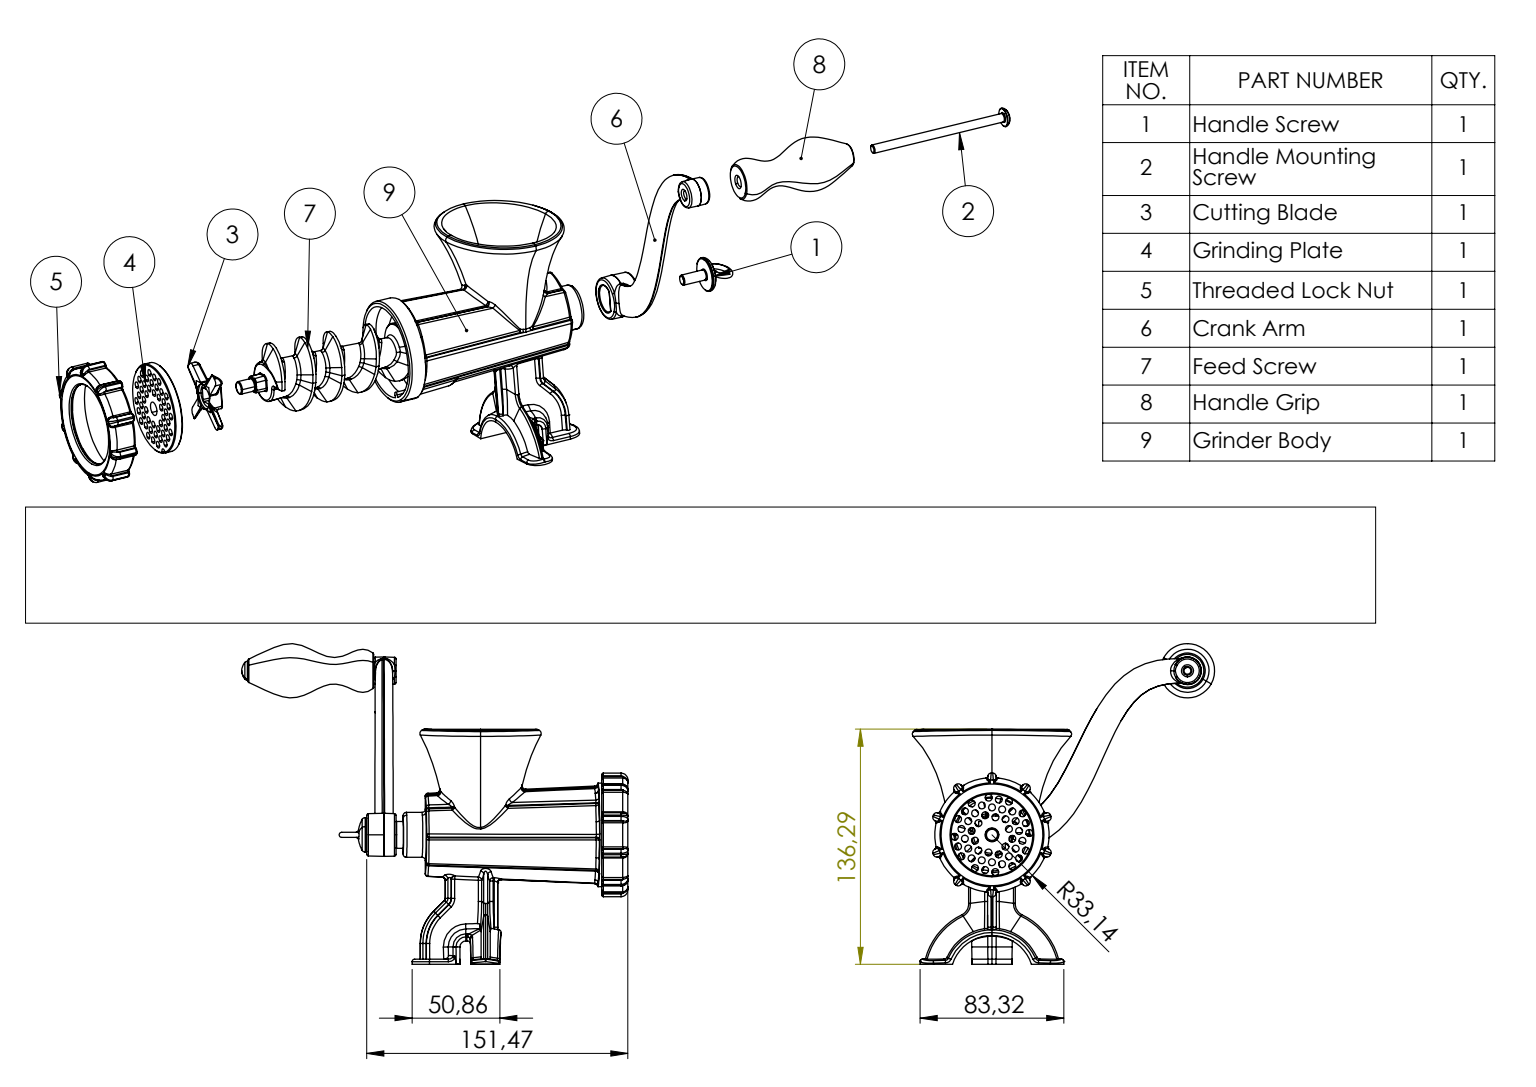
ISO-10303-21;
HEADER;
FILE_DESCRIPTION (('STEP AP214'),
    '1' );
FILE_NAME ('MAS-682',
    '2026-10-06T09:49:54',
    ( '' ),
    ( '' ),
    'SwSTEP 2.0',
    'SolidWorks 2020',
    '' );
FILE_SCHEMA (( 'AUTOMOTIVE_DESIGN' ));
ENDSEC;

DATA;
#1 = CARTESIAN_POINT ( 'NONE',  ( 0.9799183408087254188, 1466.964356560554961, 235.3982928250779310 ) ) ;
#2 = CIRCLE ( 'NONE', #35720, 101.7125698847119821 ) ;
#3 = CARTESIAN_POINT ( 'NONE',  ( -1.842962214803815835, 1515.372048948338943, 213.3835825141717351 ) ) ;
#4 = CARTESIAN_POINT ( 'NONE',  ( 9.183457267990059236, 1463.661210998930073, 215.2718514178839939 ) ) ;
#5 = CARTESIAN_POINT ( 'NONE',  ( -18.76815915579999938, 1485.949708182629820, 189.5055391954980166 ) ) ;
#6 = DIRECTION ( 'NONE',  ( -0.6736849260863841948, 0.000000000000000000, 0.7390186874254148774 ) ) ;
#7 = CARTESIAN_POINT ( 'NONE',  ( -29.55438145523249815, 1510.073575141020228, 200.5476930356480239 ) ) ;
#8 = AXIS2_PLACEMENT_3D ( 'NONE', #3263, #37391, #36278 ) ;
#9 = CARTESIAN_POINT ( 'NONE',  ( 24.07566136850000049, 1410.921070243630083, 209.6344585171510175 ) ) ;
#10 = CARTESIAN_POINT ( 'NONE',  ( 0.5551898266394985626, 1477.809674746627479, 198.7211068470872135 ) ) ;
#11 = CARTESIAN_POINT ( 'NONE',  ( 25.61451705386228284, 1436.639619060958239, 137.1797875125824362 ) ) ;
#12 = CARTESIAN_POINT ( 'NONE',  ( -1.480872463509999903, 1515.456375364289897, 204.9462865469589872 ) ) ;
#13 = CARTESIAN_POINT ( 'NONE',  ( 11.94438321470466136, 1435.361109817459010, 151.2115117280330310 ) ) ;
#14 =( BOUNDED_SURFACE ( )  B_SPLINE_SURFACE ( 3, 2, ( 
 ( #99288, #98203, #90906 ),
 ( #48377, #13076, #82520 ),
 ( #4699, #39956, #23138 ),
 ( #107158, #74130, #50021 ),
 ( #94768, #67940, #76875 ),
 ( #33745, #24238, #102047 ) ),
 .UNSPECIFIED., .F., .F., .F. ) 
 B_SPLINE_SURFACE_WITH_KNOTS ( ( 4, 2, 4 ),
 ( 3, 3 ),
 ( -1.474514954580286030E-17, 0.001312027981647312597, 0.002624055963294639939 ),
 ( 0.000000000000000000, 1.000000000000000000 ),
 .UNSPECIFIED. ) 
 GEOMETRIC_REPRESENTATION_ITEM ( )  RATIONAL_B_SPLINE_SURFACE ( (
 ( 1.000000000000000000, 0.9376006582765906705, 1.000000000000000000),
 ( 1.000000000000000000, 0.9569320108021501792, 1.000000000000000000),
 ( 1.000000000000000000, 0.9725743441620362528, 1.000000000000000000),
 ( 1.000000000000000000, 0.9942095667134138726, 1.000000000000000000),
 ( 1.000000000000000000, 1.000043666450818769, 1.000000000000000000),
 ( 1.000000000000000000, 1.000000000000000000, 1.000000000000000000) ) ) 
 REPRESENTATION_ITEM ( '' )  SURFACE ( )  );
#15 = CARTESIAN_POINT ( 'NONE',  ( 18.94656044352759849, 1455.761274322379904, 200.3458232381809694 ) ) ;
#16 = CARTESIAN_POINT ( 'NONE',  ( 1.715361092244999996, 1516.743010792419909, 212.5670474586069929 ) ) ;
#17 = CARTESIAN_POINT ( 'NONE',  ( -11.86274611122550127, 1422.387374207680068, 206.9860570071450070 ) ) ;
#18 = CARTESIAN_POINT ( 'NONE',  ( 0.1771307642749359867, 1476.157344213379929, 182.2594403546649744 ) ) ;
#20 = ORIENTED_EDGE ( 'NONE', *, *, #50403, .T. ) ;
#19 = DIRECTION ( 'NONE',  ( 0.9858563016923833633, 0.000000000000000000, 0.1675928173085483863 ) ) ;
#21 = B_SPLINE_CURVE_WITH_KNOTS ( 'NONE', 3,
 ( #95105, #62085, #88907, #54776, #87831, #29014 ),
 .UNSPECIFIED., .F., .F.,
 ( 4, 2, 4 ),
 ( 0.000000000000000000, 0.5000000000000000000, 1.000000000000000000 ),
 .UNSPECIFIED. ) ;
#22 = CARTESIAN_POINT ( 'NONE',  ( -25.18254675756193350, 1451.154070787092223, 137.5782062022625212 ) ) ;
#23 = CARTESIAN_POINT ( 'NONE',  ( -22.28696231330000188, 1506.798305107829947, 208.8466800722590051 ) ) ;
#24 = DIRECTION ( 'NONE',  ( -8.590429545572335868E-16, 0.9993908270191126375, 0.03489949670201628051 ) ) ;
#25 = CARTESIAN_POINT ( 'NONE',  ( -41.44976345434149323, 1445.539178997049930, 134.0999999985149884 ) ) ;
#26 = CARTESIAN_POINT ( 'NONE',  ( 1.285879139104720042E-15, 1391.913060387289988, 209.1218459572589836 ) ) ;
#27 = ORIENTED_EDGE ( 'NONE', *, *, #23843, .F. ) ;
#28 = CARTESIAN_POINT ( 'NONE',  ( -10.29516445159999982, 1471.669286221989978, 209.3797728120900103 ) ) ;
#29 = DIRECTION ( 'NONE',  ( -3.697785493223495027E-32, -1.000000000000000000, 1.836970198721029688E-16 ) ) ;
#30 = CARTESIAN_POINT ( 'NONE',  ( -14.66127766699999846, 1415.087974640030097, 218.7479844957980220 ) ) ;
#31 = CARTESIAN_POINT ( 'NONE',  ( -109.1321487942470014, 1384.869787291219836, 311.2644937792119322 ) ) ;
#32 = EDGE_CURVE ( 'NONE', #37900, #21516, #96808, .T. ) ;
#33 = CARTESIAN_POINT ( 'NONE',  ( -4.766037424247389964, 1433.470086930039997, 216.3697912905370231 ) ) ;
#34 = CARTESIAN_POINT ( 'NONE',  ( -2.760778634279479782, 1409.009468901610035, 188.0459411385839985 ) ) ;
#35 = AXIS2_PLACEMENT_3D ( 'NONE', #53186, #17882, #45348 ) ;
#36 = CARTESIAN_POINT ( 'NONE',  ( 21.19319384159999942, 1471.316885394430074, 209.8523956812749702 ) ) ;
#37 = CARTESIAN_POINT ( 'NONE',  ( -5.360823448879425079, 1422.265545810137382, 143.1524318712457386 ) ) ;
#38 = CARTESIAN_POINT ( 'NONE',  ( -12.43709857819999876, 1391.584050621440156, 209.7498280055400244 ) ) ;
#39 = CARTESIAN_POINT ( 'NONE',  ( -76.44887139282280941, 1385.142738521940146, 277.8929079653030385 ) ) ;
#40 = CARTESIAN_POINT ( 'NONE',  ( -11.42765938226460065, 1391.913060387289988, 211.2666090369880010 ) ) ;
#41 = CARTESIAN_POINT ( 'NONE',  ( 11.68414648092010033, 1426.908524124409951, 207.1431733947370049 ) ) ;
#42 = ORIENTED_EDGE ( 'NONE', *, *, #61891, .F. ) ;
#43 = CARTESIAN_POINT ( 'NONE',  ( -32.69752361389999606, 1451.315419473630072, 135.9818030182980237 ) ) ;
#44 = B_SPLINE_CURVE_WITH_KNOTS ( 'NONE', 3,
 ( #57452, #23800, #13187, #57991, #23253, #13738, #47922, #73698, #82058, #91579, #47375, #49043, #49590, #81500, #38947, #22130, #75882, #17028, #102702, #69152, #101057, #50145, #84272, #85931, #75348, #9234, #24355, #33305, #34970, #15944, #34425, #33864, #66948, #110030, #59640, #58541, #43391, #25996 ),
 .UNSPECIFIED., .F., .F.,
 ( 4, 2, 2, 2, 2, 2, 1, 1, 1, 1, 2, 2, 2, 2, 2, 1, 1, 1, 1, 2, 2, 2, 4 ),
 ( 0.000000000000000000, 0.1250000000000115463, 0.2500000000000230926, 0.3750000000000346390, 0.4375000000000425215, 0.4687500000000464073, 0.4843750000000510147, 0.4921875000000533462, 0.4960937500000545120, 0.4980468750000577316, 0.4990234375000622280, 0.5000000000000668354, 0.6250000000003189671, 0.6875000000004490852, 0.7187500000005095924, 0.7343750000005350165, 0.7421875000005526690, 0.7460937500005614398, 0.7480468750005607736, 0.7490234375005655476, 0.7500000000005703216, 0.8750000000002852163, 1.000000000000000000 ),
 .UNSPECIFIED. ) ;
#45 = CARTESIAN_POINT ( 'NONE',  ( 17.11746647137171706, 1443.086052842848176, 162.7559337440806644 ) ) ;
#47 = ORIENTED_EDGE ( 'NONE', *, *, #28974, .T. ) ;
#46 = CARTESIAN_POINT ( 'NONE',  ( 8.598096571001718758, 1427.995879741943554, 137.0999999980979567 ) ) ;
#48 = CARTESIAN_POINT ( 'NONE',  ( -109.4839102700000097, 1384.920896159549784, 311.2841190732590348 ) ) ;
#49 = CARTESIAN_POINT ( 'NONE',  ( 25.83534073490000083, 1509.142433023230069, 218.8511637550280113 ) ) ;
#50 = CARTESIAN_POINT ( 'NONE',  ( -8.821555121468717786, 1364.295427727885453, 207.6218459616988241 ) ) ;
#51 = CARTESIAN_POINT ( 'NONE',  ( -6.833281637050000690, 1495.558145441189936, 200.1869151102389992 ) ) ;
#52 = AXIS2_PLACEMENT_3D ( 'NONE', #79817, #89846, #28852 ) ;
#53 = CARTESIAN_POINT ( 'NONE',  ( 39.02162918670904901, 1452.247899825818649, 269.5933113026415526 ) ) ;
#54 = CARTESIAN_POINT ( 'NONE',  ( -1.906561575282239904E-08, 1509.051704408389924, 204.1347675157070114 ) ) ;
#55 = CARTESIAN_POINT ( 'NONE',  ( 5.639077273239999855, 1396.170382960830011, 219.3208623031979982 ) ) ;
#56 = CARTESIAN_POINT ( 'NONE',  ( -6.391938843916317836, 1508.551704408389696, 216.1347674408802106 ) ) ;
#57 = CARTESIAN_POINT ( 'NONE',  ( 5.798353088509999864, 1447.164911394289902, 201.8788308129090012 ) ) ;
#58 = DIRECTION ( 'NONE',  ( 0.8730704095473449389, 0.4873619484741930075, 0.01504630028510589926 ) ) ;
#59 = CARTESIAN_POINT ( 'NONE',  ( -7.009540617219531811, 1370.193319312941412, 208.3718459617010978 ) ) ;
#60 = CARTESIAN_POINT ( 'NONE',  ( -2.894710226049999946, 1455.369075570189807, 200.0025452760189921 ) ) ;
#61 = CARTESIAN_POINT ( 'NONE',  ( 2.477373605864999995, 1516.891731298979948, 206.2406231745169976 ) ) ;
#62 = CARTESIAN_POINT ( 'NONE',  ( 4.260142758989999834, 1446.575475407549902, 159.4573513494979693 ) ) ;
#63 = CYLINDRICAL_SURFACE ( 'NONE', #4748, 2.000000000000003553 ) ;
#64 = CARTESIAN_POINT ( 'NONE',  ( 13.58235818350000024, 1416.828044802929981, 196.3349386415980007 ) ) ;
#66 = EDGE_LOOP ( 'NONE', ( #105431, #26314, #4870, #3833, #51565, #60481, #89456, #79002, #97316, #37692 ) ) ;
#65 = CARTESIAN_POINT ( 'NONE',  ( -1.064557613579999895, 1496.012454471690035, 220.6945835667989968 ) ) ;
#67 = CARTESIAN_POINT ( 'NONE',  ( -1.491506560153236682, 1512.187213306747481, 242.6732489767341576 ) ) ;
#68 = ORIENTED_EDGE ( 'NONE', *, *, #43172, .F. ) ;
#69 = CARTESIAN_POINT ( 'NONE',  ( -16.59156838405375112, 1513.042027792487033, 221.1339923359998352 ) ) ;
#70 = ADVANCED_FACE ( 'NONE', ( #49805 ), #75938, .T. ) ;
#71 = CARTESIAN_POINT ( 'NONE',  ( -23.55087209330000064, 1410.914164826029946, 206.5508649875179970 ) ) ;
#73 = CARTESIAN_POINT ( 'NONE',  ( 16.84666619867320136, 1410.587845839309921, 191.9034688781510170 ) ) ;
#72 = CARTESIAN_POINT ( 'NONE',  ( -10.49968249828000033, 1425.371007265300022, 102.3058044465100096 ) ) ;
#74 = ADVANCED_FACE ( 'NONE', ( #10550 ), #8899, .T. ) ;
#75 = CARTESIAN_POINT ( 'NONE',  ( -5.770883602015000058, 1516.603620185149794, 211.4160555996369908 ) ) ;
#76 = CARTESIAN_POINT ( 'NONE',  ( 23.39541812081691674, 1509.845305380639729, 190.2643963894789181 ) ) ;
#77 = EDGE_CURVE ( 'NONE', #86690, #11573, #16701, .T. ) ;
#78 = TOROIDAL_SURFACE ( 'NONE', #103817, 9.500000000000000000, 0.5000000000000000000 ) ;
#79 = CARTESIAN_POINT ( 'NONE',  ( 21.64985223704960049, 1524.547395018738371, 234.6923279487310197 ) ) ;
#80 = B_SPLINE_CURVE_WITH_KNOTS ( 'NONE', 5,
 ( #89898, #13169, #47358, #81485, #38932, #107253 ),
 .UNSPECIFIED., .F., .F.,
 ( 6, 6 ),
 ( 0.000000000000000000, 1.000000000000000000 ),
 .UNSPECIFIED. ) ;
#81 = CARTESIAN_POINT ( 'NONE',  ( -39.02581108420000078, 1422.344276296430053, 266.4771448061979982 ) ) ;
#82 = CARTESIAN_POINT ( 'NONE',  ( -12.50903734399489942, 1378.842647904740033, 209.0065662253330174 ) ) ;
#83 = EDGE_CURVE ( 'NONE', #58839, #22042, #17431, .T. ) ;
#84 = CARTESIAN_POINT ( 'NONE',  ( 16.07415551216847049, 1461.167067577646549, 229.3519873809775333 ) ) ;
#85 = CONTEXT_DEPENDENT_SHAPE_REPRESENTATION ( #69986, #23231 ) ;
#86 = EDGE_CURVE ( 'NONE', #1893, #51148, #21, .T. ) ;
#87 = CARTESIAN_POINT ( 'NONE',  ( -4.994992778070000305, 1391.721842379389955, 214.6484993776389842 ) ) ;
#88 = CARTESIAN_POINT ( 'NONE',  ( 15.23962836178434799, 1416.181292664740113, 211.4166089860522106 ) ) ;
#89 = ORIENTED_EDGE ( 'NONE', *, *, #96759, .T. ) ;
#90 = CARTESIAN_POINT ( 'NONE',  ( 10.26791835527880004, 1396.449850368310081, 216.1922904392330338 ) ) ;
#91 = CARTESIAN_POINT ( 'NONE',  ( 9.827367186236088514, 1460.770885483560050, 206.7613957114989773 ) ) ;
#92 = AXIS2_PLACEMENT_3D ( 'NONE', #81436, #4747, #22069 ) ;
#93 = CARTESIAN_POINT ( 'NONE',  ( -17.53303485170000187, 1459.032577061930169, 228.4504051497980015 ) ) ;
#94 = ORIENTED_EDGE ( 'NONE', *, *, #44106, .T. ) ;
#96 = ORIENTED_EDGE ( 'NONE', *, *, #80068, .T. ) ;
#95 = AXIS2_PLACEMENT_3D ( 'NONE', #82965, #55590, #47722 ) ;
#97 = CARTESIAN_POINT ( 'NONE',  ( 2.803078862940000082, 1426.178365722219951, 191.2633630063989756 ) ) ;
#98 = CARTESIAN_POINT ( 'NONE',  ( 32.97913964219430483, 1512.187213306747481, 197.9697544589745632 ) ) ;
#99 = DIRECTION ( 'NONE',  ( 0.9858563016923833633, 0.000000000000000000, 0.1675928173085483863 ) ) ;
#100 = CARTESIAN_POINT ( 'NONE',  ( -12.21821484229520927, 1417.425190588804981, 199.7413714526001911 ) ) ;
#101 = AXIS2_PLACEMENT_3D ( 'NONE', #52542, #86674, #33491 ) ;
#102 = CARTESIAN_POINT ( 'NONE',  ( 4.324092179420000015, 1515.269353058490196, 209.1218459615519976 ) ) ;
#103 = CARTESIAN_POINT ( 'NONE',  ( -2.622430729442981168, 1523.621879633028584, 242.1535192357228254 ) ) ;
#104 = CARTESIAN_POINT ( 'NONE',  ( 2.470168521978398868, 1512.187213306747481, 175.3649660270905315 ) ) ;
#105 = CARTESIAN_POINT ( 'NONE',  ( 3.199785385034799923, 1421.555840881979975, 183.4721396264059763 ) ) ;
#106 = CARTESIAN_POINT ( 'NONE',  ( 9.417062327005512046, 1451.666586838229932, 209.4644760955090135 ) ) ;
#107 = CARTESIAN_POINT ( 'NONE',  ( 17.11714618744633754, 1443.086052842848630, 162.7561046190426737 ) ) ;
#108 = EDGE_CURVE ( 'NONE', #73608, #106056, #21407, .T. ) ;
#109 = CARTESIAN_POINT ( 'NONE',  ( -98.27039657997829636, 1384.868559307870100, 295.9020111865049785 ) ) ;
#110 = ORIENTED_EDGE ( 'NONE', *, *, #5630, .F. ) ;
#111 = CARTESIAN_POINT ( 'NONE',  ( 6.939219482805000005, 1516.783701990830195, 203.3409846960470020 ) ) ;
#112 = CARTESIAN_POINT ( 'NONE',  ( 5.786847739675000213, 1517.104497701820037, 209.8595134730280165 ) ) ;
#113 = ORIENTED_EDGE ( 'NONE', *, *, #67279, .T. ) ;
#114 = CARTESIAN_POINT ( 'NONE',  ( 10.79382126600000014, 1414.913060387329779, 222.1041115775979904 ) ) ;
#115 = CARTESIAN_POINT ( 'NONE',  ( 3.849857897463838885, 1511.509056589855390, 217.2694430494650248 ) ) ;
#116 = ORIENTED_EDGE ( 'NONE', *, *, #25867, .F. ) ;
#117 = CARTESIAN_POINT ( 'NONE',  ( -14.19373553490000006, 1416.535385209630022, 221.7254479851980022 ) ) ;
#118 = CARTESIAN_POINT ( 'NONE',  ( -12.93811130839999812, 1442.831169986189934, 169.4238961894979809 ) ) ;
#119 = DIRECTION ( 'NONE',  ( -5.980589973904019347E-17, 1.000000000000000000, -1.736889445713099699E-16 ) ) ;
#120 = EDGE_CURVE ( 'NONE', #81793, #103948, #97600, .T. ) ;
#121 = CARTESIAN_POINT ( 'NONE',  ( -9.628359219779209610, 1460.738556064009799, 208.1949697569470175 ) ) ;
#122 = CARTESIAN_POINT ( 'NONE',  ( -5.139599399479999775, 1425.322806783530041, 186.3313725629980127 ) ) ;
#123 = CARTESIAN_POINT ( 'NONE',  ( 10.94055631708340037, 1470.192781946979949, 206.9724510450730008 ) ) ;
#124 = CARTESIAN_POINT ( 'NONE',  ( -3.048415848927723992, 1468.134006689671196, 219.8853015524805699 ) ) ;
#125 = EDGE_CURVE ( 'NONE', #75164, #6066, #41467, .T. ) ;
#126 = CARTESIAN_POINT ( 'NONE',  ( -15.90471755817952548, 1410.840444494871690, 191.2727014167670916 ) ) ;
#127 = CARTESIAN_POINT ( 'NONE',  ( -16.54254117820000047, 1379.596826475559965, 208.2028925074129688 ) ) ;
#128 = CARTESIAN_POINT ( 'NONE',  ( 22.53878404599999641, 1411.058442739730026, 206.1986151668880041 ) ) ;
#130 = DIRECTION ( 'NONE',  ( -0.6736849260863839728, 0.000000000000000000, 0.7390186874254150995 ) ) ;
#129 = CARTESIAN_POINT ( 'NONE',  ( 17.81158319340000062, 1457.914457808930138, 229.9274238559980006 ) ) ;
#131 = CARTESIAN_POINT ( 'NONE',  ( -4.952890104507372548, 1423.293534163835830, 184.7224492574210615 ) ) ;
#132 = AXIS2_PLACEMENT_3D ( 'NONE', #29173, #87435, #11285 ) ;
#133 = B_SPLINE_SURFACE_WITH_KNOTS ( 'NONE', 5, 3, ( 
 ( #34867, #77434, #42173, #67396 ),
 ( #93646, #52248, #60652, #69055 ),
 ( #103155, #43831, #101494, #16929 ),
 ( #41622, #26457, #43287, #93111 ),
 ( #86374, #34317, #94776, #76885 ),
 ( #8007, #734, #1283, #85822 ),
 ( #35424, #50030, #76324, #8554 ),
 ( #51130, #69611, #84159, #18053 ),
 ( #24248, #109929, #16382, #42726 ) ),
 .UNSPECIFIED., .F., .F., .F.,
 ( 6, 3, 6 ),
 ( 4, 4 ),
 ( 0.000000000000000000, 5.782490304330000441, 11.25975508159999983 ),
 ( 37.69911184309999896, 40.20365518519999881 ),
 .UNSPECIFIED. ) ;
#134 = CARTESIAN_POINT ( 'NONE',  ( -17.39685236538799984, 1503.136637835580132, 222.8801028628849963 ) ) ;
#135 = ORIENTED_EDGE ( 'NONE', *, *, #51675, .F. ) ;
#136 = CARTESIAN_POINT ( 'NONE',  ( -2.793439186891359949, 1486.025328193850100, 182.0741020391329812 ) ) ;
#137 = DIRECTION ( 'NONE',  ( -1.000000000000000000, 0.000000000000000000, 0.000000000000000000 ) ) ;
#138 = CARTESIAN_POINT ( 'NONE',  ( -2.931110993877138249, 1485.094118085803984, 183.0973985693935617 ) ) ;
#139 = CARTESIAN_POINT ( 'NONE',  ( 5.979558325686289422, 1406.768155905330104, 269.6447222190780053 ) ) ;
#141 = ORIENTED_EDGE ( 'NONE', *, *, #18307, .F. ) ;
#140 = CARTESIAN_POINT ( 'NONE',  ( 0.7783252048321530614, 1515.125841190099891, 204.7939957918700316 ) ) ;
#142 = CARTESIAN_POINT ( 'NONE',  ( 0.9041354327699999693, 1416.839648768630013, 190.2140802940980109 ) ) ;
#143 = AXIS2_PLACEMENT_3D ( 'NONE', #57309, #48343, #30414 ) ;
#144 = CARTESIAN_POINT ( 'NONE',  ( -0.9578802547590020700, 1508.340034268889895, 220.7784182282989889 ) ) ;
#145 = CARTESIAN_POINT ( 'NONE',  ( -11.74804893329999800, 1426.270137612329790, 145.0346010018980110 ) ) ;
#146 = DIRECTION ( 'NONE',  ( -1.110223024629289185E-15, -0.7071067811865475727, -0.7071067811865475727 ) ) ;
#147 = CARTESIAN_POINT ( 'NONE',  ( 0.000000000000000000, 1511.163060387329779, 209.1218459616979999 ) ) ;
#148 = DIRECTION ( 'NONE',  ( 1.000000000000000000, 5.309750374689999822E-19, 2.343158368729999945E-19 ) ) ;
#149 = CARTESIAN_POINT ( 'NONE',  ( -5.649091365077420157, 1427.323616392150143, 201.6849725672220188 ) ) ;
#150 = CARTESIAN_POINT ( 'NONE',  ( -15.65821252386499829, 1513.518111364920060, 223.8216251916669819 ) ) ;
#151 = CARTESIAN_POINT ( 'NONE',  ( 9.215280650669999574, 1410.394055827930060, 230.1315963332980061 ) ) ;
#153 = FACE_OUTER_BOUND ( 'NONE', #32956, .T. ) ;
#152 = CARTESIAN_POINT ( 'NONE',  ( -25.75006378359999815, 1482.723232260229906, 211.9130519178279997 ) ) ;
#154 = DIRECTION ( 'NONE',  ( -0.02617375475769094517, 0.9996573249755578150, 0.0004088821302708953143 ) ) ;
#155 = ORIENTED_EDGE ( 'NONE', *, *, #76478, .F. ) ;
#156 = CARTESIAN_POINT ( 'NONE',  ( -2.881222795715000284, 1516.891731298979948, 206.6444723262370076 ) ) ;
#157 = CARTESIAN_POINT ( 'NONE',  ( 27.01536995560000065, 1412.459480457830068, 266.9350197775979723 ) ) ;
#158 = DIRECTION ( 'NONE',  ( 0.8672669759446630655, 0.000000000000000000, -0.4978433412588735285 ) ) ;
#159 = CARTESIAN_POINT ( 'NONE',  ( 22.53781764839999724, 1430.293776123330190, 201.7931574036180109 ) ) ;
#160 = CARTESIAN_POINT ( 'NONE',  ( -0.2682927907274870183, 1508.576597181550142, 237.9003827947630043 ) ) ;
#161 = CARTESIAN_POINT ( 'NONE',  ( -7.567241880450000124, 1385.515695150829970, 219.0512258816089854 ) ) ;
#162 = CARTESIAN_POINT ( 'NONE',  ( 21.91792426780000369, 1509.678451168330184, 227.8819284857980279 ) ) ;
#163 = CARTESIAN_POINT ( 'NONE',  ( -6.501609782144661231, 1517.151704408390060, 200.8207946853451631 ) ) ;
#164 = AXIS2_PLACEMENT_3D ( 'NONE', #96746, #87233, #71584 ) ;
#165 = CARTESIAN_POINT ( 'NONE',  ( -14.80402621179999834, 1415.917690476640018, 204.7946628682890093 ) ) ;
#166 = CARTESIAN_POINT ( 'NONE',  ( -13.11944326200000077, 1446.139497881190209, 187.9998882741980140 ) ) ;
#167 = CARTESIAN_POINT ( 'NONE',  ( -4.911821946417970430, 1485.009740505319996, 198.2803573512069875 ) ) ;
#168 = B_SPLINE_SURFACE_WITH_KNOTS ( 'NONE', 5, 5, ( 
 ( #106952, #71755, #28601, #29694, #97994, #64429 ),
 ( #81736, #88517, #89050, #98547, #97459, #20727 ),
 ( #54922, #21816, #107503, #56015, #12336, #105310 ),
 ( #90139, #13422, #62802, #46527, #11801, #45969 ),
 ( #80104, #37555, #80661, #98449, #4411, #47512 ),
 ( #96816, #3329, #28500, #89503, #82194, #106305 ),
 ( #97348, #37453, #12795, #72186, #90039, #21163 ),
 ( #90596, #62695, #38004, #13317, #4937, #12239 ),
 ( #72718, #45871, #80005, #29056, #106840, #63242 ) ),
 .UNSPECIFIED., .F., .F., .F.,
 ( 6, 3, 6 ),
 ( 6, 6 ),
 ( 14.29638737439180041, 25.07790639679999956, 35.02433850343369670 ),
 ( 0.000000000000000000, 2.000134677740009970 ),
 .UNSPECIFIED. ) ;
#169 = CARTESIAN_POINT ( 'NONE',  ( -8.621279951388869378, 1436.974942194019832, 209.5887057810519991 ) ) ;
#170 = CARTESIAN_POINT ( 'NONE',  ( -4.720696006799999900, 1497.300349750090163, 219.8012105612990013 ) ) ;
#171 = ORIENTED_EDGE ( 'NONE', *, *, #62426, .F. ) ;
#172 = CARTESIAN_POINT ( 'NONE',  ( 4.989246313819999834, 1471.909539260290103, 189.7082128665990126 ) ) ;
#173 = CARTESIAN_POINT ( 'NONE',  ( -12.50898706442170116, 1409.349883841199926, 217.3002069970499974 ) ) ;
#174 = EDGE_CURVE ( 'NONE', #66491, #29176, #106889, .T. ) ;
#175 = CARTESIAN_POINT ( 'NONE',  ( -11.30102602861320094, 1508.425847713210032, 208.0120230822289784 ) ) ;
#176 = CARTESIAN_POINT ( 'NONE',  ( -12.26345067459182658, 1378.041391332198373, 210.3086285185297868 ) ) ;
#177 = CARTESIAN_POINT ( 'NONE',  ( -23.55147266200000189, 1470.760850431830022, 269.0841978914980359 ) ) ;
#178 = DIRECTION ( 'NONE',  ( 0.000000000000000000, 0.000000000000000000, 1.000000000000000000 ) ) ;
#179 = CARTESIAN_POINT ( 'NONE',  ( -13.16128167722848552, 1513.520077403203913, 192.3341213175320092 ) ) ;
#180 = EDGE_CURVE ( 'NONE', #17368, #18936, #5451, .T. ) ;
#181 = CARTESIAN_POINT ( 'NONE',  ( -24.15092527543778189, 1444.494566185576332, 211.6397483413928455 ) ) ;
#182 = CARTESIAN_POINT ( 'NONE',  ( -76.22674438190679780, 1384.646826080419942, 301.0779023118020064 ) ) ;
#183 = CARTESIAN_POINT ( 'NONE',  ( -21.60464161394589766, 1384.953571151939968, 202.1045221056799903 ) ) ;
#184 = CIRCLE ( 'NONE', #28783, 1.000000000000007994 ) ;
#185 = CARTESIAN_POINT ( 'NONE',  ( 11.29240053233250052, 1415.034069327070029, 222.6155400430430120 ) ) ;
#186 = DIRECTION ( 'NONE',  ( -1.000000000000000000, 0.000000000000000000, 0.000000000000000000 ) ) ;
#187 = CARTESIAN_POINT ( 'NONE',  ( -14.61131892634599971, 1485.012037849769968, 224.2679068592169926 ) ) ;
#188 = CARTESIAN_POINT ( 'NONE',  ( -22.86536645260000000, 1410.206636297830073, 204.9906524142479896 ) ) ;
#189 = CIRCLE ( 'NONE', #57423, 12.49965726619999984 ) ;
#190 = CARTESIAN_POINT ( 'NONE',  ( 13.83520663969999909, 1414.913060387329779, 199.8641522158279997 ) ) ;
#191 = CARTESIAN_POINT ( 'NONE',  ( -20.12564951288306503, 1512.187213306747481, 180.7149624981946658 ) ) ;
#192 = ADVANCED_FACE ( 'NONE', ( #107906 ), #49678, .T. ) ;
#193 = CARTESIAN_POINT ( 'NONE',  ( 10.49733858283609855, 1480.659481621079976, 208.1380713321520091 ) ) ;
#194 = DIRECTION ( 'NONE',  ( -0.000000000000000000, -1.000000000000000000, 0.000000000000000000 ) ) ;
#195 = CARTESIAN_POINT ( 'NONE',  ( -17.48499182319999790, 1442.494624508590050, 219.3180649765990040 ) ) ;
#196 = CARTESIAN_POINT ( 'NONE',  ( 17.03788438627352519, 1524.775785348137333, 181.0918340916085754 ) ) ;
#197 = CARTESIAN_POINT ( 'NONE',  ( -21.44637737161449920, 1506.412668956640118, 216.0243792029939982 ) ) ;
#200 = CARTESIAN_POINT ( 'NONE',  ( 10.79382269979189957, 1414.913060387349788, 222.1041130917409987 ) ) ;
#199 = CIRCLE ( 'NONE', #3805, 0.5000000000000157652 ) ;
#198 = CARTESIAN_POINT ( 'NONE',  ( -22.57636395089999937, 1411.060965688729766, 211.7929440282880194 ) ) ;
#201 = CARTESIAN_POINT ( 'NONE',  ( 11.69274081191520054, 1426.725035085969921, 141.0012239352140000 ) ) ;
#202 = CARTESIAN_POINT ( 'NONE',  ( 9.734438220109071338, 1436.124822200840072, 210.5259218765519620 ) ) ;
#203 = CARTESIAN_POINT ( 'NONE',  ( -10.63028651890000020, 1491.023698122589849, 211.9405787866489845 ) ) ;
#204 = CARTESIAN_POINT ( 'NONE',  ( 6.587579149753620023, 1448.214850730340004, 201.2521096501800173 ) ) ;
#205 = CARTESIAN_POINT ( 'NONE',  ( -12.02002121700249937, 1447.120365805550136, 187.5076542713389927 ) ) ;
#206 = CIRCLE ( 'NONE', #57435, 2.000000000000001776 ) ;
#207 = CARTESIAN_POINT ( 'NONE',  ( -5.006329619514999330, 1516.755758396839838, 202.5714564999769891 ) ) ;
#208 = CARTESIAN_POINT ( 'NONE',  ( -4.941360932494764491, 1398.060275951993162, 221.1476519450009164 ) ) ;
#209 = CARTESIAN_POINT ( 'NONE',  ( -3.034707026709789979, 1440.440247136690004, 157.2489849372729793 ) ) ;
#210 = FACE_BOUND ( 'NONE', #98928, .T. ) ;
#211 = CARTESIAN_POINT ( 'NONE',  ( 1.951029617469999922, 1508.751449870530223, 237.3205679125979941 ) ) ;
#213 = EDGE_LOOP ( 'NONE', ( #57511, #100598, #97650, #95419, #60917 ) ) ;
#212 = CARTESIAN_POINT ( 'NONE',  ( -31.38187927383859943, 1379.627610869280034, 219.3043553578710032 ) ) ;
#214 = ORIENTED_EDGE ( 'NONE', *, *, #74162, .T. ) ;
#215 = CARTESIAN_POINT ( 'NONE',  ( 11.97689773866060037, 1433.612225593400126, 149.9683442909959865 ) ) ;
#216 = CARTESIAN_POINT ( 'NONE',  ( 21.50855465202003813, 1524.374578187333327, 184.1253178261501660 ) ) ;
#217 = EDGE_LOOP ( 'NONE', ( #25668, #43396, #24555, #73471 ) ) ;
#218 = CARTESIAN_POINT ( 'NONE',  ( -106.9777543680000065, 1379.497227361900059, 308.7284971550590171 ) ) ;
#219 = EDGE_CURVE ( 'NONE', #44996, #39203, #32843, .T. ) ;
#220 = CARTESIAN_POINT ( 'NONE',  ( -10.22078022364619976, 1448.827725899079724, 207.2905427559460065 ) ) ;
#221 = CARTESIAN_POINT ( 'NONE',  ( -4.554962005479259446, 1508.731359867455467, 211.6097811027402713 ) ) ;
#223 = CARTESIAN_POINT ( 'NONE',  ( 1.188177619867464285, 1416.835288280217583, 190.1185025207718695 ) ) ;
#222 = DIRECTION ( 'NONE',  ( 0.7071067811870476172, 0.000000000000000000, -0.7071067811860475283 ) ) ;
#224 = CARTESIAN_POINT ( 'NONE',  ( 16.85900957629469943, 1498.111060690920112, 230.7389555287900009 ) ) ;
#225 = AXIS2_PLACEMENT_3D ( 'NONE', #60606, #95291, #28634 ) ;
#226 = CARTESIAN_POINT ( 'NONE',  ( 2.328600095410000126, 1488.173045798130033, 182.1148965703980025 ) ) ;
#227 = CARTESIAN_POINT ( 'NONE',  ( 13.43167025587599817, 1509.382104656720003, 235.1752264429409820 ) ) ;
#228 = DIRECTION ( 'NONE',  ( -0.6736849260863839728, 0.000000000000000000, 0.7390186874254150995 ) ) ;
#229 =( LENGTH_UNIT ( ) NAMED_UNIT ( * ) SI_UNIT ( .MILLI., .METRE. ) );
#230 = CARTESIAN_POINT ( 'NONE',  ( 4.229167303610000594, 1436.983388288790138, 227.1518914930990150 ) ) ;
#231 = CARTESIAN_POINT ( 'NONE',  ( 13.54623987573500088, 1415.059973085240017, 197.7769859117730107 ) ) ;
#232 = CARTESIAN_POINT ( 'NONE',  ( 11.57525528770000101, 1432.243446488439986, 151.1962572209980067 ) ) ;
#233 = CARTESIAN_POINT ( 'NONE',  ( 7.300066962235000290, 1513.142795523620180, 201.9269575992269949 ) ) ;
#234 = VERTEX_POINT ( 'NONE', #57535 ) ;
#235 = CARTESIAN_POINT ( 'NONE',  ( 13.94902171141210090, 1435.073072362720040, 149.1168395385139718 ) ) ;
#236 = ORIENTED_EDGE ( 'NONE', *, *, #47228, .T. ) ;
#237 = VERTEX_POINT ( 'NONE', #65385 ) ;
#238 = EDGE_CURVE ( 'NONE', #55027, #57510, #22026, .T. ) ;
#239 = CARTESIAN_POINT ( 'NONE',  ( 13.40011037178709330, 1444.420227106130369, 169.3684798139838676 ) ) ;
#240 = CARTESIAN_POINT ( 'NONE',  ( -11.01696037870000033, 1462.338713412430252, 233.0647636304979926 ) ) ;
#241 = CARTESIAN_POINT ( 'NONE',  ( -9.862951377749247683, 1522.051704408389924, 228.3939896778649654 ) ) ;
#242 = DIRECTION ( 'NONE',  ( -8.555280247707230573E-26, -1.000000000000000000, 1.836970198721029688E-16 ) ) ;
#243 = CARTESIAN_POINT ( 'NONE',  ( -7.886135186697788235, 1512.218159651028827, 212.0631589305448301 ) ) ;
#244 = AXIS2_PLACEMENT_3D ( 'NONE', #101072, #98882, #31677 ) ;
#245 = EDGE_CURVE ( 'NONE', #43735, #91400, #105524, .T. ) ;
#246 = LINE ( 'NONE', #1902, #99740 ) ;
#247 = CARTESIAN_POINT ( 'NONE',  ( -18.61085923841566014, 1379.601406803549708, 208.6983520666371419 ) ) ;
#248 = CARTESIAN_POINT ( 'NONE',  ( -18.76550561599999867, 1380.296266888499986, 210.4015402955490117 ) ) ;
#249 = ORIENTED_EDGE ( 'NONE', *, *, #87778, .F. ) ;
#250 = CARTESIAN_POINT ( 'NONE',  ( -4.043990345725000601, 1516.983612918759945, 206.6425990843970055 ) ) ;
#251 = ORIENTED_EDGE ( 'NONE', *, *, #53107, .T. ) ;
#252 = CARTESIAN_POINT ( 'NONE',  ( 21.27308478715089990, 1440.913060387330006, 223.7805658757509946 ) ) ;
#253 = CARTESIAN_POINT ( 'NONE',  ( -18.65749898560000020, 1509.387464492830077, 230.8014192534980111 ) ) ;
#254 = EDGE_LOOP ( 'NONE', ( #74179, #87875, #88245, #39917, #100540, #44653, #57226, #30791 ) ) ;
#255 = FACE_OUTER_BOUND ( 'NONE', #49988, .T. ) ;
#256 = CARTESIAN_POINT ( 'NONE',  ( 7.213837368615000578, 1512.784460098860109, 215.9877155789269807 ) ) ;
#258 = EDGE_LOOP ( 'NONE', ( #43493, #77998, #28454, #11261 ) ) ;
#257 = CARTESIAN_POINT ( 'NONE',  ( 2.105736771246019767, 1423.442917612190058, 192.6277106367970191 ) ) ;
#259 = CARTESIAN_POINT ( 'NONE',  ( 23.78270988279999898, 1434.944176083839920, 215.5045224494480181 ) ) ;
#260 = CARTESIAN_POINT ( 'NONE',  ( -17.51735096566159910, 1508.551704408389924, 210.4017072017840064 ) ) ;
#261 = EDGE_CURVE ( 'NONE', #100109, #93900, #60124, .T. ) ;
#262 = DIRECTION ( 'NONE',  ( 1.755985294532464991E-16, -1.000000000000000000, 1.338183447452830017E-16 ) ) ;
#263 = CARTESIAN_POINT ( 'NONE',  ( 5.082331142230000154, 1453.684120746589770, 217.0135184815189859 ) ) ;
#264 = CARTESIAN_POINT ( 'NONE',  ( -24.62269181266490037, 1457.704162723289983, 212.0269868133230204 ) ) ;
#265 = EDGE_CURVE ( 'NONE', #68013, #83547, #85444, .T. ) ;
#266 = CARTESIAN_POINT ( 'NONE',  ( 7.720650135305000994, 1516.977993847330026, 214.9014730243169993 ) ) ;
#267 = CARTESIAN_POINT ( 'NONE',  ( -2.999960124414019713, 1428.921094993090037, 200.2473963957619958 ) ) ;
#268 = CARTESIAN_POINT ( 'NONE',  ( 6.161099242332739756, 1511.774605969369986, 217.7619246857520068 ) ) ;
#269 = CARTESIAN_POINT ( 'NONE',  ( 7.260544162646080046, 1508.878901399440110, 215.8879859943839961 ) ) ;
#270 = CARTESIAN_POINT ( 'NONE',  ( 3.268859396054999866, 1516.922519270759949, 211.5998327024669834 ) ) ;
#271 = CARTESIAN_POINT ( 'NONE',  ( 14.81130958389999996, 1410.375311269529902, 191.5354464119980094 ) ) ;
#272 = AXIS2_PLACEMENT_3D ( 'NONE', #31208, #50242, #83816 ) ;
#273 = CARTESIAN_POINT ( 'NONE',  ( -16.59643141521007692, 1486.110667197937119, 187.3981733332393844 ) ) ;
#275 = EDGE_LOOP ( 'NONE', ( #35605, #7044, #107686, #49764, #7625 ) ) ;
#274 = CARTESIAN_POINT ( 'NONE',  ( -62.99252469870000937, 1388.208599921950054, 284.2099993179589887 ) ) ;
#276 = CARTESIAN_POINT ( 'NONE',  ( -56.29735061249719763, 1385.085427587770027, 274.2983070328880331 ) ) ;
#277 = CARTESIAN_POINT ( 'NONE',  ( 33.67855476909999624, 1460.266122003729834, 261.9078250184979879 ) ) ;
#278 = CARTESIAN_POINT ( 'NONE',  ( 10.93308164779909930, 1490.452501404730128, 209.9926135395130018 ) ) ;
#279 = CARTESIAN_POINT ( 'NONE',  ( -29.22959469711409852, 1509.933780326070064, 211.7723416727030212 ) ) ;
#280 = CARTESIAN_POINT ( 'NONE',  ( -7.422625755698760486, 1509.173068315250021, 237.5382155034599805 ) ) ;
#281 = CARTESIAN_POINT ( 'NONE',  ( -23.72450110970000026, 1447.345343915189915, 214.6425533432180259 ) ) ;
#282 = AXIS2_PLACEMENT_3D ( 'NONE', #69728, #96558, #36645 ) ;
#284 = CARTESIAN_POINT ( 'NONE',  ( 17.19105300219910148, 1409.567693813439973, 222.3521885693010063 ) ) ;
#283 = LINE ( 'NONE', #53444, #107281 ) ;
#285 = LINE ( 'NONE', #92652, #110374 ) ;
#287 = B_SPLINE_CURVE_WITH_KNOTS ( 'NONE', 3,
 ( #66514, #15499, #49697, #83827, #109592, #28341 ),
 .UNSPECIFIED., .F., .F.,
 ( 4, 2, 4 ),
 ( 2.797157557069881010E-17, 0.001087661325621732452, 0.002175322651243436715 ),
 .UNSPECIFIED. ) ;
#286 = DIRECTION ( 'NONE',  ( 0.8775825618903774217, -3.365001152038843908E-31, 0.4794255386041944567 ) ) ;
#288 = VERTEX_POINT ( 'NONE', #17119 ) ;
#289 = CARTESIAN_POINT ( 'NONE',  ( 2.482067860225000366, 1517.099836525840146, 203.3337487049469985 ) ) ;
#290 = CARTESIAN_POINT ( 'NONE',  ( -11.00800901137619903, 1508.439403004749920, 218.3132624233929846 ) ) ;
#291 = CARTESIAN_POINT ( 'NONE',  ( 29.02628104170000256, 1509.926680456829899, 206.2525988583179810 ) ) ;
#292 = CARTESIAN_POINT ( 'NONE',  ( 24.56509571990000040, 1440.948426447710062, 213.0043250210379995 ) ) ;
#293 = CARTESIAN_POINT ( 'NONE',  ( -4.675540975309999681, 1462.620895424390028, 200.5633310686890241 ) ) ;
#294 = CARTESIAN_POINT ( 'NONE',  ( -19.66678637224480397, 1519.551704408389924, 215.8936635741279986 ) ) ;
#295 = VECTOR ( 'NONE', #1841, 999.9999999999998863 ) ;
#296 = CARTESIAN_POINT ( 'NONE',  ( 27.60463613754729906, 1435.937341596739998, 136.4952273551159863 ) ) ;
#297 = CARTESIAN_POINT ( 'NONE',  ( 36.19701834746070546, 1449.940556718190010, 136.2509691137539960 ) ) ;
#298 = CARTESIAN_POINT ( 'NONE',  ( 18.86027053263898168, 1512.187213306747481, 230.7762769316004778 ) ) ;
#299 = CARTESIAN_POINT ( 'NONE',  ( -107.7923298369999969, 1386.973993580999831, 297.6574877858589616 ) ) ;
#300 = CARTESIAN_POINT ( 'NONE',  ( -16.09127082379999862, 1410.842149181930154, 226.7264691084980086 ) ) ;
#301 = CARTESIAN_POINT ( 'NONE',  ( 11.69460626421270000, 1479.933455554200009, 210.6357844716710019 ) ) ;
#302 = CARTESIAN_POINT ( 'NONE',  ( 5.597778194180000888, 1506.679269386989972, 219.3685102149989916 ) ) ;
#303 = CIRCLE ( 'NONE', #93224, 4.820754716980014010 ) ;
#304 = LINE ( 'NONE', #17034, #54663 ) ;
#305 = ORIENTED_EDGE ( 'NONE', *, *, #65971, .T. ) ;
#306 = CARTESIAN_POINT ( 'NONE',  ( 0.8090580814599999115, 1427.166763959530044, 147.9649995502979891 ) ) ;
#307 = CARTESIAN_POINT ( 'NONE',  ( 3.902542035141590038, 1426.015650130040058, 185.2953857556300079 ) ) ;
#308 = EDGE_CURVE ( 'NONE', #12135, #84259, #7929, .T. ) ;
#309 = CARTESIAN_POINT ( 'NONE',  ( -4.487249408019919450, 1509.038630944639863, 212.6094330731689865 ) ) ;
#310 = CARTESIAN_POINT ( 'NONE',  ( -19.02974267272306719, 1517.051704408389924, 207.1627782414018100 ) ) ;
#311 = CARTESIAN_POINT ( 'NONE',  ( -0.5392968480769999573, 1417.272289817929959, 235.8882545161980033 ) ) ;
#313 = CARTESIAN_POINT ( 'NONE',  ( 31.55762699681125127, 1523.390106123591067, 196.3178534513329794 ) ) ;
#312 = CARTESIAN_POINT ( 'NONE',  ( 11.46319645939999887, 1501.893709296690076, 208.7006337201350163 ) ) ;
#314 = CARTESIAN_POINT ( 'NONE',  ( -12.99045328924907139, 1444.881939451659264, 186.2719392246208656 ) ) ;
#315 = DIRECTION ( 'NONE',  ( 0.2720708970484284062, 0.6839977328998089190, 0.6768489701308448847 ) ) ;
#316 = CARTESIAN_POINT ( 'NONE',  ( -8.788316527315000570, 1511.741868877540128, 215.3741124244170067 ) ) ;
#317 = AXIS2_PLACEMENT_3D ( 'NONE', #43515, #103956, #9895 ) ;
#318 = DIRECTION ( 'NONE',  ( 0.000000000000000000, 1.000000000000000000, -1.836970198721029688E-16 ) ) ;
#319 = CARTESIAN_POINT ( 'NONE',  ( -38.49765372626540483, 1444.525112228479884, 137.1053225085370002 ) ) ;
#320 = CARTESIAN_POINT ( 'NONE',  ( -5.102340803919999779, 1483.010473641589897, 199.7820758705289848 ) ) ;
#321 = CARTESIAN_POINT ( 'NONE',  ( 25.44234826850000175, 1436.623918441529895, 137.2992118829979802 ) ) ;
#322 = CARTESIAN_POINT ( 'NONE',  ( -10.92603999506069989, 1396.294606111510120, 207.3491235618079997 ) ) ;
#323 = VERTEX_POINT ( 'NONE', #26651 ) ;
#324 = EDGE_CURVE ( 'NONE', #40683, #47896, #52438, .T. ) ;
#325 = CARTESIAN_POINT ( 'NONE',  ( -16.89772930833600029, 1410.137463210610122, 226.0661309239629873 ) ) ;
#326 = CARTESIAN_POINT ( 'NONE',  ( 2.488082932330000219, 1441.600846913620217, 150.5962877614979902 ) ) ;
#327 = ORIENTED_EDGE ( 'NONE', *, *, #30892, .T. ) ;
#328 = VERTEX_POINT ( 'NONE', #27220 ) ;
#329 = CARTESIAN_POINT ( 'NONE',  ( -2.217375791810000329, 1495.290970025190290, 217.2501089269190118 ) ) ;
#330 = DIRECTION ( 'NONE',  ( -0.4978433412588676998, 0.000000000000000000, 0.8672669759446663962 ) ) ;
#332 = CARTESIAN_POINT ( 'NONE',  ( -0.6694169535389160597, 1457.182704574260015, 219.7360533319789795 ) ) ;
#331 = FACE_OUTER_BOUND ( 'NONE', #57581, .T. ) ;
#333 = CARTESIAN_POINT ( 'NONE',  ( 23.36041073559999859, 1411.089115351430110, 212.3712601659579775 ) ) ;
#334 = CARTESIAN_POINT ( 'NONE',  ( 4.215774578864469824, 1425.101385327330036, 185.2788908656129934 ) ) ;
#335 = CARTESIAN_POINT ( 'NONE',  ( -2.852637967456935986, 1419.721280333027380, 186.1746705150881098 ) ) ;
#336 = CARTESIAN_POINT ( 'NONE',  ( 7.206186347910000123, 1424.944465238209887, 212.8420735846389960 ) ) ;
#337 = CARTESIAN_POINT ( 'NONE',  ( -9.573037224950001089, 1423.427965722019962, 192.3355728592989919 ) ) ;
#339 = CARTESIAN_POINT ( 'NONE',  ( -5.441672317485815036, 1511.126521620285303, 201.4186169187619839 ) ) ;
#338 = B_SPLINE_CURVE_WITH_KNOTS ( 'NONE', 3,
 ( #14649, #33638, #59986, #52681 ),
 .UNSPECIFIED., .F., .F.,
 ( 4, 4 ),
 ( 0.000000000000000000, 0.0002960034161023847852 ),
 .UNSPECIFIED. ) ;
#340 = CARTESIAN_POINT ( 'NONE',  ( 2.852330403769999911, 1449.230534335530137, 183.5545985393980004 ) ) ;
#341 = PRESENTATION_LAYER_ASSIGNMENT (  '', '', ( #48608 ) ) ;
#342 = CARTESIAN_POINT ( 'NONE',  ( 9.369782510130001185, 1366.497526915280105, 207.6218459616989946 ) ) ;
#344 = ORIENTED_EDGE ( 'NONE', *, *, #61935, .F. ) ;
#343 = CARTESIAN_POINT ( 'NONE',  ( -4.951136445669599511E-10, 1417.070352045260051, 236.6937895817889910 ) ) ;
#345 = VERTEX_POINT ( 'NONE', #33388 ) ;
#346 = CARTESIAN_POINT ( 'NONE',  ( -41.48252549709999926, 1444.135617533290088, 136.5500651578979898 ) ) ;
#347 = DIRECTION ( 'NONE',  ( 0.000000000000000000, 1.000000000000000000, 0.000000000000000000 ) ) ;
#348 = CARTESIAN_POINT ( 'NONE',  ( -0.4691143273430000149, 1471.436294014529949, 269.3346704442980126 ) ) ;
#349 = CARTESIAN_POINT ( 'NONE',  ( 12.17607342826484818, 1434.037890756064598, 147.4852139652959693 ) ) ;
#350 = CARTESIAN_POINT ( 'NONE',  ( -113.4000000000000057, 1358.631207110790001, 311.1659210709989907 ) ) ;
#351 = CARTESIAN_POINT ( 'NONE',  ( 20.46339790889999932, 1475.513060387329915, 205.2504343647379983 ) ) ;
#352 = ADVANCED_FACE ( 'NONE', ( #86566 ), #108998, .T. ) ;
#353 = CARTESIAN_POINT ( 'NONE',  ( -8.173822499230000815, 1384.405547763340110, 199.6789892872290011 ) ) ;
#354 = CARTESIAN_POINT ( 'NONE',  ( 22.51991254300000023, 1410.619212212730190, 206.2037069855880134 ) ) ;
#355 = CARTESIAN_POINT ( 'NONE',  ( -20.80119636470000088, 1475.513060387329915, 204.3591166435880098 ) ) ;
#356 = CARTESIAN_POINT ( 'NONE',  ( 4.911313360425503483, 1370.788543751794350, 208.3718459617010978 ) ) ;
#357 = CARTESIAN_POINT ( 'NONE',  ( -5.603383157293649656E-09, 1406.911841289329914, 196.1218459609980300 ) ) ;
#358 = CARTESIAN_POINT ( 'NONE',  ( -12.11929752427059981, 1407.056436474629891, 267.1741674207860342 ) ) ;
#359 = EDGE_CURVE ( 'NONE', #10483, #4434, #57345, .T. ) ;
#360 = CARTESIAN_POINT ( 'NONE',  ( -13.80543509878039998, 1434.979598264029846, 148.5369193816260065 ) ) ;
#361 = EDGE_LOOP ( 'NONE', ( #97319, #80641, #79673, #74910 ) ) ;
#362 = DIRECTION ( 'NONE',  ( 1.836970198721029688E-16, 1.000000000000000000, -2.953460612019999929E-19 ) ) ;
#363 = CARTESIAN_POINT ( 'NONE',  ( 13.57336059360000036, 1443.191372133680034, 188.8849899699980028 ) ) ;
#364 = EDGE_LOOP ( 'NONE', ( #86550, #29612, #108325, #100325 ) ) ;
#365 = VERTEX_POINT ( 'NONE', #20997 ) ;
#366 = EDGE_CURVE ( 'NONE', #43369, #37055, #92016, .T. ) ;
#367 = AXIS2_PLACEMENT_3D ( 'NONE', #81942, #5812, #24233 ) ;
#368 = CARTESIAN_POINT ( 'NONE',  ( 4.479677203900762628, 1422.012945122907468, 183.9385808951501531 ) ) ;
#369 = CARTESIAN_POINT ( 'NONE',  ( 3.034145577506000446, 1440.440283345010130, 157.2495443575080003 ) ) ;
#370 = CARTESIAN_POINT ( 'NONE',  ( -1.703779643355000095, 1517.057265928030120, 213.1670284501570052 ) ) ;
#371 = CARTESIAN_POINT ( 'NONE',  ( -18.11868862529999902, 1485.487861948229920, 188.9570397301980051 ) ) ;
#372 = EDGE_CURVE ( 'NONE', #74254, #52548, #25231, .T. ) ;
#373 = FACE_OUTER_BOUND ( 'NONE', #57009, .T. ) ;
#374 = ORIENTED_EDGE ( 'NONE', *, *, #31699, .T. ) ;
#375 = CARTESIAN_POINT ( 'NONE',  ( -109.5441724410000006, 1374.437034645689891, 304.2218460466590386 ) ) ;
#376 =( BOUNDED_CURVE ( )  B_SPLINE_CURVE ( 3, ( #102045, #83062, #101486, #40501 ),
 .UNSPECIFIED., .F., .T. ) 
 B_SPLINE_CURVE_WITH_KNOTS ( ( 4, 4 ),
 ( 4.045555810179484624, 4.691360937121570096 ),
 .UNSPECIFIED. ) 
 CURVE ( )  GEOMETRIC_REPRESENTATION_ITEM ( )  RATIONAL_B_SPLINE_CURVE ( ( 1.000000000000000000, 0.9655455809096770148, 0.9655455809096770148, 1.000000000000000000 ) ) 
 REPRESENTATION_ITEM ( '' )  );
#377 = CARTESIAN_POINT ( 'NONE',  ( -3.070761075385165295, 1457.085219852218870, 218.1263196974262826 ) ) ;
#378 = CARTESIAN_POINT ( 'NONE',  ( -3.264778817514999876, 1516.727068157269969, 204.1245957781970048 ) ) ;
#379 = AXIS2_PLACEMENT_3D ( 'NONE', #95016, #67622, #7691 ) ;
#380 = CARTESIAN_POINT ( 'NONE',  ( -29.75011777940000002, 1509.993906963430163, 208.5595589157580036 ) ) ;
#381 = CARTESIAN_POINT ( 'NONE',  ( -1.569161292555000031, 1517.051704408389924, 216.8444262845069943 ) ) ;
#382 = CARTESIAN_POINT ( 'NONE',  ( -39.58883837791880467, 1384.581576029320104, 212.5204386266630081 ) ) ;
#383 = CARTESIAN_POINT ( 'NONE',  ( -1.344035116579999967, 1408.775599479229868, 195.0461770646979858 ) ) ;
#384 = CARTESIAN_POINT ( 'NONE',  ( -26.58019104509060071, 1469.327027323300172, 208.7773797362419828 ) ) ;
#386 = ORIENTED_EDGE ( 'NONE', *, *, #99268, .F. ) ;
#385 = CARTESIAN_POINT ( 'NONE',  ( 15.37090799315269152, 1506.446781340675443, 193.3909299311295626 ) ) ;
#387 = CARTESIAN_POINT ( 'NONE',  ( -27.41515663979030037, 1488.740012749160087, 208.8186931342820003 ) ) ;
#388 = CARTESIAN_POINT ( 'NONE',  ( 26.30775428189999943, 1469.245646012430143, 210.8538279144680132 ) ) ;
#389 = CARTESIAN_POINT ( 'NONE',  ( -36.13018326403506109, 1379.645813938799392, 224.1534624346936937 ) ) ;
#390 = CARTESIAN_POINT ( 'NONE',  ( 10.73298406322840037, 1460.408024784029976, 207.0975327187530013 ) ) ;
#391 = CARTESIAN_POINT ( 'NONE',  ( -23.95553108059999659, 1435.340102472350054, 136.9960523771979979 ) ) ;
#392 = ADVANCED_FACE ( 'NONE', ( #11528 ), #84870, .F. ) ;
#393 = CARTESIAN_POINT ( 'NONE',  ( 0.7576635334400020350, 1516.855632454399938, 211.9899581013969794 ) ) ;
#394 = TOROIDAL_SURFACE ( 'NONE', #71885, 30.13701971169416538, 3.000000000000000000 ) ;
#395 = CARTESIAN_POINT ( 'NONE',  ( -68.60472032309999690, 1379.747634528509707, 279.7221279746590312 ) ) ;
#396 = CARTESIAN_POINT ( 'NONE',  ( -18.69110324289999880, 1444.867398023490068, 206.3373603049990095 ) ) ;
#397 = CARTESIAN_POINT ( 'NONE',  ( -29.67375955050042791, 1525.697946996596102, 221.2718133379099186 ) ) ;
#398 = CARTESIAN_POINT ( 'NONE',  ( -2.881325412095000260, 1517.003078582959688, 208.0029426616869728 ) ) ;
#399 = EDGE_CURVE ( 'NONE', #104547, #81525, #8616, .T. ) ;
#400 = ORIENTED_EDGE ( 'NONE', *, *, #22203, .T. ) ;
#401 = DIRECTION ( 'NONE',  ( -0.03489949670255338560, 0.9993908270190677845, 2.284588940413689109E-07 ) ) ;
#402 = CARTESIAN_POINT ( 'NONE',  ( 5.375553136205760474, 1441.026369937100071, 154.8319413496199957 ) ) ;
#403 = CIRCLE ( 'NONE', #27160, 5.868098490439995985 ) ;
#404 = CARTESIAN_POINT ( 'NONE',  ( -73.55923423229999969, 1384.652831667379814, 298.9494481685590017 ) ) ;
#405 = ORIENTED_EDGE ( 'NONE', *, *, #65155, .F. ) ;
#406 = CARTESIAN_POINT ( 'NONE',  ( -13.74298021802130165, 1385.299105108359981, 219.1768037944160028 ) ) ;
#407 = CARTESIAN_POINT ( 'NONE',  ( -10.75057650454519909, 1492.402834311169954, 203.1666067258980206 ) ) ;
#408 = CARTESIAN_POINT ( 'NONE',  ( 12.69127487099669871, 1434.626206151899851, 149.6849692847659981 ) ) ;
#409 = CARTESIAN_POINT ( 'NONE',  ( 14.76180801577280022, 1459.302556161789880, 230.0031883768110106 ) ) ;
#410 = CARTESIAN_POINT ( 'NONE',  ( -21.86081811034360101, 1508.398734063270012, 226.4470915494329972 ) ) ;
#411 = CARTESIAN_POINT ( 'NONE',  ( -33.93019615848938741, 1501.977400791986611, 220.5829544587966211 ) ) ;
#412 = DIRECTION ( 'NONE',  ( -0.9999999999999995559, -4.156278225545078260E-11, 3.325661287725353434E-08 ) ) ;
#413 = CARTESIAN_POINT ( 'NONE',  ( -6.954065720117950100, 1517.051704408389924, 183.5505540514350002 ) ) ;
#415 = CARTESIAN_POINT ( 'NONE',  ( -3.619432601040000197, 1421.014464036429899, 186.0219392937979990 ) ) ;
#414 = CARTESIAN_POINT ( 'NONE',  ( -7.325541825264999751, 1516.710692850270107, 214.1269169785269924 ) ) ;
#416 = CARTESIAN_POINT ( 'NONE',  ( 20.30888173789999840, 1509.664622709230116, 187.3912422546979997 ) ) ;
#417 = CARTESIAN_POINT ( 'NONE',  ( -3.259729335964999919, 1517.119374999550018, 216.4589997383470177 ) ) ;
#418 = ORIENTED_EDGE ( 'NONE', *, *, #83682, .T. ) ;
#419 = CARTESIAN_POINT ( 'NONE',  ( -12.45665494490000214, 1416.827520077930103, 194.7672771341979967 ) ) ;
#420 = CARTESIAN_POINT ( 'NONE',  ( -16.94440841599999814, 1420.377411313550056, 203.4608118218089885 ) ) ;
#421 = ORIENTED_EDGE ( 'NONE', *, *, #109564, .F. ) ;
#422 = CARTESIAN_POINT ( 'NONE',  ( 3.316185754920000228, 1421.597412442629775, 183.5076398005980138 ) ) ;
#423 = B_SPLINE_CURVE_WITH_KNOTS ( 'NONE', 3,
 ( #95450, #45072, #95995, #54035, #1393, #107007, #19264, #35533, #28242, #53467, #78091, #854, #10331, #70288 ),
 .UNSPECIFIED., .F., .F.,
 ( 4, 2, 1, 1, 1, 1, 2, 2, 4 ),
 ( 0.000000000000000000, 0.2500000000014274693, 0.3750000000021411761, 0.4375000000024389935, 0.4687500000025079938, 0.4843750000025635605, 0.4921875000025116020, 0.5000000000024596991, 1.000000000000000000 ),
 .UNSPECIFIED. ) ;
#424 = CARTESIAN_POINT ( 'NONE',  ( -109.1307141485102790, 1384.906036703127711, 311.2647582669765711 ) ) ;
#425 = CARTESIAN_POINT ( 'NONE',  ( 2.570812331889315683, 1525.317349363550647, 176.7848501982247740 ) ) ;
#426 = CARTESIAN_POINT ( 'NONE',  ( 1275.711986934499919, 50.13405481564039690, 10006.43705117350146 ) ) ;
#427 = DIRECTION ( 'NONE',  ( -0.6736849260863839728, 0.000000000000000000, 0.7390186874254150995 ) ) ;
#428 = DIRECTION ( 'NONE',  ( -1.755985294532469921E-16, 1.000000000000000000, -1.338183447452831989E-16 ) ) ;
#429 = CARTESIAN_POINT ( 'NONE',  ( 18.88067404609999755, 1416.254459047329874, 210.2603107721379843 ) ) ;
#430 = CARTESIAN_POINT ( 'NONE',  ( -9.724834716106559089E-16, 1374.031200045389824, 209.1218459616989946 ) ) ;
#431 = CARTESIAN_POINT ( 'NONE',  ( 16.66231036550702882, 1523.604703353109699, 180.4882076302513383 ) ) ;
#432 = DIRECTION ( 'NONE',  ( -0.9417419115949053898, 0.3363363969979660806, 0.000000000000000000 ) ) ;
#433 = CARTESIAN_POINT ( 'NONE',  ( 26.36916589390109777, 1446.546730984839769, 137.7167331325649968 ) ) ;
#435 = CARTESIAN_POINT ( 'NONE',  ( -5.015825127099213354, 1391.761757684846771, 203.5511880675617249 ) ) ;
#434 = CARTESIAN_POINT ( 'NONE',  ( -13.41341432257899946, 1418.544055057069727, 200.5656092512240036 ) ) ;
#436 = CARTESIAN_POINT ( 'NONE',  ( 10.91311011200522962, 1428.352194749460068, 150.6639344388404140 ) ) ;
#437 = VERTEX_POINT ( 'NONE', #42792 ) ;
#438 = CARTESIAN_POINT ( 'NONE',  ( 14.25731394439999988, 1435.139839336880186, 149.2707523579979920 ) ) ;
#439 = CARTESIAN_POINT ( 'NONE',  ( 25.70326353240000117, 1469.149937121330140, 207.3826394511280000 ) ) ;
#440 = CARTESIAN_POINT ( 'NONE',  ( -29.19056928059999834, 1509.932417528530095, 211.8176115312480192 ) ) ;
#441 = CARTESIAN_POINT ( 'NONE',  ( 7.731075332760467766, 1410.555903148826246, 187.4988090489762271 ) ) ;
#442 = CARTESIAN_POINT ( 'NONE',  ( 0.000000000000000000, 1523.382868172864164, 209.1218459616979999 ) ) ;
#443 = CARTESIAN_POINT ( 'NONE',  ( 3.439855069772169809E-11, 1452.913060387330006, 150.8032249182200246 ) ) ;
#444 = CARTESIAN_POINT ( 'NONE',  ( -9.638115897704999213, 1520.551704408390151, 203.7504991310570119 ) ) ;
#445 = CARTESIAN_POINT ( 'NONE',  ( 12.98226561589999939, 1414.913060387329779, 198.3280246956980193 ) ) ;
#446 = CARTESIAN_POINT ( 'NONE',  ( -54.30401535559919779, 1383.804998114640057, 270.0689160511349769 ) ) ;
#447 = CARTESIAN_POINT ( 'NONE',  ( -19.53786426059057746, 1512.187213306747481, 181.5239794925695946 ) ) ;
#448 = CARTESIAN_POINT ( 'NONE',  ( -27.06966532493517974, 1508.822569575641182, 212.0394344631261561 ) ) ;
#449 = CARTESIAN_POINT ( 'NONE',  ( -2.759740495412019712, 1516.551695078709827, 201.4123589199890034 ) ) ;
#451 = EDGE_LOOP ( 'NONE', ( #81291, #94235, #88373, #80457, #8593 ) ) ;
#450 = CARTESIAN_POINT ( 'NONE',  ( 10.56937681823290021, 1452.418559324240050, 209.1099374865879952 ) ) ;
#452 = CARTESIAN_POINT ( 'NONE',  ( -1.547463840030000037, 1414.913060387329779, 225.9340782259980074 ) ) ;
#453 = CARTESIAN_POINT ( 'NONE',  ( -53.45887188369999876, 1384.635297440300064, 230.7554238970589893 ) ) ;
#454 = CARTESIAN_POINT ( 'NONE',  ( -16.19086242769280304, 1409.478452467050147, 225.0103265570539861 ) ) ;
#455 = ORIENTED_EDGE ( 'NONE', *, *, #105774, .T. ) ;
#456 = EDGE_LOOP ( 'NONE', ( #45426, #15333, #70007, #61987 ) ) ;
#457 = LINE ( 'NONE', #76585, #6239 ) ;
#458 = FACE_OUTER_BOUND ( 'NONE', #93445, .T. ) ;
#459 = CARTESIAN_POINT ( 'NONE',  ( 36.82437600794989407, 1437.810818275439942, 136.5532457654989855 ) ) ;
#461 = CARTESIAN_POINT ( 'NONE',  ( 2.470955845399090300, 1523.580203803270933, 175.3687159542604377 ) ) ;
#460 = CARTESIAN_POINT ( 'NONE',  ( 19.64184507190000062, 1452.819461535530081, 208.8935671266810061 ) ) ;
#462 = CARTESIAN_POINT ( 'NONE',  ( 11.76667485211559949, 1479.372979666780111, 208.7507148262919827 ) ) ;
#463 = CARTESIAN_POINT ( 'NONE',  ( -108.1525126060000019, 1382.602476773729904, 297.8175945742589761 ) ) ;
#464 = CARTESIAN_POINT ( 'NONE',  ( -11.83623787450240528, 1435.250172798539779, 151.2634934636774346 ) ) ;
#465 = CARTESIAN_POINT ( 'NONE',  ( -8.752237007995399054, 1384.883920018590061, 220.6821560429810063 ) ) ;
#466 = CARTESIAN_POINT ( 'NONE',  ( 2.320227349930000127, 1408.994084511829897, 187.0163958760979881 ) ) ;
#467 = CARTESIAN_POINT ( 'NONE',  ( 1.374098705546139998, 1508.999826499959909, 179.4761476500559922 ) ) ;
#468 = CARTESIAN_POINT ( 'NONE',  ( -11.04138758999999936, 1437.532134338300011, 152.0929086130979897 ) ) ;
#469 = LINE ( 'NONE', #52518, #42544 ) ;
#470 = CARTESIAN_POINT ( 'NONE',  ( -8.755578957433581166, 1424.773583938259890, 204.8410018134340191 ) ) ;
#471 = AXIS2_PLACEMENT_3D ( 'NONE', #413, #34530, #58646 ) ;
#472 = CARTESIAN_POINT ( 'NONE',  ( 11.86716023049999968, 1432.353341358199941, 147.6509521729980179 ) ) ;
#473 = CARTESIAN_POINT ( 'NONE',  ( 0.6083087506080000484, 1465.081050579229895, 236.9567715190979982 ) ) ;
#474 = ORIENTED_EDGE ( 'NONE', *, *, #24074, .F. ) ;
#475 = CARTESIAN_POINT ( 'NONE',  ( 20.33642612138580219, 1475.138353456469986, 218.0161241308549904 ) ) ;
#476 = CARTESIAN_POINT ( 'NONE',  ( -38.87545285710000087, 1457.142118430129813, 270.1626018656980364 ) ) ;
#477 = CARTESIAN_POINT ( 'NONE',  ( -23.74108753817469974, 1436.296634041249945, 212.5883363871789982 ) ) ;
#478 = CARTESIAN_POINT ( 'NONE',  ( 16.19492459430000153, 1409.478599616029896, 224.1775087544979783 ) ) ;
#479 = DIRECTION ( 'NONE',  ( -1.699538841806929935E-33, 1.000000000000000000, -1.698192320643030073E-16 ) ) ;
#480 = CARTESIAN_POINT ( 'NONE',  ( -1.371587748774959908E-10, 1469.646809014170003, 253.0669417465539652 ) ) ;
#481 = EDGE_CURVE ( 'NONE', #82285, #55990, #44994, .T. ) ;
#482 = CARTESIAN_POINT ( 'NONE',  ( -19.88572122277579979, 1484.728771715989751, 191.0592865161910083 ) ) ;
#483 = CARTESIAN_POINT ( 'NONE',  ( -0.7692391029760000665, 1415.628674266529742, 227.3871686175980074 ) ) ;
#484 = CARTESIAN_POINT ( 'NONE',  ( -9.817298943409999978, 1418.814616626229963, 230.3607498785979999 ) ) ;
#485 = CARTESIAN_POINT ( 'NONE',  ( -2.314955559389999973, 1476.586284849689946, 199.0068122257989955 ) ) ;
#486 = CARTESIAN_POINT ( 'NONE',  ( -105.7100346900000005, 1391.009939533860006, 306.5104643349590106 ) ) ;
#487 = CARTESIAN_POINT ( 'NONE',  ( -0.05082592258669504232, 1486.215346117376839, 181.8157142799529993 ) ) ;
#488 = CARTESIAN_POINT ( 'NONE',  ( 1.748848150595841977, 1360.440694539930064, 210.6218459616991936 ) ) ;
#489 = CARTESIAN_POINT ( 'NONE',  ( -45.95836323909989574, 1437.680972842699703, 268.2109776636490324 ) ) ;
#490 = DIRECTION ( 'NONE',  ( -0.000000000000000000, -1.000000000000000000, -0.000000000000000000 ) ) ;
#491 = CARTESIAN_POINT ( 'NONE',  ( -7.514967970819999898, 1426.327999703259820, 205.9160403778789998 ) ) ;
#492 = ORIENTED_EDGE ( 'NONE', *, *, #6899, .T. ) ;
#493 = CARTESIAN_POINT ( 'NONE',  ( 6.949703334655000120, 1517.130100026000036, 209.8609679372960102 ) ) ;
#494 = CARTESIAN_POINT ( 'NONE',  ( -2.478898695439999855, 1433.170136607830045, 157.5403501404979920 ) ) ;
#495 = CARTESIAN_POINT ( 'NONE',  ( -7.863671303257509848, 1471.291298022706087, 215.5245834466820440 ) ) ;
#496 = CARTESIAN_POINT ( 'NONE',  ( 7.537606959944939788, 1425.724147855899901, 212.1987702218239917 ) ) ;
#497 = CARTESIAN_POINT ( 'NONE',  ( -26.35325170641180037, 1451.992872967969788, 135.0462968633300136 ) ) ;
#498 = EDGE_LOOP ( 'NONE', ( #7346, #75123, #33311, #49048 ) ) ;
#499 = EDGE_CURVE ( 'NONE', #98535, #40166, #189, .T. ) ;
#500 = CARTESIAN_POINT ( 'NONE',  ( 25.99468486090000141, 1435.718168598109969, 225.6861378082980139 ) ) ;
#502 = CARTESIAN_POINT ( 'NONE',  ( -14.94819997777649867, 1513.870294663139930, 223.8775307694120045 ) ) ;
#501 = CARTESIAN_POINT ( 'NONE',  ( -2.478666945488134932, 1524.659148609483054, 175.7709333987998548 ) ) ;
#503 = CARTESIAN_POINT ( 'NONE',  ( 1.205243432004479809, 1487.387165744484264, 219.8907050796039755 ) ) ;
#504 = CARTESIAN_POINT ( 'NONE',  ( -2.479184146860000096E-08, 1422.360590008429881, 211.7205299278780046 ) ) ;
#505 = EDGE_CURVE ( 'NONE', #59255, #100495, #12716, .T. ) ;
#506 = CARTESIAN_POINT ( 'NONE',  ( 34.18677586421181758, 1522.382868172863937, 198.4504086008745389 ) ) ;
#507 = CARTESIAN_POINT ( 'NONE',  ( -9.786977751178733698, 1521.951704408389787, 191.2793932888540951 ) ) ;
#508 = VERTEX_POINT ( 'NONE', #77503 ) ;
#509 = CARTESIAN_POINT ( 'NONE',  ( -4.218478457446350305, 1409.928425769410069, 270.0721727225960080 ) ) ;
#510 = CARTESIAN_POINT ( 'NONE',  ( -6.952166420425000659, 1517.213554313520035, 207.4130983078469797 ) ) ;
#511 = CARTESIAN_POINT ( 'NONE',  ( 13.49846100598660037, 1421.214292344940077, 231.0218097068720056 ) ) ;
#512 = DIRECTION ( 'NONE',  ( -1.964544591288419982E-14, -1.000000000000000000, 8.043425993822650894E-15 ) ) ;
#514 = ORIENTED_EDGE ( 'NONE', *, *, #3680, .F. ) ;
#513 = CARTESIAN_POINT ( 'NONE',  ( -2.724500461543110319, 1367.224846223802842, 209.6218459617148824 ) ) ;
#515 = ORIENTED_EDGE ( 'NONE', *, *, #31765, .T. ) ;
#516 = CARTESIAN_POINT ( 'NONE',  ( -22.79252858209050103, 1409.718716787750054, 209.5234536894689938 ) ) ;
#517 = CARTESIAN_POINT ( 'NONE',  ( -0.6532819063196209086, 1409.103086040569906, 185.7260927124030161 ) ) ;
#518 = DIRECTION ( 'NONE',  ( 0.000000000000000000, 0.000000000000000000, 1.000000000000000000 ) ) ;
#519 = PLANE ( 'NONE',  #38439 ) ;
#520 = CARTESIAN_POINT ( 'NONE',  ( -19.03551611759530005, 1443.980599388390146, 194.2018241821600100 ) ) ;
#521 = CARTESIAN_POINT ( 'NONE',  ( -19.69872028629999861, 1420.831966503530111, 222.5429556983980035 ) ) ;
#522 = CARTESIAN_POINT ( 'NONE',  ( 36.52219476372820850, 1461.495432610050102, 269.2158760797449872 ) ) ;
#523 = CARTESIAN_POINT ( 'NONE',  ( -15.46700379407589843, 1461.188231737419756, 228.6959062608830209 ) ) ;
#524 = CARTESIAN_POINT ( 'NONE',  ( -2.907264515414449857, 1451.960119877520128, 184.7556101994359778 ) ) ;
#525 = CARTESIAN_POINT ( 'NONE',  ( -1.715361130375000043, 1516.743010792419909, 205.6766444437269854 ) ) ;
#526 = EDGE_CURVE ( 'NONE', #91726, #23648, #37737, .T. ) ;
#527 = ORIENTED_EDGE ( 'NONE', *, *, #22644, .F. ) ;
#528 = CARTESIAN_POINT ( 'NONE',  ( -11.74481771089999960, 1433.726929579510170, 150.9290601731980246 ) ) ;
#529 = CARTESIAN_POINT ( 'NONE',  ( -0.1150915766366530091, 1444.816874904579890, 199.0635159857669976 ) ) ;
#530 = DIRECTION ( 'NONE',  ( 0.03782478994198348876, 0.9992229352747146187, 0.01108200734653209431 ) ) ;
#531 = ORIENTED_EDGE ( 'NONE', *, *, #98190, .F. ) ;
#532 = DIRECTION ( 'NONE',  ( 0.9858563016923833633, 0.000000000000000000, 0.1675928173085483863 ) ) ;
#533 = CARTESIAN_POINT ( 'NONE',  ( 26.74533639559809828, 1450.888433640950097, 136.4325763836939984 ) ) ;
#534 = CARTESIAN_POINT ( 'NONE',  ( -3.384752634116700243, 1508.551704408389924, 213.9439043168609942 ) ) ;
#535 = CARTESIAN_POINT ( 'NONE',  ( -8.746878246584900021E-16, 1386.598172472869919, 199.6218459572590120 ) ) ;
#536 = CARTESIAN_POINT ( 'NONE',  ( -9.252564866275420741, 1386.194685219555595, 218.4639695156267578 ) ) ;
#537 = CARTESIAN_POINT ( 'NONE',  ( 18.05634065199999938, 1410.467697827129996, 193.5994654289980019 ) ) ;
#538 = CARTESIAN_POINT ( 'NONE',  ( -3.774700670050000095, 1496.332844194289919, 198.4120365050989960 ) ) ;
#539 = CARTESIAN_POINT ( 'NONE',  ( 5.158526775084939509, 1409.093200111750093, 187.9627302490250145 ) ) ;
#541 = CARTESIAN_POINT ( 'NONE',  ( -22.82877908214457463, 1432.437248394402786, 215.4934721305570520 ) ) ;
#540 = CARTESIAN_POINT ( 'NONE',  ( -1.514784269649715576, 1443.601484486217942, 218.3342104795610510 ) ) ;
#542 = CARTESIAN_POINT ( 'NONE',  ( 1.324223389204969958, 1452.129545857950006, 183.4093034293840105 ) ) ;
#543 = LINE ( 'NONE', #53148, #67817 ) ;
#544 = CARTESIAN_POINT ( 'NONE',  ( -9.786751275049999421, 1380.128435987210196, 216.7642765186190275 ) ) ;
#545 = CARTESIAN_POINT ( 'NONE',  ( 7.912312578985590150, 1418.799544019259883, 233.2448588504591669 ) ) ;
#546 = ORIENTED_EDGE ( 'NONE', *, *, #47982, .F. ) ;
#547 = CARTESIAN_POINT ( 'NONE',  ( 12.66409680412649941, 1415.935475482089942, 221.7747898017080104 ) ) ;
#548 = FACE_OUTER_BOUND ( 'NONE', #82906, .T. ) ;
#549 = FACE_OUTER_BOUND ( 'NONE', #106760, .T. ) ;
#550 = CARTESIAN_POINT ( 'NONE',  ( -13.17267676139999999, 1389.960074679450145, 205.5617118964289887 ) ) ;
#551 = CARTESIAN_POINT ( 'NONE',  ( 9.575940986468468807, 1427.729431014379998, 211.3625234817539820 ) ) ;
#552 = CARTESIAN_POINT ( 'NONE',  ( 1.154719254338330447, 1421.357514871522653, 193.7585151656728044 ) ) ;
#553 = CARTESIAN_POINT ( 'NONE',  ( 13.04266739719999890, 1417.449502458830011, 221.6520488708979713 ) ) ;
#554 = DIRECTION ( 'NONE',  ( -0.9942586961433764747, 0.000000000000000000, -0.1070030146457237041 ) ) ;
#555 = CARTESIAN_POINT ( 'NONE',  ( -9.252874484757731111, 1477.963449144112474, 214.0067384189093218 ) ) ;
#556 = CARTESIAN_POINT ( 'NONE',  ( 11.74567502190000035, 1433.530944218069862, 150.8654047345980018 ) ) ;
#557 = CARTESIAN_POINT ( 'NONE',  ( 2.984513020910000147, 1453.913060387330006, 209.1218459616979999 ) ) ;
#558 = CARTESIAN_POINT ( 'NONE',  ( -11.02797255089159911, 1462.256692482700146, 209.5173753044250020 ) ) ;
#559 = CARTESIAN_POINT ( 'NONE',  ( 18.24211828920000045, 1431.096497597789948, 200.8001355623590030 ) ) ;
#560 = CARTESIAN_POINT ( 'NONE',  ( 10.45726464265210076, 1420.924558883679993, 198.4227429697920115 ) ) ;
#561 = CARTESIAN_POINT ( 'NONE',  ( 4.780270616392929384, 1467.625973390280024, 217.8721612978610267 ) ) ;
#562 = CARTESIAN_POINT ( 'NONE',  ( 22.70509004431190192, 1409.705939603270053, 209.2982552845940063 ) ) ;
#563 = DIRECTION ( 'NONE',  ( 0.000000000000000000, 0.000000000000000000, 1.000000000000000000 ) ) ;
#564 = CARTESIAN_POINT ( 'NONE',  ( -15.28951669910000000, 1509.578191272730010, 236.7286881490979908 ) ) ;
#565 = CARTESIAN_POINT ( 'NONE',  ( 23.54254250440000007, 1430.351957799930005, 214.4849305350980160 ) ) ;
#566 = CARTESIAN_POINT ( 'NONE',  ( 0.3281250907512314741, 1477.756992672553451, 198.7115816712109506 ) ) ;
#567 = CARTESIAN_POINT ( 'NONE',  ( 26.16840185550843856, 1436.693591485223578, 136.8912855551424173 ) ) ;
#568 = CARTESIAN_POINT ( 'NONE',  ( -1.082449427729999858, 1515.225850744089939, 204.7966151436789914 ) ) ;
#569 = CARTESIAN_POINT ( 'NONE',  ( 17.42808535260000014, 1431.113060387329824, 216.7347523923079962 ) ) ;
#570 = CARTESIAN_POINT ( 'NONE',  ( -3.071477015947639888, 1470.850262397169899, 187.3986309147560121 ) ) ;
#571 = CARTESIAN_POINT ( 'NONE',  ( -3.254401441735000233, 1516.919782530640077, 213.1645757730269963 ) ) ;
#572 = CARTESIAN_POINT ( 'NONE',  ( -19.83550667398609946, 1418.664640197639983, 208.7685751368389901 ) ) ;
#573 = CARTESIAN_POINT ( 'NONE',  ( 0.1665927539581550099, 1482.335989075430234, 181.9940412649720258 ) ) ;
#575 = VERTEX_POINT ( 'NONE', #42240 ) ;
#574 = DIRECTION ( 'NONE',  ( -0.5412924984493711067, 0.1391731009598990432, -0.8292365640103210866 ) ) ;
#576 = CARTESIAN_POINT ( 'NONE',  ( -1.546869375780000055, 1416.835808399930102, 228.0212684633979734 ) ) ;
#577 = CARTESIAN_POINT ( 'NONE',  ( -16.90742456144258909, 1444.994950788469623, 162.4348202098878744 ) ) ;
#578 = DIRECTION ( 'NONE',  ( -0.000000000000000000, 1.836970198721029688E-16, 1.000000000000000000 ) ) ;
#579 = CARTESIAN_POINT ( 'NONE',  ( -35.35021333641900299, 1451.550776711729895, 134.0999999984329918 ) ) ;
#580 = CARTESIAN_POINT ( 'NONE',  ( -109.8949752469999908, 1384.902872212460125, 297.0284569597590121 ) ) ;
#581 = ORIENTED_EDGE ( 'NONE', *, *, #68778, .F. ) ;
#582 = CARTESIAN_POINT ( 'NONE',  ( -10.30263834680000024, 1471.732697784889979, 209.1299246244929861 ) ) ;
#583 = B_SPLINE_CURVE_WITH_KNOTS ( 'NONE', 3,
 ( #94797, #754, #35441, #77995 ),
 .UNSPECIFIED., .F., .F.,
 ( 4, 4 ),
 ( 0.000000000000000000, 1.000000000000000000 ),
 .UNSPECIFIED. ) ;
#584 = CARTESIAN_POINT ( 'NONE',  ( -13.93561471908700078, 1390.368461153759881, 210.8007146514599981 ) ) ;
#585 = FACE_OUTER_BOUND ( 'NONE', #42425, .T. ) ;
#586 = DIRECTION ( 'NONE',  ( -1.000000000000000000, 0.000000000000000000, 0.000000000000000000 ) ) ;
#587 = CARTESIAN_POINT ( 'NONE',  ( -3.138770468918330003, 1433.097189459889933, 217.7316335566559928 ) ) ;
#588 = CARTESIAN_POINT ( 'NONE',  ( -107.2899050854710055, 1379.886892357829993, 309.1794776302379546 ) ) ;
#589 = CARTESIAN_POINT ( 'NONE',  ( 1.842963721827329815, 1515.551704300040001, 212.9514659606769840 ) ) ;
#590 = CARTESIAN_POINT ( 'NONE',  ( -12.92544628329999945, 1379.594338187410131, 211.1425626820590082 ) ) ;
#591 = CARTESIAN_POINT ( 'NONE',  ( -11.31021147849999942, 1391.913060277239993, 206.0247873240190302 ) ) ;
#592 = CARTESIAN_POINT ( 'NONE',  ( -73.83470183118490127, 1385.130927357710107, 273.3978214202909953 ) ) ;
#593 = CARTESIAN_POINT ( 'NONE',  ( -9.878631019772029731, 1391.913060387289988, 214.6972032143189892 ) ) ;
#594 = CARTESIAN_POINT ( 'NONE',  ( 11.30421211722389963, 1422.134199828960163, 208.7798009037170175 ) ) ;
#595 = ORIENTED_EDGE ( 'NONE', *, *, #3501, .F. ) ;
#596 = CARTESIAN_POINT ( 'NONE',  ( 16.90809753623369360, 1442.831169986191526, 162.4344573440251338 ) ) ;
#598 = VERTEX_POINT ( 'NONE', #85321 ) ;
#597 = CARTESIAN_POINT ( 'NONE',  ( -7.271052316819549333, 1522.051704408389924, 225.3404165491008371 ) ) ;
#599 = CARTESIAN_POINT ( 'NONE',  ( 6.224950473385610472, 1466.920039123629977, 216.8753481341400118 ) ) ;
#600 = ORIENTED_EDGE ( 'NONE', *, *, #74040, .T. ) ;
#601 = CARTESIAN_POINT ( 'NONE',  ( 1.842962231260000028, 1515.064792882589927, 204.7923971856590128 ) ) ;
#602 = CARTESIAN_POINT ( 'NONE',  ( -7.406989585696536871, 1364.221058288796257, 209.6218459617148824 ) ) ;
#603 = CARTESIAN_POINT ( 'NONE',  ( -10.90040372089999998, 1492.525755917289871, 207.2558760794690045 ) ) ;
#604 = DIRECTION ( 'NONE',  ( -1.592428286118737079E-10, -0.9689480427665004836, 0.2472644139761486504 ) ) ;
#605 = DIRECTION ( 'NONE',  ( -1.000000000000000000, -6.997424008300000075E-18, -1.832339962680000039E-19 ) ) ;
#606 = CARTESIAN_POINT ( 'NONE',  ( 15.82611567847458289, 1431.600131786831980, 218.9583281995740833 ) ) ;
#607 = CARTESIAN_POINT ( 'NONE',  ( -5.385523200472070116, 1511.435001055929888, 200.4690698413500058 ) ) ;
#608 = CARTESIAN_POINT ( 'NONE',  ( 4.176540423850000572, 1446.483799824789912, 200.6257159222890039 ) ) ;
#609 = CARTESIAN_POINT ( 'NONE',  ( -20.15452302159999931, 1507.845791376729949, 228.9024215066979764 ) ) ;
#610 = CARTESIAN_POINT ( 'NONE',  ( -10.65892733151780369, 1368.068496973798574, 209.6218459617033432 ) ) ;
#611 = CARTESIAN_POINT ( 'NONE',  ( -3.558358605100000016, 1455.955982659790152, 200.3550966547389862 ) ) ;
#612 = CARTESIAN_POINT ( 'NONE',  ( -3.461995196814999787, 1516.906233342200039, 206.2559344154570056 ) ) ;
#613 = CARTESIAN_POINT ( 'NONE',  ( 4.220927954709999597, 1446.217199771959940, 167.4561886970979856 ) ) ;
#614 = CARTESIAN_POINT ( 'NONE',  ( -15.74187958907210039, 1412.794802208900137, 226.7867534266219991 ) ) ;
#615 = CARTESIAN_POINT ( 'NONE',  ( -2.487213358930000062, 1495.883017016489930, 197.0235130655990190 ) ) ;
#617 = ORIENTED_EDGE ( 'NONE', *, *, #44729, .F. ) ;
#616 = CARTESIAN_POINT ( 'NONE',  ( -2.182814748220000212, 1496.366357223990008, 220.5334820124990074 ) ) ;
#618 = CARTESIAN_POINT ( 'NONE',  ( -3.313501335607589748, 1397.551704408390151, 203.0565224509919915 ) ) ;
#619 = ORIENTED_EDGE ( 'NONE', *, *, #18010, .T. ) ;
#620 = ADVANCED_FACE ( 'NONE', ( #78041 ), #85891, .F. ) ;
#621 = LINE ( 'NONE', #33094, #954 ) ;
#622 = CARTESIAN_POINT ( 'NONE',  ( -21.91488071189999687, 1449.791133988690035, 197.9993651584979943 ) ) ;
#624 = CARTESIAN_POINT ( 'NONE',  ( 16.85667268330360002, 1410.729706438800122, 191.8820313785110159 ) ) ;
#623 = CARTESIAN_POINT ( 'NONE',  ( -11.54936350167399972, 1426.401857134930196, 130.8094922821749719 ) ) ;
#625 = CARTESIAN_POINT ( 'NONE',  ( -1.700706814495000163, 1516.923170579120097, 211.4225755968969906 ) ) ;
#626 = B_SPLINE_CURVE_WITH_KNOTS ( 'NONE', 3,
 ( #68362, #23563, #84575, #93517, #75649, #76185, #40921, #67801 ),
 .UNSPECIFIED., .F., .F.,
 ( 4, 2, 2, 4 ),
 ( 3.035766082959412415E-18, 0.001073044933456185606, 0.001609567400184306381, 0.002146089866912427591 ),
 .UNSPECIFIED. ) ;
#627 = CARTESIAN_POINT ( 'NONE',  ( -4.518180742295140181E-06, 1509.047264790930058, 179.1218459713510072 ) ) ;
#628 = B_SPLINE_CURVE_WITH_KNOTS ( 'NONE', 3,
 ( #92990, #23025, #91894, #57227, #91357, #49357, #48822, #7343, #24119, #83486, #42053, #109808, #82946 ),
 .UNSPECIFIED., .F., .F.,
 ( 4, 3, 3, 3, 4 ),
 ( -3.958900035302570064, -3.804518807040609740, -3.535848030339469705, -3.399392778577199792, -3.112795747787960199 ),
 .UNSPECIFIED. ) ;
#629 = CARTESIAN_POINT ( 'NONE',  ( -21.30047364560000034, 1471.312091222029949, 208.2102265936800336 ) ) ;
#630 = CARTESIAN_POINT ( 'NONE',  ( -41.56051824640000092, 1438.341700612089880, 261.5689736386979689 ) ) ;
#631 = CARTESIAN_POINT ( 'NONE',  ( 19.31522993011370204, 1509.613100981719981, 231.6083989249460160 ) ) ;
#632 = CARTESIAN_POINT ( 'NONE',  ( 3.052975896485000007, 1516.551704408390151, 217.1245693350269903 ) ) ;
#633 = EDGE_CURVE ( 'NONE', #14236, #26775, #48569, .T. ) ;
#634 = SHAPE_DEFINITION_REPRESENTATION ( #5341, #72299 ) ;
#635 = CARTESIAN_POINT ( 'NONE',  ( 4.789026039587930050, 1508.551704408389924, 212.5881120909519950 ) ) ;
#636 = CARTESIAN_POINT ( 'NONE',  ( -39.46926012269349826, 1440.456819381679907, 136.7723882296410238 ) ) ;
#637 = ORIENTED_EDGE ( 'NONE', *, *, #18509, .F. ) ;
#638 = CARTESIAN_POINT ( 'NONE',  ( 12.86231746777660057, 1396.538691440989851, 207.1246007041149824 ) ) ;
#639 = CARTESIAN_POINT ( 'NONE',  ( 9.326151436081950408, 1460.944241195969880, 206.0386860876060098 ) ) ;
#640 = CARTESIAN_POINT ( 'NONE',  ( -9.966727850805121136, 1439.480327375449860, 208.4309914983489875 ) ) ;
#641 = ORIENTED_EDGE ( 'NONE', *, *, #103472, .F. ) ;
#642 = VERTEX_POINT ( 'NONE', #25961 ) ;
#643 = CARTESIAN_POINT ( 'NONE',  ( -29.24222457024196586, 1509.934245987175927, 211.7448869334152164 ) ) ;
#644 = CARTESIAN_POINT ( 'NONE',  ( -9.298374131422571409, 1424.634617889919809, 149.7551454182870145 ) ) ;
#645 = ORIENTED_EDGE ( 'NONE', *, *, #26884, .F. ) ;
#646 = CARTESIAN_POINT ( 'NONE',  ( -1.116585105924089969E-07, 1397.914279478820163, 196.1218459578329885 ) ) ;
#647 = CARTESIAN_POINT ( 'NONE',  ( -11.16856291581570737, 1417.847332803086601, 198.5153517745319220 ) ) ;
#648 = FACE_OUTER_BOUND ( 'NONE', #91311, .T. ) ;
#649 = CARTESIAN_POINT ( 'NONE',  ( -4.656690245969999253, 1461.191637107629958, 234.3103256880980041 ) ) ;
#650 = LINE ( 'NONE', #52152, #84998 ) ;
#651 = CARTESIAN_POINT ( 'NONE',  ( 9.418151193910370367, 1451.571079816670135, 209.2450735257419865 ) ) ;
#652 = CARTESIAN_POINT ( 'NONE',  ( -113.4000000000000057, 1392.913060387289988, 304.2218459572590064 ) ) ;
#653 = CARTESIAN_POINT ( 'NONE',  ( -88.76367195209469685, 1384.833741781400022, 291.7667102089239961 ) ) ;
#654 = ORIENTED_EDGE ( 'NONE', *, *, #54816, .F. ) ;
#655 = CARTESIAN_POINT ( 'NONE',  ( -4.618119704395000191, 1516.706638732659940, 202.1845071865270143 ) ) ;
#656 = CARTESIAN_POINT ( 'NONE',  ( -6.556851034704999748, 1516.939568781210028, 209.1335575761840175 ) ) ;
#657 = ORIENTED_EDGE ( 'NONE', *, *, #45659, .F. ) ;
#658 = CARTESIAN_POINT ( 'NONE',  ( 11.73986278517180182, 1426.693600150729935, 144.3691362286979825 ) ) ;
#659 = CARTESIAN_POINT ( 'NONE',  ( 4.264166330254295367, 1511.427938673519748, 217.4025041547218109 ) ) ;
#660 = VERTEX_POINT ( 'NONE', #93714 ) ;
#661 = DIRECTION ( 'NONE',  ( 0.7067701421949666996, -0.03085961869104518474, 0.7067698706339636816 ) ) ;
#662 = CARTESIAN_POINT ( 'NONE',  ( 6.537718912151950335, 1429.433188304760051, 215.9971499089490123 ) ) ;
#663 = CARTESIAN_POINT ( 'NONE',  ( 9.406666111339999858, 1509.241548406330139, 236.7319732460980219 ) ) ;
#664 = CARTESIAN_POINT ( 'NONE',  ( -8.182145408407338394, 1490.196931670758431, 216.4137635874354828 ) ) ;
#665 = CARTESIAN_POINT ( 'NONE',  ( -5.256547791280000048, 1424.521933614530099, 186.2316258165979832 ) ) ;
#666 = CARTESIAN_POINT ( 'NONE',  ( 7.984655233845471045, 1410.580038844309911, 269.8705203775900259 ) ) ;
#667 = CARTESIAN_POINT ( 'NONE',  ( -0.4363688680027120181, 1517.051704408389924, 216.7663257121729998 ) ) ;
#668 = CARTESIAN_POINT ( 'NONE',  ( -8.211943818390000871, 1474.301007847190021, 202.7927141847590065 ) ) ;
#669 = CARTESIAN_POINT ( 'NONE',  ( -11.54583652347674416, 1410.690064926147897, 189.0055360890668510 ) ) ;
#670 = CARTESIAN_POINT ( 'NONE',  ( -18.79413418600000085, 1379.714553871910084, 209.1009770162550012 ) ) ;
#671 = VECTOR ( 'NONE', #63207, 1000.000000000000000 ) ;
#672 = CARTESIAN_POINT ( 'NONE',  ( 24.92729647353190003, 1464.542099455490188, 206.2188305520340066 ) ) ;
#674 = FACE_OUTER_BOUND ( 'NONE', #24207, .T. ) ;
#673 = FACE_OUTER_BOUND ( 'NONE', #12560, .T. ) ;
#675 = CARTESIAN_POINT ( 'NONE',  ( -5.010265762299249914, 1422.725625646132585, 184.8437789348542424 ) ) ;
#676 = CARTESIAN_POINT ( 'NONE',  ( -5.370514330159649852, 1422.356910281434239, 139.1416123588654727 ) ) ;
#677 = CARTESIAN_POINT ( 'NONE',  ( -19.73299507883049841, 1503.904988652430120, 218.6992329638289903 ) ) ;
#678 = ORIENTED_EDGE ( 'NONE', *, *, #80484, .T. ) ;
#679 = CARTESIAN_POINT ( 'NONE',  ( 18.07417247534460003, 1424.494734117629832, 224.1841365583740071 ) ) ;
#680 = CARTESIAN_POINT ( 'NONE',  ( -16.68062049856743201, 1524.382868172863937, 181.4122394607864521 ) ) ;
#681 = CARTESIAN_POINT ( 'NONE',  ( -2.959734820789013288, 1485.424150447127658, 182.8872198570792591 ) ) ;
#682 =( BOUNDED_CURVE ( )  B_SPLINE_CURVE ( 3, ( #67217, #42542, #1115, #52615 ),
 .UNSPECIFIED., .F., .F. ) 
 B_SPLINE_CURVE_WITH_KNOTS ( ( 4, 4 ),
 ( 2.436781329611985569, 3.141592653589793116 ),
 .UNSPECIFIED. ) 
 CURVE ( )  GEOMETRIC_REPRESENTATION_ITEM ( )  RATIONAL_B_SPLINE_CURVE ( ( 1.000000000000000000, 0.9590300661663091475, 0.9590300661663091475, 1.000000000000000000 ) ) 
 REPRESENTATION_ITEM ( '' )  );
#683 = CARTESIAN_POINT ( 'NONE',  ( -17.60627216660330063, 1410.895669502700230, 193.4350316886979897 ) ) ;
#685 = EDGE_LOOP ( 'NONE', ( #51444, #69652, #66163, #14641 ) ) ;
#684 = CARTESIAN_POINT ( 'NONE',  ( 0.4426438243888760060, 1515.147163425719782, 204.7945541343150069 ) ) ;
#686 = CARTESIAN_POINT ( 'NONE',  ( -8.604752758000000057, 1384.917533019219945, 199.8686412392590057 ) ) ;
#687 = CARTESIAN_POINT ( 'NONE',  ( -15.13342374508840038, 1507.606285602760181, 191.8462590464540085 ) ) ;
#688 = CARTESIAN_POINT ( 'NONE',  ( -11.83486911239999984, 1430.209948791529769, 149.5656396673979884 ) ) ;
#689 = CARTESIAN_POINT ( 'NONE',  ( 0.000000000000000000, 1405.413060387330006, 209.1218459616979999 ) ) ;
#690 = CARTESIAN_POINT ( 'NONE',  ( -10.98255251702510016, 1462.120311678340158, 210.0436777776439783 ) ) ;
#691 = CARTESIAN_POINT ( 'NONE',  ( 12.50000000000000000, 1384.913060387289988, 209.1218459572589836 ) ) ;
#692 = FACE_OUTER_BOUND ( 'NONE', #109949, .T. ) ;
#693 = CARTESIAN_POINT ( 'NONE',  ( -15.60002308836500085, 1512.080583811389943, 221.9287863060669963 ) ) ;
#694 = CARTESIAN_POINT ( 'NONE',  ( 2.737811238710000428, 1478.658245750390051, 201.8858327187489863 ) ) ;
#696 = CARTESIAN_POINT ( 'NONE',  ( -10.40955016854329962, 1480.514293831559826, 207.4814632850010128 ) ) ;
#695 = CARTESIAN_POINT ( 'NONE',  ( -20.11321007749999978, 1508.016902856529896, 228.9715373177980098 ) ) ;
#697 = CARTESIAN_POINT ( 'NONE',  ( -16.61466320086400117, 1459.965743753311926, 228.4923931122799843 ) ) ;
#698 = CARTESIAN_POINT ( 'NONE',  ( 7.708770007014999592, 1516.524310051880093, 206.8307984429870032 ) ) ;
#699 = CARTESIAN_POINT ( 'NONE',  ( 18.25484434299999847, 1409.004537368329920, 269.1701810006979940 ) ) ;
#700 = CARTESIAN_POINT ( 'NONE',  ( 0.2895775691657055395, 1465.119059868797649, 238.1348893659934163 ) ) ;
#701 = CARTESIAN_POINT ( 'NONE',  ( 19.27463171960000210, 1449.732551075340098, 192.4184640539980080 ) ) ;
#702 = CARTESIAN_POINT ( 'NONE',  ( 24.65284846709989708, 1440.998862877870124, 212.5088464049670165 ) ) ;
#703 = EDGE_CURVE ( 'NONE', #94689, #56179, #31918, .T. ) ;
#704 = CARTESIAN_POINT ( 'NONE',  ( 7.659302844740099481, 1423.043197802409850, 144.1531582648829897 ) ) ;
#705 = CARTESIAN_POINT ( 'NONE',  ( -40.27308333479999902, 1443.612076741559804, 137.1163319701979901 ) ) ;
#706 = CARTESIAN_POINT ( 'NONE',  ( -10.16044903509999919, 1409.267871086030027, 197.9277695215979804 ) ) ;
#707 = CARTESIAN_POINT ( 'NONE',  ( -14.80403897610000108, 1417.086023134510015, 204.2975919913589848 ) ) ;
#708 = CARTESIAN_POINT ( 'NONE',  ( -13.22118898579999957, 1444.932341167249888, 187.3828105311979755 ) ) ;
#709 = EDGE_CURVE ( 'NONE', #103300, #104414, #52050, .T. ) ;
#710 = CARTESIAN_POINT ( 'NONE',  ( -4.056355225345120274, 1485.204183987449824, 197.9328813784530041 ) ) ;
#711 = EDGE_CURVE ( 'NONE', #77569, #52731, #30620, .T. ) ;
#712 = CARTESIAN_POINT ( 'NONE',  ( 18.19395003950230105, 1429.625430537140119, 208.6624982699469797 ) ) ;
#713 = CARTESIAN_POINT ( 'NONE',  ( -7.496170620820000075, 1497.189208763689976, 217.7743331409489826 ) ) ;
#714 = VERTEX_POINT ( 'NONE', #62956 ) ;
#715 = CARTESIAN_POINT ( 'NONE',  ( -2.385772222184999958, 1512.160709093490141, 201.5273412906769863 ) ) ;
#716 = CARTESIAN_POINT ( 'NONE',  ( -13.94158961581099909, 1409.399911424660104, 214.4877138614390049 ) ) ;
#717 = CARTESIAN_POINT ( 'NONE',  ( 10.57777681304790107, 1481.493442856720094, 209.1910062161780104 ) ) ;
#718 = LINE ( 'NONE', #6885, #16918 ) ;
#719 = CARTESIAN_POINT ( 'NONE',  ( -27.07554453849999732, 1469.469472506630154, 267.2274423915979469 ) ) ;
#720 = CARTESIAN_POINT ( 'NONE',  ( -7.500000019065006462, 1516.813460996586855, 209.5490843734590385 ) ) ;
#721 = DIRECTION ( 'NONE',  ( 5.980589973904019347E-17, -1.000000000000000000, 1.736889445713099699E-16 ) ) ;
#722 = CARTESIAN_POINT ( 'NONE',  ( -24.69949338820000051, 1509.552011439729995, 222.6391731870980095 ) ) ;
#723 = CARTESIAN_POINT ( 'NONE',  ( -63.98295147832750018, 1384.681148330740143, 287.2755451078210172 ) ) ;
#724 = CARTESIAN_POINT ( 'NONE',  ( -27.30672991563199759, 1384.963778074569746, 204.2309128032860031 ) ) ;
#725 = CARTESIAN_POINT ( 'NONE',  ( 18.26877678840750008, 1425.191339344029757, 225.8970440910269701 ) ) ;
#726 = CARTESIAN_POINT ( 'NONE',  ( 12.08615242671140066, 1415.948038442619918, 223.4005273077049765 ) ) ;
#727 = CARTESIAN_POINT ( 'NONE',  ( -25.76956215509200021, 1482.721195220700110, 211.7561243727609792 ) ) ;
#728 = CARTESIAN_POINT ( 'NONE',  ( -19.53786426059057746, 1512.187213306747481, 179.5239794925695946 ) ) ;
#729 = CARTESIAN_POINT ( 'NONE',  ( 15.57748978360000081, 1507.212883781729943, 225.5460497861979832 ) ) ;
#730 = CARTESIAN_POINT ( 'NONE',  ( -22.96623755599999939, 1411.075251688929939, 204.6605450660979955 ) ) ;
#731 = CARTESIAN_POINT ( 'NONE',  ( 16.64491405800000123, 1416.823872462129884, 201.3696481352879744 ) ) ;
#732 = CARTESIAN_POINT ( 'NONE',  ( 3.609405579419999732, 1486.009611374690166, 219.2752556430990012 ) ) ;
#733 = CARTESIAN_POINT ( 'NONE',  ( 10.89000033453339888, 1479.690907560379856, 208.0590789013299968 ) ) ;
#734 = CARTESIAN_POINT ( 'NONE',  ( 0.8217888514169999770, 1435.943783413959864, 150.5249316333980119 ) ) ;
#735 = CARTESIAN_POINT ( 'NONE',  ( -17.57323599084560328, 1441.322512277789883, 219.0501625471149794 ) ) ;
#737 = ADVANCED_FACE ( 'NONE', ( #27645 ), #103907, .T. ) ;
#736 = CARTESIAN_POINT ( 'NONE',  ( 17.24701964721146297, 1523.844782250842400, 180.8504346226932569 ) ) ;
#738 = CARTESIAN_POINT ( 'NONE',  ( 20.56231132718039589, 1477.111355667389716, 217.7195232095880044 ) ) ;
#739 = B_SPLINE_CURVE_WITH_KNOTS ( 'NONE', 5,
 ( #42585, #61612, #95745, #102472, #34730, #601 ),
 .UNSPECIFIED., .F., .F.,
 ( 6, 6 ),
 ( 0.000000000000000000, 1.000000000000000000 ),
 .UNSPECIFIED. ) ;
#741 = CARTESIAN_POINT ( 'NONE',  ( -8.579104367239999362, 1382.291193835669901, 200.1141359521089953 ) ) ;
#740 = CARTESIAN_POINT ( 'NONE',  ( -22.98253258309999936, 1410.218983115129959, 210.7724375874179827 ) ) ;
#742 = CARTESIAN_POINT ( 'NONE',  ( 11.73122089892409825, 1426.699629391450117, 143.7537667490180127 ) ) ;
#743 = DIRECTION ( 'NONE',  ( 1.755985294532469921E-16, -1.000000000000000000, 1.338183447452831989E-16 ) ) ;
#744 = CARTESIAN_POINT ( 'NONE',  ( -10.54543569900000044, 1491.422408008689899, 212.2964277208190254 ) ) ;
#745 = CARTESIAN_POINT ( 'NONE',  ( 3.902982118626540320, 1446.676946215170119, 199.7493785281279770 ) ) ;
#746 = VECTOR ( 'NONE', #79973, 1000.000000000000000 ) ;
#747 = CARTESIAN_POINT ( 'NONE',  ( -16.78507759299379742, 1507.483737884730090, 224.6466592809620124 ) ) ;
#748 = CARTESIAN_POINT ( 'NONE',  ( 4.031142351675000235, 1516.929569650079884, 204.1114229688670036 ) ) ;
#749 = FACE_OUTER_BOUND ( 'NONE', #68574, .T. ) ;
#750 = CARTESIAN_POINT ( 'NONE',  ( 15.09629032713499974, 1514.287526756679881, 193.8365223143670164 ) ) ;
#751 = CARTESIAN_POINT ( 'NONE',  ( 7.392112708435170099, 1434.232064116840093, 226.0537490036730048 ) ) ;
#752 = CARTESIAN_POINT ( 'NONE',  ( 2.347965563550000301, 1508.995053151729962, 237.7725118035979790 ) ) ;
#753 = CARTESIAN_POINT ( 'NONE',  ( 8.026470750289130152, 1504.708605097430109, 217.7675590729679982 ) ) ;
#754 = CARTESIAN_POINT ( 'NONE',  ( -11.45094915626656018, 1505.046207261508243, 207.2314953572074785 ) ) ;
#755 = AXIS2_PLACEMENT_3D ( 'NONE', #2441, #37107, #38202 ) ;
#757 = ORIENTED_EDGE ( 'NONE', *, *, #107789, .F. ) ;
#756 = CARTESIAN_POINT ( 'NONE',  ( -59.53909452845530126, 1379.721836142610073, 264.8166016163610266 ) ) ;
#758 = VERTEX_POINT ( 'NONE', #45580 ) ;
#759 = CARTESIAN_POINT ( 'NONE',  ( 11.75556087652499926, 1433.789100478620185, 150.9322770634290123 ) ) ;
#760 = CARTESIAN_POINT ( 'NONE',  ( 27.31421232490000151, 1509.629811259429971, 216.2265006051580087 ) ) ;
#761 = ORIENTED_EDGE ( 'NONE', *, *, #76582, .F. ) ;
#762 = CARTESIAN_POINT ( 'NONE',  ( -107.5863934789999945, 1379.032352484299963, 308.9389182505590270 ) ) ;
#763 = CARTESIAN_POINT ( 'NONE',  ( -10.27580570860629905, 1448.659754571809799, 207.6397982481969962 ) ) ;
#764 = CARTESIAN_POINT ( 'NONE',  ( 3.272146740929090303, 1515.551704204679936, 205.4774934054959772 ) ) ;
#766 = CARTESIAN_POINT ( 'NONE',  ( 11.44291537990000052, 1428.994970000029980, 123.0297916884979941 ) ) ;
#765 = CARTESIAN_POINT ( 'NONE',  ( 16.02929450434690040, 1422.680592063800077, 191.1517350126889880 ) ) ;
#767 = CARTESIAN_POINT ( 'NONE',  ( 17.01221803259009846, 1498.111302379200197, 230.6454121440009999 ) ) ;
#768 = CARTESIAN_POINT ( 'NONE',  ( 1.117474349349999896, 1507.642466864929929, 181.0315143037979908 ) ) ;
#769 = CARTESIAN_POINT ( 'NONE',  ( 3.159262866049999730, 1466.676511916789877, 219.3004965968990234 ) ) ;
#770 = CARTESIAN_POINT ( 'NONE',  ( 16.66093349880000218, 1410.867388286930009, 226.5061864343979892 ) ) ;
#771 = ADVANCED_FACE ( 'NONE', ( #97611 ), #2481, .F. ) ;
#772 = B_SPLINE_SURFACE_WITH_KNOTS ( 'NONE', 2, 5, ( 
 ( #84505, #49271, #41415, #48725, #102402, #40297 ),
 ( #32462, #76660, #83398, #67178, #6696, #41961 ),
 ( #75582, #40851, #68295, #25685, #42502, #34103 ) ),
 .UNSPECIFIED., .F., .F., .F.,
 ( 3, 3 ),
 ( 6, 6 ),
 ( 110.5970879970000027, 111.5653054569999938 ),
 ( 0.000000000000000000, 2.000000000000000000 ),
 .UNSPECIFIED. ) ;
#773 = CARTESIAN_POINT ( 'NONE',  ( -4.027051443935000030, 1516.733363207009916, 211.6130343286269806 ) ) ;
#774 = CARTESIAN_POINT ( 'NONE',  ( 34.51820589317019738, 1435.725758536269950, 134.0999999979759707 ) ) ;
#775 = CARTESIAN_POINT ( 'NONE',  ( 11.86065779849999835, 1431.955919823459908, 149.9698378302979904 ) ) ;
#776 = CARTESIAN_POINT ( 'NONE',  ( 7.248946776565000860, 1514.005261957179982, 201.2133402509770121 ) ) ;
#777 = VERTEX_POINT ( 'NONE', #27103 ) ;
#778 = CARTESIAN_POINT ( 'NONE',  ( 13.87416642867090033, 1435.529565567879899, 149.9384610393090043 ) ) ;
#779 = CARTESIAN_POINT ( 'NONE',  ( -5.013279353754826140, 1375.417533171782679, 203.5257404570949973 ) ) ;
#780 = ORIENTED_EDGE ( 'NONE', *, *, #54473, .F. ) ;
#781 = ORIENTED_EDGE ( 'NONE', *, *, #58768, .F. ) ;
#782 = CARTESIAN_POINT ( 'NONE',  ( -8.664447134935000960, 1512.053281741910041, 215.6822705669570155 ) ) ;
#783 = CARTESIAN_POINT ( 'NONE',  ( -1.085556744230000037, 1465.968794482429985, 235.6834014363979861 ) ) ;
#784 = CARTESIAN_POINT ( 'NONE',  ( 20.96882344929999675, 1497.403700851489930, 212.2137616143489822 ) ) ;
#785 = CARTESIAN_POINT ( 'NONE',  ( 7.717505752974999744, 1516.857914730730045, 216.8393517232070167 ) ) ;
#786 = CARTESIAN_POINT ( 'NONE',  ( -0.9078489423485659460, 1465.209724574289794, 198.1556611775330055 ) ) ;
#787 = B_SPLINE_SURFACE_WITH_KNOTS ( 'NONE', 5, 5, ( 
 ( #32606, #26391, #34802, #33141, #68434, #7942 ),
 ( #84645, #17418, #9047, #50521, #109323, #110407 ),
 ( #25828, #7398, #92491, #43221, #42111, #33686 ),
 ( #68990, #67330, #77370, #67881, #103091, #76258 ),
 ( #60586, #101990, #101427, #25276, #59477, #40994 ),
 ( #93588, #66783, #100882, #42658, #15760, #49961 ) ),
 .UNSPECIFIED., .F., .F., .F.,
 ( 6, 6 ),
 ( 6, 6 ),
 ( 78.28065062529999807, 157.9815185129999975 ),
 ( -1.387778780779999841E-17, 1.000000000000000000 ),
 .UNSPECIFIED. ) ;
#788 = CARTESIAN_POINT ( 'NONE',  ( 11.21656023086370091, 1422.137379126830183, 210.4074592674920154 ) ) ;
#789 = CARTESIAN_POINT ( 'NONE',  ( -57.75160514174648796, 1379.717046060986377, 256.2888408195211696 ) ) ;
#790 = CARTESIAN_POINT ( 'NONE',  ( -26.65670438269999920, 1376.179549128069993, 211.2412313610989827 ) ) ;
#791 = ORIENTED_EDGE ( 'NONE', *, *, #108401, .F. ) ;
#792 = CARTESIAN_POINT ( 'NONE',  ( 3.446329775655000205, 1516.812046502680005, 206.2422037788969931 ) ) ;
#793 = ORIENTED_EDGE ( 'NONE', *, *, #35735, .T. ) ;
#794 = CARTESIAN_POINT ( 'NONE',  ( -105.5244021762739948, 1378.591211549419995, 305.0228942085889798 ) ) ;
#795 = DIRECTION ( 'NONE',  ( 0.9996573249755574819, 0.02617694830786557875, 0.000000000000000000 ) ) ;
#796 = ORIENTED_EDGE ( 'NONE', *, *, #6343, .F. ) ;
#797 = CARTESIAN_POINT ( 'NONE',  ( -11.02381067019999961, 1409.298020338630067, 190.3753894067980070 ) ) ;
#798 = CARTESIAN_POINT ( 'NONE',  ( 7.665825164484999732, 1514.407352313670117, 214.8849219750870247 ) ) ;
#800 = EDGE_LOOP ( 'NONE', ( #73155, #27198, #21110, #74200 ) ) ;
#799 = CARTESIAN_POINT ( 'NONE',  ( -1.400903968945880207, 1422.610669904860060, 192.5490106176209792 ) ) ;
#801 = CARTESIAN_POINT ( 'NONE',  ( 24.19772972739999872, 1436.897348058309944, 213.7003709038880004 ) ) ;
#802 = CARTESIAN_POINT ( 'NONE',  ( -17.67716118599750175, 1508.551704408389924, 210.4042409862270233 ) ) ;
#803 = CARTESIAN_POINT ( 'NONE',  ( 1.779428963082609894, 1456.357349037730046, 198.6855221610310309 ) ) ;
#805 = EDGE_CURVE ( 'NONE', #71147, #96332, #85826, .T. ) ;
#804 = CARTESIAN_POINT ( 'NONE',  ( 7.487063056100070391, 1517.051702153270071, 209.5621714086410066 ) ) ;
#806 = LINE ( 'NONE', #8072, #30643 ) ;
#807 = ADVANCED_FACE ( 'NONE', ( #11949 ), #61288, .F. ) ;
#808 = B_SPLINE_SURFACE_WITH_KNOTS ( 'NONE', 5, 5, ( 
 ( #65474, #14479, #6091, #93945, #7205, #59825 ),
 ( #25077, #84991, #67126, #76062, #24526, #85539 ),
 ( #58714, #68240, #110759, #101226, #33478, #86113 ),
 ( #15566, #92847, #49767, #17212, #1032, #8835 ),
 ( #102889, #16125, #42448, #8286, #59280, #51408 ),
 ( #25633, #67680, #50330, #84457, #7743, #93398 ) ),
 .UNSPECIFIED., .F., .F., .F.,
 ( 6, 6 ),
 ( 6, 6 ),
 ( 31.15146009760000112, 168.5477119569999900 ),
 ( 0.000000000000000000, 2.000000000000000000 ),
 .UNSPECIFIED. ) ;
#809 = CARTESIAN_POINT ( 'NONE',  ( 0.7560907277860019482, 1516.770163853809890, 214.1221759657669850 ) ) ;
#810 = B_SPLINE_CURVE_WITH_KNOTS ( 'NONE', 3,
 ( #86877, #102007, #10171, #16338, #84662, #19666, #72306, #44910, #11292, #105900, #29721, #45460, #38124, #106437, #63371, #38670, #12366, #95830, #3999, #54953, #96390, #71782, #63906, #98021, #87442, #29180, #89079, #88010, #81220, #79601, #21293, #89626, #46553, #19098, #4536, #2905, #20755 ),
 .UNSPECIFIED., .F., .F.,
 ( 4, 3, 3, 3, 3, 3, 3, 3, 3, 3, 3, 3, 4 ),
 ( -12.02648877283809981, -11.71886065317380066, -11.10599023740059899, -10.45513282830309976, -9.768661030076680518, -9.016051782489549637, -8.113804059961630344, -7.249942693435659891, -6.491588414576360044, -5.633190057283429475, -4.895335684179899616, -4.254313181755179585, -3.650975912550000757 ),
 .UNSPECIFIED. ) ;
#811 = FACE_OUTER_BOUND ( 'NONE', #80418, .T. ) ;
#812 = CARTESIAN_POINT ( 'NONE',  ( 156.6846457583361882, 1524.382868172863937, 340.9912860285725174 ) ) ;
#813 = CARTESIAN_POINT ( 'NONE',  ( 28.24318409530000196, 1508.132100788830030, 208.6373738428400202 ) ) ;
#814 = CARTESIAN_POINT ( 'NONE',  ( 4.625359524845000792, 1517.025470194390209, 211.6020329869469947 ) ) ;
#815 = CARTESIAN_POINT ( 'NONE',  ( 13.04207770780000075, 1409.368499776629960, 192.3005056216980222 ) ) ;
#816 = CARTESIAN_POINT ( 'NONE',  ( -18.12145421590813044, 1486.178648751641958, 188.5740549209106405 ) ) ;
#818 = ORIENTED_EDGE ( 'NONE', *, *, #64063, .F. ) ;
#817 = CARTESIAN_POINT ( 'NONE',  ( -73.59349969589999318, 1386.581895584289896, 298.9135147644589665 ) ) ;
#819 = CARTESIAN_POINT ( 'NONE',  ( 38.63863155180000319, 1453.572278011729850, 261.7057835891980631 ) ) ;
#820 = CARTESIAN_POINT ( 'NONE',  ( 10.79932292162989960, 1490.768715835539979, 211.1233481957399931 ) ) ;
#821 = CARTESIAN_POINT ( 'NONE',  ( 20.06033034266344828, 1526.189892541618974, 233.0619703228597643 ) ) ;
#822 = CARTESIAN_POINT ( 'NONE',  ( -3.857078437385809799, 1508.816503730140084, 237.6133849306840204 ) ) ;
#823 = CARTESIAN_POINT ( 'NONE',  ( -20.12017060440000193, 1455.134694269430156, 226.3336132045979809 ) ) ;
#824 = TOROIDAL_SURFACE ( 'NONE', #91997, 6.500000000000000000, 1.000000000000000000 ) ;
#825 = B_SPLINE_CURVE_WITH_KNOTS ( 'NONE', 3,
 ( #47399, #92685, #7583, #51245, #24372, #75897, #76443, #110598, #102187, #51810, #15416, #50694, #110049, #101619, #24907, #15960, #58007, #49607, #34444, #25467, #26016, #84292, #75365, #33322, #67518, #68620, #77560, #102722, #60213, #66420, #58557, #7036, #59115, #32780, #85378, #50164, #93240, #41738, #109504, #16506, #84824, #8126, #94331, #17609, #83739, #85951, #66964 ),
 .UNSPECIFIED., .F., .F.,
 ( 4, 2, 2, 2, 1, 1, 1, 1, 1, 1, 2, 2, 2, 2, 2, 1, 1, 1, 1, 2, 2, 2, 2, 2, 1, 1, 1, 2, 2, 4 ),
 ( 0.000000000000000000, 0.1249999999994302891, 0.1874999999991454336, 0.2187499999990033250, 0.2343749999989332422, 0.2421874999988981869, 0.2460937499988812005, 0.2480468749988732624, 0.2490234374988696819, 0.2495117187488680166, 0.2497558593738682942, 0.2499999999988685717, 0.3749999999990826782, 0.4374999999991906474, 0.4687499999992447708, 0.4843749999992725264, 0.4921874999992852939, 0.4960937499992913446, 0.4980468749992940647, 0.4990234374992957855, 0.4999999999992974509, 0.6249999999994888533, 0.6874999999995836664, 0.7187499999996309619, 0.7343749999996548317, 0.7421874999996680433, 0.7460937499996733724, 0.7480468749996770361, 0.7499999999996806999, 1.000000000000000000 ),
 .UNSPECIFIED. ) ;
#827 = CARTESIAN_POINT ( 'NONE',  ( 17.53216825571119841, 1409.785550747969864, 222.6111406110179871 ) ) ;
#826 = CARTESIAN_POINT ( 'NONE',  ( 11.86750639809999974, 1432.440573318600173, 149.9822236389979935 ) ) ;
#828 = CARTESIAN_POINT ( 'NONE',  ( 14.94707557629999961, 1464.413060387330006, 194.8657129345979797 ) ) ;
#829 = CARTESIAN_POINT ( 'NONE',  ( -113.4000000000000057, 1306.913060387289988, 304.2218459572590064 ) ) ;
#830 = EDGE_LOOP ( 'NONE', ( #94254, #75571, #96496 ) ) ;
#831 = CARTESIAN_POINT ( 'NONE',  ( -4.039897316195000698, 1516.787536375099990, 204.1233307748069876 ) ) ;
#832 = EDGE_CURVE ( 'NONE', #43055, #13291, #18048, .T. ) ;
#833 = CARTESIAN_POINT ( 'NONE',  ( 1.802378746250000008E-09, 1405.842710276529942, 267.2349610868979539 ) ) ;
#834 = CARTESIAN_POINT ( 'NONE',  ( 27.68516841690000163, 1508.595246553930110, 207.6423249425380106 ) ) ;
#835 = CIRCLE ( 'NONE', #7915, 0.5000000000000000000 ) ;
#836 = EDGE_CURVE ( 'NONE', #3563, #58739, #41250, .T. ) ;
#837 = CARTESIAN_POINT ( 'NONE',  ( 12.73048906560000049, 1416.839648772530154, 223.1309759830980113 ) ) ;
#839 = B_SPLINE_CURVE_WITH_KNOTS ( 'NONE', 3,
 ( #94188, #26432, #95856, #96974, #60626, #95310, #44933, #10194, #44369, #79080, #712, #94749, #20238 ),
 .UNSPECIFIED., .F., .F.,
 ( 4, 3, 3, 3, 4 ),
 ( -1.599569173379999931, -0.7029132044934469636, 0.1891147555273189340, 1.073570521650659693, 1.599569173380000375 ),
 .UNSPECIFIED. ) ;
#838 = CARTESIAN_POINT ( 'NONE',  ( 34.68852446352940433, 1522.382868172863937, 199.9946320047950223 ) ) ;
#840 = CARTESIAN_POINT ( 'NONE',  ( 3.686065144790000137, 1468.106296616489999, 218.4108491294889802 ) ) ;
#841 = CARTESIAN_POINT ( 'NONE',  ( 4.894570698429999922, 1447.010184225089915, 205.0316855332089858 ) ) ;
#842 = ADVANCED_FACE ( 'NONE', ( #71348 ), #98540, .T. ) ;
#843 = CARTESIAN_POINT ( 'NONE',  ( 26.80761308193400083, 1435.433708684199928, 135.7240834635020121 ) ) ;
#844 = CARTESIAN_POINT ( 'NONE',  ( 36.51307952743290031, 1449.798342968150109, 136.2643497551869984 ) ) ;
#845 = DIRECTION ( 'NONE',  ( -0.9125304618754018771, 0.000000000000000000, 0.4090087482554204401 ) ) ;
#846 = CARTESIAN_POINT ( 'NONE',  ( -109.2380410539999929, 1385.254002988119964, 297.1509341280589638 ) ) ;
#847 = CARTESIAN_POINT ( 'NONE',  ( 10.89269473999179993, 1480.433624861380167, 210.4306936963210148 ) ) ;
#848 = CARTESIAN_POINT ( 'NONE',  ( 18.66420869458043441, 1526.382868172864164, 185.4599087859680537 ) ) ;
#849 = CARTESIAN_POINT ( 'NONE',  ( -4.230955727593959104, 1446.180919742871311, 217.1469061245145724 ) ) ;
#850 = ORIENTED_EDGE ( 'NONE', *, *, #22937, .F. ) ;
#851 = CARTESIAN_POINT ( 'NONE',  ( 1.618115094650000030, 1427.197104430330000, 147.9439864917980287 ) ) ;
#852 = CARTESIAN_POINT ( 'NONE',  ( 13.80586431050000051, 1434.979615221880067, 146.9208280877979860 ) ) ;
#853 = ADVANCED_FACE ( 'NONE', ( #80261 ), #34845, .T. ) ;
#854 = CARTESIAN_POINT ( 'NONE',  ( -1.041174743597367502, 1450.833881364289255, 181.5282326196627594 ) ) ;
#855 = CARTESIAN_POINT ( 'NONE',  ( 16.89419322268659940, 1506.223051208969991, 188.1395524883149903 ) ) ;
#856 = CARTESIAN_POINT ( 'NONE',  ( -2.024352074859999871E-09, 1476.050155969130174, 268.4837719564979466 ) ) ;
#858 = CARTESIAN_POINT ( 'NONE',  ( 18.69816095120771493, 1522.382868172863937, 234.8576566410002897 ) ) ;
#857 = CARTESIAN_POINT ( 'NONE',  ( 12.56213108819999924, 1501.082362947789989, 211.1229812159690198 ) ) ;
#859 = CARTESIAN_POINT ( 'NONE',  ( -29.25495648809999949, 1509.872423546730033, 208.6412349914980098 ) ) ;
#860 = AXIS2_PLACEMENT_3D ( 'NONE', #53375, #104309, #3530 ) ;
#861 = CARTESIAN_POINT ( 'NONE',  ( 8.972723096110000185, 1427.878097284390151, 212.0837492402690145 ) ) ;
#862 = CARTESIAN_POINT ( 'NONE',  ( -16.22265104649770251, 1384.873541373520084, 219.7134262672329896 ) ) ;
#863 = EDGE_CURVE ( 'NONE', #108182, #30075, #109280, .T. ) ;
#864 = CARTESIAN_POINT ( 'NONE',  ( -11.09572995843272025, 1418.539393402124688, 229.3725684295395411 ) ) ;
#865 = CARTESIAN_POINT ( 'NONE',  ( -18.88067404609999755, 1416.254459047329874, 207.9833811512579871 ) ) ;
#866 = CARTESIAN_POINT ( 'NONE',  ( -8.388361968899999965, 1483.465050472690109, 201.7385226000290004 ) ) ;
#867 = CARTESIAN_POINT ( 'NONE',  ( 24.98946546190000007, 1435.376445165819860, 135.9357081857980063 ) ) ;
#868 = CARTESIAN_POINT ( 'NONE',  ( -6.019553345473489969, 1396.123267822159733, 199.8697773833820008 ) ) ;
#869 = ORIENTED_EDGE ( 'NONE', *, *, #24347, .T. ) ;
#870 = EDGE_CURVE ( 'NONE', #24039, #32377, #39575, .T. ) ;
#871 = VECTOR ( 'NONE', #57828, 1000.000000000000000 ) ;
#872 = CARTESIAN_POINT ( 'NONE',  ( -16.31993864512639902, 1409.491010191830128, 225.1742793860710208 ) ) ;
#873 = CARTESIAN_POINT ( 'NONE',  ( 4.967309476820000569, 1440.444625599219989, 150.3089546883979892 ) ) ;
#874 = ORIENTED_EDGE ( 'NONE', *, *, #74452, .T. ) ;
#875 = EDGE_LOOP ( 'NONE', ( #11921, #86315, #53502, #106235 ) ) ;
#876 = CARTESIAN_POINT ( 'NONE',  ( -11.25637332900000054, 1500.624827952490023, 211.0037260121189888 ) ) ;
#878 = EDGE_CURVE ( 'NONE', #23166, #598, #93399, .T. ) ;
#877 = CARTESIAN_POINT ( 'NONE',  ( -14.67979535943448255, 1416.151753477184002, 204.4125811959580972 ) ) ;
#880 = CARTESIAN_POINT ( 'NONE',  ( -9.954564879586309090, 1438.994910147829842, 209.5496646517129875 ) ) ;
#879 = CARTESIAN_POINT ( 'NONE',  ( 10.92028016000000079, 1426.083762019530013, 93.45830742669778601 ) ) ;
#881 = EDGE_CURVE ( 'NONE', #44275, #39082, #97366, .T. ) ;
#882 = CARTESIAN_POINT ( 'NONE',  ( -11.62823626630000184, 1433.009257201529863, 151.0297253050979975 ) ) ;
#883 = CARTESIAN_POINT ( 'NONE',  ( -2.882041267162114728, 1419.632841759689200, 186.1906303718482434 ) ) ;
#884 = CARTESIAN_POINT ( 'NONE',  ( 7.904651180169999236, 1423.075284537190100, 213.5785853047590024 ) ) ;
#885 = CARTESIAN_POINT ( 'NONE',  ( -18.32377786700000399, 1464.077817829789865, 217.4721512913189940 ) ) ;
#886 = FACE_BOUND ( 'NONE', #41380, .T. ) ;
#887 = CARTESIAN_POINT ( 'NONE',  ( 3.452230076589999808, 1448.972367684420078, 184.0844731014979914 ) ) ;
#888 = EDGE_CURVE ( 'NONE', #28394, #99599, #66657, .T. ) ;
#889 = CARTESIAN_POINT ( 'NONE',  ( 8.788288708663037241, 1364.745218052601786, 210.6218459617142003 ) ) ;
#891 = EDGE_LOOP ( 'NONE', ( #56379, #88097, #94429, #5501 ) ) ;
#890 = CARTESIAN_POINT ( 'NONE',  ( 6.121126660120000729, 1455.402339941889750, 217.8370560331890147 ) ) ;
#892 = ORIENTED_EDGE ( 'NONE', *, *, #53861, .T. ) ;
#893 = CARTESIAN_POINT ( 'NONE',  ( -41.65927775779999820, 1443.915297666309925, 135.6909731803980037 ) ) ;
#894 = CARTESIAN_POINT ( 'NONE',  ( -21.51338636340619814, 1505.551605034549766, 209.1218290568810119 ) ) ;
#895 = CARTESIAN_POINT ( 'NONE',  ( -1.417330028740000136, 1471.777279435030096, 269.8655828747980081 ) ) ;
#896 = CARTESIAN_POINT ( 'NONE',  ( 7.616929904139634999, 1500.300532160428247, 200.6431694768011482 ) ) ;
#897 = CARTESIAN_POINT ( 'NONE',  ( -30.95751052620455468, 1525.821544997590081, 201.4531494772889744 ) ) ;
#898 = CARTESIAN_POINT ( 'NONE',  ( -2.006862033407029955, 1475.288591552500066, 197.8580126313549954 ) ) ;
#899 = DIRECTION ( 'NONE',  ( 0.9980966414074828874, 0.06164810140419229451, 0.001614312349211199796 ) ) ;
#900 = CARTESIAN_POINT ( 'NONE',  ( -22.84654337453140016, 1507.483738429109962, 208.2307034531480099 ) ) ;
#901 = CARTESIAN_POINT ( 'NONE',  ( 8.279480055211028144, 1369.617909351883327, 208.3718459617010978 ) ) ;
#902 = CARTESIAN_POINT ( 'NONE',  ( -0.03232803257987929696, 1407.837594159410173, 195.9367397066039871 ) ) ;
#903 = CARTESIAN_POINT ( 'NONE',  ( -24.18583280233420041, 1410.839831453439956, 268.2351350556830312 ) ) ;
#904 = CARTESIAN_POINT ( 'NONE',  ( -13.81131977446409920, 1434.989890545529988, 148.7892102494269864 ) ) ;
#905 = ORIENTED_EDGE ( 'NONE', *, *, #70766, .T. ) ;
#906 = FACE_OUTER_BOUND ( 'NONE', #101893, .T. ) ;
#907 = CARTESIAN_POINT ( 'NONE',  ( 13.76098194390000096, 1443.039742490210074, 189.2009281145979855 ) ) ;
#908 = B_SPLINE_SURFACE_WITH_KNOTS ( 'NONE', 5, 5, ( 
 ( #76165, #109767, #85650, #40900, #100792, #42561 ),
 ( #24083, #8951, #42016, #68898, #58817, #50433 ),
 ( #50973, #580, #49321, #49872, #23545, #57737 ),
 ( #109231, #76714, #83447, #43124, #32515, #51518 ),
 ( #58272, #7306, #75632, #6742, #92956, #67235 ),
 ( #93499, #67780, #16770, #91855, #85103, #33047 ) ),
 .UNSPECIFIED., .F., .F., .F.,
 ( 6, 6 ),
 ( 6, 6 ),
 ( 29.54622938989999881, 29.61002813500000030 ),
 ( 0.000000000000000000, 2.000000000000000000 ),
 .UNSPECIFIED. ) ;
#909 = CIRCLE ( 'NONE', #106386, 2.500000000000002220 ) ;
#910 = ORIENTED_EDGE ( 'NONE', *, *, #106899, .T. ) ;
#911 = VERTEX_POINT ( 'NONE', #76256 ) ;
#912 = FACE_OUTER_BOUND ( 'NONE', #72919, .T. ) ;
#913 = CARTESIAN_POINT ( 'NONE',  ( -9.832966357650001044, 1364.062280235949856, 207.6218459616989946 ) ) ;
#914 = CIRCLE ( 'NONE', #22271, 1.999999999999997780 ) ;
#915 = CARTESIAN_POINT ( 'NONE',  ( -4.029572678834999699, 1516.858649670339901, 213.1633184439769764 ) ) ;
#916 = CARTESIAN_POINT ( 'NONE',  ( -16.49868107950000251, 1485.484778815929985, 187.9250925817980260 ) ) ;
#917 = B_SPLINE_SURFACE_WITH_KNOTS ( 'NONE', 5, 4, ( 
 ( #86063, #103389, #26695, #52480, #50808 ),
 ( #76552, #25027, #8785, #9902, #78209 ),
 ( #58665, #1521, #16073, #35654, #69844 ),
 ( #50276, #101739, #33428, #76004, #84405 ),
 ( #110708, #33998, #7692, #68191, #110157 ),
 ( #67625, #17159, #59229, #93346, #51352 ),
 ( #16611, #102295, #25580, #59773, #27259 ),
 ( #105074, #3195, #70400, #38407, #87738 ),
 ( #36767, #27816, #37875, #55240, #61442 ) ),
 .UNSPECIFIED., .F., .F., .F.,
 ( 6, 3, 6 ),
 ( 5, 5 ),
 ( 0.000000000000000000, 5.782490304330000441, 11.25975508159999983 ),
 ( 40.20365518519999881, 50.26548245740000453 ),
 .UNSPECIFIED. ) ;
#918 = EDGE_CURVE ( 'NONE', #68939, #6679, #17776, .T. ) ;
#919 = ORIENTED_EDGE ( 'NONE', *, *, #372, .T. ) ;
#920 = CARTESIAN_POINT ( 'NONE',  ( -113.4000000000000057, 1374.720597897390007, 302.6503168488589495 ) ) ;
#921 = EDGE_CURVE ( 'NONE', #25855, #45625, #9330, .T. ) ;
#922 = CARTESIAN_POINT ( 'NONE',  ( -106.1401956836040057, 1378.913060387289988, 302.5623463823779957 ) ) ;
#923 = CARTESIAN_POINT ( 'NONE',  ( 2.868433798504999910, 1517.020727862619879, 204.1095288638669842 ) ) ;
#924 = CARTESIAN_POINT ( 'NONE',  ( -27.91817790900000062, 1509.614502511829869, 204.0422066038080118 ) ) ;
#925 = B_SPLINE_SURFACE_WITH_KNOTS ( 'NONE', 5, 5, ( 
 ( #19475, #46376, #97294, #18912, #53676, #3824 ),
 ( #38484, #53110, #54765, #72133, #81042, #63188 ),
 ( #104039, #87819, #79951, #29002, #55317, #61517 ),
 ( #11106, #87247, #27891, #10538, #12182, #46923 ),
 ( #89449, #62074, #45268, #44712, #79406, #12741 ),
 ( #78863, #2717, #71032, #2170, #96760, #36285 ),
 ( #105153, #28445, #20030, #62639, #54224, #88351 ),
 ( #45818, #3268, #89993, #66483, #7097, #81581 ),
 ( #100045, #106789, #99478, #98393, #13268, #32299 ) ),
 .UNSPECIFIED., .F., .F., .F.,
 ( 6, 3, 6 ),
 ( 6, 6 ),
 ( 0.000000000000000000, 6.814644137399999302, 13.62928827480000038 ),
 ( 0.000000000000000000, 2.000000000000000000 ),
 .UNSPECIFIED. ) ;
#926 = CARTESIAN_POINT ( 'NONE',  ( -7.644479542047480258, 1517.051704408389924, 208.6854770967850072 ) ) ;
#927 = CARTESIAN_POINT ( 'NONE',  ( -75.49934453870000084, 1384.893650425089845, 276.6853632062590123 ) ) ;
#928 = CARTESIAN_POINT ( 'NONE',  ( -51.30093226525310257, 1384.625592632969756, 227.3549881365390206 ) ) ;
#929 = CARTESIAN_POINT ( 'NONE',  ( -6.294750371550000168, 1408.079328834029866, 197.5408074072979900 ) ) ;
#930 = CARTESIAN_POINT ( 'NONE',  ( -109.1320112420000044, 1384.953741877089897, 311.2644403302589353 ) ) ;
#932 = ORIENTED_EDGE ( 'NONE', *, *, #44106, .F. ) ;
#931 = CARTESIAN_POINT ( 'NONE',  ( -8.892386117350001840, 1446.653515387309881, 186.0933241611980122 ) ) ;
#933 = CARTESIAN_POINT ( 'NONE',  ( 5.983287317399999417, 1451.235340618889950, 210.0682002075799915 ) ) ;
#934 = CARTESIAN_POINT ( 'NONE',  ( 27.66125109210000232, 1508.130528729329853, 212.4510895349179975 ) ) ;
#935 = CARTESIAN_POINT ( 'NONE',  ( 20.54804277566730164, 1497.617938160230096, 225.9533463448229895 ) ) ;
#936 = ADVANCED_FACE ( 'NONE', ( #76810 ), #40125, .T. ) ;
#937 = CARTESIAN_POINT ( 'NONE',  ( -25.25411696669999984, 1436.161966705209807, 137.2604574136979920 ) ) ;
#938 = CARTESIAN_POINT ( 'NONE',  ( 4.042729802795000715, 1516.919782530640077, 212.3762473738369749 ) ) ;
#939 = CARTESIAN_POINT ( 'NONE',  ( -68.65285585769998988, 1379.747727628990106, 279.8365758267589740 ) ) ;
#940 = CARTESIAN_POINT ( 'NONE',  ( -18.84544153430000080, 1444.454624232390188, 208.1911640471150235 ) ) ;
#941 = CARTESIAN_POINT ( 'NONE',  ( -30.57821243133623668, 1525.253972588461693, 221.5701747116904130 ) ) ;
#942 = VECTOR ( 'NONE', #92209, 1000.000000000000000 ) ;
#943 = CARTESIAN_POINT ( 'NONE',  ( 2.480427254505000345, 1516.872851364150165, 208.3639601402670110 ) ) ;
#944 = VERTEX_POINT ( 'NONE', #19645 ) ;
#945 = DIRECTION ( 'NONE',  ( -1.139478816419269183E-15, -0.7071067811865474617, -0.7071067811865474617 ) ) ;
#946 = CARTESIAN_POINT ( 'NONE',  ( -12.69028397900000016, 1410.293270958429957, 227.9608284046979918 ) ) ;
#947 = CARTESIAN_POINT ( 'NONE',  ( -54.13887208369999371, 1385.096747890979941, 270.3642349231589606 ) ) ;
#948 = EDGE_LOOP ( 'NONE', ( #55161, #35565, #39412, #54250 ) ) ;
#949 = CARTESIAN_POINT ( 'NONE',  ( 22.08622291482349809, 1523.382868172864164, 233.8253038720783650 ) ) ;
#950 = EDGE_CURVE ( 'NONE', #36610, #45421, #18629, .T. ) ;
#951 = CARTESIAN_POINT ( 'NONE',  ( -11.26811797368760004, 1492.006046055339993, 204.2379200572160016 ) ) ;
#952 = CARTESIAN_POINT ( 'NONE',  ( 12.17388030439999902, 1434.392357979209919, 150.5457779309980140 ) ) ;
#953 = CARTESIAN_POINT ( 'NONE',  ( 17.06601014015459938, 1459.307105401880108, 228.6469079145479952 ) ) ;
#954 = VECTOR ( 'NONE', #58866, 1000.000000000000114 ) ;
#955 = CARTESIAN_POINT ( 'NONE',  ( -24.97341835772749974, 1509.778186992499968, 223.4246975716070267 ) ) ;
#956 = EDGE_CURVE ( 'NONE', #90273, #106841, #7354, .T. ) ;
#957 = DIRECTION ( 'NONE',  ( 0.000000000000000000, 1.000000000000000000, 0.000000000000000000 ) ) ;
#958 = CARTESIAN_POINT ( 'NONE',  ( 3.055333763765900386E-13, 1547.913060387330006, 209.1218459616979999 ) ) ;
#959 = CARTESIAN_POINT ( 'NONE',  ( 4.223877582933059927, 1441.585397622020082, 166.9011155059120028 ) ) ;
#961 = CARTESIAN_POINT ( 'NONE',  ( -14.65245215464970130, 1420.119839417710182, 213.8659310620899987 ) ) ;
#960 = CARTESIAN_POINT ( 'NONE',  ( 1.712644716155000024, 1516.636036526019780, 214.1174694231270053 ) ) ;
#962 = CARTESIAN_POINT ( 'NONE',  ( 19.75079307820000096, 1509.023212949429990, 188.3853951167980085 ) ) ;
#963 = CARTESIAN_POINT ( 'NONE',  ( -7.716878941104999612, 1516.833976295079992, 216.4517711926369827 ) ) ;
#964 = ORIENTED_EDGE ( 'NONE', *, *, #29949, .T. ) ;
#965 = CARTESIAN_POINT ( 'NONE',  ( -11.96392952312879920, 1414.971349104640012, 197.5065749685350340 ) ) ;
#966 = CARTESIAN_POINT ( 'NONE',  ( 4.987078435459999071, 1509.051704408389924, 209.1218459616989946 ) ) ;
#967 = VERTEX_POINT ( 'NONE', #52531 ) ;
#968 = CARTESIAN_POINT ( 'NONE',  ( 2.967683387859999744, 1419.631902151829991, 185.2975656967979887 ) ) ;
#969 = PRESENTATION_STYLE_ASSIGNMENT (( #77656 ) ) ;
#970 = CARTESIAN_POINT ( 'NONE',  ( 3.351189091698004940, 1524.075132568163781, 176.2264789961865006 ) ) ;
#971 = CARTESIAN_POINT ( 'NONE',  ( 2.969165624449999541, 1442.252637987289972, 217.6050255308190060 ) ) ;
#972 = CARTESIAN_POINT ( 'NONE',  ( -30.15585515321768995, 1524.425415513989719, 195.8365654344459870 ) ) ;
#973 = CARTESIAN_POINT ( 'NONE',  ( -16.64381284196683097, 1410.502069620746624, 191.7858560727107715 ) ) ;
#974 = CARTESIAN_POINT ( 'NONE',  ( -3.143430252119999935, 1447.188759692610120, 156.1111700446979853 ) ) ;
#976 = EDGE_CURVE ( 'NONE', #32267, #2539, #49404, .T. ) ;
#975 = CARTESIAN_POINT ( 'NONE',  ( 18.88375791580248730, 1507.757577934934034, 229.9162092553959837 ) ) ;
#977 = CYLINDRICAL_SURFACE ( 'NONE', #41279, 23.99999999999999289 ) ;
#978 = CARTESIAN_POINT ( 'NONE',  ( 9253.086965755297570, 5182.654794667092574, 284.7734187413164477 ) ) ;
#979 = CARTESIAN_POINT ( 'NONE',  ( 15.92242058219999912, 1419.011245157130134, 191.2650185718979685 ) ) ;
#981 = CARTESIAN_POINT ( 'NONE',  ( -5.003798055078270579, 1509.217832977240050, 179.4360497324900052 ) ) ;
#980 = CARTESIAN_POINT ( 'NONE',  ( -14.43176806938940082, 1417.361901689390152, 203.3004255274190086 ) ) ;
#982 = ORIENTED_EDGE ( 'NONE', *, *, #84481, .T. ) ;
#983 = CARTESIAN_POINT ( 'NONE',  ( -8.333035966500000669, 1508.478891882389917, 219.2689049391989897 ) ) ;
#984 = CARTESIAN_POINT ( 'NONE',  ( 24.30724142280000066, 1449.842033426479929, 206.4729385141180273 ) ) ;
#985 = ADVANCED_FACE ( 'NONE', ( #24529 ), #51856, .F. ) ;
#986 = CARTESIAN_POINT ( 'NONE',  ( -27.94676419710000204, 1509.200065883529760, 210.6896604893480003 ) ) ;
#987 = CARTESIAN_POINT ( 'NONE',  ( 10.30115261902779089, 1410.643515217512459, 188.8098223140025027 ) ) ;
#988 = FACE_OUTER_BOUND ( 'NONE', #72451, .T. ) ;
#989 = DIRECTION ( 'NONE',  ( 0.000000000000000000, 0.000000000000000000, -1.000000000000000000 ) ) ;
#990 = EDGE_CURVE ( 'NONE', #18936, #89283, #17213, .T. ) ;
#991 = CARTESIAN_POINT ( 'NONE',  ( -3.276363691050809823, 1486.691431019839911, 220.6577433852839931 ) ) ;
#992 = CARTESIAN_POINT ( 'NONE',  ( -8.229021304010000648, 1439.448076410589920, 228.6152058856989697 ) ) ;
#993 = CARTESIAN_POINT ( 'NONE',  ( -69.93979052779329209, 1383.785293178040092, 294.7370205497300049 ) ) ;
#994 = CIRCLE ( 'NONE', #29578, 2.000079901618746270 ) ;
#995 = CARTESIAN_POINT ( 'NONE',  ( -108.2039566672529958, 1378.913060387289988, 299.7295690038039879 ) ) ;
#996 = LINE ( 'NONE', #18854, #12421 ) ;
#997 = CARTESIAN_POINT ( 'NONE',  ( -1.079555022276609932, 1516.642200982659915, 201.4099888424200060 ) ) ;
#999 = ORIENTED_EDGE ( 'NONE', *, *, #53098, .T. ) ;
#998 = CARTESIAN_POINT ( 'NONE',  ( 10.57159226293329901, 1452.549534872659933, 209.4522820094259714 ) ) ;
#1000 = CARTESIAN_POINT ( 'NONE',  ( -1.499372387922010219, 1414.913526845469960, 226.2260460821569836 ) ) ;
#1001 = CARTESIAN_POINT ( 'NONE',  ( -59.38610754540000158, 1383.797318715759957, 279.8430129459590034 ) ) ;
#1002 = CARTESIAN_POINT ( 'NONE',  ( 19.95567201858020212, 1508.916776747199947, 229.6244079712500081 ) ) ;
#1003 = ORIENTED_EDGE ( 'NONE', *, *, #66990, .T. ) ;
#1004 = VERTEX_POINT ( 'NONE', #56242 ) ;
#1005 = CARTESIAN_POINT ( 'NONE',  ( 19.48180575948950022, 1507.796555935530250, 229.4922617073300160 ) ) ;
#1006 = CARTESIAN_POINT ( 'NONE',  ( 18.80464302510000252, 1425.801049065629968, 225.6039134470979945 ) ) ;
#1007 = CARTESIAN_POINT ( 'NONE',  ( 39.59123454348529947, 1440.695445213330004, 136.7962490760550054 ) ) ;
#1009 = FACE_OUTER_BOUND ( 'NONE', #20638, .T. ) ;
#1008 = DIRECTION ( 'NONE',  ( 6.938893903907222067E-15, 0.000000000000000000, 1.000000000000000000 ) ) ;
#1010 = B_SPLINE_CURVE_WITH_KNOTS ( 'NONE', 3,
 ( #7991, #34299, #67381, #75763 ),
 .UNSPECIFIED., .F., .F.,
 ( 4, 4 ),
 ( -21.04253309989999821, -13.35595807039999983 ),
 .UNSPECIFIED. ) ;
#1011 = EDGE_CURVE ( 'NONE', #13254, #104898, #107740, .T. ) ;
#1012 = DIRECTION ( 'NONE',  ( -5.980589973904019347E-17, 1.000000000000000000, -1.736889445713099699E-16 ) ) ;
#1013 = CARTESIAN_POINT ( 'NONE',  ( -107.7596963679999931, 1382.859817520469733, 297.6961126062590210 ) ) ;
#1014 = CARTESIAN_POINT ( 'NONE',  ( -0.5200257809521398045, 1450.894900823177750, 181.6063032256765553 ) ) ;
#1015 = CARTESIAN_POINT ( 'NONE',  ( -20.31333848799999942, 1485.909380060430067, 191.0034922223980232 ) ) ;
#1016 = CARTESIAN_POINT ( 'NONE',  ( 4.136067035069999953, 1409.224821449829960, 186.6613252426980125 ) ) ;
#1017 = DIRECTION ( 'NONE',  ( 0.03006000153033951128, -0.4884709562387339332, -0.8720622232497018400 ) ) ;
#1019 = ADVANCED_FACE ( 'NONE', ( #35713 ), #50299, .T. ) ;
#1018 = CARTESIAN_POINT ( 'NONE',  ( -8.778727802480000619, 1440.670317285799911, 153.7060890884979756 ) ) ;
#1020 = CARTESIAN_POINT ( 'NONE',  ( 9.327660711791368797, 1434.415577812250149, 206.2244467992360057 ) ) ;
#1021 = CARTESIAN_POINT ( 'NONE',  ( -15.14764113784119992, 1421.271689049209954, 203.4892272555310058 ) ) ;
#1022 = CARTESIAN_POINT ( 'NONE',  ( 0.8791005338980000250, 1507.105016923229869, 237.2044774393979765 ) ) ;
#1023 = CARTESIAN_POINT ( 'NONE',  ( -16.09752958667184330, 1409.475198507421055, 193.0827175891761271 ) ) ;
#1024 = ORIENTED_EDGE ( 'NONE', *, *, #4374, .T. ) ;
#1025 = CARTESIAN_POINT ( 'NONE',  ( -18.64672481365220236, 1416.851343896850040, 208.5597484336410048 ) ) ;
#1026 = AXIS2_PLACEMENT_3D ( 'NONE', #39081, #107399, #20087 ) ;
#1027 = CARTESIAN_POINT ( 'NONE',  ( -4.249593083980000685, 1482.545674215690042, 231.1654941120989974 ) ) ;
#1028 = CARTESIAN_POINT ( 'NONE',  ( -41.68718522609999155, 1445.343426362629998, 269.6415487380980380 ) ) ;
#1029 = CARTESIAN_POINT ( 'NONE',  ( -12.27023110815660090, 1416.839692126590080, 194.6640136892829958 ) ) ;
#1030 =( BOUNDED_CURVE ( )  B_SPLINE_CURVE ( 3, ( #18335, #33476, #17766, #17209 ),
 .UNSPECIFIED., .F., .T. ) 
 B_SPLINE_CURVE_WITH_KNOTS ( ( 4, 4 ),
 ( 1.455430482180659846, 1.955768190241684801 ),
 .UNSPECIFIED. ) 
 CURVE ( )  GEOMETRIC_REPRESENTATION_ITEM ( )  RATIONAL_B_SPLINE_CURVE ( ( 1.000000000000000000, 0.9792470884949975307, 0.9792470884949975307, 1.000000000000000000 ) ) 
 REPRESENTATION_ITEM ( '' )  );
#1031 = CARTESIAN_POINT ( 'NONE',  ( 17.59077139289999892, 1410.452734695029903, 223.9185061424979892 ) ) ;
#1032 = CARTESIAN_POINT ( 'NONE',  ( 16.67080554670000225, 1468.816899178029871, 189.7273712455979933 ) ) ;
#1033 = CARTESIAN_POINT ( 'NONE',  ( 7.215398911020000305, 1408.913060387329779, 192.6378332269979978 ) ) ;
#1034 = CARTESIAN_POINT ( 'NONE',  ( -20.40544550950000158, 1484.240032026089921, 212.0770037828889940 ) ) ;
#1035 = CARTESIAN_POINT ( 'NONE',  ( -0.5943821362719999835, 1416.311719779230089, 227.7090535903980140 ) ) ;
#1036 = CARTESIAN_POINT ( 'NONE',  ( -4.868964994320000628, 1417.652559593630031, 232.9301174602979927 ) ) ;
#1037 = VECTOR ( 'NONE', #102245, 1000.000000000000114 ) ;
#1038 = CARTESIAN_POINT ( 'NONE',  ( -7.601092437462869889, 1510.855104182140167, 214.7738715786570083 ) ) ;
#1039 = CARTESIAN_POINT ( 'NONE',  ( -0.7957830110718832062, 1359.403009717480018, 207.6218459616987673 ) ) ;
#1040 = CARTESIAN_POINT ( 'NONE',  ( -45.89749746886590032, 1438.271440801009931, 268.5002330264039756 ) ) ;
#1041 = CARTESIAN_POINT ( 'NONE',  ( -4.155669689119999788, 1439.704322410179884, 185.4969487639980059 ) ) ;
#1042 = ORIENTED_EDGE ( 'NONE', *, *, #56606, .F. ) ;
#1043 = CARTESIAN_POINT ( 'NONE',  ( -7.987246895440000216, 1424.400859198919989, 210.3710278188289919 ) ) ;
#1044 = ORIENTED_EDGE ( 'NONE', *, *, #84247, .F. ) ;
#1045 = CARTESIAN_POINT ( 'NONE',  ( -3.255809902135000211, 1516.837969789639828, 209.8792719553279937 ) ) ;
#1046 = CARTESIAN_POINT ( 'NONE',  ( -9.503490513250000049, 1386.215136675220037, 200.2136258941289952 ) ) ;
#1047 = CARTESIAN_POINT ( 'NONE',  ( 2.173590492602480051, 1419.636778193369992, 225.2801662438579910 ) ) ;
#1048 = CARTESIAN_POINT ( 'NONE',  ( 7.536498802507920480, 1425.740918852369987, 212.2034145707320079 ) ) ;
#1049 = CARTESIAN_POINT ( 'NONE',  ( -26.63614110428829918, 1451.915376940910164, 135.4244124481140261 ) ) ;
#1050 = ORIENTED_EDGE ( 'NONE', *, *, #94463, .T. ) ;
#1051 = CARTESIAN_POINT ( 'NONE',  ( -16.90339957579946883, 1409.749894849624980, 225.4593229189988222 ) ) ;
#1053 = CARTESIAN_POINT ( 'NONE',  ( 14.72846402789999942, 1488.814055421829835, 193.8574964441980057 ) ) ;
#1052 = CARTESIAN_POINT ( 'NONE',  ( -10.95146640095969914, 1492.561632748999955, 207.2597909512799959 ) ) ;
#1054 = DIRECTION ( 'NONE',  ( 0.000000000000000000, 1.000000000000000000, 0.000000000000000000 ) ) ;
#1055 = CARTESIAN_POINT ( 'NONE',  ( -16.86741971048520128, 1508.492928484489994, 213.3340837003470085 ) ) ;
#1056 = CARTESIAN_POINT ( 'NONE',  ( 9286.692186617183324, 54.07981494723826188, 5933.209537376913431 ) ) ;
#1057 = EDGE_LOOP ( 'NONE', ( #24193, #71471, #42216, #1770 ) ) ;
#1058 = CARTESIAN_POINT ( 'NONE',  ( -4.923540592713549380, 1408.758099391689939, 270.4264005896910135 ) ) ;
#1059 = CARTESIAN_POINT ( 'NONE',  ( -0.7533003905399979772, 1516.992029636990083, 208.3816250717139837 ) ) ;
#1060 = CARTESIAN_POINT ( 'NONE',  ( 12.66870000556460063, 1420.756754707929758, 231.4278130761680075 ) ) ;
#1061 = CARTESIAN_POINT ( 'NONE',  ( -2.820595776548121325, 1448.944293396918511, 184.2202240992435236 ) ) ;
#1063 = ORIENTED_EDGE ( 'NONE', *, *, #85947, .T. ) ;
#1062 = CARTESIAN_POINT ( 'NONE',  ( -4.743735107867810719, 1366.962391455512034, 208.3718459617061285 ) ) ;
#1064 = ORIENTED_EDGE ( 'NONE', *, *, #95879, .F. ) ;
#1065 = CARTESIAN_POINT ( 'NONE',  ( -23.55029577264210161, 1410.981915973860168, 210.4743339238279987 ) ) ;
#1066 = CARTESIAN_POINT ( 'NONE',  ( -0.2881951457637970115, 1409.862531581090025, 185.0446401549079951 ) ) ;
#1067 = CARTESIAN_POINT ( 'NONE',  ( 8.742163716520650412E-12, 1408.913060387359792, 224.1216835645979870 ) ) ;
#1068 = CARTESIAN_POINT ( 'NONE',  ( -10.60629226371171363, 1406.913668871433856, 266.9166996103302836 ) ) ;
#1069 = CARTESIAN_POINT ( 'NONE',  ( -19.79232061065411230, 1436.421083345947181, 145.6892389591389758 ) ) ;
#1070 = CARTESIAN_POINT ( 'NONE',  ( -20.24778872499999949, 1425.809854017930093, 221.9168427389980138 ) ) ;
#1071 = CIRCLE ( 'NONE', #13577, 1.000000000000000888 ) ;
#1072 = CARTESIAN_POINT ( 'NONE',  ( 28.26910033551460089, 1468.093474929750073, 269.2153630842319672 ) ) ;
#1073 = CIRCLE ( 'NONE', #8153, 2.000001664945928237 ) ;
#1074 = CARTESIAN_POINT ( 'NONE',  ( -2.606055286189628450, 1466.874310772752096, 235.1271370871118336 ) ) ;
#1075 = CARTESIAN_POINT ( 'NONE',  ( -16.93175146515636698, 1421.930406924298040, 226.8423588672406481 ) ) ;
#1076 = CARTESIAN_POINT ( 'NONE',  ( 2.477986732234999767, 1516.922519270759949, 205.8529865360470126 ) ) ;
#1077 = VERTEX_POINT ( 'NONE', #18891 ) ;
#1078 = CARTESIAN_POINT ( 'NONE',  ( 22.30287194801498529, 1411.052071534360493, 215.4069906866415067 ) ) ;
#1079 = CARTESIAN_POINT ( 'NONE',  ( 1.478215794333419986, 1479.409301536299836, 182.3215185385770098 ) ) ;
#1080 = CARTESIAN_POINT ( 'NONE',  ( 22.81124892260000081, 1409.735994817030132, 208.6040538833909750 ) ) ;
#1081 = ORIENTED_EDGE ( 'NONE', *, *, #10293, .T. ) ;
#1082 = CARTESIAN_POINT ( 'NONE',  ( 4.303235405216580212, 1508.728291632010041, 205.3334392574930121 ) ) ;
#1083 = CARTESIAN_POINT ( 'NONE',  ( 25.70093099836839912, 1451.138728924780025, 136.7959740386000078 ) ) ;
#1084 = B_SPLINE_SURFACE_WITH_KNOTS ( 'NONE', 5, 5, ( 
 ( #42749, #102620, #93139, #762, #85849, #103180 ),
 ( #34890, #218, #51153, #9687, #84733, #92581 ),
 ( #33232, #25920, #67975, #26482, #60118, #94804 ),
 ( #15853, #33779, #18079, #52274, #42199, #76350 ),
 ( #75802, #78002, #24807, #32689, #110499, #109953 ),
 ( #66869, #100977, #24273, #102083, #67421, #101520 ),
 ( #25366, #70203, #78561, #19744, #46081, #11906 ),
 ( #105977, #61246, #70749, #11367, #10810, #46631 ),
 ( #12446, #89158, #54491, #28149, #104860, #88626 ) ),
 .UNSPECIFIED., .F., .F., .F.,
 ( 6, 3, 6 ),
 ( 6, 6 ),
 ( 0.000000000000000000, 5.531936552890000414, 12.17660274970000067 ),
 ( 0.000000000000000000, 1.000000000000000000 ),
 .UNSPECIFIED. ) ;
#1085 = CARTESIAN_POINT ( 'NONE',  ( -4.733838392061969991, 1508.551704408389924, 212.7087210097289756 ) ) ;
#1086 = CARTESIAN_POINT ( 'NONE',  ( -13.39809219260000006, 1386.967483829560024, 218.7383260501090092 ) ) ;
#1087 = DIRECTION ( 'NONE',  ( 0.9977304882603014180, -0.06733403890946067227, 0.000000000000000000 ) ) ;
#1088 = CARTESIAN_POINT ( 'NONE',  ( 17.47690429329999873, 1409.523367334130171, 194.5251149749979902 ) ) ;
#1089 = CARTESIAN_POINT ( 'NONE',  ( 13.14421740897469704, 1444.740067931810472, 164.8757063741590230 ) ) ;
#1090 = CARTESIAN_POINT ( 'NONE',  ( 3.464405900125376192, 1439.692844575363779, 184.4811232741128606 ) ) ;
#1092 = CARTESIAN_POINT ( 'NONE',  ( -19.21510248855428671, 1425.233830981570009, 223.8702727496656166 ) ) ;
#1091 = CARTESIAN_POINT ( 'NONE',  ( 30.04668324475564489, 1524.739563915922872, 195.9292732422738084 ) ) ;
#1093 = CARTESIAN_POINT ( 'NONE',  ( -16.50400130224786466, 1525.907212628473644, 181.9890130758379030 ) ) ;
#1094 = CARTESIAN_POINT ( 'NONE',  ( -0.2712433553410000253, 1477.454346902830139, 230.1237008569979992 ) ) ;
#1095 = CARTESIAN_POINT ( 'NONE',  ( -10.13100692099999911, 1382.082910451279986, 217.5460056582589914 ) ) ;
#1096 = CARTESIAN_POINT ( 'NONE',  ( 12.36909147134636200, 1420.627402783089792, 231.5461179624636827 ) ) ;
#1097 = ORIENTED_EDGE ( 'NONE', *, *, #75681, .T. ) ;
#1098 = CARTESIAN_POINT ( 'NONE',  ( -1.336192060408252891, 1526.382868172863937, 178.6759496289172091 ) ) ;
#1099 = CARTESIAN_POINT ( 'NONE',  ( 11.86610049460949945, 1432.336025080309810, 149.9824239092829998 ) ) ;
#1100 = CARTESIAN_POINT ( 'NONE',  ( -0.3086018725757560532, 1408.964127551420006, 232.0914413854790155 ) ) ;
#1101 = CARTESIAN_POINT ( 'NONE',  ( -11.29470234270000084, 1390.474510999679978, 203.7985412330889972 ) ) ;
#1102 = CARTESIAN_POINT ( 'NONE',  ( 1.493039702043341022, 1421.445368576706869, 193.7871365012589706 ) ) ;
#1103 = CARTESIAN_POINT ( 'NONE',  ( -4.326994892130199055, 1515.158502928330108, 209.0793308605450136 ) ) ;
#1104 = ADVANCED_FACE ( 'NONE', ( #87795 ), #91996, .T. ) ;
#1105 = CARTESIAN_POINT ( 'NONE',  ( -8.800012970690000103, 1452.709869713229864, 209.1218459616979999 ) ) ;
#1106 = CARTESIAN_POINT ( 'NONE',  ( -14.01525996361490023, 1415.677402202029953, 204.0303134510289738 ) ) ;
#1108 = EDGE_CURVE ( 'NONE', #61133, #15891, #6544, .T. ) ;
#1107 = CARTESIAN_POINT ( 'NONE',  ( 11.03413976350000070, 1433.575028546920066, 151.7351373796979885 ) ) ;
#1109 = CARTESIAN_POINT ( 'NONE',  ( 3.268607919819999985, 1455.844446582929777, 219.6133833292979887 ) ) ;
#1110 = FACE_OUTER_BOUND ( 'NONE', #108740, .T. ) ;
#1111 = CARTESIAN_POINT ( 'NONE',  ( 18.25142110790000061, 1430.901022324190080, 200.8464198818790010 ) ) ;
#1112 = CARTESIAN_POINT ( 'NONE',  ( 22.92687821287369943, 1507.614846683499991, 210.5904746357119848 ) ) ;
#1113 = CARTESIAN_POINT ( 'NONE',  ( 9.724852847713158610, 1462.948292999750265, 211.0616404486619899 ) ) ;
#1114 = CARTESIAN_POINT ( 'NONE',  ( -9.700213616599999256, 1486.381094227929907, 183.3052980329979960 ) ) ;
#1115 = CARTESIAN_POINT ( 'NONE',  ( 33.28034951413929576, 1522.862737210649584, 217.4407153818819438 ) ) ;
#1116 = CARTESIAN_POINT ( 'NONE',  ( -29.14871631793969797, 1509.943938004060101, 200.6668815711279876 ) ) ;
#1117 = CARTESIAN_POINT ( 'NONE',  ( 21.05081438130000038, 1449.791259190219989, 221.6945081341980313 ) ) ;
#1118 = EDGE_CURVE ( 'NONE', #65949, #81284, #12787, .T. ) ;
#1119 = CARTESIAN_POINT ( 'NONE',  ( 2.500000000000000000, 1448.210448412289907, 170.5244215879980061 ) ) ;
#1120 = CARTESIAN_POINT ( 'NONE',  ( 25.18702156009318927, 1436.605886283166228, 137.6040374641183348 ) ) ;
#1121 = CARTESIAN_POINT ( 'NONE',  ( -1.448833437790000067, 1515.064791419390076, 204.7923971473389884 ) ) ;
#1122 = CARTESIAN_POINT ( 'NONE',  ( -19.58884344854149973, 1465.811382644940068, 204.1485388013770148 ) ) ;
#1123 = CARTESIAN_POINT ( 'NONE',  ( -2.865911554774999814, 1516.906233342200039, 212.5838411289170153 ) ) ;
#1124 = CARTESIAN_POINT ( 'NONE',  ( -13.94196614533020018, 1421.875924885620179, 203.6998106941310027 ) ) ;
#1125 = CARTESIAN_POINT ( 'NONE',  ( 8.723134474349999223, 1451.781317889190177, 212.2855316608589931 ) ) ;
#1127 = EDGE_LOOP ( 'NONE', ( #104674, #75950, #35545, #11204 ) ) ;
#1126 = CARTESIAN_POINT ( 'NONE',  ( 17.96785475010000255, 1431.047211114990205, 205.7578563200790143 ) ) ;
#1128 = CARTESIAN_POINT ( 'NONE',  ( -0.9043165181340000469, 1416.826388557929931, 228.0290525373980017 ) ) ;
#1129 = CARTESIAN_POINT ( 'NONE',  ( -8.083483728235815846, 1386.109445660887104, 199.6283091834757215 ) ) ;
#1130 = CARTESIAN_POINT ( 'NONE',  ( -4.475591295720000140, 1474.980283356190057, 199.4186445563689745 ) ) ;
#1132 = ORIENTED_EDGE ( 'NONE', *, *, #72781, .T. ) ;
#1131 = CARTESIAN_POINT ( 'NONE',  ( -37.84675541842290158, 1450.538956397279890, 134.0999999985309898 ) ) ;
#1133 = CARTESIAN_POINT ( 'NONE',  ( -5.469245208306690920, 1508.551704408389924, 219.5679309264459960 ) ) ;
#1134 = EDGE_LOOP ( 'NONE', ( #19550, #98250, #54353, #73848 ) ) ;
#1135 = FACE_OUTER_BOUND ( 'NONE', #76793, .T. ) ;
#1136 = CARTESIAN_POINT ( 'NONE',  ( -13.26126580242469899, 1390.209151648439956, 212.6158348635119921 ) ) ;
#1137 = CARTESIAN_POINT ( 'NONE',  ( 5.104653541605128630, 1445.782371245855984, 201.6469468901138953 ) ) ;
#1138 = DIRECTION ( 'NONE',  ( -0.9147450530333530727, 0.03449475076686789321, 0.4025563316115395862 ) ) ;
#1139 = CARTESIAN_POINT ( 'NONE',  ( -2.831065174598700551, 1367.763066558967012, 208.7333235891643142 ) ) ;
#1140 = CARTESIAN_POINT ( 'NONE',  ( -108.8427904636022134, 1381.850845790319909, 310.6994421841279745 ) ) ;
#1141 = CARTESIAN_POINT ( 'NONE',  ( -12.26108091377107634, 1377.626920165065258, 208.0100024370453298 ) ) ;
#1142 = DIRECTION ( 'NONE',  ( -0.7454942576402798782, -1.849942558231146277E-14, 0.6665120492724555534 ) ) ;
#1143 = DIRECTION ( 'NONE',  ( 0.000000000000000000, 0.000000000000000000, 1.000000000000000000 ) ) ;
#1144 = CARTESIAN_POINT ( 'NONE',  ( -86.70549396914439910, 1385.182048704240060, 290.2386611732610504 ) ) ;
#1145 = EDGE_CURVE ( 'NONE', #38215, #32285, #36581, .T. ) ;
#1146 = CARTESIAN_POINT ( 'NONE',  ( -9.946516861848831326, 1391.913060387289988, 214.5797999757839989 ) ) ;
#1147 = CARTESIAN_POINT ( 'NONE',  ( -32.53397683490000247, 1379.726329037039932, 216.1069825312089847 ) ) ;
#1148 = ORIENTED_EDGE ( 'NONE', *, *, #73078, .F. ) ;
#1149 = CARTESIAN_POINT ( 'NONE',  ( -15.78459950990369975, 1409.489682787220090, 225.5863767987009965 ) ) ;
#1151 = ORIENTED_EDGE ( 'NONE', *, *, #27606, .F. ) ;
#1150 = CARTESIAN_POINT ( 'NONE',  ( -4.378911555961889412, 1438.826708660780014, 227.2015615265439976 ) ) ;
#1152 = CARTESIAN_POINT ( 'NONE',  ( 5.622310450973170504, 1467.227804191469886, 217.3393949240599738 ) ) ;
#1153 = ORIENTED_EDGE ( 'NONE', *, *, #25538, .F. ) ;
#1154 = EDGE_CURVE ( 'NONE', #30294, #42497, #37115, .T. ) ;
#1155 = CARTESIAN_POINT ( 'NONE',  ( 19.25039672899999843, 1455.004482529790039, 207.2621563279390102 ) ) ;
#1156 = CARTESIAN_POINT ( 'NONE',  ( -6.674371810360079316, 1362.851205800406888, 210.6218459617142003 ) ) ;
#1157 = CYLINDRICAL_SURFACE ( 'NONE', #96556, 2.000000000000003553 ) ;
#1158 = CARTESIAN_POINT ( 'NONE',  ( 35.60280822696602598, 1457.100005120390506, 269.5399490414274055 ) ) ;
#1159 = CARTESIAN_POINT ( 'NONE',  ( -30.04822308544821041, 1524.382868172804365, 221.7633950662771838 ) ) ;
#1160 = DIRECTION ( 'NONE',  ( 0.000000000000000000, -2.700129756073415263E-15, -1.000000000000000000 ) ) ;
#1161 = CARTESIAN_POINT ( 'NONE',  ( -10887.13479812350670, -2340.220200558883789, 7538.395907487779368 ) ) ;
#1162 = CARTESIAN_POINT ( 'NONE',  ( 21.56441682630240209, 1490.297454983860234, 209.3949090393569747 ) ) ;
#1163 = CARTESIAN_POINT ( 'NONE',  ( -20.79162153139938951, 1507.840283869027871, 228.0156022542989263 ) ) ;
#1164 = CARTESIAN_POINT ( 'NONE',  ( -7.811405798887459895, 1367.739269854435861, 210.6218459616991936 ) ) ;
#1165 = CARTESIAN_POINT ( 'NONE',  ( 0.5801875626090010618, 1457.903154489290046, 199.5761716166789768 ) ) ;
#1166 = CARTESIAN_POINT ( 'NONE',  ( -6.563254928984999736, 1517.139039350860003, 206.6385234782069915 ) ) ;
#1167 = CARTESIAN_POINT ( 'NONE',  ( 3.897009773650441211, 1519.551704408389924, 231.0205787112126075 ) ) ;
#1168 = CARTESIAN_POINT ( 'NONE',  ( -2.500000000000000000, 1438.826994403640128, 157.7142568068980211 ) ) ;
#1169 = CARTESIAN_POINT ( 'NONE',  ( -2.952024859200000240, 1496.639021482089902, 198.1365015686990034 ) ) ;
#1171 = EDGE_LOOP ( 'NONE', ( #75646, #66184, #110162, #28068 ) ) ;
#1170 = CARTESIAN_POINT ( 'NONE',  ( -2.178754852690000021, 1496.647359717190056, 220.9005516230989770 ) ) ;
#1172 = AXIS2_PLACEMENT_3D ( 'NONE', #32306, #7103, #49123 ) ;
#1173 = CARTESIAN_POINT ( 'NONE',  ( 13.08147543293499915, 1513.492015765619954, 222.9104281842669764 ) ) ;
#1174 = ORIENTED_EDGE ( 'NONE', *, *, #86900, .F. ) ;
#1175 = DIRECTION ( 'NONE',  ( -0.9998780014336184907, 0.000000000000000000, 0.01561993114942984012 ) ) ;
#1176 = CARTESIAN_POINT ( 'NONE',  ( -24.70281712020000242, 1449.797141331690000, 204.5697651700980089 ) ) ;
#1178 = CARTESIAN_POINT ( 'NONE',  ( 16.82553512313559807, 1410.448925550840158, 191.9397864464299914 ) ) ;
#1177 = CARTESIAN_POINT ( 'NONE',  ( -11.57305820287779952, 1425.905705694889775, 139.7073144656000068 ) ) ;
#1179 = CARTESIAN_POINT ( 'NONE',  ( -4.027697264044999947, 1516.766397346390022, 212.0005392193770035 ) ) ;
#1180 = CARTESIAN_POINT ( 'NONE',  ( 24.41443735958936401, 1509.880090222447734, 191.6102450087062152 ) ) ;
#1181 = CARTESIAN_POINT ( 'NONE',  ( 12.53380499169999851, 1442.773887286369927, 169.4755105685979970 ) ) ;
#1182 = CARTESIAN_POINT ( 'NONE',  ( -13.60515979240000028, 1408.134947171630074, 264.8398025118980286 ) ) ;
#1183 = CARTESIAN_POINT ( 'NONE',  ( 15.67891837840150160, 1509.462974027039991, 234.0097172023010046 ) ) ;
#1184 = CARTESIAN_POINT ( 'NONE',  ( 18.22805055419890152, 1459.311389626190021, 227.8763770136359881 ) ) ;
#1185 = CARTESIAN_POINT ( 'NONE',  ( -4.992439150849999230, 1391.624323207190173, 214.5505945479090144 ) ) ;
#1186 = CARTESIAN_POINT ( 'NONE',  ( -34.47180251477740143, 1437.054646050100018, 136.5467630333359921 ) ) ;
#1187 = ORIENTED_EDGE ( 'NONE', *, *, #109085, .T. ) ;
#1188 = CARTESIAN_POINT ( 'NONE',  ( 6.220296828871760830, 1397.477110675040194, 220.4683221253430077 ) ) ;
#1189 = CARTESIAN_POINT ( 'NONE',  ( 10.02612625315829931, 1461.114985608630150, 207.7185774112350032 ) ) ;
#1190 = CARTESIAN_POINT ( 'NONE',  ( -16.32194098420000117, 1459.453082325529977, 228.9511321261979901 ) ) ;
#1191 = ORIENTED_EDGE ( 'NONE', *, *, #89082, .F. ) ;
#1192 = EDGE_LOOP ( 'NONE', ( #45908, #29426, #27970, #23465, #53686, #75685 ) ) ;
#1193 = CARTESIAN_POINT ( 'NONE',  ( -20.58427237330537096, 1512.187213306747481, 216.4826520421591738 ) ) ;
#1194 = CARTESIAN_POINT ( 'NONE',  ( -3.134082760970000159, 1421.411057458130017, 144.1516174827979739 ) ) ;
#1195 = ORIENTED_EDGE ( 'NONE', *, *, #21286, .F. ) ;
#1196 = CARTESIAN_POINT ( 'NONE',  ( -7.680767148276910206, 1508.410451920919968, 219.5486563066939993 ) ) ;
#1197 = CARTESIAN_POINT ( 'NONE',  ( -14.73343723154779994, 1508.551704405130067, 210.0752011545839935 ) ) ;
#1198 = CARTESIAN_POINT ( 'NONE',  ( 0.000000000000000000, 1518.913060387330006, 209.1218459616979999 ) ) ;
#1199 = CARTESIAN_POINT ( 'NONE',  ( -3.859940384109999734, 1461.192844946329842, 234.5475963274979847 ) ) ;
#1200 = DIRECTION ( 'NONE',  ( -1.836970198721029688E-16, -1.000000000000000000, 0.000000000000000000 ) ) ;
#1201 = CARTESIAN_POINT ( 'NONE',  ( 9.592369369698889869, 1451.333035786799883, 207.7642936628679990 ) ) ;
#1202 = CARTESIAN_POINT ( 'NONE',  ( 19.04547816490000045, 1456.669743087390088, 205.4226615881689781 ) ) ;
#1203 = CARTESIAN_POINT ( 'NONE',  ( -97.03291587454688738, 1384.864417997589953, 295.5831496746029643 ) ) ;
#1204 = EDGE_LOOP ( 'NONE', ( #64781, #77382, #86140, #102380, #14395, #88297, #13141, #23084, #98114, #72274 ) ) ;
#1205 = CARTESIAN_POINT ( 'NONE',  ( -4.037378294184999383, 1516.688761843659904, 202.5730239910470232 ) ) ;
#1206 = CARTESIAN_POINT ( 'NONE',  ( 4.618583391875000110, 1516.939762005280045, 209.1087859301640322 ) ) ;
#1207 = ORIENTED_EDGE ( 'NONE', *, *, #69473, .T. ) ;
#1208 = CARTESIAN_POINT ( 'NONE',  ( 11.75126242882070038, 1426.765985215520004, 145.1646422661519864 ) ) ;
#1209 = DIRECTION ( 'NONE',  ( 1.000000000000000000, 0.000000000000000000, 0.000000000000000000 ) ) ;
#1210 = ORIENTED_EDGE ( 'NONE', *, *, #80921, .F. ) ;
#1211 = CARTESIAN_POINT ( 'NONE',  ( -1.440135193375450040, 1453.598502451769946, 183.7985014132709978 ) ) ;
#1212 = CARTESIAN_POINT ( 'NONE',  ( -13.14421740897469704, 1443.086052842850677, 164.8757063741590230 ) ) ;
#1213 = CARTESIAN_POINT ( 'NONE',  ( 4.916348328289999792, 1507.184349319130206, 235.7144663231979962 ) ) ;
#1214 = CARTESIAN_POINT ( 'NONE',  ( -11.02689301977250125, 1462.508944275419935, 208.4529861560579889 ) ) ;
#1215 = CARTESIAN_POINT ( 'NONE',  ( -4.976708597980000093, 1421.169633119030095, 186.3323561761980045 ) ) ;
#1216 = CARTESIAN_POINT ( 'NONE',  ( 3.048590950930369914, 1410.469311925999818, 269.3357931879770035 ) ) ;
#1217 = CARTESIAN_POINT ( 'NONE',  ( -0.4354997994421860308, 1517.051704408389924, 216.8053818660609977 ) ) ;
#1218 = CARTESIAN_POINT ( 'NONE',  ( -7.027808362610000081, 1475.334978324289978, 201.5104037304890028 ) ) ;
#1219 = CARTESIAN_POINT ( 'NONE',  ( 10.45331111600000185, 1492.246367015789929, 213.2054363916189743 ) ) ;
#1220 = CARTESIAN_POINT ( 'NONE',  ( -16.52535657530000179, 1379.585817439869743, 208.2843806234300246 ) ) ;
#1221 = CARTESIAN_POINT ( 'NONE',  ( 8.995217975349083517, 1425.047741747077225, 195.6353441828489110 ) ) ;
#1223 = CARTESIAN_POINT ( 'NONE',  ( 15.32936212569999945, 1453.152003547329969, 195.3739065139980084 ) ) ;
#1222 = CARTESIAN_POINT ( 'NONE',  ( -21.10523119420000171, 1505.940419546890098, 209.1830678612959957 ) ) ;
#1224 = CARTESIAN_POINT ( 'NONE',  ( -68.75533708345575690, 1379.747887839387431, 280.3280563178295210 ) ) ;
#1225 = CARTESIAN_POINT ( 'NONE',  ( 17.95685989722359821, 1422.251379684970061, 225.1386422400370009 ) ) ;
#1226 = CARTESIAN_POINT ( 'NONE',  ( -10.70847609427080016, 1506.854789404229905, 189.5201119528840081 ) ) ;
#1227 = VERTEX_POINT ( 'NONE', #62367 ) ;
#1228 = CARTESIAN_POINT ( 'NONE',  ( 29.86461515634908892, 1525.960063244516959, 197.2746849027934957 ) ) ;
#1229 = CARTESIAN_POINT ( 'NONE',  ( -21.15382147014703662, 1525.425665131969254, 234.2558076767862190 ) ) ;
#1230 = CARTESIAN_POINT ( 'NONE',  ( -2.898745121111036660, 1484.370110010407188, 183.3086963780446581 ) ) ;
#1231 = CARTESIAN_POINT ( 'NONE',  ( -14.75858115399999981, 1415.739699861750069, 212.8702772705990185 ) ) ;
#1233 = ORIENTED_EDGE ( 'NONE', *, *, #80838, .T. ) ;
#1232 = CARTESIAN_POINT ( 'NONE',  ( -0.5056391281412709882, 1515.143808641139913, 204.7944662863439760 ) ) ;
#1234 = CARTESIAN_POINT ( 'NONE',  ( -15.84297102958074532, 1415.885071821111978, 209.7209629398730328 ) ) ;
#1235 = CARTESIAN_POINT ( 'NONE',  ( -24.23599894299999846, 1443.366957020490190, 211.5779768989180241 ) ) ;
#1236 = CARTESIAN_POINT ( 'NONE',  ( -11.81055660949999897, 1428.757038210530027, 148.7013752713980068 ) ) ;
#1237 = CARTESIAN_POINT ( 'NONE',  ( 19.96736869389999924, 1474.314440584889780, 212.0838811099789893 ) ) ;
#1238 = CARTESIAN_POINT ( 'NONE',  ( -11.01732325727999928, 1462.230258711259921, 209.6174576145919843 ) ) ;
#1239 = CARTESIAN_POINT ( 'NONE',  ( -13.57816498729999921, 1379.569537801319939, 207.8818212186490086 ) ) ;
#1240 = CARTESIAN_POINT ( 'NONE',  ( 13.16277144537490074, 1428.831732683049950, 222.5358085910779948 ) ) ;
#1241 = CARTESIAN_POINT ( 'NONE',  ( -15.56957305056499941, 1512.571022561239943, 222.6873122058669878 ) ) ;
#1242 = CARTESIAN_POINT ( 'NONE',  ( 11.16993257140000040, 1412.737055366430013, 229.4626520222979877 ) ) ;
#1243 = CARTESIAN_POINT ( 'NONE',  ( -11.63790511286740070, 1482.566214428189824, 206.5868431706369961 ) ) ;
#1244 = CARTESIAN_POINT ( 'NONE',  ( -16.80253214529999894, 1461.096644362530014, 228.2779737265979918 ) ) ;
#1245 = CARTESIAN_POINT ( 'NONE',  ( -1.136004312195000088, 1516.815173273089840, 206.2562091229970065 ) ) ;
#1246 = CARTESIAN_POINT ( 'NONE',  ( 23.35190786599999768, 1411.509783186830191, 269.4730611836980074 ) ) ;
#1247 = CARTESIAN_POINT ( 'NONE',  ( 23.17024198529999879, 1435.306528354219836, 138.2719568257980143 ) ) ;
#1248 = CARTESIAN_POINT ( 'NONE',  ( 18.06189968659999678, 1430.309388431030129, 192.0308204566979953 ) ) ;
#1249 = CARTESIAN_POINT ( 'NONE',  ( -23.46079095940000059, 1434.934186800890075, 213.0598433132079776 ) ) ;
#1250 = EDGE_CURVE ( 'NONE', #83385, #104688, #28736, .T. ) ;
#1251 = CARTESIAN_POINT ( 'NONE',  ( -10.25304834626500039, 1513.301704408390151, 214.4251468100669911 ) ) ;
#1252 = CARTESIAN_POINT ( 'NONE',  ( 17.73223409949387275, 1524.152444737676660, 237.7705223289944172 ) ) ;
#1253 = CARTESIAN_POINT ( 'NONE',  ( -41.66134498533040187, 1443.796928201230003, 135.6885309535949773 ) ) ;
#1254 = CARTESIAN_POINT ( 'NONE',  ( -6.244762112600730219, 1407.784308377609932, 197.6511685975619912 ) ) ;
#1255 = CARTESIAN_POINT ( 'NONE',  ( -15.39978337890000049, 1415.475588077589919, 208.2578686251449938 ) ) ;
#1256 = CARTESIAN_POINT ( 'NONE',  ( -12.41994595579999938, 1442.757755574029943, 186.2442043369979956 ) ) ;
#1257 = ADVANCED_FACE ( 'NONE', ( #14112 ), #32095, .T. ) ;
#1258 = CARTESIAN_POINT ( 'NONE',  ( -3.792791800014749803, 1485.262872875560106, 197.8389773509790075 ) ) ;
#1259 = CARTESIAN_POINT ( 'NONE',  ( -30.79851420400000350, 1435.573204670519999, 135.5995097962980083 ) ) ;
#1260 = DIRECTION ( 'NONE',  ( -0.1867376760110624201, -0.7251253628122718009, 0.6628138868222048785 ) ) ;
#1261 = EDGE_LOOP ( 'NONE', ( #28337, #104669, #33068, #9186 ) ) ;
#1262 = CARTESIAN_POINT ( 'NONE',  ( -2.564633821555000193, 1511.308638870219966, 201.5496530815769916 ) ) ;
#1263 = CARTESIAN_POINT ( 'NONE',  ( -12.51401920766459952, 1409.350059567480230, 200.9511622912029907 ) ) ;
#1264 = CARTESIAN_POINT ( 'NONE',  ( 14.60984432997775251, 1434.489065057944799, 221.3746616866943100 ) ) ;
#1265 = CARTESIAN_POINT ( 'NONE',  ( 32.38845791999495560, 1518.913060387330006, 202.1182848005512085 ) ) ;
#1266 = AXIS2_PLACEMENT_3D ( 'NONE', #76000, #101734, #93889 ) ;
#1267 = CARTESIAN_POINT ( 'NONE',  ( -12.67405358299999918, 1474.477408728030014, 268.9829747063979539 ) ) ;
#1268 = FACE_OUTER_BOUND ( 'NONE', #50912, .T. ) ;
#1269 = LINE ( 'NONE', #35408, #31651 ) ;
#1270 = CARTESIAN_POINT ( 'NONE',  ( -24.51545692169827362, 1444.726069595008994, 210.9879020001179697 ) ) ;
#1271 = CARTESIAN_POINT ( 'NONE',  ( -77.89971934322829838, 1384.643069586999900, 302.3865563694679963 ) ) ;
#1272 = CARTESIAN_POINT ( 'NONE',  ( -18.95953277411649651, 1384.948900335349890, 201.3970670253520154 ) ) ;
#1273 = CARTESIAN_POINT ( 'NONE',  ( 18.27461809169380302, 1424.830734655089827, 227.7279702984320124 ) ) ;
#1274 = CARTESIAN_POINT ( 'NONE',  ( 21.32829263799999708, 1509.431654392129985, 227.8062006340979906 ) ) ;
#1275 = CARTESIAN_POINT ( 'NONE',  ( 14.47057979809999928, 1463.299097360029918, 223.0641482907979878 ) ) ;
#1276 = CARTESIAN_POINT ( 'NONE',  ( -26.33121976050560065, 1495.363534167619946, 211.7508342357739934 ) ) ;
#1277 = CARTESIAN_POINT ( 'NONE',  ( 4.287908595200000228, 1515.369371658090131, 208.3885716294179815 ) ) ;
#1278 = CARTESIAN_POINT ( 'NONE',  ( -8.125988388849998856, 1509.268893885830039, 180.2859049925980059 ) ) ;
#1279 = CARTESIAN_POINT ( 'NONE',  ( -23.87261416360000155, 1410.668553464130127, 207.8050958171579907 ) ) ;
#1280 = CARTESIAN_POINT ( 'NONE',  ( 16.76079635960000047, 1415.087818611729972, 206.4452941520080174 ) ) ;
#1281 = CARTESIAN_POINT ( 'NONE',  ( 5.027891267510000262, 1485.388390063490078, 218.6205902490090125 ) ) ;
#1282 = CARTESIAN_POINT ( 'NONE',  ( 10.57494700539420052, 1480.041567197929908, 207.7444763255160183 ) ) ;
#1283 = CARTESIAN_POINT ( 'NONE',  ( 1.643576684049999903, 1435.943783413959864, 150.4860296878979682 ) ) ;
#1285 = AXIS2_PLACEMENT_3D ( 'NONE', #34811, #68998, #94716 ) ;
#1284 = B_SPLINE_CURVE_WITH_KNOTS ( 'NONE', 3,
 ( #68712, #35081, #51899, #102816, #69263, #9338 ),
 .UNSPECIFIED., .F., .F.,
 ( 4, 2, 4 ),
 ( 1.219745810294720132E-06, 0.01184121947742510124, 0.02355703793478339941 ),
 .UNSPECIFIED. ) ;
#1286 = CARTESIAN_POINT ( 'NONE',  ( 0.7066465098517540344, 1461.574489129789981, 230.4559209505140132 ) ) ;
#1287 = CARTESIAN_POINT ( 'NONE',  ( 16.62425451295026946, 1524.075000532257491, 180.5391494807173842 ) ) ;
#1288 = CARTESIAN_POINT ( 'NONE',  ( 9.738308991446089635, 1493.400139332539993, 188.2659903719689680 ) ) ;
#1289 = CARTESIAN_POINT ( 'NONE',  ( -8.219449892280000114, 1384.003553985900226, 199.7324766670489851 ) ) ;
#1290 = CARTESIAN_POINT ( 'NONE',  ( 0.7174281048909999514, 1414.384036990830054, 233.3111233936980113 ) ) ;
#1291 = CARTESIAN_POINT ( 'NONE',  ( 9.815434228962379493, 1435.417726128900085, 208.8923042721449974 ) ) ;
#1292 = CARTESIAN_POINT ( 'NONE',  ( -11.75194039070000152, 1490.261998080790136, 210.2102649680689979 ) ) ;
#1293 = FACE_OUTER_BOUND ( 'NONE', #104183, .T. ) ;
#1294 = CARTESIAN_POINT ( 'NONE',  ( 2.480813884984999884, 1517.051603658920158, 204.1089070683270279 ) ) ;
#1295 = CARTESIAN_POINT ( 'NONE',  ( 4.180945349216710127, 1429.153325867737976, 216.2854025766479822 ) ) ;
#1296 = CARTESIAN_POINT ( 'NONE',  ( 16.21240999383499570, 1514.452905717119847, 194.1945360481670093 ) ) ;
#1297 = CARTESIAN_POINT ( 'NONE',  ( -19.53786426059057746, 1501.977400791986611, 181.5239794925695946 ) ) ;
#1298 = CARTESIAN_POINT ( 'NONE',  ( 2.798741256239999586, 1509.010794585629810, 238.1786444319979807 ) ) ;
#1299 = CARTESIAN_POINT ( 'NONE',  ( 8.551703227357981163, 1503.794247392529996, 218.6779256640890026 ) ) ;
#1300 = CARTESIAN_POINT ( 'NONE',  ( -10.04607665504151370, 1422.599490385782929, 210.6606566106900118 ) ) ;
#1303 = ORIENTED_EDGE ( 'NONE', *, *, #97292, .F. ) ;
#1302 = CARTESIAN_POINT ( 'NONE',  ( -66.37701120922260145, 1379.742216766350111, 277.0613536044180023 ) ) ;
#1301 = CIRCLE ( 'NONE', #74597, 2.000013666866326201 ) ;
#1304 = VERTEX_POINT ( 'NONE', #22492 ) ;
#1305 = CARTESIAN_POINT ( 'NONE',  ( 11.94418194357199958, 1433.568413397649920, 150.1854698904059831 ) ) ;
#1306 = CARTESIAN_POINT ( 'NONE',  ( 21.30905559964021023, 1524.964230758883104, 184.3256122676305893 ) ) ;
#1307 = EDGE_LOOP ( 'NONE', ( #102465, #35282, #41395, #32770 ) ) ;
#1308 = CARTESIAN_POINT ( 'NONE',  ( -0.4151546846821903003, 1512.187213306747481, 174.3106345060153046 ) ) ;
#1309 = CARTESIAN_POINT ( 'NONE',  ( -22.39336929169999735, 1508.437846497230112, 193.8456439799980160 ) ) ;
#1310 = CARTESIAN_POINT ( 'NONE',  ( -7.767687465479999886, 1384.983142744430097, 218.9170564598889825 ) ) ;
#1312 = CARTESIAN_POINT ( 'NONE',  ( 2.205156445730000137, 1428.435894572430016, 91.31218443469779800 ) ) ;
#1311 = CARTESIAN_POINT ( 'NONE',  ( 10.96946812545280103, 1432.347663862999980, 151.7701354189910035 ) ) ;
#1313 = CARTESIAN_POINT ( 'NONE',  ( 13.28903619059999919, 1507.808443900629982, 233.1137254224979927 ) ) ;
#1314 = CARTESIAN_POINT ( 'NONE',  ( 3.162092520659999906, 1488.171764278530190, 182.3076926873980028 ) ) ;
#1315 = CARTESIAN_POINT ( 'NONE',  ( 2.739535155620000051, 1466.840063050689878, 219.4352059655989819 ) ) ;
#1316 = CARTESIAN_POINT ( 'NONE',  ( -24.43504968562070445, 1444.778680445579994, 211.0911670020710176 ) ) ;
#1317 = CARTESIAN_POINT ( 'NONE',  ( 6.950214933285000285, 1517.129577905929864, 211.9934263588270085 ) ) ;
#1318 = CARTESIAN_POINT ( 'NONE',  ( 36.90142499543770072, 1436.372079654780009, 134.0999999968939846 ) ) ;
#1319 = CARTESIAN_POINT ( 'NONE',  ( 32.78250617288045987, 1511.187213306747708, 218.3079823578266314 ) ) ;
#1320 = CARTESIAN_POINT ( 'NONE',  ( 6.781132878754999815, 1512.686126173230150, 201.8548505242569888 ) ) ;
#1321 = EDGE_LOOP ( 'NONE', ( #91856, #48422, #19864, #38432, #109528, #81310, #103020, #40751, #105848, #86397, #80547, #54136, #50283, #42213, #34449, #7573, #54234, #106974, #18075, #43433 ) ) ;
#1322 = CARTESIAN_POINT ( 'NONE',  ( 14.38916750008629997, 1435.820125812520018, 149.8242534154239820 ) ) ;
#1323 = CARTESIAN_POINT ( 'NONE',  ( -18.26023438560000045, 1443.256148476890075, 213.5656046648789754 ) ) ;
#1324 = ORIENTED_EDGE ( 'NONE', *, *, #28391, .T. ) ;
#1325 = VERTEX_POINT ( 'NONE', #56693 ) ;
#1326 = CARTESIAN_POINT ( 'NONE',  ( -7.084879081845000037, 1512.024017243139951, 216.0683601470269934 ) ) ;
#1327 = CARTESIAN_POINT ( 'NONE',  ( 16.67556690833916022, 1513.118420042606658, 196.8779830456916216 ) ) ;
#1328 = CARTESIAN_POINT ( 'NONE',  ( 5.157704406284129827E-09, 1406.911841301380036, 222.1218459627310153 ) ) ;
#1329 = AXIS2_PLACEMENT_3D ( 'NONE', #10990, #55217, #12641 ) ;
#1330 = CARTESIAN_POINT ( 'NONE',  ( -6.554778571775000451, 1516.929962200689943, 216.8412383526069789 ) ) ;
#1331 = CARTESIAN_POINT ( 'NONE',  ( -0.2723979594944390126, 1465.344599497509989, 198.1196121825180114 ) ) ;
#1332 = DIRECTION ( 'NONE',  ( -0.9993779840591179298, 0.0009463129470705568952, 0.03525265195329010254 ) ) ;
#1333 = CARTESIAN_POINT ( 'NONE',  ( -49.27402874327646742, 1379.685930775072848, 238.1797779762692926 ) ) ;
#1334 = CARTESIAN_POINT ( 'NONE',  ( 4.221309089957250293, 1446.219906947470236, 169.0695559285369995 ) ) ;
#1335 =( BOUNDED_CURVE ( )  B_SPLINE_CURVE ( 3, ( #24512, #18735, #33463, #84443 ),
 .UNSPECIFIED., .F., .F. ) 
 B_SPLINE_CURVE_WITH_KNOTS ( ( 4, 4 ),
 ( 4.625649227539959440, 4.863861644479719359 ),
 .UNSPECIFIED. ) 
 CURVE ( )  GEOMETRIC_REPRESENTATION_ITEM ( )  RATIONAL_B_SPLINE_CURVE ( ( 1.000000000000000000, 0.9952768246915880690, 0.9952768246915880690, 1.000000000000000000 ) ) 
 REPRESENTATION_ITEM ( '' )  );
#1336 = CARTESIAN_POINT ( 'NONE',  ( 8.645456105984701267, 1437.915333935219905, 209.8214125568420059 ) ) ;
#1337 = EDGE_LOOP ( 'NONE', ( #26400, #72792, #8720, #28875, #102883, #62231 ) ) ;
#1338 = CARTESIAN_POINT ( 'NONE',  ( -2.881222795715000284, 1516.891731298979948, 206.6444723262370076 ) ) ;
#1339 = ORIENTED_EDGE ( 'NONE', *, *, #56860, .T. ) ;
#1340 = CARTESIAN_POINT ( 'NONE',  ( 23.15392403432699808, 1440.913060387330006, 232.3890819680619870 ) ) ;
#1341 = CARTESIAN_POINT ( 'NONE',  ( -20.05348316079999904, 1509.507670961230133, 230.4164826494980218 ) ) ;
#1342 = ORIENTED_EDGE ( 'NONE', *, *, #58015, .F. ) ;
#1343 = CARTESIAN_POINT ( 'NONE',  ( -7.203718089889590281, 1508.728103933889997, 202.3962606498199932 ) ) ;
#1344 = CARTESIAN_POINT ( 'NONE',  ( -13.85637388489999999, 1409.898955760130093, 190.3611264359980169 ) ) ;
#1345 = CARTESIAN_POINT ( 'NONE',  ( -24.91017436590000145, 1441.730135535790168, 210.4543706807980072 ) ) ;
#1346 = CARTESIAN_POINT ( 'NONE',  ( -0.5495911971522959849, 1422.810403843149970, 192.5012090975810111 ) ) ;
#1347 = CARTESIAN_POINT ( 'NONE',  ( 0.0002660152826350496214, 1396.305602673456860, 196.9300748754315293 ) ) ;
#1348 = CARTESIAN_POINT ( 'NONE',  ( -13.80599379854099951, 1434.979619881170038, 146.4346930281899972 ) ) ;
#1349 = CARTESIAN_POINT ( 'NONE',  ( 3.555115653736739510E-15, 1384.926148861439970, 209.1218459572589836 ) ) ;
#1350 = CARTESIAN_POINT ( 'NONE',  ( -31.34137657934001098, 1512.187213306747481, 221.9025654077414345 ) ) ;
#1352 = CARTESIAN_POINT ( 'NONE',  ( -104.6408027911641483, 1379.604531764216517, 304.0225355773446836 ) ) ;
#1351 = DIRECTION ( 'NONE',  ( -1.755985294532469921E-16, 1.000000000000000000, -1.338183447452831989E-16 ) ) ;
#1353 = AXIS2_PLACEMENT_3D ( 'NONE', #75150, #16294, #109298 ) ;
#1354 = CARTESIAN_POINT ( 'NONE',  ( 7.719392382375000139, 1516.929962200689943, 215.6766245038770080 ) ) ;
#1355 = CARTESIAN_POINT ( 'NONE',  ( -2.492811848245119588, 1429.200768276920144, 200.0866537460539973 ) ) ;
#1356 = DIRECTION ( 'NONE',  ( 0.1115146187057051708, 0.9937625037592048294, -0.0007589052364158857143 ) ) ;
#1357 = CARTESIAN_POINT ( 'NONE',  ( 28.56957134109999785, 1509.608813749330011, 207.7212829969979850 ) ) ;
#1358 = CARTESIAN_POINT ( 'NONE',  ( -7.321193745875000047, 1516.534976163889951, 211.4135222436570132 ) ) ;
#1359 = CARTESIAN_POINT ( 'NONE',  ( 13.61519732589999876, 1409.388513550129801, 192.1720528023979853 ) ) ;
#1360 = CARTESIAN_POINT ( 'NONE',  ( -18.73404851560655615, 1486.221193578838211, 189.0895470789506305 ) ) ;
#1362 = ORIENTED_EDGE ( 'NONE', *, *, #19366, .T. ) ;
#1361 = CARTESIAN_POINT ( 'NONE',  ( -73.55519582189999994, 1385.011955127469946, 298.9534985252589649 ) ) ;
#1363 = CARTESIAN_POINT ( 'NONE',  ( 43.15854606300000285, 1446.267111671710154, 263.9123177541979999 ) ) ;
#1364 = CARTESIAN_POINT ( 'NONE',  ( -4.987078442593329441, 1508.551704408389924, 211.6097810465890063 ) ) ;
#1365 = DIRECTION ( 'NONE',  ( -0.7384854939282339270, 4.128709092058512866E-17, 0.6742693640212139572 ) ) ;
#1366 = CARTESIAN_POINT ( 'NONE',  ( -1.628803710539000082, 1508.952962138009980, 238.4908458976950101 ) ) ;
#1367 = CARTESIAN_POINT ( 'NONE',  ( -20.01739162620000201, 1456.480130098429981, 225.1960475761980263 ) ) ;
#1368 = CIRCLE ( 'NONE', #63973, 1.999999999999997780 ) ;
#1370 = CARTESIAN_POINT ( 'NONE',  ( 17.99896784699780383, 1410.879795390830168, 222.9861481690849985 ) ) ;
#1369 = CARTESIAN_POINT ( 'NONE',  ( 11.58215542740000181, 1432.723885441809898, 151.1956759764979950 ) ) ;
#1371 = CARTESIAN_POINT ( 'NONE',  ( -0.3789282637219999472, 1488.814055421429885, 187.9137241168980097 ) ) ;
#1372 = CARTESIAN_POINT ( 'NONE',  ( -108.8616956595720069, 1383.655566382730058, 311.0497432310580166 ) ) ;
#1373 = ORIENTED_EDGE ( 'NONE', *, *, #31031, .F. ) ;
#1374 = CARTESIAN_POINT ( 'NONE',  ( -5.007588685045000432, 1516.804776704140068, 203.3466091393569855 ) ) ;
#1375 = CARTESIAN_POINT ( 'NONE',  ( 0.5589011644189999517, 1405.751811759530028, 267.5370429348980110 ) ) ;
#1376 = CARTESIAN_POINT ( 'NONE',  ( 27.92328160759999989, 1509.198544193830003, 207.5288794971980053 ) ) ;
#1377 = AXIS2_PLACEMENT_3D ( 'NONE', #103027, #26324, #9531 ) ;
#1378 = CARTESIAN_POINT ( 'NONE',  ( 24.59810391050000078, 1443.913212907020124, 213.1604229849380090 ) ) ;
#1379 = CARTESIAN_POINT ( 'NONE',  ( -24.15153490410000359, 1438.063247892820073, 212.1983423404379892 ) ) ;
#1380 = CARTESIAN_POINT ( 'NONE',  ( 3.466155636220000336, 1466.556171815189828, 219.1989959499990164 ) ) ;
#1381 = FACE_OUTER_BOUND ( 'NONE', #3200, .T. ) ;
#1382 = CARTESIAN_POINT ( 'NONE',  ( -37.98804544047590070, 1440.913060390229930, 256.2617115235140091 ) ) ;
#1383 = CARTESIAN_POINT ( 'NONE',  ( 37.45767776268139926, 1449.247412760440056, 136.3260996822840241 ) ) ;
#1384 = CARTESIAN_POINT ( 'NONE',  ( -1.171202044737849945, 1450.815562201780040, 154.2439547528010166 ) ) ;
#1385 = DIRECTION ( 'NONE',  ( -0.000000000000000000, -1.000000000000000000, 0.000000000000000000 ) ) ;
#1386 = ADVANCED_FACE ( 'NONE', ( #90829 ), #74050, .T. ) ;
#1387 = CARTESIAN_POINT ( 'NONE',  ( 11.33822704553409899, 1479.770480605789999, 209.4503463167290249 ) ) ;
#1388 = CARTESIAN_POINT ( 'NONE',  ( 3.529345253949999872, 1506.116810073189981, 220.6266478869990237 ) ) ;
#1389 = CARTESIAN_POINT ( 'NONE',  ( 19.74164504280149757, 1455.376031929259852, 226.0788368184279875 ) ) ;
#1390 = ORIENTED_EDGE ( 'NONE', *, *, #83101, .T. ) ;
#1391 = CARTESIAN_POINT ( 'NONE',  ( 0.8066080222970000158, 1426.500992774829911, 146.0666368882980066 ) ) ;
#1392 = CARTESIAN_POINT ( 'NONE',  ( 12.06136797880000167, 1433.903288664979982, 146.9203525914979878 ) ) ;
#1393 = CARTESIAN_POINT ( 'NONE',  ( -1.387456962977127395, 1450.687505278765684, 181.9496466349601747 ) ) ;
#1394 = CARTESIAN_POINT ( 'NONE',  ( 14.91734427364780124, 1443.896427911540059, 190.0889645647779957 ) ) ;
#1395 = CARTESIAN_POINT ( 'NONE',  ( -0.8945447425290000698, 1417.298088064829926, 235.8147206259980067 ) ) ;
#1397 = AXIS2_PLACEMENT_3D ( 'NONE', #83042, #57321, #98183 ) ;
#1396 = CARTESIAN_POINT ( 'NONE',  ( 11.41988475489999999, 1502.185962516789914, 211.2997121632290032 ) ) ;
#1398 = CARTESIAN_POINT ( 'NONE',  ( -31.81407709660784988, 1522.382868172863937, 196.2902540610631945 ) ) ;
#1399 = CARTESIAN_POINT ( 'NONE',  ( 8.877586941319998814, 1422.885318649510054, 212.4206501655689863 ) ) ;
#1400 = DIRECTION ( 'NONE',  ( -0.03006000153037464637, -0.4884709562387478665, -0.8720622232496929582 ) ) ;
#1401 = CARTESIAN_POINT ( 'NONE',  ( -18.50064172359999759, 1416.067629290630066, 208.4803912601460070 ) ) ;
#1402 = CARTESIAN_POINT ( 'NONE',  ( -16.70118312301810093, 1414.971390223319986, 209.0342377526849873 ) ) ;
#1403 = CARTESIAN_POINT ( 'NONE',  ( -9.960850764644041178, 1396.260900962979804, 204.3086104707440143 ) ) ;
#1404 = ORIENTED_EDGE ( 'NONE', *, *, #13862, .F. ) ;
#1405 = CARTESIAN_POINT ( 'NONE',  ( -17.28133596328079946, 1410.461149824280028, 225.8190134910500149 ) ) ;
#1406 = CARTESIAN_POINT ( 'NONE',  ( 2.455820327400000114, 1434.541746329560056, 150.3615916412979914 ) ) ;
#1407 = VERTEX_POINT ( 'NONE', #25256 ) ;
#1408 = ORIENTED_EDGE ( 'NONE', *, *, #89707, .F. ) ;
#1409 = CARTESIAN_POINT ( 'NONE',  ( 1.850333291829999949, 1499.742999841690107, 230.3385376657990093 ) ) ;
#1410 = CARTESIAN_POINT ( 'NONE',  ( -15.17407649454405139, 1416.062935498875049, 206.0915010440276660 ) ) ;
#1412 = CARTESIAN_POINT ( 'NONE',  ( 0.2230871135786579862, 1456.931719161489809, 219.7455025295530220 ) ) ;
#1411 = CARTESIAN_POINT ( 'NONE',  ( 11.05913215650000048, 1426.494667556230070, 94.99634540869780608 ) ) ;
#1413 = DIRECTION ( 'NONE',  ( 0.1159387279768451934, 0.9932563673871469545, 0.000000000000000000 ) ) ;
#1414 = CARTESIAN_POINT ( 'NONE',  ( -11.71296687490000110, 1433.008354761999954, 150.8502298933980228 ) ) ;
#1415 = ADVANCED_FACE ( 'NONE', ( #58346 ), #55745, .F. ) ;
#1416 = VECTOR ( 'NONE', #69193, 1000.000000000000000 ) ;
#1417 = CARTESIAN_POINT ( 'NONE',  ( -2.708795395750633439, 1420.182185210162970, 186.0140258646650864 ) ) ;
#1418 = CARTESIAN_POINT ( 'NONE',  ( 7.494293556130000589, 1424.653638210349982, 212.2908972313289837 ) ) ;
#1419 = CARTESIAN_POINT ( 'NONE',  ( 11.27339694790000024, 1433.557990534789951, 225.8166789514989716 ) ) ;
#1420 = CARTESIAN_POINT ( 'NONE',  ( 8.353214826769999490, 1509.201657029630042, 181.3236374839979987 ) ) ;
#1421 = CARTESIAN_POINT ( 'NONE',  ( -109.5441724370000003, 1379.437061298989875, 305.1680627026370303 ) ) ;
#1422 = CARTESIAN_POINT ( 'NONE',  ( 8.829530141155370160, 1365.516248932926601, 207.6218459616988241 ) ) ;
#1424 = ORIENTED_EDGE ( 'NONE', *, *, #96163, .T. ) ;
#1423 = CARTESIAN_POINT ( 'NONE',  ( 6.708537208820000153, 1454.558820378589871, 216.3279882152490075 ) ) ;
#1425 = ORIENTED_EDGE ( 'NONE', *, *, #92483, .T. ) ;
#1426 = CARTESIAN_POINT ( 'NONE',  ( -41.48601633919999188, 1444.048446191809944, 136.5661428469979910 ) ) ;
#1427 = CARTESIAN_POINT ( 'NONE',  ( 7.522201442634911750, 1510.631883379783403, 203.2096215414982510 ) ) ;
#1428 = CARTESIAN_POINT ( 'NONE',  ( -2.230923574740000248, 1471.396667871830005, 269.3352507041980175 ) ) ;
#1429 = CARTESIAN_POINT ( 'NONE',  ( -110.7672523143288856, 1378.813060387289852, 305.6601225730716465 ) ) ;
#1430 = CARTESIAN_POINT ( 'NONE',  ( -0.5791816274180000557, 1486.229018827529899, 181.7900702770979819 ) ) ;
#1431 = CARTESIAN_POINT ( 'NONE',  ( -32.09351624765574940, 1524.374142163904025, 201.5415833658115901 ) ) ;
#1432 = CARTESIAN_POINT ( 'NONE',  ( 1.506981856204509862, 1476.106228118699846, 197.7392248870460207 ) ) ;
#1433 = CARTESIAN_POINT ( 'NONE',  ( 16.66231036550724198, 1523.604703353109699, 237.7554842931445478 ) ) ;
#1434 = CARTESIAN_POINT ( 'NONE',  ( -2.500000000000000000, 1448.206111001999943, 170.1385578322760068 ) ) ;
#1435 = CARTESIAN_POINT ( 'NONE',  ( 8.305289958184035370, 1368.611760151032058, 207.6218459616987673 ) ) ;
#1436 = CARTESIAN_POINT ( 'NONE',  ( 13.11441086409999990, 1409.193432151429988, 216.3239404139079909 ) ) ;
#1437 = CARTESIAN_POINT ( 'NONE',  ( -0.7694941353355659874, 1406.265043692640120, 269.2947833301390119 ) ) ;
#1438 = DIRECTION ( 'NONE',  ( -0.9942586961433761417, -1.225281874271768203E-16, -0.1070030146457283393 ) ) ;
#1439 = VERTEX_POINT ( 'NONE', #8465 ) ;
#1440 = CARTESIAN_POINT ( 'NONE',  ( -11.86550948169999842, 1432.301447584650077, 150.3971867772980033 ) ) ;
#1441 = CARTESIAN_POINT ( 'NONE',  ( 13.54476740079999963, 1443.929709051740019, 188.0927821155979984 ) ) ;
#1442 = ORIENTED_EDGE ( 'NONE', *, *, #72907, .T. ) ;
#1443 = VECTOR ( 'NONE', #3619, 1000.000000000000000 ) ;
#1444 = EDGE_LOOP ( 'NONE', ( #20128, #45401, #22569, #42921 ) ) ;
#1445 = CARTESIAN_POINT ( 'NONE',  ( -4.060232945970000173, 1454.025412599190076, 199.8833095181790043 ) ) ;
#1446 = CARTESIAN_POINT ( 'NONE',  ( -4.533972342531168209, 1368.949167379208347, 207.6218459616989946 ) ) ;
#1447 = VECTOR ( 'NONE', #59102, 1000.000000000000000 ) ;
#1448 = CARTESIAN_POINT ( 'NONE',  ( 0.7564342142240020328, 1516.783665406140017, 213.7345173100169973 ) ) ;
#1449 = CARTESIAN_POINT ( 'NONE',  ( 3.276907026574999993, 1511.440441732939917, 216.8388625892569905 ) ) ;
#1450 = B_SPLINE_SURFACE_WITH_KNOTS ( 'NONE', 5, 5, ( 
 ( #90304, #23657, #57839, #21975, #56167, #91966 ),
 ( #81906, #38256, #5775, #72439, #106571, #29857 ),
 ( #39364, #98160, #89765, #73538, #75188, #85766 ),
 ( #58381, #66797, #17432, #24733, #33156, #58930 ),
 ( #75733, #25842, #67896, #686, #7958, #109877 ),
 ( #110422, #67345, #101443, #93061, #16335, #17998 ) ),
 .UNSPECIFIED., .F., .F., .F.,
 ( 6, 6 ),
 ( 6, 6 ),
 ( 0.9322655043309999723, 1.047387711740000116 ),
 ( 0.000000000000000000, 2.000000000000000000 ),
 .UNSPECIFIED. ) ;
#1451 = AXIS2_PLACEMENT_3D ( 'NONE', #97655, #36648, #80859 ) ;
#1452 = ORIENTED_EDGE ( 'NONE', *, *, #34105, .T. ) ;
#1453 = ADVANCED_FACE ( 'NONE', ( #67858 ), #93650, .F. ) ;
#1454 = CARTESIAN_POINT ( 'NONE',  ( -87.43041093610000303, 1379.577971548199912, 299.9734862988590294 ) ) ;
#1455 = CIRCLE ( 'NONE', #51483, 1.999999999999997780 ) ;
#1456 = ADVANCED_FACE ( 'NONE', ( #108738 ), #94755, .F. ) ;
#1457 = EDGE_CURVE ( 'NONE', #35149, #76715, #34783, .T. ) ;
#1458 = ADVANCED_FACE ( 'NONE', ( #94687 ), #103644, .T. ) ;
#1459 = B_SPLINE_CURVE_WITH_KNOTS ( 'NONE', 3,
 ( #105967, #71293, #62904, #97014, #89149, #20276, #46071, #54480, #3520, #65482, #71851, #12434, #99591, #48118, #102360, #101798, #25088, #66038, #110215, #7213, #32414, #17223, #93958, #91754, #15029, #75536, #83353, #110770, #51419, #49776, #100698, #49228, #76074, #76618, #7753, #85550, #50872, #66594, #6652, #85002, #109671, #59835, #109132 ),
 .UNSPECIFIED., .F., .F.,
 ( 4, 3, 3, 3, 3, 3, 3, 3, 3, 3, 3, 3, 3, 3, 4 ),
 ( -2.000000000000000000, -1.936215008427339956, -1.791913135960270020, -1.645609380878030104, -1.498043589331059966, -1.348593918407889891, -1.198178442218299944, -1.047113558058780036, -0.8957606298038101045, -0.7380121483472110722, -0.5877609036753239646, -0.4386042209462979180, -0.2908102820543170264, -0.1445690464712710011, 0.000000000000000000 ),
 .UNSPECIFIED. ) ;
#1460 = CARTESIAN_POINT ( 'NONE',  ( 7.292853372139999735, 1414.971279908829956, 224.4496626855979855 ) ) ;
#1461 = CARTESIAN_POINT ( 'NONE',  ( 2.288357407604999949, 1517.116049120239950, 203.3334095979369920 ) ) ;
#1462 = B_SPLINE_CURVE_WITH_KNOTS ( 'NONE', 5,
 ( #85322, #26530, #8071, #43357, #77504, #102127 ),
 .UNSPECIFIED., .F., .F.,
 ( 6, 6 ),
 ( -1.020724565110000093, 5.536280491323250175 ),
 .UNSPECIFIED. ) ;
#1463 = CARTESIAN_POINT ( 'NONE',  ( -29.17336326509999722, 1509.870405653630087, 207.9069865368680041 ) ) ;
#1464 = EDGE_CURVE ( 'NONE', #13274, #40624, #28589, .T. ) ;
#1465 = CARTESIAN_POINT ( 'NONE',  ( -0.5920813016230001002, 1487.765345405229937, 230.8947267201980083 ) ) ;
#1467 = EDGE_CURVE ( 'NONE', #89438, #10483, #27113, .T. ) ;
#1466 = CARTESIAN_POINT ( 'NONE',  ( -58.30221543510000259, 1384.791840522580060, 240.0691493971590091 ) ) ;
#1468 = CARTESIAN_POINT ( 'NONE',  ( -65.89286211545359606, 1384.710728713680055, 257.0461978634630213 ) ) ;
#1469 =( BOUNDED_SURFACE ( )  B_SPLINE_SURFACE ( 3, 2, ( 
 ( #99789, #74073, #14692 ),
 ( #48881, #91415, #47213 ),
 ( #106559, #13573, #56157 ),
 ( #90292, #81893, #72427 ),
 ( #29846, #5196, #81339 ),
 ( #83007, #65671, #39351 ),
 ( #82464, #99234, #4120 ),
 ( #32049, #90848, #56713 ),
 ( #73527, #31491, #6299 ),
 ( #40446, #107661, #4653 ),
 ( #30947, #65122, #22511 ),
 ( #66238, #89206, #46682 ) ),
 .UNSPECIFIED., .F., .F., .T. ) 
 B_SPLINE_SURFACE_WITH_KNOTS ( ( 4, 2, 2, 2, 2, 4 ),
 ( 3, 3 ),
 ( 0.000000000000000000, 0.001069581499716159949, 0.001604372249574239923, 0.002139162999432319898, 0.003208744499148479846, 0.004278325998864639795 ),
 ( 0.000000000000000000, 1.000000000000000000 ),
 .UNSPECIFIED. ) 
 GEOMETRIC_REPRESENTATION_ITEM ( )  RATIONAL_B_SPLINE_SURFACE ( (
 ( 1.000000000000000000, 0.7071067811863054331, 1.000000000000000000),
 ( 1.000000000000000000, 0.7227602064011806604, 1.000000000000000000),
 ( 1.000000000000000000, 0.7381100937480321589, 1.000000000000000000),
 ( 1.000000000000000000, 0.7607230651862928461, 1.000000000000000000),
 ( 1.000000000000000000, 0.7681914495759601946, 1.000000000000000000),
 ( 1.000000000000000000, 0.7829826642569391870, 1.000000000000000000),
 ( 1.000000000000000000, 0.7903039095410622217, 1.000000000000000000),
 ( 1.000000000000000000, 0.8113823828798899518, 1.000000000000000000),
 ( 1.000000000000000000, 0.8244993778341390689, 1.000000000000000000),
 ( 1.000000000000000000, 0.8485230146284407082, 1.000000000000000000),
 ( 1.000000000000000000, 0.8591868199085809232, 1.000000000000000000),
 ( 1.000000000000000000, 0.8676549144810682401, 1.000000000000000000) ) ) 
 REPRESENTATION_ITEM ( '' )  SURFACE ( )  );
#1470 = CARTESIAN_POINT ( 'NONE',  ( -6.244762126029999472, 1407.784308383030066, 197.6511686028979966 ) ) ;
#1471 = CARTESIAN_POINT ( 'NONE',  ( -103.5990824459999970, 1389.912137903419989, 305.4537645068589882 ) ) ;
#1473 = ORIENTED_EDGE ( 'NONE', *, *, #96056, .F. ) ;
#1472 = CARTESIAN_POINT ( 'NONE',  ( -10.63892929799999898, 1445.506293354350191, 185.8359387749980272 ) ) ;
#1474 = DIRECTION ( 'NONE',  ( -0.6736849260863841948, 0.000000000000000000, 0.7390186874254148774 ) ) ;
#1475 = CARTESIAN_POINT ( 'NONE',  ( -25.85373363512699996, 1440.913060485959932, 221.0820133274520174 ) ) ;
#1476 = CARTESIAN_POINT ( 'NONE',  ( 19.65515833015399849, 1477.262508678489894, 226.0632499707639909 ) ) ;
#1477 = CARTESIAN_POINT ( 'NONE',  ( -24.35667143039999516, 1435.422350721090197, 137.0292528702979951 ) ) ;
#1478 = AXIS2_PLACEMENT_3D ( 'NONE', #2381, #34836, #69582 ) ;
#1479 = CARTESIAN_POINT ( 'NONE',  ( -3.446329813785000251, 1516.812046502680005, 212.0014881234369852 ) ) ;
#1480 = CARTESIAN_POINT ( 'NONE',  ( -68.67274465469999711, 1379.748163774529985, 279.9618448723590518 ) ) ;
#1481 = CARTESIAN_POINT ( 'NONE',  ( 17.17241001986483795, 1512.187213306747481, 179.6185504016043240 ) ) ;
#1482 = CARTESIAN_POINT ( 'NONE',  ( -115.5939564047259296, 1379.013060387289897, 305.4204098037694735 ) ) ;
#1483 = CARTESIAN_POINT ( 'NONE',  ( -18.92739890465090014, 1503.345986874440086, 222.1981604764409894 ) ) ;
#1484 = CARTESIAN_POINT ( 'NONE',  ( 3.255809864005000165, 1516.837969789639828, 208.3644199470059846 ) ) ;
#1485 = EDGE_LOOP ( 'NONE', ( #33168, #31647, #63478, #110389 ) ) ;
#1486 = CARTESIAN_POINT ( 'NONE',  ( 4.363122647530000009, 1417.926080483629903, 166.9581667359979917 ) ) ;
#1488 = EDGE_CURVE ( 'NONE', #32360, #66058, #13266, .T. ) ;
#1487 = CARTESIAN_POINT ( 'NONE',  ( 2.470168521978401088, 1523.481610426287716, 242.8787258963054683 ) ) ;
#1489 = CARTESIAN_POINT ( 'NONE',  ( -38.49223698079999423, 1385.058880994630044, 239.3118539506589855 ) ) ;
#1490 = VERTEX_POINT ( 'NONE', #17960 ) ;
#1491 = CARTESIAN_POINT ( 'NONE',  ( -105.7942887633819993, 1378.913060387289988, 304.0474587704230203 ) ) ;
#1492 = CARTESIAN_POINT ( 'NONE',  ( -3.359680129360000045, 1429.147736159890201, 201.1390560926290050 ) ) ;
#1493 = CARTESIAN_POINT ( 'NONE',  ( 12.12127920967330041, 1433.956690957220189, 149.8582645731989942 ) ) ;
#1494 = B_SPLINE_CURVE_WITH_KNOTS ( 'NONE', 5,
 ( #71750, #95254, #20722, #61140, #62230, #54918 ),
 .UNSPECIFIED., .F., .F.,
 ( 6, 6 ),
 ( 0.000000000000000000, 1.000000000000000000 ),
 .UNSPECIFIED. ) ;
#1495 = CARTESIAN_POINT ( 'NONE',  ( 16.68871050416229807, 1478.708306862099789, 229.8628164125950093 ) ) ;
#1496 = ADVANCED_FACE ( 'NONE', ( #9028 ), #7081, .T. ) ;
#1497 = CARTESIAN_POINT ( 'NONE',  ( -24.69773639504949969, 1509.761573056400039, 223.9593781233639902 ) ) ;
#1498 = CARTESIAN_POINT ( 'NONE',  ( 3.830726099870000123, 1487.263094006890014, 197.7783884857990131 ) ) ;
#1499 = ADVANCED_FACE ( 'NONE', ( #70628 ), #95038, .T. ) ;
#1500 = CARTESIAN_POINT ( 'NONE',  ( -0.04532349001890000062, 1409.423585831229957, 233.0275901203980027 ) ) ;
#1501 = VECTOR ( 'NONE', #9818, 1000.000000000000114 ) ;
#1503 = CARTESIAN_POINT ( 'NONE',  ( -3.770547026519999623, 1420.469916612930092, 186.2929298669980085 ) ) ;
#1502 = CARTESIAN_POINT ( 'NONE',  ( 3.262264650305000124, 1516.633288330999903, 215.6694029015669969 ) ) ;
#1504 = CARTESIAN_POINT ( 'NONE',  ( 18.70459387589999878, 1509.566239198529956, 186.5372755683980017 ) ) ;
#1505 = DIRECTION ( 'NONE',  ( -0.9455185755993178454, 0.000000000000000000, 0.3255681544571539243 ) ) ;
#1506 = EDGE_LOOP ( 'NONE', ( #67420, #97199, #19165, #75833 ) ) ;
#1507 = CARTESIAN_POINT ( 'NONE',  ( -12.73136601901759946, 1416.225364278609959, 196.2684121632169933 ) ) ;
#1508 = B_SPLINE_CURVE_WITH_KNOTS ( 'NONE', 3,
 ( #110150, #9352, #101176, #24470, #42390, #60313 ),
 .UNSPECIFIED., .F., .F.,
 ( 4, 2, 4 ),
 ( 0.000000000000000000, 0.5000000000000000000, 1.000000000000000000 ),
 .UNSPECIFIED. ) ;
#1509 = CARTESIAN_POINT ( 'NONE',  ( -20.49035733430000050, 1504.313428628929842, 189.6781957060979948 ) ) ;
#1510 = VERTEX_POINT ( 'NONE', #35900 ) ;
#1511 = EDGE_CURVE ( 'NONE', #61012, #77321, #48001, .T. ) ;
#1512 = CARTESIAN_POINT ( 'NONE',  ( 2.677300865789999929, 1420.709102647230111, 184.9509449586979883 ) ) ;
#1513 =( NAMED_UNIT ( * ) SI_UNIT ( $, .STERADIAN. ) SOLID_ANGLE_UNIT ( ) );
#1514 = CARTESIAN_POINT ( 'NONE',  ( 7.518184181947409783, 1510.874996213040049, 203.1087175251330166 ) ) ;
#1515 = CARTESIAN_POINT ( 'NONE',  ( 2.613887865783830033, 1424.090078648330064, 191.3525227764439762 ) ) ;
#1516 = CARTESIAN_POINT ( 'NONE',  ( -30.24841015875323791, 1524.082740465118832, 195.7700776127339566 ) ) ;
#1517 = CARTESIAN_POINT ( 'NONE',  ( -16.31009655498456823, 1409.653544930775070, 192.3727841784286738 ) ) ;
#1518 = CARTESIAN_POINT ( 'NONE',  ( 17.56720881609999907, 1415.048591087029763, 210.3588846212080057 ) ) ;
#1519 = CARTESIAN_POINT ( 'NONE',  ( -17.96296818009999896, 1424.130910211129958, 225.8903661153979954 ) ) ;
#1520 = FACE_OUTER_BOUND ( 'NONE', #99932, .T. ) ;
#1521 = CARTESIAN_POINT ( 'NONE',  ( -4.978523888090000682, 1441.600846913620217, 150.3430135618980046 ) ) ;
#1522 = CARTESIAN_POINT ( 'NONE',  ( -1.073559340110749938, 1444.993510080170154, 218.0402162255370229 ) ) ;
#1524 = DIRECTION ( 'NONE',  ( 0.9455185755993178454, 0.000000000000000000, -0.3255681544571537578 ) ) ;
#1523 = CARTESIAN_POINT ( 'NONE',  ( 10.57339846829999885, 1490.054618766489966, 202.8450963736189863 ) ) ;
#1525 = CARTESIAN_POINT ( 'NONE',  ( 2.397475438392864255, 1525.713797967456685, 243.2249543484664400 ) ) ;
#1526 = ORIENTED_EDGE ( 'NONE', *, *, #72632, .T. ) ;
#1527 = CARTESIAN_POINT ( 'NONE',  ( 1.556457968405000170, 1415.007830321620077, 191.6742979189480138 ) ) ;
#1528 = CARTESIAN_POINT ( 'NONE',  ( -4.833436873729840322, 1508.551704408090018, 212.3464058856069983 ) ) ;
#1529 = CARTESIAN_POINT ( 'NONE',  ( -23.88515968680000157, 1436.380149434200121, 211.3762814741380112 ) ) ;
#1530 = CARTESIAN_POINT ( 'NONE',  ( 8.915053209252663535, 1410.596227120273625, 188.0708813341610437 ) ) ;
#1531 = CIRCLE ( 'NONE', #87365, 1.000000000000000888 ) ;
#1532 = CARTESIAN_POINT ( 'NONE',  ( 5.161277877375379575, 1424.205378946189967, 193.2953230041809718 ) ) ;
#1533 = CARTESIAN_POINT ( 'NONE',  ( -11.90000415720300175, 1434.913060496859998, 147.6452464505769910 ) ) ;
#1534 = DIRECTION ( 'NONE',  ( 0.9858563016923833633, 0.000000000000000000, 0.1675928173085483863 ) ) ;
#1535 = CIRCLE ( 'NONE', #87369, 12.26364123839999998 ) ;
#1536 = CARTESIAN_POINT ( 'NONE',  ( -2.731551787915110108, 1488.063880473559948, 219.6750998402769994 ) ) ;
#1537 = CARTESIAN_POINT ( 'NONE',  ( 20.10527798697370017, 1430.877974082169885, 215.1856728963680041 ) ) ;
#1538 = CARTESIAN_POINT ( 'NONE',  ( -75.52559667918460207, 1383.780383530929839, 300.2699059305949731 ) ) ;
#1539 = CIRCLE ( 'NONE', #69491, 2.000000000000001776 ) ;
#1540 = CARTESIAN_POINT ( 'NONE',  ( 21.54229287260000092, 1452.160786943630228, 141.5333698742980175 ) ) ;
#1541 = ADVANCED_FACE ( 'NONE', ( #10697 ), #23125, .F. ) ;
#1542 = CARTESIAN_POINT ( 'NONE',  ( -5.034946147495399593, 1391.797004273162884, 214.6764752712134339 ) ) ;
#1543 = CARTESIAN_POINT ( 'NONE',  ( 14.20882688731320975, 1410.783320216355833, 191.3835041209767951 ) ) ;
#1545 = VERTEX_POINT ( 'NONE', #63867 ) ;
#1544 = CARTESIAN_POINT ( 'NONE',  ( 10.34950188612880062, 1451.639534178259964, 207.2650128704659949 ) ) ;
#1546 = CARTESIAN_POINT ( 'NONE',  ( -18.07191983094158161, 1459.591554196664219, 227.9854841469545192 ) ) ;
#1547 = CARTESIAN_POINT ( 'NONE',  ( -87.19453865519999169, 1382.337400661289848, 307.1204035211590053 ) ) ;
#1548 = DIRECTION ( 'NONE',  ( 0.9455185755993178454, 0.000000000000000000, -0.3255681544571537578 ) ) ;
#1549 = ORIENTED_EDGE ( 'NONE', *, *, #45523, .F. ) ;
#1550 = VERTEX_POINT ( 'NONE', #21250 ) ;
#1551 = FACE_OUTER_BOUND ( 'NONE', #21340, .T. ) ;
#1552 = DIRECTION ( 'NONE',  ( -1.755985294532469921E-16, 1.000000000000000000, -1.338183447452831989E-16 ) ) ;
#1553 = CARTESIAN_POINT ( 'NONE',  ( 39.14220602846550179, 1439.921242502060068, 136.7207080452419916 ) ) ;
#1555 = CARTESIAN_POINT ( 'NONE',  ( -40.57811314119999935, 1448.614249393429873, 261.6156832257979659 ) ) ;
#1554 = CARTESIAN_POINT ( 'NONE',  ( 18.05542495219999921, 1416.825784017130218, 208.7596466302459817 ) ) ;
#1556 = CARTESIAN_POINT ( 'NONE',  ( 8.983348777261449314, 1436.547473071500008, 210.1510915947499996 ) ) ;
#1557 = CARTESIAN_POINT ( 'NONE',  ( -109.2768968829999920, 1384.496076674440019, 297.1408104247589677 ) ) ;
#1558 = ADVANCED_FACE ( 'NONE', ( #55461 ), #67926, .T. ) ;
#1559 = CARTESIAN_POINT ( 'NONE',  ( -0.3197736172905292218, 1452.655606759615466, 183.2748911063349055 ) ) ;
#1560 = CARTESIAN_POINT ( 'NONE',  ( -19.88544360889999751, 1484.719772526229917, 191.4492701382980044 ) ) ;
#1561 = TOROIDAL_SURFACE ( 'NONE', #51590, 2.030931026690000252, 0.5000000000000000000 ) ;
#1562 = CARTESIAN_POINT ( 'NONE',  ( 1.734313731699999916, 1409.141427551030120, 185.9428025286979960 ) ) ;
#1563 = CARTESIAN_POINT ( 'NONE',  ( 5.808871921319999743, 1423.519516101330055, 186.0672565399979987 ) ) ;
#1564 = CARTESIAN_POINT ( 'NONE',  ( -7.733451861169999830, 1440.968359749710089, 154.0956080340980066 ) ) ;
#1565 = CARTESIAN_POINT ( 'NONE',  ( -9.179291680683139276, 1449.804744045379948, 209.6468028662770280 ) ) ;
#1566 = CARTESIAN_POINT ( 'NONE',  ( -10.52065382388829917, 1423.715440622650021, 204.4033256026779952 ) ) ;
#1567 = DIRECTION ( 'NONE',  ( 0.000000000000000000, 0.000000000000000000, -1.000000000000000000 ) ) ;
#1568 = CARTESIAN_POINT ( 'NONE',  ( 8.840620885073873225, 1512.187213306747481, 223.8289249455313268 ) ) ;
#1569 = EDGE_LOOP ( 'NONE', ( #50451, #68937, #11902, #3529 ) ) ;
#1570 = CARTESIAN_POINT ( 'NONE',  ( -2.398688105316478580, 1426.758990796949320, 141.3562649765487436 ) ) ;
#1571 = CARTESIAN_POINT ( 'NONE',  ( 5.076297622210270255, 1469.790078878110080, 187.8425686012589892 ) ) ;
#1572 = CARTESIAN_POINT ( 'NONE',  ( -39.29615804430000026, 1457.459686057429963, 269.7910478776980199 ) ) ;
#1573 = FACE_OUTER_BOUND ( 'NONE', #66351, .T. ) ;
#1574 = CARTESIAN_POINT ( 'NONE',  ( 6.510459374210000760, 1435.947057077009958, 154.7340827710979738 ) ) ;
#1575 = DIRECTION ( 'NONE',  ( 0.000000000000000000, 0.000000000000000000, 1.000000000000000000 ) ) ;
#1576 = EDGE_CURVE ( 'NONE', #57810, #42994, #14529, .T. ) ;
#1577 = CARTESIAN_POINT ( 'NONE',  ( -11.81780673814840021, 1517.051704408389924, 222.7166774759110126 ) ) ;
#1578 = CARTESIAN_POINT ( 'NONE',  ( 2.924524102719100238, 1410.358758242020031, 231.6291648917529926 ) ) ;
#1579 = CARTESIAN_POINT ( 'NONE',  ( -1.455250893790000166, 1415.140114704729967, 226.9749634510980059 ) ) ;
#1580 = CARTESIAN_POINT ( 'NONE',  ( -3.026978396589999676, 1416.096969111230010, 232.7842076799979907 ) ) ;
#1581 = CARTESIAN_POINT ( 'NONE',  ( -1.068647241811354398, 1484.851163306396302, 182.1517477618084229 ) ) ;
#1582 = CARTESIAN_POINT ( 'NONE',  ( 3.726002059892866480, 1358.803007711198916, 208.3718459617010978 ) ) ;
#1583 = CARTESIAN_POINT ( 'NONE',  ( -45.58450343905819580, 1439.256682012769943, 268.9762893008089577 ) ) ;
#1584 = DIRECTION ( 'NONE',  ( 0.000000000000000000, 0.000000000000000000, -1.000000000000000000 ) ) ;
#1585 = VERTEX_POINT ( 'NONE', #48716 ) ;
#1586 = CARTESIAN_POINT ( 'NONE',  ( -9.227567128520000495, 1423.503386125029920, 208.4707392769450109 ) ) ;
#1587 = ORIENTED_EDGE ( 'NONE', *, *, #48761, .T. ) ;
#1588 = CARTESIAN_POINT ( 'NONE',  ( -7.713648872314999849, 1516.710624944440042, 209.8745175203999906 ) ) ;
#1589 = CARTESIAN_POINT ( 'NONE',  ( -9.088549428918609507, 1447.355647609609832, 212.1269012052750043 ) ) ;
#1590 = CARTESIAN_POINT ( 'NONE',  ( 19.26602811997136655, 1456.117940503140971, 225.0698710879842110 ) ) ;
#1591 = CARTESIAN_POINT ( 'NONE',  ( -11.38922736439999994, 1425.413087568229912, 188.2682818651980199 ) ) ;
#1592 = CARTESIAN_POINT ( 'NONE',  ( 0.6958875083883689916, 1496.027399175239907, 221.4434803195429993 ) ) ;
#1593 = B_SPLINE_SURFACE_WITH_KNOTS ( 'NONE', 5, 5, ( 
 ( #91827, #49848, #15105, #82335, #66115, #75608, #109738, #107530, #49296, #22953, #91283, #100764 ),
 ( #83424, #64458, #90166, #39785, #73944, #108075, #39218, #48197, #6170, #99114, #31370, #6720 ),
 ( #73394, #30819, #64996, #108635, #40876, #65553, #57159, #14564, #48754, #82877, #75054, #27983 ),
 ( #41990, #85622, #93470, #16202, #102427, #34681, #50406, #86189, #61026, #76140, #9481, #110284 ),
 ( #77798, #68319, #85073, #8365, #24598, #556, #42533, #76686, #78349, #101304, #25158, #77257 ),
 ( #18409, #84532, #44205, #95149, #59910, #34131, #102972, #67754, #25709, #103536, #52607, #68869 ),
 ( #94031, #26270, #86743, #8921, #60460, #35235, #94578, #43645, #17295, #51491, #59362, #1107 ),
 ( #17854, #43096, #7820, #10035, #52054, #69423, #26839, #33019, #16741, #67206, #58791, #92930 ),
 ( #50948, #33560, #101865, #62125, #54817, #88942, #80000, #55365, #29052, #1658, #20614, #71648 ),
 ( #36337, #44766, #11694, #3324, #104095, #72182, #63238, #37449, #106301, #87870, #27944, #70530 ),
 ( #20083, #89498, #97344, #71083, #105208, #104647, #29584, #45867, #53732, #105767, #12234, #2223 ),
 ( #27386, #46424, #36889, #11160, #45321, #61565, #80556, #79459, #2769, #46969, #69979, #96252 ) ),
 .UNSPECIFIED., .F., .F., .F.,
 ( 6, 3, 3, 6 ),
 ( 6, 3, 3, 6 ),
 ( 8.878046405300000998, 9.092838726940000171, 9.522423370220000294, 9.923260654589999064 ),
 ( 0.000000000000000000, 0.6020156018279999577, 1.679451024060000019, 2.218168735169999906 ),
 .UNSPECIFIED. ) ;
#1594 = ORIENTED_EDGE ( 'NONE', *, *, #76038, .T. ) ;
#1595 = CYLINDRICAL_SURFACE ( 'NONE', #11642, 2.000000000000003553 ) ;
#1597 = CARTESIAN_POINT ( 'NONE',  ( 14.17386987649999952, 1470.816980702629962, 194.4171917781980028 ) ) ;
#1596 = DIRECTION ( 'NONE',  ( -0.6736849260863841948, 0.000000000000000000, 0.7390186874254148774 ) ) ;
#1598 = EDGE_CURVE ( 'NONE', #58469, #46920, #64728, .T. ) ;
#1599 = CARTESIAN_POINT ( 'NONE',  ( 1.802870145850000050, 1411.461756991529910, 232.2427255196980127 ) ) ;
#1600 = CARTESIAN_POINT ( 'NONE',  ( -11.50670236126252810, 1425.933829454640545, 139.0400858972396918 ) ) ;
#1601 = EDGE_CURVE ( 'NONE', #93351, #108323, #72640, .T. ) ;
#1602 = CARTESIAN_POINT ( 'NONE',  ( -1.974748282550000011, 1461.153703759689961, 228.6317503212989948 ) ) ;
#1603 = CARTESIAN_POINT ( 'NONE',  ( -8.888452916799840509, 1439.739375908359989, 206.8159864752560111 ) ) ;
#1604 = ORIENTED_EDGE ( 'NONE', *, *, #54213, .T. ) ;
#1605 = CARTESIAN_POINT ( 'NONE',  ( -6.833925870029700533, 1408.295428044619939, 270.2841559995019907 ) ) ;
#1606 = CARTESIAN_POINT ( 'NONE',  ( -5.013429394184999666, 1517.123342927159911, 207.9998951881570122 ) ) ;
#1607 = CARTESIAN_POINT ( 'NONE',  ( 4.139239280457269743, 1417.946269731450002, 233.0858131667390012 ) ) ;
#1608 = CARTESIAN_POINT ( 'NONE',  ( 2.157536728407479565, 1378.013060387289897, 207.9431782750405659 ) ) ;
#1610 = ORIENTED_EDGE ( 'NONE', *, *, #15204, .F. ) ;
#1609 = CARTESIAN_POINT ( 'NONE',  ( -7.811405798920000088, 1367.739269854440181, 207.6218459616989946 ) ) ;
#1611 = ORIENTED_EDGE ( 'NONE', *, *, #77581, .F. ) ;
#1612 = DIRECTION ( 'NONE',  ( -1.000000000000000000, 0.000000000000000000, 0.000000000000000000 ) ) ;
#1613 = EDGE_CURVE ( 'NONE', #46627, #39656, #1849, .T. ) ;
#1614 = CARTESIAN_POINT ( 'NONE',  ( -4.287767397939999725, 1424.648436861230039, 185.9532686480980033 ) ) ;
#1615 = CARTESIAN_POINT ( 'NONE',  ( 3.709069522732904911, 1425.316856860248663, 185.1233798031099980 ) ) ;
#1616 = CARTESIAN_POINT ( 'NONE',  ( -0.01642798734072890149, 1408.968555449449923, 186.0689978232310011 ) ) ;
#1617 = VECTOR ( 'NONE', #90374, 1000.000000000000114 ) ;
#1618 = CIRCLE ( 'NONE', #23085, 2.000000000000001776 ) ;
#1619 = EDGE_CURVE ( 'NONE', #42338, #31705, #37819, .T. ) ;
#1620 = CARTESIAN_POINT ( 'NONE',  ( -20.52576279630359579, 1436.445955288497771, 144.8643394113350666 ) ) ;
#1621 = CARTESIAN_POINT ( 'NONE',  ( -18.04944458410000152, 1425.819836014529983, 225.8836100296980192 ) ) ;
#1622 = CARTESIAN_POINT ( 'NONE',  ( 29.82179391674280211, 1467.143751206999923, 269.1831960069300180 ) ) ;
#1623 = CARTESIAN_POINT ( 'NONE',  ( -14.43048377810894500, 1462.029581583880372, 229.5409151307926265 ) ) ;
#1624 = CARTESIAN_POINT ( 'NONE',  ( 8.735250064049999708, 1446.655199166789998, 185.9308358984979748 ) ) ;
#1625 = CARTESIAN_POINT ( 'NONE',  ( -6.949574985774999547, 1517.102359858469754, 205.8627441332170065 ) ) ;
#1626 = ORIENTED_EDGE ( 'NONE', *, *, #36492, .T. ) ;
#1627 = FACE_OUTER_BOUND ( 'NONE', #78029, .T. ) ;
#1628 = CARTESIAN_POINT ( 'NONE',  ( -5.018135829431690453, 1516.818301249122669, 203.5289603568284065 ) ) ;
#1629 = CARTESIAN_POINT ( 'NONE',  ( 22.66310764289999824, 1409.704358029729974, 208.7414267666439969 ) ) ;
#1630 = ORIENTED_EDGE ( 'NONE', *, *, #44015, .F. ) ;
#1631 = CARTESIAN_POINT ( 'NONE',  ( -1.369904464291739954, 1457.995076032020052, 229.8762231575159944 ) ) ;
#1632 = CARTESIAN_POINT ( 'NONE',  ( 24.51785944913020288, 1452.041301548709953, 136.2948944376120153 ) ) ;
#1633 = DIRECTION ( 'NONE',  ( -0.6736849260863841948, 0.000000000000000000, 0.7390186874254148774 ) ) ;
#1634 = CARTESIAN_POINT ( 'NONE',  ( -20.33527840200000014, 1390.981646659919761, 210.8560405308990084 ) ) ;
#1635 = CARTESIAN_POINT ( 'NONE',  ( -14.24353422718318463, 1390.369519709444148, 210.8398536836253356 ) ) ;
#1636 = CARTESIAN_POINT ( 'NONE',  ( 18.27919210119999960, 1410.914348715230062, 193.9485672390979971 ) ) ;
#1637 = CARTESIAN_POINT ( 'NONE',  ( -3.958123615280000784, 1496.263532292789932, 198.4814042619989891 ) ) ;
#1638 = CARTESIAN_POINT ( 'NONE',  ( 3.920879176457659820, 1439.701872010520219, 184.6839060028229937 ) ) ;
#1640 = CARTESIAN_POINT ( 'NONE',  ( -18.81494228913341971, 1424.684930363856893, 224.5303940569564531 ) ) ;
#1639 = CARTESIAN_POINT ( 'NONE',  ( 0.1494614725679999923, 1415.405923509830018, 233.4379070838980113 ) ) ;
#1641 = ADVANCED_FACE ( 'NONE', ( #64847 ), #92910, .F. ) ;
#1642 = DIRECTION ( 'NONE',  ( -1.755985294532469921E-16, 1.000000000000000000, -1.338183447452831989E-16 ) ) ;
#1643 = CARTESIAN_POINT ( 'NONE',  ( 18.22805055419890152, 1459.311389626190021, 227.8763770136359881 ) ) ;
#1644 = VECTOR ( 'NONE', #9431, 999.9999999999998863 ) ;
#1645 = CARTESIAN_POINT ( 'NONE',  ( -8.680550271810000496, 1382.887713811429876, 218.3027530060789729 ) ) ;
#1646 = CARTESIAN_POINT ( 'NONE',  ( 6.946748518954999341, 1516.983995446890049, 214.1250666973070054 ) ) ;
#1647 = EDGE_CURVE ( 'NONE', #19483, #69912, #41409, .T. ) ;
#1648 = CARTESIAN_POINT ( 'NONE',  ( -32.86802468386279941, 1523.382868172864164, 217.2040256693919957 ) ) ;
#1649 = EDGE_LOOP ( 'NONE', ( #99391, #52672, #101833, #73552 ) ) ;
#1650 = DIRECTION ( 'NONE',  ( 1.755985294532469921E-16, -1.000000000000000000, 1.338183447452831989E-16 ) ) ;
#1651 = CARTESIAN_POINT ( 'NONE',  ( 19.37374569213946174, 1526.382868172863937, 234.3668155954418921 ) ) ;
#1652 = CARTESIAN_POINT ( 'NONE',  ( -9.414212789456051667, 1483.762164573529844, 201.8265950495219840 ) ) ;
#1653 = CARTESIAN_POINT ( 'NONE',  ( 6.694559447547406172, 1420.584111001019892, 222.6458102056001565 ) ) ;
#1654 = CARTESIAN_POINT ( 'NONE',  ( -22.69876404240057965, 1501.977400791986611, 236.8953202675781426 ) ) ;
#1655 = CARTESIAN_POINT ( 'NONE',  ( -4.329271545279450351, 1515.071561052280003, 207.5714932352460096 ) ) ;
#1656 = CARTESIAN_POINT ( 'NONE',  ( -19.46212512329999811, 1448.109899945180132, 224.8635561905979898 ) ) ;
#1657 = CARTESIAN_POINT ( 'NONE',  ( -2.646139193785439936, 1458.417740263149881, 184.4338440838500333 ) ) ;
#1658 = CARTESIAN_POINT ( 'NONE',  ( 11.14906425410000068, 1433.235768261610247, 151.6390481664980143 ) ) ;
#1659 = CARTESIAN_POINT ( 'NONE',  ( 25.52872275119999657, 1450.634754197290022, 248.0989693098979956 ) ) ;
#1660 = CARTESIAN_POINT ( 'NONE',  ( 26.67910011776079671, 1440.913060392740135, 225.3147551850250068 ) ) ;
#1661 = CARTESIAN_POINT ( 'NONE',  ( -17.64133914897380251, 1419.302713979609962, 207.1869683601410088 ) ) ;
#1662 = CARTESIAN_POINT ( 'NONE',  ( -106.3976693117229928, 1390.939243848519936, 307.7527733253859878 ) ) ;
#1663 = CARTESIAN_POINT ( 'NONE',  ( 24.45953054869999832, 1435.631735371460081, 137.6709130696980026 ) ) ;
#1664 = CARTESIAN_POINT ( 'NONE',  ( -9.684780809540001201, 1486.248617649129983, 183.3457608578980000 ) ) ;
#1665 = CARTESIAN_POINT ( 'NONE',  ( -1.191524307911308700, 1526.382868172864164, 239.2353018730791518 ) ) ;
#1666 = CARTESIAN_POINT ( 'NONE',  ( -29.28791600580530030, 1509.974769825920021, 200.6261233647479969 ) ) ;
#1667 = CIRCLE ( 'NONE', #48101, 1.999999999999998668 ) ;
#1668 = CARTESIAN_POINT ( 'NONE',  ( 24.09077679649999837, 1449.794656634499916, 215.4601383587679777 ) ) ;
#1669 = CARTESIAN_POINT ( 'NONE',  ( -15.57808073540140015, 1420.358152465259991, 210.5578313205389804 ) ) ;
#1670 = CARTESIAN_POINT ( 'NONE',  ( 26.34431982013864015, 1436.712149879578192, 136.8400218608261127 ) ) ;
#1671 = CARTESIAN_POINT ( 'NONE',  ( -31.84935467931069297, 1383.839719338520126, 229.8416280207219984 ) ) ;
#1672 = CARTESIAN_POINT ( 'NONE',  ( 19.03958015586209740, 1453.804226984369734, 200.7927591122619901 ) ) ;
#1673 = CARTESIAN_POINT ( 'NONE',  ( 4.041472473744999405, 1516.858649670339901, 213.1514186109370144 ) ) ;
#1675 =( BOUNDED_SURFACE ( )  B_SPLINE_SURFACE ( 1, 2, ( 
 ( #51920, #17718, #978 ),
 ( #35102, #42398, #77665 ) ),
 .UNSPECIFIED., .F., .F., .F. ) 
 B_SPLINE_SURFACE_WITH_KNOTS ( ( 2, 2 ),
 ( 3, 3 ),
 ( -10000.00000000000000, 10000.00000000000000 ),
 ( 5.770213223686299742, 6.084699837289689661 ),
 .UNSPECIFIED. ) 
 GEOMETRIC_REPRESENTATION_ITEM ( )  RATIONAL_B_SPLINE_SURFACE ( (
 ( 0.8711730261270910214, 0.8915130006034900356, 0.9353332883307809986),
 ( 0.8711730261270910214, 0.8915130006034900356, 0.9353332883307809986) ) ) 
 REPRESENTATION_ITEM ( '' )  SURFACE ( )  );
#1674 = CARTESIAN_POINT ( 'NONE',  ( 1970.025574498409924, -8382.262153571269664, 413.0777247525010125 ) ) ;
#1676 = CARTESIAN_POINT ( 'NONE',  ( 0.1633892455278690148, 1484.235898642210259, 181.9124132699890026 ) ) ;
#1678 = VERTEX_POINT ( 'NONE', #59194 ) ;
#1677 = CARTESIAN_POINT ( 'NONE',  ( 30.90487439922560498, 1525.907212628473644, 216.4335774778780035 ) ) ;
#1679 = DIRECTION ( 'NONE',  ( -6.922360974429999144E-17, -1.000000000000000000, 2.302693041820029802E-16 ) ) ;
#1680 = CARTESIAN_POINT ( 'NONE',  ( -1.458447685501650145E-16, 1382.910363916049846, 199.8625637235290071 ) ) ;
#1681 = CARTESIAN_POINT ( 'NONE',  ( -4.845900717560000182, 1475.703791084489922, 200.0054995007290017 ) ) ;
#1683 = ORIENTED_EDGE ( 'NONE', *, *, #98768, .F. ) ;
#1682 = CARTESIAN_POINT ( 'NONE',  ( -35.74845714583440071, 1451.452973098360189, 134.0999999985519935 ) ) ;
#1684 = CARTESIAN_POINT ( 'NONE',  ( -5.312643570539870019, 1508.551704408389924, 219.6039287689250159 ) ) ;
#1685 = EDGE_LOOP ( 'NONE', ( #19186, #71769, #109831, #40295 ) ) ;
#1686 = B_SPLINE_SURFACE_WITH_KNOTS ( 'NONE', 5, 1, ( 
 ( #74996, #40266 ),
 ( #6664, #109145 ),
 ( #76630, #7225 ),
 ( #66606, #84478 ),
 ( #41384, #32960 ),
 ( #33500, #57097 ) ),
 .UNSPECIFIED., .F., .F., .F.,
 ( 6, 6 ),
 ( 2, 2 ),
 ( 0.000000000000000000, 3.644487327430000256 ),
 ( 0.000000000000000000, 14.00000000000000000 ),
 .UNSPECIFIED. ) ;
#1687 = CARTESIAN_POINT ( 'NONE',  ( -14.52654072983339972, 1379.768571760160057, 208.3454318067070119 ) ) ;
#1688 = CARTESIAN_POINT ( 'NONE',  ( 7.124063054187752542, 1447.290098683538417, 203.4859220507082114 ) ) ;
#1689 = CARTESIAN_POINT ( 'NONE',  ( -16.66936639845609491, 1523.382868172864164, 237.7608804993221838 ) ) ;
#1690 = CARTESIAN_POINT ( 'NONE',  ( -2.852161174780241559, 1367.911847845928150, 208.3703648968576942 ) ) ;
#1691 = ADVANCED_FACE ( 'NONE', ( #49136 ), #52131, .T. ) ;
#1692 = CARTESIAN_POINT ( 'NONE',  ( 0.3570378922979989822, 1430.313573167290087, 217.4716923096189873 ) ) ;
#1693 = CARTESIAN_POINT ( 'NONE',  ( -10.47820675957179937, 1471.893954719099838, 206.9970117854870182 ) ) ;
#1694 = CARTESIAN_POINT ( 'NONE',  ( 14.50852758997319825, 1409.419709334970094, 205.5898239192270012 ) ) ;
#1695 = CARTESIAN_POINT ( 'NONE',  ( -12.08187496630000091, 1391.708070121689843, 207.0208056324590018 ) ) ;
#1696 = CARTESIAN_POINT ( 'NONE',  ( -98.94538731745480220, 1385.218168442259866, 296.0687099710040115 ) ) ;
#1697 = CARTESIAN_POINT ( 'NONE',  ( -17.22534334500000242, 1417.728649700130063, 191.7604894772980231 ) ) ;
#1698 = DIRECTION ( 'NONE',  ( 0.000000000000000000, -1.000000000000000000, 0.000000000000000000 ) ) ;
#1699 = ORIENTED_EDGE ( 'NONE', *, *, #62887, .F. ) ;
#1700 = AXIS2_PLACEMENT_3D ( 'NONE', #47499, #79993, #57014 ) ;
#1701 = CARTESIAN_POINT ( 'NONE',  ( 11.15529992359070022, 1491.248582895630079, 209.3143910749519705 ) ) ;
#1703 = ORIENTED_EDGE ( 'NONE', *, *, #71721, .T. ) ;
#1702 = CARTESIAN_POINT ( 'NONE',  ( -1.547462741870939906, 1414.913060391199906, 225.9340804956229931 ) ) ;
#1704 = CARTESIAN_POINT ( 'NONE',  ( 5.409313786005300884, 1467.330720308250193, 217.4825536316049863 ) ) ;
#1705 = CIRCLE ( 'NONE', #83677, 6.988489866870006395 ) ;
#1706 = ORIENTED_EDGE ( 'NONE', *, *, #85099, .F. ) ;
#1707 = CARTESIAN_POINT ( 'NONE',  ( 24.21955345239999957, 1509.534796804930011, 222.9919670691980116 ) ) ;
#1708 = CARTESIAN_POINT ( 'NONE',  ( -7.910792383497443403, 1364.512313338026843, 208.3718459617061285 ) ) ;
#1709 = CARTESIAN_POINT ( 'NONE',  ( -114.7007400580323520, 1391.413060387289988, 302.0868810157617190 ) ) ;
#1710 = EDGE_CURVE ( 'NONE', #5224, #18098, #40044, .T. ) ;
#1711 = CARTESIAN_POINT ( 'NONE',  ( 25.36436853360955368, 1465.298048299637685, 269.4265643490046500 ) ) ;
#1712 = CARTESIAN_POINT ( 'NONE',  ( 11.41287573240554032, 1427.618782186570115, 209.6357587079445182 ) ) ;
#1713 = CARTESIAN_POINT ( 'NONE',  ( 3.851850563460000210, 1397.715876698029888, 221.6434075889979738 ) ) ;
#1714 = B_SPLINE_CURVE_WITH_KNOTS ( 'NONE', 3,
 ( #52850, #103786, #61271, #9715, #95386, #51175, #25391, #60141, #93698, #36040, #52300, #85873, #70228, #9175, #8054, #104333, #78025, #27626, #43340, #16976, #86425, #85305, #43881, #8602, #42775, #34373, #18651, #77488, #102646, #106534, #72403, #3008, #62364, #104888, #97589, #10837, #106001, #29823, #12476, #28179, #80790, #11392, #37681, #13004, #21396, #38221, #64010, #89182, #98121, #19769, #79153, #105444, #2462, #55606, #29277, #54517, #47190, #88652, #19196, #38768, #46658, #81315 ),
 .UNSPECIFIED., .F., .F.,
 ( 4, 2, 1, 1, 1, 1, 1, 2, 2, 2, 1, 1, 1, 1, 1, 2, 2, 2, 2, 1, 1, 1, 1, 1, 2, 2, 2, 2, 2, 1, 1, 1, 1, 1, 2, 2, 2, 2, 2, 2, 4 ),
 ( 0.000000000000000000, 0.06249999999613299606, 0.09374999999417588104, 0.1093749999931755840, 0.1171874999926754285, 0.1210937499924412686, 0.1230468749923069038, 0.1240234374922550842, 0.1249999999922032645, 0.1874999999915968607, 0.2187499999912936588, 0.2343749999911442228, 0.2421874999910673953, 0.2460937499910139659, 0.2480468749909872650, 0.2490234374909866266, 0.2499999999909859882, 0.3749999999922498661, 0.4374999999928675942, 0.4687499999931619699, 0.4843749999933071870, 0.4921874999933816830, 0.4960937499934078287, 0.4980468749934336969, 0.4990234374934356398, 0.4999999999934376937, 0.6249999999958949504, 0.6874999999971151965, 0.7187499999977342569, 0.7343749999980366816, 0.7421874999981893373, 0.7460937499982656096, 0.7480468749983038013, 0.7490234374983243404, 0.7495117187483266719, 0.7499999999983288923, 0.8124999999987432275, 0.8437499999989501731, 0.8593749999990548671, 0.8749999999991596722, 1.000000000000000000 ),
 .UNSPECIFIED. ) ;
#1715 = CARTESIAN_POINT ( 'NONE',  ( 2.632641773180000477, 1417.642867858430009, 234.7516729256979886 ) ) ;
#1716 = CARTESIAN_POINT ( 'NONE',  ( 3.297786776830000210, 1446.227578061590066, 199.9593577526889874 ) ) ;
#1717 = CARTESIAN_POINT ( 'NONE',  ( -113.4000000000000057, 1306.483669372790018, 297.4506287831990221 ) ) ;
#1718 = CARTESIAN_POINT ( 'NONE',  ( -9.441793314685410721, 1368.076698943698375, 210.6218459617030021 ) ) ;
#1719 = CARTESIAN_POINT ( 'NONE',  ( -17.04962538713110121, 1486.805668029350045, 197.2415639623459924 ) ) ;
#1720 = CARTESIAN_POINT ( 'NONE',  ( -15.69795926999090163, 1517.151704408390060, 195.4758181584410011 ) ) ;
#1721 = CARTESIAN_POINT ( 'NONE',  ( 2.282622912365000367, 1516.861367446839949, 206.8218623544969716 ) ) ;
#1722 = CARTESIAN_POINT ( 'NONE',  ( -12.94800087099079988, 1434.761335965779836, 149.4045837073300049 ) ) ;
#1723 = B_SPLINE_CURVE_WITH_KNOTS ( 'NONE', 3,
 ( #35580, #37799, #61924, #53513, #18212, #79259, #10375, #88205, #2569, #97149, #11499, #78131, #52408, #9827, #20418, #36146, #88756, #44548, #19873, #45117, #3119, #105562, #54080, #104442, #95491, #94943, #45675, #79813, #18759, #87656, #43996, #86533, #12039, #27189, #80355, #37247, #71445, #28848, #46221, #3671, #103314, #2010, #26622, #1434, #60818, #69772 ),
 .UNSPECIFIED., .F., .F.,
 ( 4, 3, 3, 3, 3, 3, 3, 3, 3, 3, 3, 3, 3, 3, 3, 4 ),
 ( 10.13148339209999982, 11.92987739649050027, 12.20407613010000070, 14.42827119532750046, 16.14045415531399996, 17.68759836607059910, 19.09865219163459926, 19.90566978349999872, 21.14179169827090021, 22.42859032020150067, 23.78131544472190129, 25.30278979458900324, 26.99779043053199956, 29.30852037210000560, 29.67356826380000001, 30.47641535120000356 ),
 .UNSPECIFIED. ) ;
#1724 = B_SPLINE_SURFACE_WITH_KNOTS ( 'NONE', 5, 1, ( 
 ( #92066, #41669 ),
 ( #83658, #94260 ),
 ( #57933, #15338 ),
 ( #49533, #76934 ),
 ( #15879, #66891 ),
 ( #42221, #42773 ) ),
 .UNSPECIFIED., .F., .F., .F.,
 ( 6, 6 ),
 ( 2, 2 ),
 ( 0.000000000000000000, 3.703380931809999943 ),
 ( 0.000000000000000000, 14.00000000000000000 ),
 .UNSPECIFIED. ) ;
#1725 = CARTESIAN_POINT ( 'NONE',  ( -10.81507089441019964, 1424.921187596680056, 144.1620444830689962 ) ) ;
#1726 = CARTESIAN_POINT ( 'NONE',  ( 44.07821130980000390, 1452.218472917530107, 269.0164675534979892 ) ) ;
#1728 = ORIENTED_EDGE ( 'NONE', *, *, #7058, .T. ) ;
#1727 = CARTESIAN_POINT ( 'NONE',  ( 0.1390463022569990159, 1495.976490991190076, 221.0825533988989946 ) ) ;
#1729 = DIRECTION ( 'NONE',  ( 0.02091224828123159837, -0.9990482215818557998, 0.03827961371219689574 ) ) ;
#1730 = ORIENTED_EDGE ( 'NONE', *, *, #66449, .F. ) ;
#1731 = FACE_OUTER_BOUND ( 'NONE', #74136, .T. ) ;
#1732 = CARTESIAN_POINT ( 'NONE',  ( -27.27473106140000070, 1488.690404415530111, 208.0215548677279855 ) ) ;
#1734 = CARTESIAN_POINT ( 'NONE',  ( 16.18670465684310145, 1409.478287066380062, 193.0621080980399995 ) ) ;
#1733 = CARTESIAN_POINT ( 'NONE',  ( -10.90364899684709954, 1425.308507793300123, 127.8401879169430089 ) ) ;
#1735 = CARTESIAN_POINT ( 'NONE',  ( 1.716392741775000008, 1516.788317650260069, 211.9856338259669997 ) ) ;
#1736 = DIRECTION ( 'NONE',  ( -0.1402804634180439824, 0.9901118076173108795, 3.469446951951086598E-18 ) ) ;
#1737 = VECTOR ( 'NONE', #83866, 1000.000000000000227 ) ;
#1738 = CARTESIAN_POINT ( 'NONE',  ( 1.763299156880000132E-09, 1413.741945241729809, 248.5896189551980058 ) ) ;
#1739 = CARTESIAN_POINT ( 'NONE',  ( -13.86717347501279995, 1379.678627288110192, 208.3009849253440109 ) ) ;
#1741 = EDGE_CURVE ( 'NONE', #35056, #37407, #61947, .T. ) ;
#1740 = CARTESIAN_POINT ( 'NONE',  ( 28.25247054925810275, 1508.179583159759886, 209.3874533882519984 ) ) ;
#1742 = CARTESIAN_POINT ( 'NONE',  ( 3.664296634863810187, 1508.551704408389924, 213.8143107331380008 ) ) ;
#1743 = FACE_OUTER_BOUND ( 'NONE', #8453, .T. ) ;
#1744 = ORIENTED_EDGE ( 'NONE', *, *, #703, .T. ) ;
#1745 = CARTESIAN_POINT ( 'NONE',  ( 5.519893427111519202, 1440.499866072189889, 154.7645221071819890 ) ) ;
#1746 = CARTESIAN_POINT ( 'NONE',  ( 10.57327070435720096, 1460.185313085440157, 206.4178343085929725 ) ) ;
#1747 = EDGE_CURVE ( 'NONE', #43414, #35107, #74345, .T. ) ;
#1748 = CARTESIAN_POINT ( 'NONE',  ( -16.94875024379999928, 1459.649199545330021, 228.5285952991980025 ) ) ;
#1749 = ORIENTED_EDGE ( 'NONE', *, *, #3895, .F. ) ;
#1750 = ORIENTED_EDGE ( 'NONE', *, *, #94245, .T. ) ;
#1751 = DIRECTION ( 'NONE',  ( -0.7414773880254664773, 0.000000000000000000, 0.6709778558543730842 ) ) ;
#1752 = CARTESIAN_POINT ( 'NONE',  ( 8.386023354940000729, 1423.866883236690001, 196.1572597689990118 ) ) ;
#1753 = EDGE_CURVE ( 'NONE', #23788, #59464, #24444, .T. ) ;
#1754 = ORIENTED_EDGE ( 'NONE', *, *, #76872, .F. ) ;
#1755 = CARTESIAN_POINT ( 'NONE',  ( -0.7091552652710000348, 1410.300368832030017, 185.1037611371980063 ) ) ;
#1756 = CARTESIAN_POINT ( 'NONE',  ( 9.348425627764461510, 1446.614265060813068, 153.6205959845594577 ) ) ;
#1757 = CARTESIAN_POINT ( 'NONE',  ( 17.84338787571921969, 1512.187213306747481, 180.3600277896298110 ) ) ;
#1758 = EDGE_CURVE ( 'NONE', #70893, #20110, #58084, .T. ) ;
#1759 = CARTESIAN_POINT ( 'NONE',  ( -0.5626263542969999198, 1461.199651506930195, 235.3168487328979950 ) ) ;
#1760 = CARTESIAN_POINT ( 'NONE',  ( 5.513240533218949579, 1508.551563895499839, 201.9548267187850001 ) ) ;
#1761 = CARTESIAN_POINT ( 'NONE',  ( 10.12479509396839994, 1452.415778204070193, 209.5091751999849805 ) ) ;
#1762 = DIRECTION ( 'NONE',  ( -0.5202960232132588514, 0.000000000000000000, -0.8539859765994216589 ) ) ;
#1763 = CARTESIAN_POINT ( 'NONE',  ( -102.6485531311329993, 1384.882470662279957, 296.6730287615140469 ) ) ;
#1764 = CARTESIAN_POINT ( 'NONE',  ( -7.719392420504999741, 1516.929962200689943, 202.5670673984569703 ) ) ;
#1765 = CARTESIAN_POINT ( 'NONE',  ( 0.01012488564660149991, 1516.989863902050047, 210.2497743036369968 ) ) ;
#1766 = ORIENTED_EDGE ( 'NONE', *, *, #67993, .T. ) ;
#1767 = CARTESIAN_POINT ( 'NONE',  ( 11.86158182214910006, 1432.020402734500067, 149.9731981294450236 ) ) ;
#1768 = AXIS2_PLACEMENT_3D ( 'NONE', #65477, #83348, #91749 ) ;
#1769 = CARTESIAN_POINT ( 'NONE',  ( 12.71821945952179256, 1445.010168364093943, 186.4037021029734547 ) ) ;
#1770 = ORIENTED_EDGE ( 'NONE', *, *, #81687, .F. ) ;
#1771 = LINE ( 'NONE', #96358, #74990 ) ;
#1772 = CARTESIAN_POINT ( 'NONE',  ( -7.764617407222809575, 1508.427764620530070, 219.4967056752809924 ) ) ;
#1773 = CARTESIAN_POINT ( 'NONE',  ( 2.890489020249999985, 1507.108937781629947, 235.9439513813980227 ) ) ;
#1774 = CARTESIAN_POINT ( 'NONE',  ( -9.335957737771540366, 1471.828384389039911, 213.1700668700030121 ) ) ;
#1775 = B_SPLINE_CURVE_WITH_KNOTS ( 'NONE', 3,
 ( #104351, #46129, #43897, #86441, #95403, #9732, #19787, #71903, #27644, #29295, #79173, #18666, #2480, #45027, #95952, #88122, #53988, #96507, #61830, #61287, #28195, #78040, #53415, #1348 ),
 .UNSPECIFIED., .F., .F.,
 ( 4, 2, 2, 2, 2, 1, 2, 2, 2, 1, 2, 2, 4 ),
 ( 0.000000000000000000, 0.1249999999999030775, 0.1874999999999517608, 0.2500000000000004441, 0.3750000000002716716, 0.4375000000004031775, 0.4687500000004693468, 0.5000000000005355716, 0.6250000000005783152, 0.6875000000005520029, 0.7187500000005322409, 0.7500000000005124789, 1.000000000000000000 ),
 .UNSPECIFIED. ) ;
#1776 = CARTESIAN_POINT ( 'NONE',  ( -5.752888337419999942, 1422.114707807429795, 186.4775914538980146 ) ) ;
#1777 = CIRCLE ( 'NONE', #8847, 1.000002395377252107 ) ;
#1778 = CARTESIAN_POINT ( 'NONE',  ( 2.236972126526609816, 1410.279550646489952, 269.6153997192959650 ) ) ;
#1779 = CARTESIAN_POINT ( 'NONE',  ( -2.370970874524632510, 1427.002265528473799, 137.0999999980979851 ) ) ;
#1780 = CARTESIAN_POINT ( 'NONE',  ( 10.26709333669999857, 1491.783873301489848, 213.2283046884589908 ) ) ;
#1781 = CARTESIAN_POINT ( 'NONE',  ( -41.95996988479999601, 1379.671663521220125, 226.0894461641589999 ) ) ;
#1782 = CARTESIAN_POINT ( 'NONE',  ( 0.03096724798627218528, 1410.169160866321590, 233.2107615507483445 ) ) ;
#1783 = CARTESIAN_POINT ( 'NONE',  ( -17.87013932006249917, 1448.191556807570123, 190.6845719629749851 ) ) ;
#1784 = CARTESIAN_POINT ( 'NONE',  ( -68.56276905708799063, 1379.747764319654607, 280.1490247722647950 ) ) ;
#1785 = CARTESIAN_POINT ( 'NONE',  ( 17.92235813230709951, 1421.133839370329952, 225.1061056996060188 ) ) ;
#1786 = EDGE_CURVE ( 'NONE', #39621, #5728, #110104, .T. ) ;
#1787 = CARTESIAN_POINT ( 'NONE',  ( -2.499950883797279921, 1420.112351832789955, 91.39149109222310585 ) ) ;
#1788 = VERTEX_POINT ( 'NONE', #48586 ) ;
#1789 = CARTESIAN_POINT ( 'NONE',  ( 4.290289617690000057, 1420.418457356630142, 243.9198229205979942 ) ) ;
#1790 = VECTOR ( 'NONE', #84858, 1000.000000000000000 ) ;
#1791 = CARTESIAN_POINT ( 'NONE',  ( 13.00933603280000028, 1434.785429338880022, 149.1498346358980029 ) ) ;
#1792 = CARTESIAN_POINT ( 'NONE',  ( -21.63849897568203673, 1519.551704408389924, 215.5584779398195678 ) ) ;
#1793 = CARTESIAN_POINT ( 'NONE',  ( 5.067689999509999765, 1506.887323632490052, 219.6537200326989989 ) ) ;
#1794 = ADVANCED_FACE ( 'NONE', ( #6010 ), #43808, .F. ) ;
#1795 = DIRECTION ( 'NONE',  ( -0.000000000000000000, -1.000000000000000000, -0.000000000000000000 ) ) ;
#1797 = ORIENTED_EDGE ( 'NONE', *, *, #100031, .F. ) ;
#1796 = CARTESIAN_POINT ( 'NONE',  ( -1.107569330198709956, 1515.100382602269974, 204.7933291353800200 ) ) ;
#1798 = CARTESIAN_POINT ( 'NONE',  ( -15.91585955922337980, 1416.028785253251044, 209.7484352619693198 ) ) ;
#1799 = CARTESIAN_POINT ( 'NONE',  ( -7.545064063707340729, 1384.907232462019920, 219.0876311385090105 ) ) ;
#1800 = CARTESIAN_POINT ( 'NONE',  ( -16.16142260170000000, 1416.488921252410137, 208.6362116258320043 ) ) ;
#1801 = CARTESIAN_POINT ( 'NONE',  ( 20.12874795999999833, 1473.837606016890049, 209.1218459616989946 ) ) ;
#1802 = CARTESIAN_POINT ( 'NONE',  ( 11.25155670613500014, 1512.842772631639946, 225.3231501446670109 ) ) ;
#1803 = CARTESIAN_POINT ( 'NONE',  ( 4.225988784556967914, 1370.419465002912375, 209.6763548415352432 ) ) ;
#1804 = CARTESIAN_POINT ( 'NONE',  ( 1.124603181250000139, 1449.146011021990034, 189.9697284036990368 ) ) ;
#1805 = FACE_OUTER_BOUND ( 'NONE', #29524, .T. ) ;
#1806 = CARTESIAN_POINT ( 'NONE',  ( -16.38335856736500062, 1512.258183966690012, 220.9924808180670084 ) ) ;
#1807 = CARTESIAN_POINT ( 'NONE',  ( 15.39869794680000048, 1410.406122991029861, 227.2465235211980144 ) ) ;
#1808 = CARTESIAN_POINT ( 'NONE',  ( -10.50091854186509899, 1480.819183498580060, 208.0986103929409694 ) ) ;
#1809 = CARTESIAN_POINT ( 'NONE',  ( -16.16510620389999886, 1460.221770685330057, 228.5003369000980058 ) ) ;
#1810 = AXIS2_PLACEMENT_3D ( 'NONE', #25428, #9218, #51212 ) ;
#1811 = CARTESIAN_POINT ( 'NONE',  ( -5.012317106364999830, 1517.020727862619879, 206.2534121335969814 ) ) ;
#1812 = CARTESIAN_POINT ( 'NONE',  ( 18.34911816089999803, 1408.676262367329855, 267.0969396382980108 ) ) ;
#1813 = CARTESIAN_POINT ( 'NONE',  ( -32.92528853941059452, 1523.611961620354123, 217.2368972417797863 ) ) ;
#1814 = CARTESIAN_POINT ( 'NONE',  ( 24.21241066229999817, 1488.577768217629909, 198.4900566605979861 ) ) ;
#1815 = CARTESIAN_POINT ( 'NONE',  ( -20.35145834579999757, 1427.842720165429682, 222.5291350759979991 ) ) ;
#1816 = DIRECTION ( 'NONE',  ( 0.000000000000000000, -1.000000000000000000, 3.531714064933559186E-16 ) ) ;
#1817 = DIRECTION ( 'NONE',  ( 0.1225044380228070551, 0.9831695928899274461, -0.1355367635786350333 ) ) ;
#1818 = CARTESIAN_POINT ( 'NONE',  ( 4.709520687179999499, 1480.407452823689937, 228.9869292435990076 ) ) ;
#1819 = B_SPLINE_CURVE_WITH_KNOTS ( 'NONE', 3,
 ( #30359, #12465, #46648, #5161, #89719, #12996, #55596, #65087, #4088, #38212 ),
 .UNSPECIFIED., .F., .F.,
 ( 4, 2, 2, 2, 4 ),
 ( 0.000000000000000000, 0.2500000000000224265, 0.3750000000000168754, 0.5000000000000113243, 1.000000000000000000 ),
 .UNSPECIFIED. ) ;
#1820 = FACE_OUTER_BOUND ( 'NONE', #94074, .T. ) ;
#1821 = CARTESIAN_POINT ( 'NONE',  ( -15.39672782999999967, 1414.987016207339821, 208.1293397230249980 ) ) ;
#1822 = AXIS2_PLACEMENT_3D ( 'NONE', #75535, #15573, #83352 ) ;
#1823 = CARTESIAN_POINT ( 'NONE',  ( -13.11094645300000039, 1442.914509522559911, 187.2395568284980243 ) ) ;
#1824 = CARTESIAN_POINT ( 'NONE',  ( -7.628194758486819715, 1383.866806825199774, 218.9897990120470013 ) ) ;
#1825 = CARTESIAN_POINT ( 'NONE',  ( -33.13365710820000487, 1436.983726026989871, 136.5854365510979846 ) ) ;
#1826 = CARTESIAN_POINT ( 'NONE',  ( -0.3973340087122340103, 1418.672806152889962, 184.7148007238050127 ) ) ;
#1827 = ORIENTED_EDGE ( 'NONE', *, *, #23117, .T. ) ;
#1828 = CARTESIAN_POINT ( 'NONE',  ( -2.229731647334999955, 1512.142919181319940, 201.5278066827870020 ) ) ;
#1829 = CARTESIAN_POINT ( 'NONE',  ( -14.78586735916750072, 1409.429394253109876, 211.1975209631870030 ) ) ;
#1830 = B_SPLINE_SURFACE_WITH_KNOTS ( 'NONE', 4, 5, ( 
 ( #33681, #84640, #14686, #84092, #109319, #23639 ),
 ( #32602, #7936, #15755, #82458, #66779, #39897 ),
 ( #67875, #48874, #33136, #100878, #24171, #7393 ),
 ( #56707, #14127, #41558, #57281, #22505, #75713 ),
 ( #109859, #16315, #74066, #67324, #5755, #74616 ) ),
 .UNSPECIFIED., .F., .F., .F.,
 ( 5, 5 ),
 ( 6, 6 ),
 ( 4.528383477379999356, 21.94916619720000028 ),
 ( 0.000000000000000000, 1.000000000000000000 ),
 .UNSPECIFIED. ) ;
#1831 = CARTESIAN_POINT ( 'NONE',  ( 17.14950075666149587, 1517.051704408389924, 222.8506259189660170 ) ) ;
#1832 = DIRECTION ( 'NONE',  ( 0.000000000000000000, 1.000000000000000000, 0.000000000000000000 ) ) ;
#1833 = CARTESIAN_POINT ( 'NONE',  ( -30.03533176510000047, 1467.264374321729974, 268.9518348310980400 ) ) ;
#1834 = CARTESIAN_POINT ( 'NONE',  ( -30.15498238787951379, 1525.730671215514803, 196.9950476445848722 ) ) ;
#1835 = CARTESIAN_POINT ( 'NONE',  ( 0.1985875301063339815, 1419.813287738610143, 184.1956569253020177 ) ) ;
#1836 = LINE ( 'NONE', #44943, #68305 ) ;
#1837 = CARTESIAN_POINT ( 'NONE',  ( -69.10968088804719400, 1384.665037752149829, 294.0407317603679758 ) ) ;
#1838 = CARTESIAN_POINT ( 'NONE',  ( -15.47609788629169891, 1384.942714744960085, 200.6910050388860043 ) ) ;
#1839 = CARTESIAN_POINT ( 'NONE',  ( 17.85778552263929697, 1424.389883610459719, 228.2680410153979835 ) ) ;
#1840 = CARTESIAN_POINT ( 'NONE',  ( 13.50674874259999925, 1414.971287085330005, 218.9120235863680080 ) ) ;
#1841 = DIRECTION ( 'NONE',  ( -0.9993902469249968945, -0.03489947640978578736, 0.001077449542479110099 ) ) ;
#1842 = CARTESIAN_POINT ( 'NONE',  ( -27.08645728671159958, 1507.996806876479923, 211.2375099390570199 ) ) ;
#1843 = CARTESIAN_POINT ( 'NONE',  ( -1.105745987349477488, 1370.041125217912850, 206.9838924340121196 ) ) ;
#1844 = CARTESIAN_POINT ( 'NONE',  ( -9.985313959770000025, 1508.918243844630069, 181.8527837295979737 ) ) ;
#1845 = CARTESIAN_POINT ( 'NONE',  ( -22.70634968689999766, 1409.870434428829867, 205.6103426976079902 ) ) ;
#1846 = CARTESIAN_POINT ( 'NONE',  ( 16.17135635129999827, 1414.913060387329779, 206.5448528754380106 ) ) ;
#1847 = CARTESIAN_POINT ( 'NONE',  ( 3.394586460100000203, 1484.752177863690122, 220.4731790066989845 ) ) ;
#1848 = CIRCLE ( 'NONE', #64422, 1.999999999999998668 ) ;
#1849 = B_SPLINE_CURVE_WITH_KNOTS ( 'NONE', 3,
 ( #523, #1623, #2189, #26236, #59869, #52016, #79426, #60425, #104615, #18377, #10559, #35759, #52573, #70498, #53128, #27350, #69387, #86707, #27911, #10000, #9449, #18932, #62093, #87838, #43614, #93997, #77763, #17261, #51453, #85585, #61534, #34648, #95664, #68832, #1074, #102934, #94543, #35200, #103498, #71616, #79969, #90008, #28464, #55335, #21128, #54244, #106269, #56428 ),
 .UNSPECIFIED., .F., .F.,
 ( 4, 2, 2, 1, 1, 1, 1, 1, 2, 2, 2, 1, 1, 1, 2, 2, 2, 2, 2, 2, 2, 2, 2, 2, 2, 2, 2, 4 ),
 ( 0.000000000000000000, 0.2500000000005769274, 0.3750000000008642531, 0.4375000000010069168, 0.4687500000010855206, 0.4843750000011176615, 0.4921875000011337598, 0.4960937500011416978, 0.4980468750011447510, 0.5000000000011477486, 0.6250000000009476864, 0.6875000000008416601, 0.7187500000007887024, 0.7343750000007658318, 0.7421875000007500667, 0.7500000000007343015, 0.8125000000005889733, 0.8437500000005155876, 0.8593750000004759526, 0.8671875000004583001, 0.8710937500004467537, 0.8750000000004350964, 0.9062500000003413936, 0.9218750000002963185, 0.9296875000002715606, 0.9335937500002587930, 0.9375000000002459144, 1.000000000000000000 ),
 .UNSPECIFIED. ) ;
#1850 = DIRECTION ( 'NONE',  ( -0.9455185755993178454, 0.000000000000000000, 0.3255681544571537578 ) ) ;
#1851 = B_SPLINE_SURFACE_WITH_KNOTS ( 'NONE', 5, 5, ( 
 ( #43005, #53633, #53069, #87776, #1560, #77163 ),
 ( #68774, #35692, #70438, #52514, #102875, #26173 ),
 ( #87206, #69882, #60359, #94481, #2126, #17754 ),
 ( #51957, #1015, #35141, #60926, #95056, #18323 ),
 ( #9940, #36250, #27295, #103998, #29492, #72618 ),
 ( #72095, #2680, #79918, #64230, #12146, #38988 ),
 ( #79366, #105678, #3231, #63687, #55832, #80467 ),
 ( #54733, #88861, #90499, #106210, #46337, #73164 ),
 ( #13775, #37914, #97798, #105114, #55281, #97251 ),
 ( #89411, #107309, #98354, #54185, #28405, #96719 ),
 ( #3782, #28962, #62604, #71559, #19992, #30038 ),
 ( #37358, #21076, #63151, #70996, #38444, #106749 ) ),
 .UNSPECIFIED., .F., .F., .F.,
 ( 6, 3, 3, 6 ),
 ( 6, 6 ),
 ( 0.9635945383279999055, 4.198788347969999890, 5.913340936670000048, 6.825063656079999319 ),
 ( 0.000000000000000000, 2.000000000000000000 ),
 .UNSPECIFIED. ) ;
#1852 = CARTESIAN_POINT ( 'NONE',  ( -106.6950745027010043, 1391.913060387289988, 305.9031442834140080 ) ) ;
#1853 = CARTESIAN_POINT ( 'NONE',  ( -9.960918163209999676, 1449.652119265389956, 190.8907471528989959 ) ) ;
#1854 = CARTESIAN_POINT ( 'NONE',  ( 3.246772394788719929, 1511.187213306747708, 177.1492560608742224 ) ) ;
#1855 = CARTESIAN_POINT ( 'NONE',  ( 18.32583680416279748, 1473.764155899330035, 194.8973843979659932 ) ) ;
#1857 = CARTESIAN_POINT ( 'NONE',  ( -14.08318393682589864, 1379.709325990200114, 211.5303917806009792 ) ) ;
#1856 = CARTESIAN_POINT ( 'NONE',  ( -21.92806448420000009, 1409.678805267029929, 210.7898312680979984 ) ) ;
#1858 = CARTESIAN_POINT ( 'NONE',  ( -5.076113882429999613, 1391.871667267490011, 203.5799967627289675 ) ) ;
#1859 = DIRECTION ( 'NONE',  ( -1.755985294532469921E-16, 1.000000000000000000, -1.338183447452831989E-16 ) ) ;
#1860 = CONICAL_SURFACE ( 'NONE', #23233, 1.000000000000007327, 0.7853981633970000820 ) ;
#1861 = CARTESIAN_POINT ( 'NONE',  ( -15.26258821600000104, 1420.451304246630116, 211.3041522489459965 ) ) ;
#1862 = CARTESIAN_POINT ( 'NONE',  ( 9.538751646130227968, 1491.433371252692041, 189.9872483449992728 ) ) ;
#1863 = CARTESIAN_POINT ( 'NONE',  ( -8.696701630030000629, 1367.135748871429996, 210.6218459616991936 ) ) ;
#1864 = CARTESIAN_POINT ( 'NONE',  ( 7.324914918154999732, 1516.685667699390024, 204.5043554653269950 ) ) ;
#1865 = DIRECTION ( 'NONE',  ( 7.105427357601001859E-15, 0.000000000000000000, 1.000000000000000000 ) ) ;
#1866 = CARTESIAN_POINT ( 'NONE',  ( -14.26747435372389994, 1485.844175363280101, 186.1892725996659976 ) ) ;
#1867 = CARTESIAN_POINT ( 'NONE',  ( -18.24639174359999672, 1430.281446294329953, 193.9508323147979922 ) ) ;
#1868 = AXIS2_PLACEMENT_3D ( 'NONE', #1577, #95621, #69899 ) ;
#1869 = CARTESIAN_POINT ( 'NONE',  ( 6.506813043129500151, 1504.727164751039936, 219.6746885927560129 ) ) ;
#1870 = CARTESIAN_POINT ( 'NONE',  ( -34.18677586421173231, 1512.187213306747481, 219.7932833225216882 ) ) ;
#1872 = ORIENTED_EDGE ( 'NONE', *, *, #17077, .F. ) ;
#1871 = CARTESIAN_POINT ( 'NONE',  ( -65.43163292693739663, 1379.743657604059763, 275.4463174256679849 ) ) ;
#1873 = ORIENTED_EDGE ( 'NONE', *, *, #366, .T. ) ;
#1874 = CARTESIAN_POINT ( 'NONE',  ( 11.73806480614890013, 1433.731339164239898, 150.9439538071720222 ) ) ;
#1875 = CARTESIAN_POINT ( 'NONE',  ( 21.42841630977322254, 1524.678872986481338, 184.2224299175816782 ) ) ;
#1876 = VERTEX_POINT ( 'NONE', #26095 ) ;
#1877 = DIRECTION ( 'NONE',  ( 0.03489949655844001852, 0.9993908270241265157, 1.111776183576166572E-08 ) ) ;
#1878 = CARTESIAN_POINT ( 'NONE',  ( -10.29190872868499973, 1448.598814390959888, 207.7705778465489743 ) ) ;
#1880 = CARTESIAN_POINT ( 'NONE',  ( 11.30500403589999792, 1428.976642997429963, 112.4493539157979995 ) ) ;
#1879 = CARTESIAN_POINT ( 'NONE',  ( -32.37018134260410562, 1511.187213306747708, 200.1723992780599986 ) ) ;
#1881 = CARTESIAN_POINT ( 'NONE',  ( 4.039020860156879777, 1467.562285101070074, 215.1688013428469901 ) ) ;
#1882 = CARTESIAN_POINT ( 'NONE',  ( 0.4151546846821903003, 1512.187213306747481, 174.3106345060153046 ) ) ;
#1883 = CARTESIAN_POINT ( 'NONE',  ( -1.713873510270000011, 1469.335086563190089, 219.0204275940589866 ) ) ;
#1884 = CARTESIAN_POINT ( 'NONE',  ( -24.39284326694200189, 1444.780737751010065, 211.1468293442990216 ) ) ;
#1885 = ADVANCED_FACE ( 'NONE', ( #104481 ), #66090, .T. ) ;
#1886 = CARTESIAN_POINT ( 'NONE',  ( -0.7355686809059980291, 1517.012231669750008, 212.3888856620870058 ) ) ;
#1887 = CARTESIAN_POINT ( 'NONE',  ( 34.72084050058860072, 1435.748200648169814, 134.0999999979019890 ) ) ;
#1888 = CARTESIAN_POINT ( 'NONE',  ( -6.146133249640749696, 1425.318217922679878, 208.0573756490000221 ) ) ;
#1889 = CARTESIAN_POINT ( 'NONE',  ( -20.61186923340000021, 1484.905403178689994, 208.1155942278690247 ) ) ;
#1890 = ORIENTED_EDGE ( 'NONE', *, *, #68688, .F. ) ;
#1891 = CARTESIAN_POINT ( 'NONE',  ( 14.32178456671769951, 1435.822963899329807, 149.8685163660410069 ) ) ;
#1892 = DIRECTION ( 'NONE',  ( 0.4794255386042031719, 0.000000000000000000, 0.8775825618903726477 ) ) ;
#1893 = VERTEX_POINT ( 'NONE', #110668 ) ;
#1894 = VERTEX_POINT ( 'NONE', #27773 ) ;
#1895 = VERTEX_POINT ( 'NONE', #51314 ) ;
#1896 = CARTESIAN_POINT ( 'NONE',  ( 12.78525141209750871, 1444.986522992021037, 169.4510567559931644 ) ) ;
#1897 = CARTESIAN_POINT ( 'NONE',  ( -1.674556947779999971, 1464.910406147030017, 237.1062727332979989 ) ) ;
#1898 = VECTOR ( 'NONE', #41052, 1000.000000000000000 ) ;
#1899 = CARTESIAN_POINT ( 'NONE',  ( 25.25200551730000242, 1450.804230319249882, 137.6134878989979882 ) ) ;
#1900 = CARTESIAN_POINT ( 'NONE',  ( 7.550503318189189628, 1510.480349263560129, 203.5706572562480119 ) ) ;
#1901 = CARTESIAN_POINT ( 'NONE',  ( 10.14837267200000070, 1461.673059420789968, 209.1843067467119965 ) ) ;
#1902 = CARTESIAN_POINT ( 'NONE',  ( 40.27308137180000358, 1443.612049545939954, 137.1163288300980128 ) ) ;
#1903 = CARTESIAN_POINT ( 'NONE',  ( -44.66902661210603043, 1379.669579522011190, 230.0472852312407497 ) ) ;
#1904 = CARTESIAN_POINT ( 'NONE',  ( 4.272474999264660234, 1446.725045888410023, 157.6426782973369995 ) ) ;
#1905 = EDGE_CURVE ( 'NONE', #90721, #25072, #15288, .T. ) ;
#1906 = CARTESIAN_POINT ( 'NONE',  ( 0.4073663215339999866, 1508.683555889429954, 238.1699978998979930 ) ) ;
#1907 = VERTEX_POINT ( 'NONE', #61964 ) ;
#1908 = CARTESIAN_POINT ( 'NONE',  ( 5.771797426184999580, 1516.647618671360078, 206.2459958378869942 ) ) ;
#1909 = ORIENTED_EDGE ( 'NONE', *, *, #65995, .T. ) ;
#1910 = CARTESIAN_POINT ( 'NONE',  ( 25.66502446409790039, 1440.913060387330006, 241.2077300345669926 ) ) ;
#1911 = AXIS2_PLACEMENT_3D ( 'NONE', #63244, #45873, #62132 ) ;
#1912 = CARTESIAN_POINT ( 'NONE',  ( -13.70491113640000158, 1508.146349762730097, 184.2329986728979918 ) ) ;
#1913 = ORIENTED_EDGE ( 'NONE', *, *, #78321, .T. ) ;
#1914 = CARTESIAN_POINT ( 'NONE',  ( -6.766176630772359424, 1508.878902422570036, 201.8612697231370134 ) ) ;
#1915 = EDGE_CURVE ( 'NONE', #68857, #40412, #43486, .T. ) ;
#1916 = CARTESIAN_POINT ( 'NONE',  ( -14.51125708719999885, 1410.352142336630095, 190.4994541838979956 ) ) ;
#1917 = CARTESIAN_POINT ( 'NONE',  ( -24.35464616639999846, 1441.602688108240045, 211.7287004059179765 ) ) ;
#1918 = CARTESIAN_POINT ( 'NONE',  ( -2.370970874524632510, 1427.002265528473799, 137.0999999980979851 ) ) ;
#1919 = FACE_OUTER_BOUND ( 'NONE', #94382, .T. ) ;
#1920 = CARTESIAN_POINT ( 'NONE',  ( -14.49568595290499928, 1514.921196705999819, 193.9190483465280010 ) ) ;
#1921 = CARTESIAN_POINT ( 'NONE',  ( 17.05226155321927095, 1516.729020916208583, 222.6134475786040525 ) ) ;
#1922 = CARTESIAN_POINT ( 'NONE',  ( -3.318767601309999815, 1508.056473026189906, 220.8617977084990116 ) ) ;
#1924 = CARTESIAN_POINT ( 'NONE',  ( -105.0581303879369983, 1379.236400313860031, 304.0328620142400382 ) ) ;
#1923 = CARTESIAN_POINT ( 'NONE',  ( -25.77261374515159886, 1483.519019013160005, 212.0189592763409792 ) ) ;
#1925 = CARTESIAN_POINT ( 'NONE',  ( 0.01289778877310149806, 1516.939723362869927, 214.1281058189269970 ) ) ;
#1926 = DIRECTION ( 'NONE',  ( 0.000000000000000000, 0.000000000000000000, -1.000000000000000000 ) ) ;
#1927 = CARTESIAN_POINT ( 'NONE',  ( 6.247704779676360509, 1510.876154134890157, 216.5661308656380015 ) ) ;
#1928 = CARTESIAN_POINT ( 'NONE',  ( 28.26084317239999777, 1508.649017702329957, 208.6067999643450150 ) ) ;
#1929 = CARTESIAN_POINT ( 'NONE',  ( 2.493073829755000137, 1516.826109302209943, 211.9861720575370043 ) ) ;
#1930 = CARTESIAN_POINT ( 'NONE',  ( 14.54195235379999929, 1410.802016681730038, 191.4776931444980050 ) ) ;
#1931 = ADVANCED_FACE ( 'NONE', ( #27226 ), #69810, .F. ) ;
#1932 = CARTESIAN_POINT ( 'NONE',  ( 30.15954682509860518, 1524.412928176728883, 222.4099428256023145 ) ) ;
#1934 = VERTEX_POINT ( 'NONE', #95529 ) ;
#1933 = CARTESIAN_POINT ( 'NONE',  ( -74.25289801200000284, 1388.141632471819776, 298.2335420860590034 ) ) ;
#1935 = CARTESIAN_POINT ( 'NONE',  ( -0.5943821362719999835, 1416.311719779230089, 227.7090535903980140 ) ) ;
#1936 = CARTESIAN_POINT ( 'NONE',  ( 26.69977470740000314, 1442.651301016559955, 225.7788486252980249 ) ) ;
#1937 = CARTESIAN_POINT ( 'NONE',  ( 5.939587785669203868, 1485.462588962051768, 218.1262196687094388 ) ) ;
#1938 = PLANE ( 'NONE',  #73670 ) ;
#1939 = CARTESIAN_POINT ( 'NONE',  ( -5.309335150381779833, 1508.059062283110052, 236.4392518008919808 ) ) ;
#1940 = CARTESIAN_POINT ( 'NONE',  ( -10.33299517979799909, 1447.717325788079961, 209.8084994951809961 ) ) ;
#1942 = CARTESIAN_POINT ( 'NONE',  ( 19.24310214189999968, 1455.949671055829867, 226.1911111612980108 ) ) ;
#1941 = CARTESIAN_POINT ( 'NONE',  ( 11.77874534290000064, 1433.007534236340007, 150.8097953682980119 ) ) ;
#1943 = CARTESIAN_POINT ( 'NONE',  ( -9.135375560561769248, 1450.134946103599987, 207.9596124096709673 ) ) ;
#1944 = CARTESIAN_POINT ( 'NONE',  ( -105.6599733740739993, 1378.369188341159997, 305.5461949359690266 ) ) ;
#1945 = VERTEX_POINT ( 'NONE', #102263 ) ;
#1946 = CARTESIAN_POINT ( 'NONE',  ( 5.000083827734999709, 1516.858456333729919, 204.1129977322069919 ) ) ;
#1947 = CARTESIAN_POINT ( 'NONE',  ( 0.2161160260170000014, 1405.776202818429965, 268.4837592986979757 ) ) ;
#1948 = VECTOR ( 'NONE', #101539, 1000.000000000000114 ) ;
#1949 = CARTESIAN_POINT ( 'NONE',  ( 28.66995857139999870, 1509.914237401530045, 206.7534942493879839 ) ) ;
#1950 = CARTESIAN_POINT ( 'NONE',  ( 30.57166591494479846, 1464.042419567909974, 270.1181552200280294 ) ) ;
#1951 = CARTESIAN_POINT ( 'NONE',  ( 5.405732451549999595, 1434.707887834109897, 154.6595955769979867 ) ) ;
#1952 = CARTESIAN_POINT ( 'NONE',  ( 20.78416965899999980, 1496.368170310390042, 205.3334059301089951 ) ) ;
#1953 = CARTESIAN_POINT ( 'NONE',  ( -0.3966884594078615711, 1469.475063426553106, 219.1656958591027831 ) ) ;
#1954 = CARTESIAN_POINT ( 'NONE',  ( -36.06691658716020044, 1440.913060387480073, 252.9701890490810285 ) ) ;
#1955 = CARTESIAN_POINT ( 'NONE',  ( 33.91369266730000476, 1450.440660192670066, 136.2454535554979884 ) ) ;
#1956 = CARTESIAN_POINT ( 'NONE',  ( 21.62164173326539895, 1519.551704408389924, 208.0273405521070060 ) ) ;
#1957 = CARTESIAN_POINT ( 'NONE',  ( 1.248319727109999944, 1432.832940530890028, 200.7627304074090091 ) ) ;
#1958 = CARTESIAN_POINT ( 'NONE',  ( 2.500592263345220001, 1448.944489456090196, 154.5202628404780114 ) ) ;
#1959 = CARTESIAN_POINT ( 'NONE',  ( 2.586184907469999850, 1507.324410716090142, 220.5577431766989775 ) ) ;
#1960 = FACE_OUTER_BOUND ( 'NONE', #14772, .T. ) ;
#1962 = DIRECTION ( 'NONE',  ( -1.755985294532464991E-16, 1.000000000000000000, -1.338183447452830017E-16 ) ) ;
#1961 = CIRCLE ( 'NONE', #12873, 1.999999999999998668 ) ;
#1963 = EDGE_LOOP ( 'NONE', ( #6488, #63190, #36975, #109476, #109814 ) ) ;
#1964 = CARTESIAN_POINT ( 'NONE',  ( -12.85916294159999929, 1411.892799971530167, 268.3665355202980436 ) ) ;
#1965 = CARTESIAN_POINT ( 'NONE',  ( -0.09132851563079860679, 1485.606224300089934, 197.9629336334990057 ) ) ;
#1966 = CARTESIAN_POINT ( 'NONE',  ( 8.026943330234900031, 1467.154782912119799, 202.9971560891700051 ) ) ;
#1967 = AXIS2_PLACEMENT_3D ( 'NONE', #95143, #19521, #53727 ) ;
#1968 = CARTESIAN_POINT ( 'NONE',  ( -1.331593054780000118, 1475.969838803829816, 267.2342691169980640 ) ) ;
#1969 = CARTESIAN_POINT ( 'NONE',  ( -33.91369114349999592, 1451.728768196330066, 134.7155300131979914 ) ) ;
#1970 = CARTESIAN_POINT ( 'NONE',  ( -27.79064038249999768, 1508.605033447930055, 210.4916515659980121 ) ) ;
#1971 = CARTESIAN_POINT ( 'NONE',  ( 8.528404547750000120, 1427.401138475999915, 211.7487601184689936 ) ) ;
#1972 = CARTESIAN_POINT ( 'NONE',  ( -9.627136608023121767, 1384.891069265470151, 218.7309310236159945 ) ) ;
#1973 = CARTESIAN_POINT ( 'NONE',  ( -18.41105348850000212, 1415.553739807329976, 208.0605876747880245 ) ) ;
#1974 = CIRCLE ( 'NONE', #59192, 2.000000000000001776 ) ;
#1975 = B_SPLINE_CURVE_WITH_KNOTS ( 'NONE', 3,
 ( #55220, #37302, #79860, #82037, #11547, #12644 ),
 .UNSPECIFIED., .F., .F.,
 ( 4, 2, 4 ),
 ( -1.285435071114344984E-05, 0.001079388306740470182, 0.002171630964192083728 ),
 .UNSPECIFIED. ) ;
#1976 = CARTESIAN_POINT ( 'NONE',  ( -9.604374367299998383, 1481.821681780390008, 204.6246279580790031 ) ) ;
#1977 = CARTESIAN_POINT ( 'NONE',  ( 26.66179749201589644, 1435.630288477099839, 136.0743949063709977 ) ) ;
#1978 = CARTESIAN_POINT ( 'NONE',  ( -5.343479917770609156, 1396.099658817820000, 199.4684377796870081 ) ) ;
#1979 = ORIENTED_EDGE ( 'NONE', *, *, #8655, .T. ) ;
#1980 = CONICAL_SURFACE ( 'NONE', #64570, 0.9999999999999962252, 0.7853981633970000820 ) ;
#1981 = CARTESIAN_POINT ( 'NONE',  ( -17.21443206581249896, 1410.737832039549858, 226.0138299294659987 ) ) ;
#1982 = CARTESIAN_POINT ( 'NONE',  ( 7.450897614389999646, 1442.756953654919926, 149.7755488681980012 ) ) ;
#1983 = ORIENTED_EDGE ( 'NONE', *, *, #38974, .T. ) ;
#1984 = CARTESIAN_POINT ( 'NONE',  ( -19.65008011549999978, 1466.825520213989876, 211.9829227778189988 ) ) ;
#1985 = CARTESIAN_POINT ( 'NONE',  ( -15.29554544528689597, 1416.036841487845777, 206.5879621630117242 ) ) ;
#1986 = FACE_OUTER_BOUND ( 'NONE', #45042, .T. ) ;
#1988 = CARTESIAN_POINT ( 'NONE',  ( -9.821317627027500663, 1438.502739476040233, 210.5947021706759870 ) ) ;
#1987 = CARTESIAN_POINT ( 'NONE',  ( 9.946025746629999276, 1425.248710433229917, 91.15452341569790917 ) ) ;
#1989 = CARTESIAN_POINT ( 'NONE',  ( 0.1076058614650010070, 1458.116229757589963, 202.2619487776389917 ) ) ;
#1990 = CARTESIAN_POINT ( 'NONE',  ( 4.237000157206120221, 1423.967056607189988, 184.0491610448669917 ) ) ;
#1991 = CARTESIAN_POINT ( 'NONE',  ( -5.004442077115000664, 1516.690345681169902, 201.4087281291169802 ) ) ;
#1992 = CARTESIAN_POINT ( 'NONE',  ( 7.540798545940000430, 1425.730109158910182, 212.1916703474689996 ) ) ;
#1993 = CARTESIAN_POINT ( 'NONE',  ( 4.677562605459999467, 1434.889072344290071, 228.7640133631989841 ) ) ;
#1994 = CARTESIAN_POINT ( 'NONE',  ( -23.79000955475941836, 1411.113042535969726, 210.2403600569826096 ) ) ;
#1995 = CARTESIAN_POINT ( 'NONE',  ( 8.126234247455000670, 1514.923664147150021, 215.2485921136969864 ) ) ;
#1996 = CARTESIAN_POINT ( 'NONE',  ( 3.264324498270000152, 1450.280157591569832, 183.9712559857979954 ) ) ;
#1997 = CARTESIAN_POINT ( 'NONE',  ( 9.671060821790000261, 1366.060403940050037, 207.6218459616989946 ) ) ;
#1999 = ORIENTED_EDGE ( 'NONE', *, *, #72805, .F. ) ;
#1998 = CARTESIAN_POINT ( 'NONE',  ( 5.588245553200000160, 1454.953086687389941, 217.2248557766390036 ) ) ;
#2000 = ORIENTED_EDGE ( 'NONE', *, *, #5665, .F. ) ;
#2001 = PLANE ( 'NONE',  #78383 ) ;
#2002 = CARTESIAN_POINT ( 'NONE',  ( -0.3541148012579999893, 1466.691116367230052, 235.5895199573979824 ) ) ;
#2003 = CARTESIAN_POINT ( 'NONE',  ( -0.4843842464630000455, 1473.264972808229913, 270.4290818601980391 ) ) ;
#2004 = CARTESIAN_POINT ( 'NONE',  ( -8.463742342545000241, 1511.382391139620040, 213.9463409611770146 ) ) ;
#2005 =( BOUNDED_CURVE ( )  B_SPLINE_CURVE ( 3, ( #34455, #41747, #68630, #75906 ),
 .UNSPECIFIED., .F., .F. ) 
 B_SPLINE_CURVE_WITH_KNOTS ( ( 4, 4 ),
 ( 4.612172254335380472, 4.862528044142459649 ),
 .UNSPECIFIED. ) 
 CURVE ( )  GEOMETRIC_REPRESENTATION_ITEM ( )  RATIONAL_B_SPLINE_CURVE ( ( 1.000000000000000000, 0.9947836483532912499, 0.9947836483532912499, 1.000000000000000000 ) ) 
 REPRESENTATION_ITEM ( '' )  );
#2006 = CARTESIAN_POINT ( 'NONE',  ( -121.4211954113600029, 1309.112692017090239, 304.2218459572590064 ) ) ;
#2007 = CARTESIAN_POINT ( 'NONE',  ( -32.54505059146748636, 1524.547395018738371, 201.1603553390793877 ) ) ;
#2008 = CARTESIAN_POINT ( 'NONE',  ( -2.333876373187340203, 1475.197367001489965, 197.9245314158600024 ) ) ;
#2009 = CARTESIAN_POINT ( 'NONE',  ( 12.48640425065659976, 1423.660394517820123, 223.7918487953089937 ) ) ;
#2010 = CARTESIAN_POINT ( 'NONE',  ( -2.500000000000000000, 1448.204021880610071, 169.8582428316960033 ) ) ;
#2011 = CARTESIAN_POINT ( 'NONE',  ( 9.222591024579390506, 1396.235120365410012, 215.2291610791590131 ) ) ;
#2012 = CARTESIAN_POINT ( 'NONE',  ( 3.205045813472149785, 1408.488127767880087, 195.5730862361089919 ) ) ;
#2013 = DIRECTION ( 'NONE',  ( 0.2020439943617916845, -0.9583089389155642346, 0.2020450492757928096 ) ) ;
#2014 = CARTESIAN_POINT ( 'NONE',  ( -10.93238010534558313, 1414.913060581097170, 195.9940915879461159 ) ) ;
#2015 = ORIENTED_EDGE ( 'NONE', *, *, #26089, .F. ) ;
#2016 = CARTESIAN_POINT ( 'NONE',  ( 3.827327205999999649, 1424.046157813729906, 183.3886489380980152 ) ) ;
#2017 = CARTESIAN_POINT ( 'NONE',  ( 12.85143379750000037, 1446.481137621939979, 188.4927750485979914 ) ) ;
#2018 = ORIENTED_EDGE ( 'NONE', *, *, #878, .T. ) ;
#2019 = ORIENTED_EDGE ( 'NONE', *, *, #82259, .F. ) ;
#2020 = B_SPLINE_CURVE_WITH_KNOTS ( 'NONE', 3,
 ( #107977, #22849, #101210, #92280, #83329, #22292, #15549, #55945, #31274, #13903, #6625, #48090, #32384, #65458, #40779, #99565, #74955, #66567, #49749, #90066, #13348, #47541, #41882, #78240, #7722, #85518, #459, #33457, #93923, #92829, #103424, #8264, #16104, #86637, #9932, #77696, #68220, #84970, #44102, #50839, #34581, #50308, #8814, #102325, #84438, #24506, #25611, #102869, #59803, #76587, #60920, #1553, #35134, #17190, #51386, #42997, #77155, #1007, #68766, #26166, #60352, #93376, #52508, #76041, #42428, #34029, #110186, #58697, #67659, #110738, #35685, #94475, #17748, #86092, #51950, #69876, #9386, #25056, #95049 ),
 .UNSPECIFIED., .F., .F.,
 ( 4, 3, 3, 3, 3, 3, 3, 3, 3, 3, 3, 3, 3, 3, 3, 3, 3, 3, 3, 3, 3, 3, 3, 3, 3, 3, 4 ),
 ( 0.000000000000000000, 0.4548555274129320036, 0.9190079891053550831, 1.398119237412919880, 1.886365508051579987, 2.387648495461230258, 2.516896244989999865, 3.033433463757130077, 3.554872652308640024, 4.076782264074299889, 4.594593341653459895, 5.099843107827240374, 5.596159927621140007, 6.077963950408490135, 6.410372910170000438, 7.036818067524451159, 7.682305271035700933, 8.346433156759069050, 9.030012755689879711, 9.715260639136369392, 10.38844028647699780, 10.64487668199999959, 11.49777674247360082, 12.38410586200980035, 13.29134611626929896, 14.23087319025490061, 14.62789107123472121 ),
 .UNSPECIFIED. ) ;
#2021 = CARTESIAN_POINT ( 'NONE',  ( -3.467945401910000225, 1455.040194281890081, 200.2251794624690149 ) ) ;
#2022 = CARTESIAN_POINT ( 'NONE',  ( 8.379275254590000443, 1362.454991452509830, 207.6218459616989946 ) ) ;
#2023 = CARTESIAN_POINT ( 'NONE',  ( 2.490245914424999985, 1516.691389976299888, 213.7302634767470124 ) ) ;
#2024 = CARTESIAN_POINT ( 'NONE',  ( 4.036380747524999535, 1511.355055856609852, 217.1076883285369945 ) ) ;
#2025 = AXIS2_PLACEMENT_3D ( 'NONE', #103889, #7617, #68656 ) ;
#2026 = ORIENTED_EDGE ( 'NONE', *, *, #78076, .F. ) ;
#2027 = CARTESIAN_POINT ( 'NONE',  ( -77.18524044800000183, 1379.656469663269945, 292.4664101653590365 ) ) ;
#2028 = B_SPLINE_CURVE_WITH_KNOTS ( 'NONE', 3,
 ( #5077, #83430, #49305, #5644, #14573, #57169 ),
 .UNSPECIFIED., .F., .F.,
 ( 4, 2, 4 ),
 ( -0.2778631976372760159, -0.1390217908135579772, -1.347131930007350320E-06 ),
 .UNSPECIFIED. ) ;
#2029 = AXIS2_PLACEMENT_3D ( 'NONE', #73611, #81412, #69901 ) ;
#2030 = CARTESIAN_POINT ( 'NONE',  ( 10.07457632729999908, 1416.825421876529845, 224.7882279959979996 ) ) ;
#2031 = CARTESIAN_POINT ( 'NONE',  ( 5.000083827734999709, 1516.858456333729919, 204.1129977322069919 ) ) ;
#2032 = CARTESIAN_POINT ( 'NONE',  ( 30.31052258194596760, 1523.604703353109699, 222.4930856806589645 ) ) ;
#2033 = CARTESIAN_POINT ( 'NONE',  ( -5425.877332847427169, 54.28084076250834755, 8448.741457306947268 ) ) ;
#2034 = CARTESIAN_POINT ( 'NONE',  ( -113.4000000000000057, 1385.138976307909843, 297.2272069998589927 ) ) ;
#2035 = CARTESIAN_POINT ( 'NONE',  ( -60.36450283880899548, 1384.675237924389876, 244.7949774597909993 ) ) ;
#2036 = CARTESIAN_POINT ( 'NONE',  ( 9.634908749268699779, 1462.534321465409903, 207.6260219664079898 ) ) ;
#2037 = CARTESIAN_POINT ( 'NONE',  ( -5.943866765360000137, 1409.623546987629879, 231.2954894698980013 ) ) ;
#2039 = ORIENTED_EDGE ( 'NONE', *, *, #25225, .T. ) ;
#2038 = CARTESIAN_POINT ( 'NONE',  ( -8.896201126819999416, 1446.954173154499813, 186.2107498446980003 ) ) ;
#2040 = CARTESIAN_POINT ( 'NONE',  ( -14.56153818869126049, 1435.986600758549912, 149.8060885009444974 ) ) ;
#2041 = CARTESIAN_POINT ( 'NONE',  ( 1.734605482336269988, 1474.701058242480030, 235.0720777047329761 ) ) ;
#2042 = CARTESIAN_POINT ( 'NONE',  ( 20.73258896465929979, 1507.783937758249749, 226.5135743084329931 ) ) ;
#2043 = DIRECTION ( 'NONE',  ( -0.9211327884476211425, -0.3892484888175031799, 0.000000000000000000 ) ) ;
#2044 = CARTESIAN_POINT ( 'NONE',  ( -25.23204818860000032, 1435.454757579879924, 136.2099880446980080 ) ) ;
#2045 = CIRCLE ( 'NONE', #64625, 2.000000000000003109 ) ;
#2046 = CARTESIAN_POINT ( 'NONE',  ( 0.7574259850960020080, 1516.837969789639828, 212.3776558342370038 ) ) ;
#2047 = CARTESIAN_POINT ( 'NONE',  ( -65.32973268749998397, 1379.744446857699813, 273.2270638632589908 ) ) ;
#2048 = CARTESIAN_POINT ( 'NONE',  ( -3.659368786598335088, 1424.416642863884363, 227.7607030046739283 ) ) ;
#2049 = CARTESIAN_POINT ( 'NONE',  ( -29.86461515634905695, 1525.960063244516959, 220.9690070206026178 ) ) ;
#2050 = CARTESIAN_POINT ( 'NONE',  ( -21.46486317390879961, 1504.440058737759955, 215.6677353464210114 ) ) ;
#2051 = CARTESIAN_POINT ( 'NONE',  ( 4.623892060624999800, 1517.066898074209803, 209.8584071487349831 ) ) ;
#2052 = ORIENTED_EDGE ( 'NONE', *, *, #13448, .F. ) ;
#2053 = CARTESIAN_POINT ( 'NONE',  ( 2.500000000000000000, 1432.393161327160215, 157.4962941367979852 ) ) ;
#2054 = CARTESIAN_POINT ( 'NONE',  ( -0.4885209890020000834, 1412.847411980229936, 233.2840911246979942 ) ) ;
#2055 = CARTESIAN_POINT ( 'NONE',  ( -38.48821451509999747, 1384.926710553620069, 239.3141293533589931 ) ) ;
#2056 = ORIENTED_EDGE ( 'NONE', *, *, #95674, .T. ) ;
#2058 = VECTOR ( 'NONE', #84789, 1000.000000000000000 ) ;
#2057 = CARTESIAN_POINT ( 'NONE',  ( 21.84020450211309949, 1523.481610118014487, 234.9798068777342621 ) ) ;
#2059 = CARTESIAN_POINT ( 'NONE',  ( -4.858360392517085735, 1508.551704411667288, 206.6339107026657018 ) ) ;
#2060 = CARTESIAN_POINT ( 'NONE',  ( 11.99823785417749988, 1434.648096261249975, 150.9684152172500262 ) ) ;
#2061 = CARTESIAN_POINT ( 'NONE',  ( 10.31468017153819972, 1478.700932630890065, 232.9778818359829984 ) ) ;
#2062 = TOROIDAL_SURFACE ( 'NONE', #27074, 2.000000000000000000, 1.000000000000000000 ) ;
#2063 = CARTESIAN_POINT ( 'NONE',  ( -24.30765313494389801, 1509.765688098410010, 225.8104982504189877 ) ) ;
#2064 = CARTESIAN_POINT ( 'NONE',  ( -2.445261619629999661, 1408.998450803630021, 187.5560518005979986 ) ) ;
#2065 = DIRECTION ( 'NONE',  ( 0.7067700363771036720, 0.03085824620770448445, -0.7067700363771035610 ) ) ;
#2066 = CARTESIAN_POINT ( 'NONE',  ( 0.06322423967616179474, 1420.447901757230056, 182.6808383609890143 ) ) ;
#2068 = CARTESIAN_POINT ( 'NONE',  ( -3.075414810399999865, 1420.210582609129915, 186.1942670208979962 ) ) ;
#2067 = CARTESIAN_POINT ( 'NONE',  ( 2.487103419534999915, 1516.577434278289957, 215.6681487122470173 ) ) ;
#2069 = CARTESIAN_POINT ( 'NONE',  ( 18.84890159040000057, 1508.241238762730291, 188.4656274554980087 ) ) ;
#2070 = CARTESIAN_POINT ( 'NONE',  ( 18.24053064527407741, 1425.259887461422977, 223.9475156348823646 ) ) ;
#2071 = VERTEX_POINT ( 'NONE', #86573 ) ;
#2072 = CARTESIAN_POINT ( 'NONE',  ( -12.66409680412509964, 1415.935475482089942, 196.4689021216840104 ) ) ;
#2073 = CARTESIAN_POINT ( 'NONE',  ( -19.91074080903786481, 1526.211528530236592, 184.7300577086374460 ) ) ;
#2074 = ORIENTED_EDGE ( 'NONE', *, *, #106146, .T. ) ;
#2075 = AXIS2_PLACEMENT_3D ( 'NONE', #44071, #94439, #26132 ) ;
#2076 = DIRECTION ( 'NONE',  ( 1.755985294532469921E-16, -1.000000000000000000, 1.338183447452831989E-16 ) ) ;
#2077 = CARTESIAN_POINT ( 'NONE',  ( 10.02841049835654275, 1435.644464287910068, 152.4726594247936191 ) ) ;
#2078 = CARTESIAN_POINT ( 'NONE',  ( 7.658720530103260593, 1511.445028088800200, 203.0218979614350019 ) ) ;
#2079 = PRODUCT_DEFINITION_CONTEXT ( 'detailed design', #26278, 'design' ) ;
#2080 = CARTESIAN_POINT ( 'NONE',  ( 2.840612313169999847, 1441.622523712489965, 218.2291133001489811 ) ) ;
#2081 = DIRECTION ( 'NONE',  ( 0.6742693640208961003, 0.000000000000000000, 0.7384854939285241393 ) ) ;
#2082 = CARTESIAN_POINT ( 'NONE',  ( 740.1067050506055693, 11216.44053380570949, 2045.284436369865034 ) ) ;
#2083 = CARTESIAN_POINT ( 'NONE',  ( -2.500000000000000000, 1448.685390522050056, 157.9322779416980040 ) ) ;
#2084 = CARTESIAN_POINT ( 'NONE',  ( 34.18677586421183889, 1524.726013923371283, 198.4504086008744821 ) ) ;
#2085 = CARTESIAN_POINT ( 'NONE',  ( -14.75023390800000023, 1435.013611184930141, 147.9283531795979911 ) ) ;
#2086 = CARTESIAN_POINT ( 'NONE',  ( -5.134146397328430922, 1464.447298219960203, 199.3723941709099847 ) ) ;
#2087 = CARTESIAN_POINT ( 'NONE',  ( 17.61169129089999785, 1418.990866690829989, 192.1965113226980293 ) ) ;
#2089 = LINE ( 'NONE', #96684, #8615 ) ;
#2088 = CARTESIAN_POINT ( 'NONE',  ( 1.138216366218499864, 1409.887084221469877, 232.8382466657240002 ) ) ;
#2090 = CARTESIAN_POINT ( 'NONE',  ( 6.520293444144174444, 1509.032998982614345, 201.8615402263750127 ) ) ;
#2091 = ORIENTED_EDGE ( 'NONE', *, *, #110275, .F. ) ;
#2092 = CARTESIAN_POINT ( 'NONE',  ( 1.468632314148109907, 1507.614846007670167, 186.1949685577550042 ) ) ;
#2093 = CARTESIAN_POINT ( 'NONE',  ( -5399.190729149936487, 50.28429875023819307, -8134.791976861672083 ) ) ;
#2094 = CARTESIAN_POINT ( 'NONE',  ( -24.68077715769999969, 1437.736179642080060, 210.5119845752080039 ) ) ;
#2095 = CARTESIAN_POINT ( 'NONE',  ( -2.205748714679999889, 1484.684221590389825, 198.4976517307989923 ) ) ;
#2096 = CARTESIAN_POINT ( 'NONE',  ( -11.41675697748640061, 1482.775670443970057, 205.7339590229720159 ) ) ;
#2097 = CARTESIAN_POINT ( 'NONE',  ( -3.503594166644271368, 1426.007756115946222, 185.8779573887631216 ) ) ;
#2098 = PRESENTATION_LAYER_ASSIGNMENT (  '', '', ( #75387 ) ) ;
#2099 = CARTESIAN_POINT ( 'NONE',  ( 2.496055909974519427, 1410.375802592201580, 231.6937116688994820 ) ) ;
#2100 = CARTESIAN_POINT ( 'NONE',  ( -3.827327205999999649, 1418.913060387330006, 172.2701767054979882 ) ) ;
#2101 = CARTESIAN_POINT ( 'NONE',  ( -11.28648375916229973, 1489.673514985999873, 212.4366478923779766 ) ) ;
#2102 = CARTESIAN_POINT ( 'NONE',  ( 13.52267151192459949, 1497.923547478540286, 227.8730108396369758 ) ) ;
#2103 = CARTESIAN_POINT ( 'NONE',  ( -101.9385972633359927, 1383.762759256019990, 310.8318512473720148 ) ) ;
#2104 = ADVANCED_FACE ( 'NONE', ( #59734 ), #62997, .F. ) ;
#2105 = EDGE_CURVE ( 'NONE', #33006, #74270, #109360, .T. ) ;
#2106 = CARTESIAN_POINT ( 'NONE',  ( -109.0682903905509988, 1384.413520338990111, 311.2316106067269743 ) ) ;
#2107 = DIRECTION ( 'NONE',  ( -0.000000000000000000, -1.000000000000000000, -0.000000000000000000 ) ) ;
#2108 = CARTESIAN_POINT ( 'NONE',  ( -1.951485868198830076, 1516.530904812869949, 201.4129032351939657 ) ) ;
#2110 = VERTEX_POINT ( 'NONE', #30527 ) ;
#2109 = CARTESIAN_POINT ( 'NONE',  ( 10.56407631929999980, 1452.658139941989930, 209.7432180256290053 ) ) ;
#2111 = CARTESIAN_POINT ( 'NONE',  ( -18.72407526530000155, 1458.246115540929850, 227.3156487912980026 ) ) ;
#2112 = CARTESIAN_POINT ( 'NONE',  ( -85.86261655710001151, 1384.821806127680020, 289.6800030968590249 ) ) ;
#2113 = CARTESIAN_POINT ( 'NONE',  ( 20.55900035540929949, 1509.660753117409968, 230.5261133655430115 ) ) ;
#2114 = VERTEX_POINT ( 'NONE', #98835 ) ;
#2115 = ORIENTED_EDGE ( 'NONE', *, *, #100899, .T. ) ;
#2116 = EDGE_CURVE ( 'NONE', #42951, #41116, #80771, .T. ) ;
#2117 = CARTESIAN_POINT ( 'NONE',  ( -10.96946876072200006, 1432.347663854339999, 151.7701362700559855 ) ) ;
#2118 = CARTESIAN_POINT ( 'NONE',  ( 13.41954733660536370, 1443.449734802816920, 169.3662105687162978 ) ) ;
#2120 = CARTESIAN_POINT ( 'NONE',  ( -41.23304476799999918, 1446.065281864440067, 261.5842295713979979 ) ) ;
#2119 = CARTESIAN_POINT ( 'NONE',  ( 21.41971086555086501, 1512.187213306747481, 185.1638823089577670 ) ) ;
#2121 = CARTESIAN_POINT ( 'NONE',  ( 9.001848782638129265, 1436.441033338579928, 209.9342506180670114 ) ) ;
#2122 = CARTESIAN_POINT ( 'NONE',  ( -109.9959328080000063, 1384.355667310579975, 296.9977477969590041 ) ) ;
#2123 = B_SPLINE_CURVE_WITH_KNOTS ( 'NONE', 3,
 ( #81265, #28680, #62313, #72353, #98073, #87493, #29768, #54460, #72890, #4581, #38715, #19714, #88598, #29229 ),
 .UNSPECIFIED., .F., .F.,
 ( 4, 2, 2, 2, 2, 2, 4 ),
 ( 0.000000000000000000, 0.001128757102284214499, 0.002257514204568428998, 0.002821892755710748643, 0.003386271306853069155, 0.003950649857995389667, 0.004515028409137709746 ),
 .UNSPECIFIED. ) ;
#2124 = CIRCLE ( 'NONE', #91458, 1.999999999999942935 ) ;
#2125 = CARTESIAN_POINT ( 'NONE',  ( 25.23662664879999795, 1509.794342810929948, 195.3591958783979976 ) ) ;
#2126 = CARTESIAN_POINT ( 'NONE',  ( -19.90114970400000161, 1485.011347091429798, 190.9790800808980009 ) ) ;
#2127 = CARTESIAN_POINT ( 'NONE',  ( -1.693092047772239983, 1443.235800395060096, 218.9922115469449864 ) ) ;
#2128 = CARTESIAN_POINT ( 'NONE',  ( 5.557914828519999517, 1420.826195899929871, 186.0956685246979987 ) ) ;
#2129 = CARTESIAN_POINT ( 'NONE',  ( -9.548319411750000540, 1438.548742442639877, 152.9855554426980007 ) ) ;
#2130 = CARTESIAN_POINT ( 'NONE',  ( -9.184076889506968655, 1450.489465732099916, 208.2759141665609945 ) ) ;
#2131 = CARTESIAN_POINT ( 'NONE',  ( -9.418568788532940772, 1424.364165527140131, 204.6686179336989824 ) ) ;
#2132 = CARTESIAN_POINT ( 'NONE',  ( -19.71294296389999801, 1452.081684968429954, 145.2800229328979924 ) ) ;
#2133 = DIRECTION ( 'NONE',  ( 0.9942586961433768078, -1.225281874271768203E-16, 0.1070030146457215670 ) ) ;
#2134 = ORIENTED_EDGE ( 'NONE', *, *, #30820, .F. ) ;
#2135 = CARTESIAN_POINT ( 'NONE',  ( -3.176056732109739933, 1508.610720109290014, 213.8016369874950158 ) ) ;
#2136 = CARTESIAN_POINT ( 'NONE',  ( 16.44572865500000347, 1495.267817486490003, 192.9050346917990169 ) ) ;
#2138 = EDGE_CURVE ( 'NONE', #104484, #77864, #77374, .T. ) ;
#2137 = CARTESIAN_POINT ( 'NONE',  ( -44.56544972020000728, 1444.219545419719907, 269.9128112642979431 ) ) ;
#2139 = CARTESIAN_POINT ( 'NONE',  ( -23.75705825515298031, 1436.072652686797028, 211.7065605907733357 ) ) ;
#2140 = CARTESIAN_POINT ( 'NONE',  ( 17.54329103400000278, 1410.021606951229842, 223.3339101244980043 ) ) ;
#2141 = CARTESIAN_POINT ( 'NONE',  ( -14.05027195639999960, 1463.289392627530106, 223.4969360966980219 ) ) ;
#2142 = AXIS2_PLACEMENT_3D ( 'NONE', #10875, #61851, #26549 ) ;
#2143 = CARTESIAN_POINT ( 'NONE',  ( 4.329407853939748918, 1515.066355634550064, 210.8164016152200020 ) ) ;
#2144 = CARTESIAN_POINT ( 'NONE',  ( 2.852115976134160125, 1409.175191729200151, 230.8570650992599838 ) ) ;
#2145 = CARTESIAN_POINT ( 'NONE',  ( 2.173985094599999890, 1508.988976439630051, 238.5378654763979966 ) ) ;
#2146 = CARTESIAN_POINT ( 'NONE',  ( -7.617228954449999812, 1417.322863989330017, 231.1379649406979979 ) ) ;
#2147 = EDGE_CURVE ( 'NONE', #10764, #80757, #107327, .T. ) ;
#2148 =( BOUNDED_CURVE ( )  B_SPLINE_CURVE ( 3, ( #59261, #8266, #50841, #58699 ),
 .UNSPECIFIED., .F., .T. ) 
 B_SPLINE_CURVE_WITH_KNOTS ( ( 4, 4 ),
 ( 0.000000000000000000, 0.7048113239778038830 ),
 .UNSPECIFIED. ) 
 CURVE ( )  GEOMETRIC_REPRESENTATION_ITEM ( )  RATIONAL_B_SPLINE_CURVE ( ( 1.000000000000000000, 0.9590300661663093695, 0.9590300661663093695, 1.000000000000000000 ) ) 
 REPRESENTATION_ITEM ( '' )  );
#2149 = CARTESIAN_POINT ( 'NONE',  ( -1.435153818974767237, 1484.396021952602950, 182.4491198709524724 ) ) ;
#2150 = CARTESIAN_POINT ( 'NONE',  ( 9.444074105595053226, 1360.911098639617876, 208.3718459617010978 ) ) ;
#2151 = CARTESIAN_POINT ( 'NONE',  ( -45.64771259127410019, 1435.560685441120086, 266.9890804707069378 ) ) ;
#2152 = CARTESIAN_POINT ( 'NONE',  ( -76.99707197885047094, 1526.382868172863937, 398.8876973329340672 ) ) ;
#2153 = ORIENTED_EDGE ( 'NONE', *, *, #64701, .T. ) ;
#2154 = CARTESIAN_POINT ( 'NONE',  ( 24.40199393649999848, 1435.349635217629839, 136.1409814179979776 ) ) ;
#2155 = EDGE_CURVE ( 'NONE', #105726, #27470, #27209, .T. ) ;
#2156 = ORIENTED_EDGE ( 'NONE', *, *, #106868, .F. ) ;
#2157 = CARTESIAN_POINT ( 'NONE',  ( -1.122033430074999893, 1516.972341476009888, 209.8777854684929878 ) ) ;
#2158 = CARTESIAN_POINT ( 'NONE',  ( -4.026786250540000722, 1422.913060387330006, 172.2701767054979882 ) ) ;
#2159 = CARTESIAN_POINT ( 'NONE',  ( -21.92443624460000251, 1509.678678571630144, 190.3581774935979922 ) ) ;
#2160 = FACE_OUTER_BOUND ( 'NONE', #37349, .T. ) ;
#2161 = VECTOR ( 'NONE', #110428, 1000.000000000000114 ) ;
#2162 = CARTESIAN_POINT ( 'NONE',  ( -3.703568358935259930, 1497.311626042180023, 220.9591690318370070 ) ) ;
#2163 = ORIENTED_EDGE ( 'NONE', *, *, #35189, .T. ) ;
#2164 = CARTESIAN_POINT ( 'NONE',  ( -17.38127759599958466, 1410.742336404525759, 225.7780505793990926 ) ) ;
#2166 = CARTESIAN_POINT ( 'NONE',  ( -28.27139721233049485, 1526.382868172864164, 198.6830693683576499 ) ) ;
#2165 = CARTESIAN_POINT ( 'NONE',  ( 0.5697990016583959205, 1450.893162567740092, 181.2939912002310052 ) ) ;
#2167 = CIRCLE ( 'NONE', #36115, 1.999999999999998668 ) ;
#2168 = CARTESIAN_POINT ( 'NONE',  ( 5.350728454891725328, 1427.748570762830695, 215.4189187839067188 ) ) ;
#2169 = CARTESIAN_POINT ( 'NONE',  ( -17.00038391736149990, 1508.541898703860170, 212.8847129985989852 ) ) ;
#2170 = CARTESIAN_POINT ( 'NONE',  ( 9.211869141260001115, 1471.980260610790083, 214.4234941383089961 ) ) ;
#2171 = FACE_OUTER_BOUND ( 'NONE', #70001, .T. ) ;
#2172 = ORIENTED_EDGE ( 'NONE', *, *, #97884, .T. ) ;
#2173 = CARTESIAN_POINT ( 'NONE',  ( -12.95209671980339827, 1411.808719174920043, 269.3556024724110216 ) ) ;
#2174 = CARTESIAN_POINT ( 'NONE',  ( 6.938478784765000462, 1516.719999691880048, 208.3679751968140010 ) ) ;
#2175 = FACE_OUTER_BOUND ( 'NONE', #89613, .T. ) ;
#2176 = CARTESIAN_POINT ( 'NONE',  ( 8.468745670032260975, 1436.332250083529971, 207.5732686620520155 ) ) ;
#2178 = ORIENTED_EDGE ( 'NONE', *, *, #38568, .F. ) ;
#2177 = CARTESIAN_POINT ( 'NONE',  ( -5.236338392966255917, 1368.774323667083991, 210.6218459616987957 ) ) ;
#2179 = ORIENTED_EDGE ( 'NONE', *, *, #106940, .T. ) ;
#2180 = CARTESIAN_POINT ( 'NONE',  ( -23.51878303699330175, 1410.727184521670097, 210.4338679270009891 ) ) ;
#2181 = CARTESIAN_POINT ( 'NONE',  ( -4.526843557140001195, 1425.874817585629899, 186.1888505123980053 ) ) ;
#2182 = FACE_BOUND ( 'NONE', #61413, .T. ) ;
#2183 = CARTESIAN_POINT ( 'NONE',  ( -3.818068226668779541, 1406.099103250517146, 266.9557811492330757 ) ) ;
#2184 = CARTESIAN_POINT ( 'NONE',  ( 6.541070334811199594, 1517.051704644130041, 212.7912326336579838 ) ) ;
#2185 = CARTESIAN_POINT ( 'NONE',  ( -20.42021094099999701, 1430.789239710730044, 222.0598896059980234 ) ) ;
#2186 = PRODUCT_RELATED_PRODUCT_CATEGORY ( 'part', '', ( #82225 ) ) ;
#2187 = CARTESIAN_POINT ( 'NONE',  ( 5.341374517573029834, 1476.050173402869859, 268.4837847659439944 ) ) ;
#2188 = B_SPLINE_CURVE_WITH_KNOTS ( 'NONE', 5,
 ( #32849, #39617, #23350, #75442, #7114, #75969 ),
 .UNSPECIFIED., .F., .F.,
 ( 6, 6 ),
 ( 0.000000000000000000, 1.000000000000000000 ),
 .UNSPECIFIED. ) ;
#2189 = CARTESIAN_POINT ( 'NONE',  ( -13.34651281871636286, 1462.782296786469715, 230.3199898465639990 ) ) ;
#2190 = CARTESIAN_POINT ( 'NONE',  ( 10.26047870550000063, 1446.726006776589884, 186.8445627053979763 ) ) ;
#2191 = CARTESIAN_POINT ( 'NONE',  ( -7.336844680545000053, 1517.106845464700200, 205.6683011064770312 ) ) ;
#2192 = ORIENTED_EDGE ( 'NONE', *, *, #46877, .T. ) ;
#2193 = CARTESIAN_POINT ( 'NONE',  ( 24.08426297012860218, 1411.115209414830133, 209.6325633951909708 ) ) ;
#2194 = CARTESIAN_POINT ( 'NONE',  ( 1.475845351969280017, 1481.308154728749969, 182.2386903793839963 ) ) ;
#2195 = VERTEX_POINT ( 'NONE', #5887 ) ;
#2196 = CARTESIAN_POINT ( 'NONE',  ( 3.224549562455929941, 1508.551704408489968, 204.2884091523009999 ) ) ;
#2197 = CARTESIAN_POINT ( 'NONE',  ( 25.37084254212440371, 1451.310454143999777, 137.0122259544509973 ) ) ;
#2198 = CARTESIAN_POINT ( 'NONE',  ( 13.79555462530000121, 1416.822690122329959, 196.3351664771980154 ) ) ;
#2199 = CARTESIAN_POINT ( 'NONE',  ( -24.70417392370000087, 1389.604960788569997, 206.5185001640990095 ) ) ;
#2200 = CARTESIAN_POINT ( 'NONE',  ( -18.65749898563134579, 1509.387464492826666, 230.8014192534890014 ) ) ;
#2201 = CARTESIAN_POINT ( 'NONE',  ( 19.05936272150000121, 1410.940464818530018, 195.3780893796979967 ) ) ;
#2202 = CARTESIAN_POINT ( 'NONE',  ( -3.983585865099999790, 1497.196993069489963, 198.5852023898990240 ) ) ;
#2203 = CARTESIAN_POINT ( 'NONE',  ( 2.903677228125761900, 1439.669927704568863, 183.9752002117523091 ) ) ;
#2205 = CARTESIAN_POINT ( 'NONE',  ( -18.63621073208100398, 1424.448676634511685, 224.8155311996966930 ) ) ;
#2204 = CARTESIAN_POINT ( 'NONE',  ( 0.7916551353930000312, 1417.386977067530097, 235.1101550285980011 ) ) ;
#2206 = CARTESIAN_POINT ( 'NONE',  ( 0.8296033197978609497, 1451.436690953809830, 182.8542985698300072 ) ) ;
#2207 = ADVANCED_FACE ( 'NONE', ( #57418 ), #23769, .T. ) ;
#2208 = CARTESIAN_POINT ( 'NONE',  ( 12.26870259150531872, 1428.415420825756428, 194.9349402552377057 ) ) ;
#2209 = EDGE_CURVE ( 'NONE', #26627, #53103, #57965, .T. ) ;
#2210 = CARTESIAN_POINT ( 'NONE',  ( -6.549762485114999144, 1516.729202374750002, 213.7405950387170037 ) ) ;
#2211 = CARTESIAN_POINT ( 'NONE',  ( -4.329791528864999961, 1515.051704408389924, 212.4519801359869859 ) ) ;
#2212 = EDGE_LOOP ( 'NONE', ( #89470, #53230, #10682, #27900 ) ) ;
#2213 = CARTESIAN_POINT ( 'NONE',  ( -16.84534104709999980, 1417.257337058139910, 207.1240090553390019 ) ) ;
#2214 = FACE_OUTER_BOUND ( 'NONE', #35175, .T. ) ;
#2215 = CARTESIAN_POINT ( 'NONE',  ( -6.267272736393399768, 1484.683887506470001, 198.9978965073320012 ) ) ;
#2216 = CARTESIAN_POINT ( 'NONE',  ( -20.75777115397048433, 1507.865918544692931, 209.5048640109985172 ) ) ;
#2217 = CARTESIAN_POINT ( 'NONE',  ( -34.75239981097760023, 1450.355854787910175, 136.2303794071760024 ) ) ;
#2218 = CARTESIAN_POINT ( 'NONE',  ( -4.327148319164989765, 1515.152643786279896, 208.8010119524350046 ) ) ;
#2219 = AXIS2_PLACEMENT_3D ( 'NONE', #101752, #25040, #67643 ) ;
#2220 = CARTESIAN_POINT ( 'NONE',  ( -13.21926163380000041, 1460.466222979229997, 248.0989693022980020 ) ) ;
#2221 = ADVANCED_FACE ( 'NONE', ( #43767 ), #11279, .F. ) ;
#2222 = CARTESIAN_POINT ( 'NONE',  ( 44.66359154829995504, 1448.409698723047768, 266.2173270182975671 ) ) ;
#2223 = CARTESIAN_POINT ( 'NONE',  ( 10.98204826459999950, 1433.094938567290001, 151.7693906807980113 ) ) ;
#2224 = CARTESIAN_POINT ( 'NONE',  ( -32.54472331756920767, 1464.064700655210117, 269.9033746748029898 ) ) ;
#2225 = CARTESIAN_POINT ( 'NONE',  ( -9.613516620566301185, 1460.231789534549989, 209.9813920803319718 ) ) ;
#2226 = CARTESIAN_POINT ( 'NONE',  ( -9.292082803063870244, 1422.258564872340003, 192.2454125014830026 ) ) ;
#2227 = ORIENTED_EDGE ( 'NONE', *, *, #30453, .T. ) ;
#2228 = CARTESIAN_POINT ( 'NONE',  ( 6.499999980935001531, 1516.051704408390151, 209.1218459511669892 ) ) ;
#2229 = CARTESIAN_POINT ( 'NONE',  ( 25.00977876991279913, 1436.598012848749931, 137.9330263815630246 ) ) ;
#2230 = CARTESIAN_POINT ( 'NONE',  ( -12.27295469420000096, 1486.509335314930013, 184.4397015064979826 ) ) ;
#2231 = CARTESIAN_POINT ( 'NONE',  ( -0.7790227543749990158, 1442.687262046989872, 200.2740145245590213 ) ) ;
#2232 = CARTESIAN_POINT ( 'NONE',  ( -20.11385680769999951, 1487.601373209189887, 204.1067431612489997 ) ) ;
#2233 = EDGE_CURVE ( 'NONE', #93915, #86873, #79381, .T. ) ;
#2234 = AXIS2_PLACEMENT_3D ( 'NONE', #36746, #10997, #20467 ) ;
#2235 = CARTESIAN_POINT ( 'NONE',  ( 24.75581127549999749, 1430.360917243230006, 210.2728189765479954 ) ) ;
#2236 = DIRECTION ( 'NONE',  ( 0.000000000000000000, 0.000000000000000000, 1.000000000000000000 ) ) ;
#2237 = CARTESIAN_POINT ( 'NONE',  ( 8.454790733525280544, 1428.363638633589972, 213.4109935021670026 ) ) ;
#2238 = CARTESIAN_POINT ( 'NONE',  ( -35.56111957166950077, 1383.834697306850103, 234.6955540351449940 ) ) ;
#2239 = EDGE_CURVE ( 'NONE', #10343, #12135, #19253, .T. ) ;
#2240 = FACE_OUTER_BOUND ( 'NONE', #51460, .T. ) ;
#2241 = DIRECTION ( 'NONE',  ( -5.980589973904019347E-17, 1.000000000000000000, -1.736889445713099699E-16 ) ) ;
#2242 = B_SPLINE_CURVE_WITH_KNOTS ( 'NONE', 3,
 ( #64901, #20109, #29611, #46449 ),
 .UNSPECIFIED., .F., .F.,
 ( 4, 4 ),
 ( 0.000000000000000000, 1.000000000000000000 ),
 .UNSPECIFIED. ) ;
#2243 = CARTESIAN_POINT ( 'NONE',  ( 234.5897387251999930, 11221.53578756869865, -1757.702084499889907 ) ) ;
#2244 = CARTESIAN_POINT ( 'NONE',  ( 0.1678350090582330090, 1481.603268379459905, 182.0255188484140092 ) ) ;
#2245 = EDGE_CURVE ( 'NONE', #101350, #84627, #84705, .T. ) ;
#2247 = EDGE_LOOP ( 'NONE', ( #62076, #91279, #55048, #2892, #99074, #45713, #80231, #44012, #64267 ) ) ;
#2246 = FACE_OUTER_BOUND ( 'NONE', #26866, .T. ) ;
#2248 = CARTESIAN_POINT ( 'NONE',  ( -105.0581303879369983, 1379.236400313860031, 304.0328620142400382 ) ) ;
#2249 = CARTESIAN_POINT ( 'NONE',  ( -8.296934851823509760, 1386.806139525614526, 199.8388016180733473 ) ) ;
#2250 = CARTESIAN_POINT ( 'NONE',  ( -5.375553179505209833, 1441.026369770150040, 154.8319413312549955 ) ) ;
#2252 = ORIENTED_EDGE ( 'NONE', *, *, #54613, .T. ) ;
#2251 = CARTESIAN_POINT ( 'NONE',  ( -32.09337683451324352, 1524.374578187333555, 216.7020508011439972 ) ) ;
#2253 = CARTESIAN_POINT ( 'NONE',  ( -9.104767224130160486, 1421.478911732549932, 192.1853015429209961 ) ) ;
#2254 = ORIENTED_EDGE ( 'NONE', *, *, #36492, .F. ) ;
#2255 = CARTESIAN_POINT ( 'NONE',  ( -12.31958819330829868, 1391.699967522870111, 210.6753496357469828 ) ) ;
#2256 = CARTESIAN_POINT ( 'NONE',  ( -17.84204423069999734, 1415.932840167130053, 209.4661914366780024 ) ) ;
#2257 = CARTESIAN_POINT ( 'NONE',  ( -5.524058921557154278, 1509.111545497368979, 238.0554591568478031 ) ) ;
#2259 = ADVANCED_FACE ( 'NONE', ( #50931 ), #6146, .T. ) ;
#2258 = CARTESIAN_POINT ( 'NONE',  ( -2.928726385117801367, 1368.451830327553807, 207.8117072160285090 ) ) ;
#2260 = CARTESIAN_POINT ( 'NONE',  ( -2.854504612459999979, 1433.072736100190014, 218.2391856586490064 ) ) ;
#2261 = CARTESIAN_POINT ( 'NONE',  ( -10.39285233026310173, 1472.009416248819889, 207.0409344721679759 ) ) ;
#2262 = CARTESIAN_POINT ( 'NONE',  ( 13.71176819436150041, 1409.391885883779878, 203.1931630247410112 ) ) ;
#2263 = CARTESIAN_POINT ( 'NONE',  ( -7.966114795899199130, 1384.917223774180002, 199.4892816035240060 ) ) ;
#2264 = CARTESIAN_POINT ( 'NONE',  ( -102.2538918586309933, 1385.226474943340008, 296.6373044331759843 ) ) ;
#2265 = CARTESIAN_POINT ( 'NONE',  ( -17.91583404220000020, 1424.173795738829995, 192.2475373850980134 ) ) ;
#2266 = CARTESIAN_POINT ( 'NONE',  ( 10.14173938847820189, 1422.829424262219845, 209.7691254332700055 ) ) ;
#2267 = ORIENTED_EDGE ( 'NONE', *, *, #90513, .T. ) ;
#2268 = EDGE_CURVE ( 'NONE', #106220, #56418, #68854, .T. ) ;
#2269 = CARTESIAN_POINT ( 'NONE',  ( 10.95672069168569962, 1490.579439969769965, 207.2253856564389878 ) ) ;
#2271 = VERTEX_POINT ( 'NONE', #94565 ) ;
#2270 = FACE_OUTER_BOUND ( 'NONE', #4358, .T. ) ;
#2272 = ORIENTED_EDGE ( 'NONE', *, *, #46910, .F. ) ;
#2273 = CARTESIAN_POINT ( 'NONE',  ( 25.84050225520000055, 1509.815430613229864, 221.3404165686980036 ) ) ;
#2274 = CARTESIAN_POINT ( 'NONE',  ( -5.675785208868349585, 1362.218944691939669, 207.6218459616988241 ) ) ;
#2275 = CARTESIAN_POINT ( 'NONE',  ( -12.00426221419999884, 1433.697247254759986, 150.2718049272980068 ) ) ;
#2276 = CARTESIAN_POINT ( 'NONE',  ( 29.51415436607676313, 1509.963328502264176, 211.7137289823847652 ) ) ;
#2277 = CARTESIAN_POINT ( 'NONE',  ( 12.32624855160359978, 1427.184147377119871, 207.2003428294259777 ) ) ;
#2278 = CARTESIAN_POINT ( 'NONE',  ( 2.349396271509999856, 1396.056274664130115, 220.6130876232980143 ) ) ;
#2279 = CARTESIAN_POINT ( 'NONE',  ( 32.09337683451773415, 1524.374578187332645, 201.5416411222501267 ) ) ;
#2280 = CARTESIAN_POINT ( 'NONE',  ( 19.52793876076239954, 1443.814291013210095, 209.3879297421120214 ) ) ;
#2281 = FACE_OUTER_BOUND ( 'NONE', #55547, .T. ) ;
#2282 = CARTESIAN_POINT ( 'NONE',  ( -8.284884219063519240, 1369.613879705106001, 208.3718459617010978 ) ) ;
#2283 = CARTESIAN_POINT ( 'NONE',  ( -26.66311519709438116, 1436.746818294333934, 136.7889187690164761 ) ) ;
#2284 = EDGE_CURVE ( 'NONE', #99393, #77212, #39309, .T. ) ;
#2285 = CARTESIAN_POINT ( 'NONE',  ( -5.013274999515000552, 1517.068517094990057, 206.8347616620369820 ) ) ;
#2286 = CARTESIAN_POINT ( 'NONE',  ( -13.13860279428170053, 1434.935977728519902, 149.7031307944440073 ) ) ;
#2287 = CARTESIAN_POINT ( 'NONE',  ( 9.061759573819999858, 1423.804867913830094, 133.5337813787979826 ) ) ;
#2288 = CARTESIAN_POINT ( 'NONE',  ( 0.9541163229580019722, 1497.352948200390074, 197.4851080636989877 ) ) ;
#2289 = CARTESIAN_POINT ( 'NONE',  ( -2.432658854300000062, 1495.143052030289937, 220.0417648853990045 ) ) ;
#2290 = EDGE_CURVE ( 'NONE', #6066, #15508, #7175, .T. ) ;
#2291 = CARTESIAN_POINT ( 'NONE',  ( -106.6038969349999945, 1381.976044154610008, 298.3535665123590093 ) ) ;
#2292 = EDGE_LOOP ( 'NONE', ( #38318, #90683, #29383, #41414 ) ) ;
#2293 = DIRECTION ( 'NONE',  ( -9.152776640618289361E-47, 1.000000000000000000, -1.836970198721029688E-16 ) ) ;
#2294 = CARTESIAN_POINT ( 'NONE',  ( -26.12765557870000066, 1469.244184481629873, 206.5858184781079956 ) ) ;
#2296 = CARTESIAN_POINT ( 'NONE',  ( 16.24908062485310012, 1409.480479830250033, 193.1391318611629799 ) ) ;
#2295 = CARTESIAN_POINT ( 'NONE',  ( -10.68704931835589989, 1425.705646839379824, 93.54238571512179590 ) ) ;
#2297 = CARTESIAN_POINT ( 'NONE',  ( -3.445685115514999897, 1516.778761582560037, 211.6139765934069885 ) ) ;
#2298 = CARTESIAN_POINT ( 'NONE',  ( 0.4003602064798469917, 1395.927041273810119, 198.1267992979170174 ) ) ;
#2299 = DIRECTION ( 'NONE',  ( -1.755985294532469921E-16, 1.000000000000000000, -1.338183447452831989E-16 ) ) ;
#2300 = CARTESIAN_POINT ( 'NONE',  ( -28.33103133930000084, 1431.247806717810136, 240.1819618842980049 ) ) ;
#2301 = DIRECTION ( 'NONE',  ( -1.755985294532469921E-16, 1.000000000000000000, -1.338183447452831989E-16 ) ) ;
#2302 = CARTESIAN_POINT ( 'NONE',  ( 29.03159036030189810, 1509.651961614089942, 209.5599309260780103 ) ) ;
#2303 = CARTESIAN_POINT ( 'NONE',  ( -5.292247061280000331, 1391.913060387289988, 214.4361776263990009 ) ) ;
#2304 = CARTESIAN_POINT ( 'NONE',  ( -24.02849098739518041, 1410.733038014311205, 208.6273191338911772 ) ) ;
#2305 = ORIENTED_EDGE ( 'NONE', *, *, #6899, .F. ) ;
#2306 = CARTESIAN_POINT ( 'NONE',  ( 6.225972109890000716, 1494.795958560490135, 219.7811165620990153 ) ) ;
#2307 = CARTESIAN_POINT ( 'NONE',  ( 14.86633461655332233, 1514.624327954312776, 225.3233414037949842 ) ) ;
#2308 = CARTESIAN_POINT ( 'NONE',  ( -16.12485330519999849, 1459.081998215830026, 229.9878740626980118 ) ) ;
#2309 = ORIENTED_EDGE ( 'NONE', *, *, #87057, .F. ) ;
#2310 = VERTEX_POINT ( 'NONE', #53149 ) ;
#2311 = CARTESIAN_POINT ( 'NONE',  ( 8.784510176764259270, 1452.237572000909950, 212.1743866200270077 ) ) ;
#2312 = CARTESIAN_POINT ( 'NONE',  ( -9.330551624163069491, 1426.784211110280012, 151.9956449679999935 ) ) ;
#2313 = VERTEX_POINT ( 'NONE', #78901 ) ;
#2314 = CARTESIAN_POINT ( 'NONE',  ( 0.1022255644269999819, 1415.641329274630152, 184.7537210817980338 ) ) ;
#2315 = CARTESIAN_POINT ( 'NONE',  ( 9.883113931189466683, 1446.592767805756466, 153.4333270483208196 ) ) ;
#2316 = CARTESIAN_POINT ( 'NONE',  ( 17.22592475670000312, 1443.913060387330006, 162.9227486557980171 ) ) ;
#2317 = FACE_OUTER_BOUND ( 'NONE', #41238, .T. ) ;
#2318 = ADVANCED_FACE ( 'NONE', ( #87286 ), #107382, .F. ) ;
#2319 = CARTESIAN_POINT ( 'NONE',  ( 1.211738532285810077, 1420.845824148819929, 182.9724934397759739 ) ) ;
#2320 =( LENGTH_UNIT ( ) NAMED_UNIT ( * ) SI_UNIT ( .MILLI., .METRE. ) );
#2321 = CARTESIAN_POINT ( 'NONE',  ( -12.25307189289999954, 1391.743053431310045, 210.3744810088190036 ) ) ;
#2322 = CARTESIAN_POINT ( 'NONE',  ( 0.04809667444139999887, 1420.202366602630036, 183.9005171462980002 ) ) ;
#2323 = EDGE_LOOP ( 'NONE', ( #105995, #70389, #91707, #39981 ) ) ;
#2324 = CARTESIAN_POINT ( 'NONE',  ( -1.130607502004999931, 1516.632821972880038, 202.5736453444569918 ) ) ;
#2325 = CARTESIAN_POINT ( 'NONE',  ( -3.253301419385000504, 1516.790374942449944, 210.2573062871869922 ) ) ;
#2326 = ORIENTED_EDGE ( 'NONE', *, *, #108860, .T. ) ;
#2327 = CARTESIAN_POINT ( 'NONE',  ( 11.86603321975120018, 1432.331321816350055, 149.9824224880240138 ) ) ;
#2328 = CARTESIAN_POINT ( 'NONE',  ( 13.30719000516407391, 1444.579980391261415, 187.5321241343243059 ) ) ;
#2329 = ORIENTED_EDGE ( 'NONE', *, *, #108317, .F. ) ;
#2330 = CARTESIAN_POINT ( 'NONE',  ( -2.188078410709979771, 1508.020976590390092, 220.9453026643990086 ) ) ;
#2331 = CARTESIAN_POINT ( 'NONE',  ( -13.31970894439942832, 1443.086052842850449, 169.4013815678669346 ) ) ;
#2332 = CARTESIAN_POINT ( 'NONE',  ( 5.138925822920000108, 1509.092515631430160, 237.3859384438979987 ) ) ;
#2333 = CARTESIAN_POINT ( 'NONE',  ( -9.105445285308739756, 1471.726587830969947, 213.6544575909670129 ) ) ;
#2334 = CARTESIAN_POINT ( 'NONE',  ( -5.656371325420000318, 1421.415623769629747, 186.5737237497980061 ) ) ;
#2335 = CARTESIAN_POINT ( 'NONE',  ( 4.903601556030229958, 1409.407506479329868, 270.3706464830609661 ) ) ;
#2336 = CARTESIAN_POINT ( 'NONE',  ( 9.221676543900459322, 1450.699204871009897, 209.5818517409399817 ) ) ;
#2337 = CARTESIAN_POINT ( 'NONE',  ( -6.917540847650000657, 1474.438802919490172, 201.2803177021589818 ) ) ;
#2338 = CARTESIAN_POINT ( 'NONE',  ( 9.489398001770000590, 1491.701139852389815, 214.8220554479490261 ) ) ;
#2339 = CARTESIAN_POINT ( 'NONE',  ( -44.27735363219999698, 1379.663868217249956, 229.4728106293590031 ) ) ;
#2340 = CARTESIAN_POINT ( 'NONE',  ( 8.556778216962817041, 1424.669736104401181, 195.7159935075917474 ) ) ;
#2342 = CARTESIAN_POINT ( 'NONE',  ( -2.500000000000000000, 1426.966631815929986, 170.4008037693979816 ) ) ;
#2341 = CARTESIAN_POINT ( 'NONE',  ( -20.26886524579999715, 1505.341425002289952, 209.1373927737770089 ) ) ;
#2343 = CARTESIAN_POINT ( 'NONE',  ( -67.15060528499047621, 1379.747519056922101, 278.1647121854331886 ) ) ;
#2344 = EDGE_CURVE ( 'NONE', #57510, #28393, #37987, .T. ) ;
#2345 = CARTESIAN_POINT ( 'NONE',  ( 17.88485182696830122, 1419.918979540250120, 225.0707500705920268 ) ) ;
#2346 = CARTESIAN_POINT ( 'NONE',  ( -7.779264728704999854, 1514.199187793449937, 202.4059200890270063 ) ) ;
#2347 = ORIENTED_EDGE ( 'NONE', *, *, #88292, .T. ) ;
#2348 = CARTESIAN_POINT ( 'NONE',  ( 22.74199304079999706, 1435.511682894840078, 234.3916895645979821 ) ) ;
#2349 = CARTESIAN_POINT ( 'NONE',  ( 13.67952642077979952, 1434.971887304759775, 148.6457544281230128 ) ) ;
#2350 = CARTESIAN_POINT ( 'NONE',  ( -67.08107980928619440, 1385.034953735319959, 291.5504916563910456 ) ) ;
#2351 = CARTESIAN_POINT ( 'NONE',  ( -18.88880210473032761, 1524.667648926078527, 179.4140113511354855 ) ) ;
#2352 = CARTESIAN_POINT ( 'NONE',  ( -8.970890765399998301, 1384.951408361539961, 199.9338804842589923 ) ) ;
#2353 = CARTESIAN_POINT ( 'NONE',  ( 39.86227344171260256, 1422.528661024590292, 269.1410521188619782 ) ) ;
#2354 =( BOUNDED_SURFACE ( )  B_SPLINE_SURFACE ( 3, 2, ( 
 ( #65120, #13571, #21961 ),
 ( #48879, #74620, #64030 ),
 ( #48321, #30945, #98144 ),
 ( #4651, #30392, #5760 ),
 ( #38243, #99231, #22509 ),
 ( #56711, #90846, #14131 ),
 ( #99787, #64582, #107103 ),
 ( #98702, #90290, #47211 ),
 ( #5194, #23078, #55630 ),
 ( #15224, #4118, #39901 ) ),
 .UNSPECIFIED., .F., .F., .T. ) 
 B_SPLINE_SURFACE_WITH_KNOTS ( ( 4, 2, 2, 2, 4 ),
 ( 3, 3 ),
 ( 1.570796326794896558, 1.963495408493620697, 2.356194490192344837, 2.748893571891068976, 3.141592653589793116 ),
 ( 0.000000000000000000, 1.000000000000000000 ),
 .UNSPECIFIED. ) 
 GEOMETRIC_REPRESENTATION_ITEM ( )  RATIONAL_B_SPLINE_SURFACE ( (
 ( 1.000000000000000000, 0.7071067811865862085, 1.000000000000000000),
 ( 1.000000000000000000, 0.7166207884822426433, 1.000000000000000000),
 ( 1.000000000000000000, 0.7259222650906650420, 1.000000000000000000),
 ( 1.000000000000000000, 0.7428408967930791862, 1.000000000000000000),
 ( 1.000000000000000000, 0.7504512394528564112, 1.000000000000000000),
 ( 1.000000000000000000, 0.7630177051946440692, 1.000000000000000000),
 ( 1.000000000000000000, 0.7679730451973161287, 1.000000000000000000),
 ( 1.000000000000000000, 0.7746454561797309069, 1.000000000000000000),
 ( 1.000000000000000000, 0.7763684247035169683, 1.000000000000000000),
 ( 1.000000000000000000, 0.7763623250684379418, 1.000000000000000000) ) ) 
 REPRESENTATION_ITEM ( '' )  SURFACE ( )  );
#2356 = ORIENTED_EDGE ( 'NONE', *, *, #32389, .T. ) ;
#2355 = CARTESIAN_POINT ( 'NONE',  ( -1.480922050758809894, 1515.075000927520023, 204.7926644938669938 ) ) ;
#2357 = CARTESIAN_POINT ( 'NONE',  ( -15.87953847626955373, 1415.948856948393768, 209.7347139027639287 ) ) ;
#2358 = CARTESIAN_POINT ( 'NONE',  ( -24.15641795129999991, 1444.538778010680062, 211.4627077540479831 ) ) ;
#2359 = EDGE_CURVE ( 'NONE', #5115, #10547, #107935, .T. ) ;
#2360 = CARTESIAN_POINT ( 'NONE',  ( -2.332679820760331424, 1449.698752274461867, 154.4191734171435257 ) ) ;
#2361 = CARTESIAN_POINT ( 'NONE',  ( 8.311307340579794811, 1438.191820051692957, 214.6582588010098220 ) ) ;
#2362 = CARTESIAN_POINT ( 'NONE',  ( 10.47043688597563182, 1522.051704408389924, 197.0050518223378333 ) ) ;
#2363 = DIRECTION ( 'NONE',  ( 0.000000000000000000, 1.000000000000000000, 0.000000000000000000 ) ) ;
#2364 = CARTESIAN_POINT ( 'NONE',  ( 21.50779739108499911, 1509.664126782800167, 229.6171678230790008 ) ) ;
#2365 = ADVANCED_FACE ( 'NONE', ( #55352 ), #21144, .T. ) ;
#2366 = DIRECTION ( 'NONE',  ( 0.0001171895853481130984, -0.004053780167009412259, -0.9999917765326665764 ) ) ;
#2367 = CARTESIAN_POINT ( 'NONE',  ( -13.31005321830910049, 1421.758539284290009, 222.0611081425300029 ) ) ;
#2368 = CARTESIAN_POINT ( 'NONE',  ( 16.67088892840000014, 1415.091340903430137, 226.7043766012980370 ) ) ;
#2369 = CARTESIAN_POINT ( 'NONE',  ( 9.756855720090040762, 1469.870621582290141, 211.6163541429820043 ) ) ;
#2370 = LINE ( 'NONE', #21301, #78244 ) ;
#2371 = CARTESIAN_POINT ( 'NONE',  ( -0.7576635715699989726, 1516.855632454399938, 206.2537338009369989 ) ) ;
#2372 = CARTESIAN_POINT ( 'NONE',  ( 35.49642997870000016, 1419.115857373830067, 269.2425788070980275 ) ) ;
#2373 = DIRECTION ( 'NONE',  ( 0.000000000000000000, -1.000000000000000000, 6.123233995736769734E-17 ) ) ;
#2374 = CARTESIAN_POINT ( 'NONE',  ( 18.54481337859999712, 1435.291263500080049, 145.9381164648980018 ) ) ;
#2375 = CARTESIAN_POINT ( 'NONE',  ( 21.33248983229999851, 1469.154932495629964, 194.2950544196980047 ) ) ;
#2376 = CARTESIAN_POINT ( 'NONE',  ( -23.20318700179999993, 1433.765057477279925, 215.6666483125179923 ) ) ;
#2377 = CARTESIAN_POINT ( 'NONE',  ( 20.79738390328738973, 1512.187213306747481, 237.0406858230487899 ) ) ;
#2378 = DIRECTION ( 'NONE',  ( -0.6736849260863839728, 0.000000000000000000, 0.7390186874254150995 ) ) ;
#2379 = CARTESIAN_POINT ( 'NONE',  ( 17.43549085681724620, 1525.211473355384896, 237.2113236654630555 ) ) ;
#2380 = CARTESIAN_POINT ( 'NONE',  ( 20.85715831679999965, 1508.960610662329827, 227.8108772789979923 ) ) ;
#2381 = CARTESIAN_POINT ( 'NONE',  ( -17.79016152762200065, 1578.884136531910144, 256.3461289262040168 ) ) ;
#2382 = CARTESIAN_POINT ( 'NONE',  ( -16.80421781410000293, 1416.570018552790089, 209.4889783200769955 ) ) ;
#2383 = CARTESIAN_POINT ( 'NONE',  ( -13.40137408230000027, 1443.240311850900071, 187.4864273396979968 ) ) ;
#2384 = EDGE_CURVE ( 'NONE', #41410, #69866, #97870, .T. ) ;
#2385 = CARTESIAN_POINT ( 'NONE',  ( -7.768355502971520110, 1383.288536228370049, 218.8604790520440133 ) ) ;
#2386 = CARTESIAN_POINT ( 'NONE',  ( -31.78593504660000235, 1435.767691617939818, 136.0101313228979905 ) ) ;
#2387 = CARTESIAN_POINT ( 'NONE',  ( 19.53786426059039982, 1512.187213306747481, 236.7197124308265188 ) ) ;
#2388 = ORIENTED_EDGE ( 'NONE', *, *, #77734, .T. ) ;
#2389 = EDGE_CURVE ( 'NONE', #104546, #62931, #33940, .T. ) ;
#2390 = CARTESIAN_POINT ( 'NONE',  ( 5.857434645806802287, 1510.600498174433824, 216.6525474564166416 ) ) ;
#2391 = CARTESIAN_POINT ( 'NONE',  ( -13.26148688360019889, 1409.376161713930060, 215.9976612687219983 ) ) ;
#2393 = ADVANCED_FACE ( 'NONE', ( #13301 ), #4921, .F. ) ;
#2392 = CARTESIAN_POINT ( 'NONE',  ( -12.56042467189510070, 1508.551704408300111, 210.1774334085390024 ) ) ;
#2394 = DIRECTION ( 'NONE',  ( -0.8090169943749422332, 0.000000000000000000, 0.5877852522924802425 ) ) ;
#2395 = CARTESIAN_POINT ( 'NONE',  ( -30.02861084270000092, 1467.289302230230078, 266.6068817451980522 ) ) ;
#2396 = CARTESIAN_POINT ( 'NONE',  ( -11.87618687435380060, 1481.834444412209905, 209.2076145084409973 ) ) ;
#2397 = CARTESIAN_POINT ( 'NONE',  ( 0.2074656164648590040, 1420.466249280530064, 183.0472788335430039 ) ) ;
#2398 = CARTESIAN_POINT ( 'NONE',  ( 3.835404308833624043, 1396.046995657106436, 216.1425064568209677 ) ) ;
#2399 = CARTESIAN_POINT ( 'NONE',  ( -76.64144279794061276, 1384.645875352879784, 301.4166218965220310 ) ) ;
#2400 = CARTESIAN_POINT ( 'NONE',  ( -31.39107788089150120, 1384.971443476370041, 206.3467394566210089 ) ) ;
#2401 = CARTESIAN_POINT ( 'NONE',  ( 17.72398368343529995, 1424.436447516579847, 227.0786475391319925 ) ) ;
#2402 = CARTESIAN_POINT ( 'NONE',  ( 20.59563400740000105, 1507.764823632930074, 227.7386540762980189 ) ) ;
#2403 = CARTESIAN_POINT ( 'NONE',  ( 14.22148428500000072, 1463.290759296229908, 223.5797348918979992 ) ) ;
#2404 = EDGE_CURVE ( 'NONE', #19958, #1894, #81618, .T. ) ;
#2405 = CARTESIAN_POINT ( 'NONE',  ( -10.06401538933667617, 1494.155344878688538, 204.3007335798515953 ) ) ;
#2406 = DIRECTION ( 'NONE',  ( -0.000000000000000000, -1.000000000000000000, -0.000000000000000000 ) ) ;
#2407 = CARTESIAN_POINT ( 'NONE',  ( -8.847848347470000263, 1384.943898188619869, 199.9248160043189841 ) ) ;
#2408 = CARTESIAN_POINT ( 'NONE',  ( 9.548870672246419389, 1470.075437067029952, 212.3439895025789781 ) ) ;
#2409 = CARTESIAN_POINT ( 'NONE',  ( 16.02395358489999921, 1414.971262582530017, 204.1331252983779905 ) ) ;
#2410 = CARTESIAN_POINT ( 'NONE',  ( -12.72965162820000096, 1416.819756528429934, 195.1130951807980125 ) ) ;
#2411 = CARTESIAN_POINT ( 'NONE',  ( 3.296743891669999815, 1423.732652684919913, 192.8007254636989956 ) ) ;
#2412 = CARTESIAN_POINT ( 'NONE',  ( 23.64646709530000024, 1410.660431756829894, 211.3066953406180346 ) ) ;
#2413 = CARTESIAN_POINT ( 'NONE',  ( -12.58535514000000077, 1434.516889947230084, 149.4256401672980132 ) ) ;
#2414 = CARTESIAN_POINT ( 'NONE',  ( 8.092055354027909431, 1461.514282906779954, 228.8774819441619854 ) ) ;
#2415 = CARTESIAN_POINT ( 'NONE',  ( -15.80894762269999987, 1421.035220212730110, 227.0411592943979997 ) ) ;
#2417 = CARTESIAN_POINT ( 'NONE',  ( -9.813982587879999997, 1383.225161719749849, 200.4195862986289853 ) ) ;
#2416 = CARTESIAN_POINT ( 'NONE',  ( -10.97117066409999886, 1432.448735918919965, 151.7701026906980246 ) ) ;
#2418 = CARTESIAN_POINT ( 'NONE',  ( 0.7147005917380000461, 1413.022813240129835, 233.2540336019980032 ) ) ;
#2419 = DIRECTION ( 'NONE',  ( -0.9510565162951559737, 0.000000000000000000, 0.3090169943749403458 ) ) ;
#2420 = CARTESIAN_POINT ( 'NONE',  ( -15.57808073540140015, 1420.358152465259991, 210.5578313205389804 ) ) ;
#2421 = ADVANCED_FACE ( 'NONE', ( #67608 ), #17297, .T. ) ;
#2422 = DIRECTION ( 'NONE',  ( 0.000000000000000000, 1.000000000000000000, 0.000000000000000000 ) ) ;
#2423 = CARTESIAN_POINT ( 'NONE',  ( -9.655745333040000489, 1363.739547551589794, 210.6218459616991936 ) ) ;
#2424 = CARTESIAN_POINT ( 'NONE',  ( 7.323974606304999746, 1516.647924054489977, 205.0857262875869935 ) ) ;
#2425 = CARTESIAN_POINT ( 'NONE',  ( -18.26675480510339966, 1424.840341062940070, 227.6848255537819909 ) ) ;
#2426 = CARTESIAN_POINT ( 'NONE',  ( -12.99662007391709828, 1486.035101518850070, 185.1546605780280004 ) ) ;
#2427 = EDGE_CURVE ( 'NONE', #57154, #5163, #43285, .T. ) ;
#2428 =( LENGTH_UNIT ( ) NAMED_UNIT ( * ) SI_UNIT ( .MILLI., .METRE. ) );
#2429 = CARTESIAN_POINT ( 'NONE',  ( -4.267907479344899890, 1441.147145201229932, 158.2247601545199984 ) ) ;
#2431 = ORIENTED_EDGE ( 'NONE', *, *, #101280, .T. ) ;
#2430 = CARTESIAN_POINT ( 'NONE',  ( -65.82654097011999283, 1379.741992558670063, 276.1399068737349580 ) ) ;
#2432 = B_SPLINE_CURVE_WITH_KNOTS ( 'NONE', 3,
 ( #2111, #9379, #60345, #70424, #78233, #34573, #45212, #2665, #17183, #35127, #68758, #53619, #69309, #96139, #94467, #102316, #78795, #51377, #17740, #1546, #36237, #52501, #27280, #87192, #95041, #19418, #102862, #26159, #51941, #104543, #93916, #27839, #42989, #86085, #87761 ),
 .UNSPECIFIED., .F., .F.,
 ( 4, 2, 2, 1, 1, 1, 2, 2, 2, 2, 1, 1, 2, 2, 2, 2, 1, 1, 2, 2, 4 ),
 ( 0.000000000000000000, 0.1250000000010763057, 0.1875000000015372703, 0.2187500000018319513, 0.2343750000020440594, 0.2421875000021461444, 0.2460937500021343760, 0.2500000000021225799, 0.3125000000017883472, 0.3750000000014541146, 0.4375000000011198265, 0.4687500000009520162, 0.4843750000009499623, 0.5000000000009479084, 0.6250000000006392664, 0.6875000000004880540, 0.7187500000005031531, 0.7343750000006038503, 0.7421875000006541434, 0.7500000000007044365, 1.000000000000000000 ),
 .UNSPECIFIED. ) ;
#2433 = VERTEX_POINT ( 'NONE', #33412 ) ;
#2434 = CARTESIAN_POINT ( 'NONE',  ( 11.94589852435660049, 1433.532020350129869, 150.0906635879709938 ) ) ;
#2435 = CARTESIAN_POINT ( 'NONE',  ( 27.59571790329999885, 1509.876735559930012, 217.1915671101180010 ) ) ;
#2436 = ORIENTED_EDGE ( 'NONE', *, *, #3034, .T. ) ;
#2437 = CYLINDRICAL_SURFACE ( 'NONE', #49131, 1.999999999999999556 ) ;
#2438 = CARTESIAN_POINT ( 'NONE',  ( 1.441539424170000139, 1414.983771850430003, 191.7394860166979811 ) ) ;
#2440 = CARTESIAN_POINT ( 'NONE',  ( 7.097634907420000694, 1427.571433844230114, 133.6118001900980232 ) ) ;
#2439 = CARTESIAN_POINT ( 'NONE',  ( 15.92079754877469888, 1418.953290843069908, 191.2668077924519991 ) ) ;
#2441 = CARTESIAN_POINT ( 'NONE',  ( 1.600048698852036821, 1402.754281879943164, 135.5999999980979851 ) ) ;
#2442 = CARTESIAN_POINT ( 'NONE',  ( 2.807222226979999569, 1507.639813928429930, 181.3621223444980046 ) ) ;
#2443 = CARTESIAN_POINT ( 'NONE',  ( -106.0207696801649888, 1378.913060388890017, 305.3967244531619940 ) ) ;
#2444 = CARTESIAN_POINT ( 'NONE',  ( 15.60455980150000066, 1409.457983623130076, 225.4781096464980124 ) ) ;
#2445 = SHAPE_REPRESENTATION_RELATIONSHIP ( 'NONE' , 'NONE' ,  #49395, #43980 ) ;
#2446 = CARTESIAN_POINT ( 'NONE',  ( 6.561995960394999550, 1517.083030555940013, 212.3803205491769859 ) ) ;
#2447 = CARTESIAN_POINT ( 'NONE',  ( 14.02570581375280057, 1415.492117401590122, 197.2936844647439898 ) ) ;
#2448 = CARTESIAN_POINT ( 'NONE',  ( -8.430248171497698451, 1423.638267348000227, 208.7623137433450040 ) ) ;
#2449 = DIRECTION ( 'NONE',  ( 0.9993908264651745199, 0.03489951250826475032, -1.985168277816197220E-06 ) ) ;
#2450 = ORIENTED_EDGE ( 'NONE', *, *, #90057, .F. ) ;
#2451 = CARTESIAN_POINT ( 'NONE',  ( 14.41724164474389980, 1435.959222008799998, 149.8873962520480063 ) ) ;
#2452 = CARTESIAN_POINT ( 'NONE',  ( -0.2658540493943280514, 1507.120020986029886, 237.3289608297170048 ) ) ;
#2453 = ORIENTED_EDGE ( 'NONE', *, *, #40652, .F. ) ;
#2454 = ORIENTED_EDGE ( 'NONE', *, *, #62551, .F. ) ;
#2455 = ORIENTED_EDGE ( 'NONE', *, *, #89035, .F. ) ;
#2456 = CIRCLE ( 'NONE', #52702, 8.432239102140000497 ) ;
#2457 = FACE_OUTER_BOUND ( 'NONE', #57047, .T. ) ;
#2458 = CARTESIAN_POINT ( 'NONE',  ( -1.450401227179999974, 1465.036285835330091, 237.9109516336980334 ) ) ;
#2459 = CARTESIAN_POINT ( 'NONE',  ( 15.21996770522959075, 1451.144474064526321, 149.5789455636493983 ) ) ;
#2460 = CARTESIAN_POINT ( 'NONE',  ( -8.862374925020001015, 1384.916129524170174, 218.6851829152190305 ) ) ;
#2461 = CARTESIAN_POINT ( 'NONE',  ( 10.95832423829999946, 1461.079497205190137, 209.0421603647289999 ) ) ;
#2462 = CARTESIAN_POINT ( 'NONE',  ( -17.29202514838780047, 1448.661259662438624, 218.6898848943429812 ) ) ;
#2463 = CARTESIAN_POINT ( 'NONE',  ( -49.26428229891999422, 1379.685895086444134, 238.1610838164967845 ) ) ;
#2464 = CARTESIAN_POINT ( 'NONE',  ( 4.234072258626359719, 1446.327634590550133, 164.0209402114229817 ) ) ;
#2465 = DIRECTION ( 'NONE',  ( 0.000000000000000000, 0.000000000000000000, 1.000000000000000000 ) ) ;
#2466 = VERTEX_POINT ( 'NONE', #101717 ) ;
#2467 = CARTESIAN_POINT ( 'NONE',  ( -7.338411997524999286, 1517.170512887980067, 206.6372682748769876 ) ) ;
#2468 = ORIENTED_EDGE ( 'NONE', *, *, #61058, .F. ) ;
#2469 = CARTESIAN_POINT ( 'NONE',  ( 24.18808457932529876, 1440.913060387330006, 236.3222631112920169 ) ) ;
#2470 = B_SPLINE_CURVE_WITH_KNOTS ( 'NONE', 3,
 ( #80697, #56045, #90172, #47644, #14015, #91291, #48205, #99120, #82343, #65559 ),
 .UNSPECIFIED., .F., .F.,
 ( 4, 2, 2, 2, 4 ),
 ( 0.000000000000000000, 0.0007403986298595355894, 0.001480797259719071179, 0.002221195889578606551, 0.002961594519438142357 ),
 .UNSPECIFIED. ) ;
#2471 = CARTESIAN_POINT ( 'NONE',  ( -20.35720481940000326, 1509.285579243329948, 188.5733115188980094 ) ) ;
#2472 = ORIENTED_EDGE ( 'NONE', *, *, #39779, .T. ) ;
#2473 = CARTESIAN_POINT ( 'NONE',  ( -6.961854465055609786, 1508.551568319609714, 202.5699773954310103 ) ) ;
#2474 = CARTESIAN_POINT ( 'NONE',  ( -14.27671737280000031, 1409.578295415130015, 190.9808476275980240 ) ) ;
#2475 = DIRECTION ( 'NONE',  ( 5.980589973904019347E-17, -1.000000000000000000, 1.736889445713099699E-16 ) ) ;
#2477 = CARTESIAN_POINT ( 'NONE',  ( 10.11243515225073253, 1384.926148861439970, 216.4689601570716206 ) ) ;
#2476 = CARTESIAN_POINT ( 'NONE',  ( -24.67047192240000086, 1440.997076622129725, 210.6883048062180137 ) ) ;
#2478 = CARTESIAN_POINT ( 'NONE',  ( 0.05881865638218039538, 1422.953928556980145, 192.4959481148550253 ) ) ;
#2479 = DIRECTION ( 'NONE',  ( -0.5877852522924780221, 0.000000000000000000, -0.8090169943749438985 ) ) ;
#2480 = CARTESIAN_POINT ( 'NONE',  ( -12.45980060270386325, 1434.393920058226058, 147.3155158375118106 ) ) ;
#2481 = CYLINDRICAL_SURFACE ( 'NONE', #3800, 2.000000000000003109 ) ;
#2482 = CARTESIAN_POINT ( 'NONE',  ( 23.17024198529999879, 1435.306528354219836, 138.2719568257980143 ) ) ;
#2484 = CARTESIAN_POINT ( 'NONE',  ( -104.8708816957486079, 1379.440243493634625, 304.0281164857488534 ) ) ;
#2483 = CARTESIAN_POINT ( 'NONE',  ( 6.312923550360000746, 1466.069290330830199, 233.5697152015980009 ) ) ;
#2485 = CARTESIAN_POINT ( 'NONE',  ( -6.552897405075000847, 1516.858146885269889, 215.6784973415170157 ) ) ;
#2486 = CARTESIAN_POINT ( 'NONE',  ( -31.55061275096994322, 1525.712830164893376, 217.0331825386441835 ) ) ;
#2487 = CARTESIAN_POINT ( 'NONE',  ( -9.094257307180781069, 1384.874748761890260, 199.9429999480310016 ) ) ;
#2488 = CARTESIAN_POINT ( 'NONE',  ( 28.77213281849999760, 1509.917805405330000, 206.8662417206580244 ) ) ;
#2489 = CARTESIAN_POINT ( 'NONE',  ( -1.118903308544999975, 1517.003078582959688, 212.0031713441969998 ) ) ;
#2490 = CARTESIAN_POINT ( 'NONE',  ( -22.28696231330000188, 1506.798305107930219, 208.8466800722590051 ) ) ;
#2491 = CARTESIAN_POINT ( 'NONE',  ( -15.47297587689426557, 1486.079131676784073, 186.6300910287472448 ) ) ;
#2493 = VERTEX_POINT ( 'NONE', #74906 ) ;
#2492 = CARTESIAN_POINT ( 'NONE',  ( -102.7364941740000006, 1384.940050820800025, 311.2335147922589726 ) ) ;
#2494 = CARTESIAN_POINT ( 'NONE',  ( -16.55387768533248760, 1524.739563915921963, 237.4558587828119300 ) ) ;
#2495 = CARTESIAN_POINT ( 'NONE',  ( 31.95512683279999777, 1442.955673907409846, 244.1805851208980300 ) ) ;
#2496 = CARTESIAN_POINT ( 'NONE',  ( -17.07358046210000069, 1458.578126118629825, 230.5958457830979853 ) ) ;
#2497 = CARTESIAN_POINT ( 'NONE',  ( -20.46002591053339970, 1487.323977817510013, 205.7581023369010040 ) ) ;
#2498 = CARTESIAN_POINT ( 'NONE',  ( 2.424144924439999738, 1411.756412224629912, 231.8070165610980098 ) ) ;
#2499 = CARTESIAN_POINT ( 'NONE',  ( -19.55701159389999688, 1456.127805513129942, 228.1967745823979783 ) ) ;
#2501 = CARTESIAN_POINT ( 'NONE',  ( 5.360343482560489647, 1422.243226290559960, 144.1300244169619873 ) ) ;
#2500 = CARTESIAN_POINT ( 'NONE',  ( 11.77285469709999965, 1432.580854644329975, 150.8112884974979977 ) ) ;
#2502 = CARTESIAN_POINT ( 'NONE',  ( -0.08582555699890000167, 1434.820761659839945, 190.2315579290979883 ) ) ;
#2503 = CARTESIAN_POINT ( 'NONE',  ( -105.9021060456189929, 1378.331563972840058, 306.6119379298179979 ) ) ;
#2504 = ORIENTED_EDGE ( 'NONE', *, *, #99232, .F. ) ;
#2505 = CARTESIAN_POINT ( 'NONE',  ( 4.612507273904999039, 1516.886345593249871, 204.1123678647870179 ) ) ;
#2506 = CARTESIAN_POINT ( 'NONE',  ( 0.8891455584299999826, 1405.782266041229832, 268.4834380686980353 ) ) ;
#2507 = CARTESIAN_POINT ( 'NONE',  ( 1.448833437790000067, 1515.064791419390076, 213.4512947760589725 ) ) ;
#2508 = CARTESIAN_POINT ( 'NONE',  ( 6.451457836568720516, 1472.045055758229864, 270.0713883367370727 ) ) ;
#2509 = CARTESIAN_POINT ( 'NONE',  ( 5.449707646490000279, 1437.831544062859848, 154.7230940508980268 ) ) ;
#2510 = CARTESIAN_POINT ( 'NONE',  ( -27.95267559379999867, 1445.173348659859812, 137.3670106800980193 ) ) ;
#2511 = EDGE_CURVE ( 'NONE', #36154, #43673, #59211, .T. ) ;
#2512 = CARTESIAN_POINT ( 'NONE',  ( -39.04178053251449398, 1440.913060396100036, 257.8928201085430487 ) ) ;
#2513 = CARTESIAN_POINT ( 'NONE',  ( 35.96429464762940142, 1450.032176740089881, 136.2433800175030001 ) ) ;
#2514 = LINE ( 'NONE', #19254, #14480 ) ;
#2515 = CARTESIAN_POINT ( 'NONE',  ( -1.041670117440000043, 1431.845129037589913, 200.7519452021190034 ) ) ;
#2516 = ADVANCED_FACE ( 'NONE', ( #76536 ), #83285, .T. ) ;
#2517 = CARTESIAN_POINT ( 'NONE',  ( -1.280362375963175925, 1451.774120661134702, 183.7183834684909129 ) ) ;
#2518 = CARTESIAN_POINT ( 'NONE',  ( -1.441032304519999974, 1508.469141107589849, 220.8031696840990037 ) ) ;
#2519 = FACE_OUTER_BOUND ( 'NONE', #17744, .T. ) ;
#2520 = ORIENTED_EDGE ( 'NONE', *, *, #7279, .T. ) ;
#2521 = CARTESIAN_POINT ( 'NONE',  ( -5.513435911474870110, 1508.551704408389924, 202.1089243664339961 ) ) ;
#2522 = CIRCLE ( 'NONE', #40049, 5.000000000000000888 ) ;
#2523 = CARTESIAN_POINT ( 'NONE',  ( 2.117784065689999995, 1485.870414137690204, 198.4209573190990170 ) ) ;
#2524 = CARTESIAN_POINT ( 'NONE',  ( 5.461196333839980710, 1466.354709272569835, 200.5519884797059831 ) ) ;
#2525 = CARTESIAN_POINT ( 'NONE',  ( -1.323475895380000100, 1475.548043385830169, 269.2940999293979871 ) ) ;
#2526 = DIRECTION ( 'NONE',  ( -0.6736849260863841948, 0.000000000000000000, 0.7390186874254148774 ) ) ;
#2527 = CARTESIAN_POINT ( 'NONE',  ( -28.14152818990000071, 1508.624282259429947, 209.9763561811920169 ) ) ;
#2528 = CARTESIAN_POINT ( 'NONE',  ( -3.160714151128600768, 1448.277390616477760, 184.6271217223835208 ) ) ;
#2529 = CARTESIAN_POINT ( 'NONE',  ( -21.51311642161260096, 1384.857552017839907, 221.6326953624779890 ) ) ;
#2530 = EDGE_CURVE ( 'NONE', #53058, #98779, #37933, .T. ) ;
#2531 = B_SPLINE_SURFACE_WITH_KNOTS ( 'NONE', 5, 5, ( 
 ( #105964, #29242, #12431, #27583, #86936, #36538 ),
 ( #80752, #37086, #53931, #4060, #11353, #27043 ),
 ( #69620, #45524, #70735, #61230, #104848, #95344 ),
 ( #79665, #71290, #70187, #18605, #10227, #104296 ),
 ( #90788, #39844, #99726, #5699, #93403, #48260 ),
 ( #30879, #59285, #76066, #106498, #13513, #98635 ) ),
 .UNSPECIFIED., .F., .F., .F.,
 ( 6, 6 ),
 ( 6, 6 ),
 ( 30.28564970649999921, 65.26196872020000228 ),
 ( -5.551115123129999410E-17, 2.000000000000000000 ),
 .UNSPECIFIED. ) ;
#2532 = CARTESIAN_POINT ( 'NONE',  ( -18.73327636269999985, 1416.067629296030191, 207.5724925610480227 ) ) ;
#2533 = CARTESIAN_POINT ( 'NONE',  ( 11.87347576087729983, 1432.890358733870244, 149.9808790610170206 ) ) ;
#2534 = CARTESIAN_POINT ( 'NONE',  ( 26.42364260034900170, 1435.420366583209898, 135.3851555990079873 ) ) ;
#2535 = CARTESIAN_POINT ( 'NONE',  ( -4.748065736170270057, 1396.078866497700119, 219.0788021602359663 ) ) ;
#2536 = CARTESIAN_POINT ( 'NONE',  ( -14.92155151709999927, 1422.314549104929938, 229.4637292825979955 ) ) ;
#2537 = CARTESIAN_POINT ( 'NONE',  ( -16.22807784372640327, 1409.487890249900147, 225.2828359470929627 ) ) ;
#2538 = CARTESIAN_POINT ( 'NONE',  ( 7.362632729190000447, 1435.943783413959864, 149.6281905168980302 ) ) ;
#2539 = VERTEX_POINT ( 'NONE', #82737 ) ;
#2540 = CARTESIAN_POINT ( 'NONE',  ( -11.38338690025777566, 1501.299005368582584, 207.9712302931637851 ) ) ;
#2541 = CARTESIAN_POINT ( 'NONE',  ( -13.58182138314900023, 1508.547225165770215, 210.2471086096300041 ) ) ;
#2542 = CARTESIAN_POINT ( 'NONE',  ( -19.67699484670000132, 1505.884115603990040, 219.0034652596590092 ) ) ;
#2544 = CARTESIAN_POINT ( 'NONE',  ( -9.939836244837959356, 1438.908082076499795, 209.7414840783459908 ) ) ;
#2543 = CARTESIAN_POINT ( 'NONE',  ( 11.06146551219999985, 1426.045375945929891, 103.4405617616979924 ) ) ;
#2545 = DIRECTION ( 'NONE',  ( 0.000000000000000000, 1.000000000000000000, -6.123233995736769734E-17 ) ) ;
#2546 = CARTESIAN_POINT ( 'NONE',  ( 4.342007114105989274, 1423.862343561519765, 183.6384043889740099 ) ) ;
#2547 = CARTESIAN_POINT ( 'NONE',  ( 3.259729297834999873, 1517.119374999550018, 201.7846921639870175 ) ) ;
#2548 = CARTESIAN_POINT ( 'NONE',  ( 7.508655101499999596, 1425.090260414829800, 212.1994906295190049 ) ) ;
#2549 = CARTESIAN_POINT ( 'NONE',  ( -18.65941870309999828, 1468.219763198689861, 201.0822021908089994 ) ) ;
#2550 = CARTESIAN_POINT ( 'NONE',  ( 7.105603315319999780, 1508.968284067629838, 181.5155069444980143 ) ) ;
#2551 = FACE_OUTER_BOUND ( 'NONE', #82195, .T. ) ;
#2552 = CARTESIAN_POINT ( 'NONE',  ( 3.686444929539999915, 1449.169999442819972, 184.1879160448980031 ) ) ;
#2553 = CIRCLE ( 'NONE', #40081, 33.13701971169416538 ) ;
#2554 = EDGE_CURVE ( 'NONE', #73642, #32988, #47243, .T. ) ;
#2555 = CARTESIAN_POINT ( 'NONE',  ( 8.553883624160958377, 1365.586653183476074, 210.6218459617142003 ) ) ;
#2557 = ORIENTED_EDGE ( 'NONE', *, *, #36332, .F. ) ;
#2556 = CARTESIAN_POINT ( 'NONE',  ( 4.492546581380000958, 1453.878649273890005, 217.3453973181289882 ) ) ;
#2558 = ORIENTED_EDGE ( 'NONE', *, *, #1457, .F. ) ;
#2559 = DIRECTION ( 'NONE',  ( 0.3188159025760192167, 6.661338147751048295E-13, -0.9478166596260261256 ) ) ;
#2560 = DIRECTION ( 'NONE',  ( 0.000000000000000000, 0.000000000000000000, 1.000000000000000000 ) ) ;
#2561 = CARTESIAN_POINT ( 'NONE',  ( 4.063550476549999679, 1497.713060387329961, 230.5763704537980061 ) ) ;
#2562 = CARTESIAN_POINT ( 'NONE',  ( -7.548380910495000151, 1510.399296111369949, 213.9269235281369959 ) ) ;
#2565 = ADVANCED_FACE ( 'NONE', ( #42380 ), #83049, .T. ) ;
#2564 = CARTESIAN_POINT ( 'NONE',  ( -0.5757066863040000149, 1486.369792037530033, 181.7416807582980027 ) ) ;
#2563 = CARTESIAN_POINT ( 'NONE',  ( -107.2481891120000057, 1387.964334016630119, 309.9317261882590628 ) ) ;
#2566 = CARTESIAN_POINT ( 'NONE',  ( -32.70818033930468971, 1524.201670966335314, 201.1172547305815499 ) ) ;
#2567 = CARTESIAN_POINT ( 'NONE',  ( -2.765433514615380339, 1464.871865108300199, 198.4563297728979876 ) ) ;
#2568 = CARTESIAN_POINT ( 'NONE',  ( 32.37018134260406299, 1511.187213306747708, 218.0712926453362002 ) ) ;
#2569 = CARTESIAN_POINT ( 'NONE',  ( -2.500000000000000000, 1448.666881541910243, 158.2772778262040276 ) ) ;
#2570 = CARTESIAN_POINT ( 'NONE',  ( 7.480565282176630859, 1396.174287483810076, 217.2553306272309896 ) ) ;
#2571 = CARTESIAN_POINT ( 'NONE',  ( 13.95725854910000052, 1409.400458595830059, 216.7863739448980027 ) ) ;
#2572 = CARTESIAN_POINT ( 'NONE',  ( -0.7741896587115789652, 1405.842756057490078, 267.2348683375010410 ) ) ;
#2573 = CARTESIAN_POINT ( 'NONE',  ( 41.14953079480000042, 1443.861296646169876, 136.9341326470980107 ) ) ;
#2574 = VERTEX_POINT ( 'NONE', #32870 ) ;
#2575 = CARTESIAN_POINT ( 'NONE',  ( -11.30152483640000050, 1432.323726368159896, 151.5220244150980307 ) ) ;
#2576 = CARTESIAN_POINT ( 'NONE',  ( 12.77277809070000103, 1442.800511918249867, 187.2257584126980134 ) ) ;
#2577 = VERTEX_POINT ( 'NONE', #101166 ) ;
#2578 = ORIENTED_EDGE ( 'NONE', *, *, #35703, .F. ) ;
#2579 = CARTESIAN_POINT ( 'NONE',  ( -3.850432596239999672, 1454.142522157690109, 199.7891201249690027 ) ) ;
#2580 = CARTESIAN_POINT ( 'NONE',  ( 10.02176186330000007, 1364.879735892739973, 207.6218459616989946 ) ) ;
#2581 = CARTESIAN_POINT ( 'NONE',  ( 0.01289778877310149806, 1516.939723362869927, 214.1281058189269970 ) ) ;
#2582 = CARTESIAN_POINT ( 'NONE',  ( 2.933667421895000516, 1512.215430505229961, 217.0052628094269949 ) ) ;
#2583 = ORIENTED_EDGE ( 'NONE', *, *, #102915, .T. ) ;
#2584 = CARTESIAN_POINT ( 'NONE',  ( 7.892794852110000647, 1424.253103618490059, 211.9974886484589831 ) ) ;
#2585 = CARTESIAN_POINT ( 'NONE',  ( -77.18524045069999318, 1374.656469662890004, 292.4664101653590365 ) ) ;
#2586 = CARTESIAN_POINT ( 'NONE',  ( -106.9163825377050046, 1378.913060387289988, 301.2728918013489761 ) ) ;
#2587 = CARTESIAN_POINT ( 'NONE',  ( 4.998515157294999511, 1516.787536375099990, 205.0819486540370065 ) ) ;
#2588 = CARTESIAN_POINT ( 'NONE',  ( -23.46990153750000019, 1440.913060387330006, 234.5287104542979932 ) ) ;
#2589 = CARTESIAN_POINT ( 'NONE',  ( -3.415238448984999842, 1511.775527460079957, 205.7066075212470082 ) ) ;
#2590 = CARTESIAN_POINT ( 'NONE',  ( 5.004475574535000248, 1517.026025493960105, 201.3999380438669959 ) ) ;
#2591 = CARTESIAN_POINT ( 'NONE',  ( -2.820494496349999825, 1409.011554225530062, 231.0801550522980108 ) ) ;
#2593 = ORIENTED_EDGE ( 'NONE', *, *, #108261, .T. ) ;
#2592 = CARTESIAN_POINT ( 'NONE',  ( -7.473911413859999797, 1445.831988935439767, 184.4657707173980157 ) ) ;
#2594 = DIRECTION ( 'NONE',  ( -1.000000000000000000, 0.000000000000000000, 0.000000000000000000 ) ) ;
#2595 = DIRECTION ( 'NONE',  ( 0.03489949670250328678, -0.9993908270190956511, 0.000000000000000000 ) ) ;
#2596 = CIRCLE ( 'NONE', #93734, 1.999999999999998668 ) ;
#2597 = CARTESIAN_POINT ( 'NONE',  ( -8.743435183079999007, 1384.548231727749908, 218.5812667456789882 ) ) ;
#2598 = LINE ( 'NONE', #45147, #87430 ) ;
#2599 = CARTESIAN_POINT ( 'NONE',  ( -25.68312509100000085, 1435.472708640420024, 135.9883602099980067 ) ) ;
#2600 = CARTESIAN_POINT ( 'NONE',  ( 36.10026286240969995, 1420.948621320099846, 270.1974792939670351 ) ) ;
#2601 = CARTESIAN_POINT ( 'NONE',  ( 4.043366220174999803, 1516.951766529250108, 211.9887038632370206 ) ) ;
#2602 = CARTESIAN_POINT ( 'NONE',  ( -65.82430152899999598, 1379.749194687180079, 274.2810710116589803 ) ) ;
#2603 = CIRCLE ( 'NONE', #108064, 0.5000000000000000000 ) ;
#2604 = CARTESIAN_POINT ( 'NONE',  ( 0.01879578147808497537, 1507.445532545652668, 237.3948011092800527 ) ) ;
#2605 = CARTESIAN_POINT ( 'NONE',  ( 16.19637447162289945, 1427.902519050969886, 200.9814647519390007 ) ) ;
#2606 = CARTESIAN_POINT ( 'NONE',  ( 19.19561268899386164, 1410.945033757853935, 195.6515498416322885 ) ) ;
#2607 = CARTESIAN_POINT ( 'NONE',  ( 7.724874613184999461, 1517.139320148880188, 209.8621665372610039 ) ) ;
#2608 = ORIENTED_EDGE ( 'NONE', *, *, #64704, .T. ) ;
#2609 = CARTESIAN_POINT ( 'NONE',  ( -1.837422785889859966, 1451.937235225580025, 184.2647726144609805 ) ) ;
#2610 = CARTESIAN_POINT ( 'NONE',  ( -2.354922572530000036, 1415.377356045230044, 232.9301894368979902 ) ) ;
#2611 = CARTESIAN_POINT ( 'NONE',  ( -47.38272174249999580, 1385.138016709929843, 256.2741787814589998 ) ) ;
#2612 = ORIENTED_EDGE ( 'NONE', *, *, #24045, .T. ) ;
#2613 = CARTESIAN_POINT ( 'NONE',  ( -33.03375078350489957, 1385.219055440710008, 231.5328850939089875 ) ) ;
#2614 = CARTESIAN_POINT ( 'NONE',  ( -41.95590887306661187, 1512.187213306747481, 225.5974093378525254 ) ) ;
#2615 = PRODUCT_DEFINITION_SHAPE ( 'NONE', 'NONE',  #63131 ) ;
#2616 = CARTESIAN_POINT ( 'NONE',  ( 7.976687763616449267, 1478.700324351950030, 233.7293620187649879 ) ) ;
#2617 = CARTESIAN_POINT ( 'NONE',  ( -23.16109911851550152, 1509.676460279360299, 226.5529115091270000 ) ) ;
#2618 = CARTESIAN_POINT ( 'NONE',  ( -2.680555363329999885, 1409.943153559129996, 186.5983026406979945 ) ) ;
#2619 = CARTESIAN_POINT ( 'NONE',  ( -0.3489575399770000197, 1409.432092532930028, 233.0021930383979907 ) ) ;
#2620 = DIRECTION ( 'NONE',  ( 0.000000000000000000, 0.000000000000000000, 1.000000000000000000 ) ) ;
#2622 = CARTESIAN_POINT ( 'NONE',  ( -3.895671750679999601, 1421.575785769229924, 185.6035415176980052 ) ) ;
#2621 = CARTESIAN_POINT ( 'NONE',  ( 0.01244693565920149993, 1516.939646076049939, 214.9034317483770167 ) ) ;
#2623 = CARTESIAN_POINT ( 'NONE',  ( 18.85941592800000066, 1507.948893524529922, 188.5324247627980014 ) ) ;
#2624 = CARTESIAN_POINT ( 'NONE',  ( -10.73514660131351839, 1424.973046421745494, 139.1354236205272343 ) ) ;
#2625 = ORIENTED_EDGE ( 'NONE', *, *, #23915, .T. ) ;
#2626 = CARTESIAN_POINT ( 'NONE',  ( -12.70695307632060000, 1416.230844595159851, 196.1160997689679846 ) ) ;
#2627 = CARTESIAN_POINT ( 'NONE',  ( -20.79738390328697761, 1512.187213306747481, 237.0406858230491025 ) ) ;
#2628 = ORIENTED_EDGE ( 'NONE', *, *, #102846, .F. ) ;
#2629 = DIRECTION ( 'NONE',  ( -1.755985294532469921E-16, 1.000000000000000000, -1.338183447452831989E-16 ) ) ;
#2630 = DIRECTION ( 'NONE',  ( -5.980589973904019347E-17, 1.000000000000000000, -1.736889445713099699E-16 ) ) ;
#2631 = CARTESIAN_POINT ( 'NONE',  ( 7.899080318006880930, 1511.275365984429982, 203.5511717028010139 ) ) ;
#2632 = VECTOR ( 'NONE', #26109, 1000.000000000000114 ) ;
#2633 = CARTESIAN_POINT ( 'NONE',  ( 3.255456066760000322, 1443.056962053689858, 217.4032295331390117 ) ) ;
#2634 = CARTESIAN_POINT ( 'NONE',  ( -34.09079054513859575, 1524.667648926078755, 200.3377533957330172 ) ) ;
#2635 = CARTESIAN_POINT ( 'NONE',  ( -20.87481493262672316, 1525.712830164893376, 234.0672365764787628 ) ) ;
#2636 = CARTESIAN_POINT ( 'NONE',  ( -17.60627563539920004, 1410.895669414250051, 194.0661810348550205 ) ) ;
#2637 = CARTESIAN_POINT ( 'NONE',  ( -18.46184065339999592, 1425.292999754929951, 225.8901492113980112 ) ) ;
#2638 = CARTESIAN_POINT ( 'NONE',  ( -18.60903282430000161, 1435.578292681360153, 146.4159160996979949 ) ) ;
#2639 = DIRECTION ( 'NONE',  ( -0.6742693640212139572, -4.521919481779819710E-17, -0.7384854939282339270 ) ) ;
#2640 = DIRECTION ( 'NONE',  ( 0.000000000000000000, -1.000000000000000000, 0.000000000000000000 ) ) ;
#2642 = CARTESIAN_POINT ( 'NONE',  ( -4.996962189119175335, 1391.699467640956755, 203.5364589991260118 ) ) ;
#2641 = CARTESIAN_POINT ( 'NONE',  ( 4.127868055549999582, 1487.366509936789953, 197.8725145131990075 ) ) ;
#2643 = CARTESIAN_POINT ( 'NONE',  ( 0.4260839224734190300, 1523.429859730332510, 244.8289481157567593 ) ) ;
#2644 = ORIENTED_EDGE ( 'NONE', *, *, #20930, .T. ) ;
#2645 = DIRECTION ( 'NONE',  ( -0.7071067811865492381, 0.000000000000000000, -0.7071067811865457964 ) ) ;
#2646 = CARTESIAN_POINT ( 'NONE',  ( 27.24409202460000046, 1507.989521382530029, 207.2276950740879897 ) ) ;
#2647 = CARTESIAN_POINT ( 'NONE',  ( -20.36287103150000277, 1507.711394158289977, 209.4617748114379765 ) ) ;
#2648 = CARTESIAN_POINT ( 'NONE',  ( -2.721324782990000468, 1483.631500244790004, 198.7950877463990196 ) ) ;
#2649 = CARTESIAN_POINT ( 'NONE',  ( -16.50171338560091883, 1417.502269239514590, 205.9477000315035582 ) ) ;
#2650 = CARTESIAN_POINT ( 'NONE',  ( -2.136371150128812957, 1525.856065479248173, 241.3693944374256546 ) ) ;
#2651 = CARTESIAN_POINT ( 'NONE',  ( 11.31902516476188403, 1434.496189561966730, 151.5389523139992036 ) ) ;
#2652 = B_SPLINE_SURFACE_WITH_KNOTS ( 'NONE', 5, 1, ( 
 ( #62206, #72793 ),
 ( #106920, #19611 ),
 ( #53813, #54354 ),
 ( #87949, #105845 ),
 ( #79541, #98523 ),
 ( #21789, #2844 ),
 ( #38075, #71159 ),
 ( #105282, #88485 ),
 ( #37526, #62773 ),
 ( #72252, #20158 ),
 ( #97429, #66612 ),
 ( #49796, #91772 ),
 ( #31870, #57104 ),
 ( #66059, #85432 ),
 ( #58193, #15050 ),
 ( #23466, #100183 ),
 ( #99610, #42910 ),
 ( #81709, #90669 ),
 ( #49248, #68676 ),
 ( #77067, #92321 ),
 ( #108584, #40271 ),
 ( #75002, #47584 ),
 ( #48142, #32436 ),
 ( #109152, #15592 ) ),
 .UNSPECIFIED., .F., .F., .F.,
 ( 6, 3, 3, 3, 3, 3, 3, 6 ),
 ( 2, 2 ),
 ( 21.22849039669999982, 21.28303926239999910, 21.63383848259999809, 29.22288786549999884, 33.07574020050000030, 38.86051041610000567, 44.90455290039999880, 44.92448007948200228 ),
 ( 0.000000000000000000, 4.091690576229590093 ),
 .UNSPECIFIED. ) ;
#2653 = CARTESIAN_POINT ( 'NONE',  ( -24.89734149463049917, 1440.895437401190065, 210.4282814422280126 ) ) ;
#2654 = CARTESIAN_POINT ( 'NONE',  ( -22.48884418427819654, 1509.698386039090110, 189.0638421303760026 ) ) ;
#2655 = CARTESIAN_POINT ( 'NONE',  ( -11.02047842716129900, 1489.051096228969982, 214.3262357338399795 ) ) ;
#2656 = CARTESIAN_POINT ( 'NONE',  ( 18.46111059403260057, 1471.786040807520067, 195.2229583357160152 ) ) ;
#2658 = EDGE_CURVE ( 'NONE', #75744, #32788, #24653, .T. ) ;
#2657 = CARTESIAN_POINT ( 'NONE',  ( -93.71881660438820916, 1383.767977992140004, 309.5718267011319540 ) ) ;
#2659 = CARTESIAN_POINT ( 'NONE',  ( -109.2480983758639894, 1384.372607579929991, 311.2262217477910440 ) ) ;
#2661 = FACE_OUTER_BOUND ( 'NONE', #7524, .T. ) ;
#2660 =( BOUNDED_CURVE ( )  B_SPLINE_CURVE ( 3, ( #67670, #49211, #50851, #58160 ),
 .UNSPECIFIED., .F., .F. ) 
 B_SPLINE_CURVE_WITH_KNOTS ( ( 4, 4 ),
 ( 4.148177588089209777, 5.276600406385650643 ),
 .UNSPECIFIED. ) 
 CURVE ( )  GEOMETRIC_REPRESENTATION_ITEM ( )  RATIONAL_B_SPLINE_CURVE ( ( 1.000000000000000000, 0.8966737078530113703, 0.8966737078530113703, 1.000000000000000000 ) ) 
 REPRESENTATION_ITEM ( '' )  );
#2662 = CARTESIAN_POINT ( 'NONE',  ( -2.000106894569579907, 1516.529320347400244, 201.4129447258819994 ) ) ;
#2664 = ORIENTED_EDGE ( 'NONE', *, *, #37056, .F. ) ;
#2663 = CARTESIAN_POINT ( 'NONE',  ( -18.65443362373700253, 1443.700676952599906, 211.5885854860179904 ) ) ;
#2665 = CARTESIAN_POINT ( 'NONE',  ( -18.44192439828749386, 1458.893192691106606, 227.6840821340426828 ) ) ;
#2666 = CARTESIAN_POINT ( 'NONE',  ( -92.78435512849998190, 1384.849527344140142, 294.1459074807589786 ) ) ;
#2667 = CARTESIAN_POINT ( 'NONE',  ( -18.69816095120731347, 1522.382868172863937, 234.8576566410005171 ) ) ;
#2668 = ADVANCED_FACE ( 'NONE', ( #103945 ), #50924, .F. ) ;
#2669 = ORIENTED_EDGE ( 'NONE', *, *, #55867, .F. ) ;
#2670 = EDGE_LOOP ( 'NONE', ( #50814, #100737, #66353, #10024 ) ) ;
#2671 = CARTESIAN_POINT ( 'NONE',  ( 18.24633262864339756, 1416.842625005220043, 209.2839319684169936 ) ) ;
#2672 = CARTESIAN_POINT ( 'NONE',  ( -109.3498435130000104, 1384.940401497779931, 297.1386112594590259 ) ) ;
#2673 = CARTESIAN_POINT ( 'NONE',  ( 13.05900637259455088, 1442.991450065072740, 169.4123328598832927 ) ) ;
#2675 = CARTESIAN_POINT ( 'NONE',  ( -45.67178388729999483, 1443.699401684990107, 266.1886045289979847 ) ) ;
#2674 = CARTESIAN_POINT ( 'NONE',  ( 38.89664643686552381, 1429.356341322375329, 269.5911935481951218 ) ) ;
#2676 = AXIS2_PLACEMENT_3D ( 'NONE', #83147, #74218, #41693 ) ;
#2677 = CARTESIAN_POINT ( 'NONE',  ( 9.820871455967859376, 1435.437962752369913, 208.9438784677120111 ) ) ;
#2678 = FACE_OUTER_BOUND ( 'NONE', #50434, .T. ) ;
#2679 = CARTESIAN_POINT ( 'NONE',  ( 1.788309357509999975, 1480.920316621989969, 229.5180507505990022 ) ) ;
#2680 = CARTESIAN_POINT ( 'NONE',  ( -19.74739994659999809, 1486.108233622730040, 190.1528327617980096 ) ) ;
#2681 = CARTESIAN_POINT ( 'NONE',  ( 13.85929416610000153, 1410.325638497430191, 191.1496551215980162 ) ) ;
#2682 = CARTESIAN_POINT ( 'NONE',  ( 5.419569259119999316, 1423.396285514930014, 185.7614624571979789 ) ) ;
#2684 = CARTESIAN_POINT ( 'NONE',  ( -6.070028495709999916, 1440.055555071880008, 154.5780773277979847 ) ) ;
#2683 = AXIS2_PLACEMENT_3D ( 'NONE', #72839, #63899, #54407 ) ;
#2685 = CARTESIAN_POINT ( 'NONE',  ( 7.539474771970000155, 1438.620589226539778, 153.9375993584980051 ) ) ;
#2686 = CARTESIAN_POINT ( 'NONE',  ( 1.959285310369999866, 1474.800623465989929, 220.3715843581990157 ) ) ;
#2687 = CIRCLE ( 'NONE', #18699, 11.73843354579999954 ) ;
#2688 = CARTESIAN_POINT ( 'NONE',  ( -10.99273638719279944, 1491.630725221910097, 209.8916735765129715 ) ) ;
#2689 = DIRECTION ( 'NONE',  ( -1.755985294532469921E-16, 1.000000000000000000, -1.338183447452831989E-16 ) ) ;
#2690 = ORIENTED_EDGE ( 'NONE', *, *, #104370, .F. ) ;
#2691 = CARTESIAN_POINT ( 'NONE',  ( -2.487924095911139943, 1509.038643251730036, 213.6090949890719912 ) ) ;
#2692 = CARTESIAN_POINT ( 'NONE',  ( -21.57663945839999897, 1488.879494602689874, 202.2366601406689881 ) ) ;
#2693 = CARTESIAN_POINT ( 'NONE',  ( -42.28244123120000353, 1440.913087102529971, 269.8809842803979677 ) ) ;
#2694 = CARTESIAN_POINT ( 'NONE',  ( 2.175409717514719593E-31, 1397.551704408390151, 209.1218459616989946 ) ) ;
#2695 = CARTESIAN_POINT ( 'NONE',  ( 17.84692852179999889, 1410.032953050229935, 222.8512888978980016 ) ) ;
#2696 = FACE_OUTER_BOUND ( 'NONE', #32323, .T. ) ;
#2697 = CARTESIAN_POINT ( 'NONE',  ( 9.202936508599998788, 1519.913060387329779, 187.9174701372980110 ) ) ;
#2698 = DIRECTION ( 'NONE',  ( 0.8386695113602744556, -0.4884709562387554715, 0.2408932868012610695 ) ) ;
#2699 = CARTESIAN_POINT ( 'NONE',  ( -6.502638733110000402, 1458.675974398089920, 216.3652329231589704 ) ) ;
#2700 = CARTESIAN_POINT ( 'NONE',  ( 10.24616803579280955, 1362.814633186277206, 207.6218459616987673 ) ) ;
#2701 = CARTESIAN_POINT ( 'NONE',  ( -43.64288401327429767, 1430.870968838220051, 269.0307669793850209 ) ) ;
#2702 = FACE_OUTER_BOUND ( 'NONE', #87860, .T. ) ;
#2703 = ORIENTED_EDGE ( 'NONE', *, *, #78909, .F. ) ;
#2704 = CARTESIAN_POINT ( 'NONE',  ( -113.4000000000000057, 1390.913060387289988, 304.2218459572590064 ) ) ;
#2705 = ORIENTED_EDGE ( 'NONE', *, *, #13807, .F. ) ;
#2706 = CARTESIAN_POINT ( 'NONE',  ( 0.01012488564660149991, 1516.989863902050047, 210.2497743036369968 ) ) ;
#2707 = FACE_OUTER_BOUND ( 'NONE', #62290, .T. ) ;
#2708 = B_SPLINE_CURVE_WITH_KNOTS ( 'NONE', 3,
 ( #29885, #55678, #22008, #65718, #23130, #6348, #29339, #63540, #97656, #20926, #49469, #60081, #25881, #23687, #57872, #109375, #68482, #179, #109911, #100404, #58416, #17468, #92002, #7447, #42158, #51118, #41045, #101480, #51669, #94197, #24231, #85805, #8538, #93634, #66287, #85242, #32652, #16369, #75223, #102583, #92542, #9103, #76310, #15276, #24768, #43270, #110460, #108807, #50567, #83589 ),
 .UNSPECIFIED., .F., .F.,
 ( 4, 2, 2, 1, 1, 2, 2, 2, 2, 1, 1, 1, 2, 2, 2, 2, 1, 1, 1, 2, 2, 2, 2, 1, 1, 1, 1, 2, 2, 2, 4 ),
 ( 0.000000000000000000, 0.1249999999987768118, 0.1874999999981652177, 0.2187499999978483323, 0.2343749999976874887, 0.2421874999976066367, 0.2499999999975258125, 0.3749999999967162934, 0.4374999999962853603, 0.4687499999960699770, 0.4843749999959355845, 0.4921874999958685826, 0.4960937499958351093, 0.4999999999958015806, 0.6249999999951432184, 0.6874999999948141483, 0.7187499999946499463, 0.7343749999945659024, 0.7421874999945267115, 0.7460937499945041740, 0.7499999999944817475, 0.8124999999947372098, 0.8437499999948295804, 0.8593749999948757656, 0.8671874999948987472, 0.8710937499949140683, 0.8730468749949186202, 0.8740234374949206186, 0.8749999999949225060, 0.9374999999974612530, 1.000000000000000000 ),
 .UNSPECIFIED. ) ;
#2709 = CARTESIAN_POINT ( 'NONE',  ( -21.92423686329999910, 1509.678671609130106, 190.3411753249980052 ) ) ;
#2710 = CARTESIAN_POINT ( 'NONE',  ( -11.93035415709999825, 1425.413819132130129, 188.4997697822980172 ) ) ;
#2711 = CARTESIAN_POINT ( 'NONE',  ( -0.06724585139096760089, 1496.218926208830226, 221.4696802319550102 ) ) ;
#2712 = EDGE_LOOP ( 'NONE', ( #76998, #67436, #41942, #17145, #20832, #42478, #88108, #19322, #74311 ) ) ;
#2713 = AXIS2_PLACEMENT_3D ( 'NONE', #58056, #35038, #18772 ) ;
#2714 = CARTESIAN_POINT ( 'NONE',  ( 11.60004869885203860, 1425.798524488559224, 137.3564486607050128 ) ) ;
#2716 = CARTESIAN_POINT ( 'NONE',  ( -18.82283039985420103, 1508.494552192559922, 210.3700853329929998 ) ) ;
#2715 = B_SPLINE_CURVE_WITH_KNOTS ( 'NONE', 3,
 ( #43010, #51962, #470, #87212, #28411, #2131, #36810, #19439, #17759, #69887, #1566, #52519, #44675, #10503, #53074, #95061, #86104, #53638, #43560, #18328, #44118, #102880, #61481, #27857, #78816, #104563, #34594, #62038, #96161, #85531, #9397, #77710, #1021, #35146, #71001, #9945, #8825, #78252, #62610, #95609, #87782, #11062, #45232, #68780, #27300, #26178, #35698, #79371, #18876 ),
 .UNSPECIFIED., .F., .F.,
 ( 4, 3, 3, 3, 3, 3, 3, 3, 3, 3, 3, 3, 3, 3, 3, 3, 4 ),
 ( 18.80849845009409904, 19.89523491153060064, 20.96856624117300072, 22.02675316388739901, 23.06319306041429940, 24.08912262180639985, 25.10114662952789999, 26.07035490390000021, 27.16676746860280289, 28.25787814313009960, 28.80892602879999842, 29.95369467953739928, 30.17821159120000019, 30.86285437239999752, 31.20517576310000152, 31.47730732964389944, 31.54749715370000018 ),
 .UNSPECIFIED. ) ;
#2717 = CARTESIAN_POINT ( 'NONE',  ( 8.720808663110000580, 1471.131229068790162, 214.3482137472890088 ) ) ;
#2719 = AXIS2_PLACEMENT_3D ( 'NONE', #1308, #2982, #44980 ) ;
#2718 = CARTESIAN_POINT ( 'NONE',  ( -9.835408609723900852, 1439.978059041610095, 207.2081094720800252 ) ) ;
#2720 = VERTEX_POINT ( 'NONE', #85468 ) ;
#2721 = CARTESIAN_POINT ( 'NONE',  ( -22.30921403175210216, 1414.773190229989950, 269.6722363558229745 ) ) ;
#2722 = CARTESIAN_POINT ( 'NONE',  ( 3.255809864005000165, 1516.837969789639828, 208.3644199470059846 ) ) ;
#2723 = CARTESIAN_POINT ( 'NONE',  ( 2.075990293979999676E-15, 1427.305457135430061, 123.0297916884979941 ) ) ;
#2724 = DIRECTION ( 'NONE',  ( -0.000000000000000000, -1.000000000000000000, -0.000000000000000000 ) ) ;
#2726 = ORIENTED_EDGE ( 'NONE', *, *, #17330, .T. ) ;
#2725 = CARTESIAN_POINT ( 'NONE',  ( -7.454882155592339465, 1365.567498750975801, 209.6218459617148824 ) ) ;
#2727 = ORIENTED_EDGE ( 'NONE', *, *, #2658, .T. ) ;
#2728 = CARTESIAN_POINT ( 'NONE',  ( 45.58236131563670313, 1442.587618990865167, 268.9762474203030820 ) ) ;
#2729 = CARTESIAN_POINT ( 'NONE',  ( -0.9715543786848610530, 1467.707556206300069, 220.1856978582200099 ) ) ;
#2730 = CARTESIAN_POINT ( 'NONE',  ( 3.631811699416766182, 1424.449122815756482, 184.4189500110305744 ) ) ;
#2731 = CARTESIAN_POINT ( 'NONE',  ( -0.7722883701989260441, 1405.989080711971610, 266.9611463895769248 ) ) ;
#2732 = B_SPLINE_SURFACE_WITH_KNOTS ( 'NONE', 3, 5, ( 
 ( #62215, #96341, #54364, #87960, #11249, #45410 ),
 ( #36976, #71168, #88494, #46509, #69516, #103637 ),
 ( #26934, #61125, #48152, #63859, #64956, #23476 ),
 ( #5589, #39738, #107479, #65510, #57113, #72260 ) ),
 .UNSPECIFIED., .F., .F., .F.,
 ( 4, 4 ),
 ( 6, 6 ),
 ( 9.885439000899999940, 20.49136985950000067 ),
 ( -1.110223024629999900E-16, 1.000000000000000000 ),
 .UNSPECIFIED. ) ;
#2733 = CARTESIAN_POINT ( 'NONE',  ( -21.03310440946566118, 1506.473666153777458, 215.6352647881066389 ) ) ;
#2734 = CARTESIAN_POINT ( 'NONE',  ( -19.33962896530000108, 1430.793376614329873, 224.1389769688979925 ) ) ;
#2735 = CARTESIAN_POINT ( 'NONE',  ( -14.45783241110000006, 1416.839692138830060, 221.3920770704979759 ) ) ;
#2736 = EDGE_CURVE ( 'NONE', #69095, #5037, #100762, .T. ) ;
#2737 = CARTESIAN_POINT ( 'NONE',  ( -11.65147249325539924, 1391.913060387150153, 208.7366933367970034 ) ) ;
#2738 = CARTESIAN_POINT ( 'NONE',  ( 5.582246511119999255, 1448.050470245740144, 184.8003903095979865 ) ) ;
#2739 = CARTESIAN_POINT ( 'NONE',  ( -2.493699806765000027, 1516.858326417339867, 206.6451124560869914 ) ) ;
#2740 = ORIENTED_EDGE ( 'NONE', *, *, #68131, .T. ) ;
#2741 = CARTESIAN_POINT ( 'NONE',  ( -5.940539704407486354, 1521.951704408389787, 229.2045057395878871 ) ) ;
#2742 = CARTESIAN_POINT ( 'NONE',  ( 1.470748360624610118, 1485.779233187629870, 182.0437263276170086 ) ) ;
#2743 = ORIENTED_EDGE ( 'NONE', *, *, #15924, .T. ) ;
#2744 = CARTESIAN_POINT ( 'NONE',  ( 2.487922401834560038, 1508.551704408489968, 204.2892346663010130 ) ) ;
#2745 = CARTESIAN_POINT ( 'NONE',  ( 26.02147390689500028, 1451.119159405719984, 136.5906395866829826 ) ) ;
#2746 = EDGE_CURVE ( 'NONE', #82445, #48574, #85257, .T. ) ;
#2747 = CARTESIAN_POINT ( 'NONE',  ( 13.58235846979999906, 1416.828040475229955, 196.3349388281980055 ) ) ;
#2748 = CARTESIAN_POINT ( 'NONE',  ( -25.91586689989999925, 1384.961148014880109, 203.4475886829490037 ) ) ;
#2749 = CARTESIAN_POINT ( 'NONE',  ( -7.821732098484999618, 1513.613303996360173, 201.3872288444869980 ) ) ;
#2750 = CARTESIAN_POINT ( 'NONE',  ( 17.53069353509999928, 1410.450030956830005, 192.7292893744979949 ) ) ;
#2751 = CARTESIAN_POINT ( 'NONE',  ( 16.90742463041998178, 1444.994950788469168, 162.4348201727410981 ) ) ;
#2752 = CARTESIAN_POINT ( 'NONE',  ( 16.19062492770000006, 1409.478449468330155, 224.9177422266980102 ) ) ;
#2753 = CARTESIAN_POINT ( 'NONE',  ( -19.39313673858097786, 1425.487805292472331, 223.5657354981669016 ) ) ;
#2754 = CARTESIAN_POINT ( 'NONE',  ( 0.4857184740991669636, 1450.960785378189939, 181.9315177450459942 ) ) ;
#2755 = CARTESIAN_POINT ( 'NONE',  ( -8.001312726290001009, 1383.415254610280044, 218.6981543553289953 ) ) ;
#2756 = CARTESIAN_POINT ( 'NONE',  ( 3.456007385174999946, 1516.647534046129977, 215.6697273451470096 ) ) ;
#2757 = CARTESIAN_POINT ( 'NONE',  ( 26.02532873005809932, 1446.299728326420109, 138.3445498427680036 ) ) ;
#2758 = ORIENTED_EDGE ( 'NONE', *, *, #78090, .T. ) ;
#2759 = CARTESIAN_POINT ( 'NONE',  ( -17.00797534510000020, 1417.537219551289809, 207.7155427019889942 ) ) ;
#2760 = B_SPLINE_CURVE_WITH_KNOTS ( 'NONE', 3,
 ( #91547, #40036, #5890, #83688, #100491, #6984, #76396, #68026, #75852, #57959, #24862, #25414 ),
 .UNSPECIFIED., .F., .F.,
 ( 4, 2, 2, 2, 2, 4 ),
 ( 0.000000000000000000, 0.0007194225121803652289, 0.001079133768270242044, 0.001438845024360118968, 0.002158267536539317053, 0.002877690048718515789 ),
 .UNSPECIFIED. ) ;
#2761 = CARTESIAN_POINT ( 'NONE',  ( -8.826538978809569613, 1481.764331815820015, 203.1249516821810062 ) ) ;
#2762 = CARTESIAN_POINT ( 'NONE',  ( -9.233179502644661696, 1483.825061176979943, 201.6045247071639892 ) ) ;
#2763 = CARTESIAN_POINT ( 'NONE',  ( -1275.711986934299830, 50.13405481578730161, 10006.43705117240097 ) ) ;
#2764 = VECTOR ( 'NONE', #6624, 1000.000000000000000 ) ;
#2765 = CARTESIAN_POINT ( 'NONE',  ( -38.10256990246180209, 1448.730340511050144, 136.3926152995410064 ) ) ;
#2766 = CARTESIAN_POINT ( 'NONE',  ( -10.67290635632400075, 1462.958185458769776, 206.2378460151369950 ) ) ;
#2767 = CARTESIAN_POINT ( 'NONE',  ( -4.540901342749999792, 1462.614442895030152, 248.0989693022980020 ) ) ;
#2768 = CARTESIAN_POINT ( 'NONE',  ( -14.48634920707452345, 1416.023439644662858, 203.8591738278827563 ) ) ;
#2769 = CARTESIAN_POINT ( 'NONE',  ( 11.21203837859999908, 1433.014098020569918, 151.5746018212979891 ) ) ;
#2770 = CARTESIAN_POINT ( 'NONE',  ( -1.531246620494349863E-13, 1515.064792882589927, 204.7923971856590128 ) ) ;
#2771 = B_SPLINE_SURFACE_WITH_KNOTS ( 'NONE', 5, 5, ( 
 ( #2231, #69988, #105217, #28505, #104656, #96824 ),
 ( #29062, #20093, #38010, #88952, #62136, #71660 ),
 ( #97895, #46433, #74934, #30701, #91159, #31251 ),
 ( #47518, #40756, #65434, #81640, #74388, #32363 ),
 ( #109082, #4417, #73265, #22827, #98993, #22268 ),
 ( #89507, #38544, #66544, #40206, #57032, #72723 ),
 ( #49180, #100647, #14434, #83310, #99543, #98453 ),
 ( #90602, #56470, #48632, #48066, #82200, #23933 ),
 ( #13325, #12798, #39086, #82762, #6054, #57585 ) ),
 .UNSPECIFIED., .F., .F., .F.,
 ( 6, 3, 6 ),
 ( 6, 6 ),
 ( 13.37707388139999942, 15.22166854640000011, 20.70300873780000117 ),
 ( 0.000000000000000000, 2.000000000000000000 ),
 .UNSPECIFIED. ) ;
#2772 = CARTESIAN_POINT ( 'NONE',  ( -9.941270763631750995, 1461.322045364539918, 211.0756248058849849 ) ) ;
#2773 = CARTESIAN_POINT ( 'NONE',  ( -109.8950784940000034, 1385.179886903279794, 297.0358873837590181 ) ) ;
#2774 = CARTESIAN_POINT ( 'NONE',  ( 14.37971982616849864, 1427.198226358100101, 195.4139261895699917 ) ) ;
#2775 = ORIENTED_EDGE ( 'NONE', *, *, #42629, .T. ) ;
#2776 = CARTESIAN_POINT ( 'NONE',  ( -2.500000000000000000, 1425.929641636930000, 184.1455913746980002 ) ) ;
#2777 = FACE_OUTER_BOUND ( 'NONE', #106070, .T. ) ;
#2778 = CARTESIAN_POINT ( 'NONE',  ( -3.521375377790000094, 1486.251522346130059, 181.9026547285980087 ) ) ;
#2779 = CARTESIAN_POINT ( 'NONE',  ( 0.9465674214180413992, 1397.942249001653408, 196.1218459535367344 ) ) ;
#2780 = CARTESIAN_POINT ( 'NONE',  ( -9.445105015150314642, 1490.485136446142405, 189.9884643024701916 ) ) ;
#2781 = CARTESIAN_POINT ( 'NONE',  ( 24.62246550709999937, 1430.359249624430277, 210.8418034199980013 ) ) ;
#2782 = DIRECTION ( 'NONE',  ( 9.500914144214121536E-47, -1.000000000000000000, 1.836970198721029688E-16 ) ) ;
#2783 = CARTESIAN_POINT ( 'NONE',  ( -14.23402513019999915, 1509.239477817229954, 233.4640051292979877 ) ) ;
#2784 = CARTESIAN_POINT ( 'NONE',  ( -23.70810543552709859, 1383.849544535609994, 222.6483769287150096 ) ) ;
#2785 = CARTESIAN_POINT ( 'NONE',  ( 1.332267629549999902E-15, 1391.913060387289988, 209.1218459616989946 ) ) ;
#2786 = CARTESIAN_POINT ( 'NONE',  ( 2.499937251232230206, 1420.100124192889780, 93.04876811845220175 ) ) ;
#2787 = DIRECTION ( 'NONE',  ( 1.835183309750130004E-16, 1.000000000000000000, 1.599799320660000123E-19 ) ) ;
#2788 = CARTESIAN_POINT ( 'NONE',  ( 8.835383234542518949, 1451.659256596650039, 211.9451859889190075 ) ) ;
#2790 = VERTEX_POINT ( 'NONE', #961 ) ;
#2789 = CARTESIAN_POINT ( 'NONE',  ( 3.584819811890000096, 1441.506325834089921, 217.6012887279890151 ) ) ;
#2791 = CARTESIAN_POINT ( 'NONE',  ( -0.5621806315070000393, 1416.843576368729828, 227.7683147415980045 ) ) ;
#2792 = CARTESIAN_POINT ( 'NONE',  ( -8.911791977641406959, 1388.063585253917608, 200.4736995634368100 ) ) ;
#2793 = CARTESIAN_POINT ( 'NONE',  ( -4.683500221610000125, 1475.763858493990028, 199.9162038546990061 ) ) ;
#2794 = EDGE_CURVE ( 'NONE', #62471, #93599, #3249, .T. ) ;
#2796 = ORIENTED_EDGE ( 'NONE', *, *, #85629, .T. ) ;
#2795 = CARTESIAN_POINT ( 'NONE',  ( -35.54866228632759828, 1451.502040174180138, 134.0999999984919668 ) ) ;
#2797 = CARTESIAN_POINT ( 'NONE',  ( -13.97982192548539970, 1420.196024271650003, 195.9955606719640002 ) ) ;
#2798 = ORIENTED_EDGE ( 'NONE', *, *, #52789, .T. ) ;
#2799 = AXIS2_PLACEMENT_3D ( 'NONE', #81723, #3960, #12877 ) ;
#2800 =( BOUNDED_CURVE ( )  B_SPLINE_CURVE ( 3, ( #65459, #91182, #14462, #48656 ),
 .UNSPECIFIED., .F., .T. ) 
 B_SPLINE_CURVE_WITH_KNOTS ( ( 4, 4 ),
 ( 1.569840739599899893, 1.584370187438904898 ),
 .UNSPECIFIED. ) 
 CURVE ( )  GEOMETRIC_REPRESENTATION_ITEM ( )  RATIONAL_B_SPLINE_CURVE ( ( 1.000000000000000000, 0.9999824080061611165, 0.9999824080061611165, 1.000000000000000000 ) ) 
 REPRESENTATION_ITEM ( '' )  );
#2801 = CARTESIAN_POINT ( 'NONE',  ( -12.56550536004469976, 1389.228114667070031, 215.4313542344819723 ) ) ;
#2802 = CARTESIAN_POINT ( 'NONE',  ( 7.599227146675000100, 1512.341036988540054, 206.8869224911269953 ) ) ;
#2803 = CARTESIAN_POINT ( 'NONE',  ( 23.52438575543722266, 1410.744643456190261, 207.8036212700959027 ) ) ;
#2804 = CARTESIAN_POINT ( 'NONE',  ( -0.3695175741990010532, 1431.482447068790179, 217.8907632844189664 ) ) ;
#2805 = CARTESIAN_POINT ( 'NONE',  ( 32.37018134260397062, 1512.187213306747481, 200.1723992780595438 ) ) ;
#2806 = CARTESIAN_POINT ( 'NONE',  ( 10.95613331925090073, 1409.295656986259928, 219.2973035561870176 ) ) ;
#2807 = CARTESIAN_POINT ( 'NONE',  ( 7.271052316819548444, 1522.051704408389924, 192.9032753742981470 ) ) ;
#2808 = CARTESIAN_POINT ( 'NONE',  ( -104.7009857956030032, 1385.232336910320100, 296.9001550543150074 ) ) ;
#2809 = CARTESIAN_POINT ( 'NONE',  ( -18.21532205240000124, 1430.623180213430032, 192.4625600593979868 ) ) ;
#2810 = CARTESIAN_POINT ( 'NONE',  ( 12.12282008797060051, 1491.484709589460181, 207.0783957174520253 ) ) ;
#2812 = ORIENTED_EDGE ( 'NONE', *, *, #94728, .T. ) ;
#2811 = FACE_OUTER_BOUND ( 'NONE', #36135, .T. ) ;
#2813 = VERTEX_POINT ( 'NONE', #60303 ) ;
#2814 = CARTESIAN_POINT ( 'NONE',  ( -11.48964235823120106, 1415.152886232609944, 195.4311914138980057 ) ) ;
#2815 = CARTESIAN_POINT ( 'NONE',  ( 0.1056718228839060025, 1496.587049647489948, 196.7558449521239936 ) ) ;
#2816 = CARTESIAN_POINT ( 'NONE',  ( 29.63432559401041644, 1509.974525581411626, 210.8805246852537891 ) ) ;
#2817 = CARTESIAN_POINT ( 'NONE',  ( 11.91400850019820012, 1427.411956927870051, 208.4948976547729842 ) ) ;
#2818 = CARTESIAN_POINT ( 'NONE',  ( 3.843918134389999963, 1397.403951559329926, 221.5816238264980029 ) ) ;
#2819 = CARTESIAN_POINT ( 'NONE',  ( 1.704993463989999958, 1417.527066604930042, 233.7744655226979944 ) ) ;
#2820 = CARTESIAN_POINT ( 'NONE',  ( -5.783578535681273003, 1516.788854543809975, 213.9010045776934419 ) ) ;
#2821 = CARTESIAN_POINT ( 'NONE',  ( -0.5133842287350000033, 1453.574655232029954, 183.2220989632980093 ) ) ;
#2822 = CARTESIAN_POINT ( 'NONE',  ( -9.690020260104200034, 1366.026910387847920, 210.6218459616991936 ) ) ;
#2823 = DIRECTION ( 'NONE',  ( -0.4770263929453174567, 0.7067418228236591604, -0.5224574779878943254 ) ) ;
#2824 = EDGE_CURVE ( 'NONE', #27879, #39872, #55388, .T. ) ;
#2825 = CARTESIAN_POINT ( 'NONE',  ( 2.864326087304999824, 1516.826109302209943, 206.6287721023469999 ) ) ;
#2826 = CARTESIAN_POINT ( 'NONE',  ( -12.88529584148609963, 1435.823228682630088, 150.7601930830520018 ) ) ;
#2827 = CARTESIAN_POINT ( 'NONE',  ( 3.047790189539999695, 1421.605827388129910, 133.5221414154979698 ) ) ;
#2828 = CARTESIAN_POINT ( 'NONE',  ( 22.08622291482349809, 1523.456872492435195, 233.8253038720783366 ) ) ;
#2829 = CARTESIAN_POINT ( 'NONE',  ( 15.20279577643499991, 1516.814170398969964, 225.0317485278669949 ) ) ;
#2830 = CARTESIAN_POINT ( 'NONE',  ( 40.82021089259919933, 1444.183590552639998, 136.9680080752169999 ) ) ;
#2831 = ORIENTED_EDGE ( 'NONE', *, *, #37412, .T. ) ;
#2832 = CARTESIAN_POINT ( 'NONE',  ( -23.31685689360000069, 1508.124115171030098, 195.2425524244979727 ) ) ;
#2835 = CARTESIAN_POINT ( 'NONE',  ( -0.6474865636856289575, 1507.275793736380137, 231.8019763530149930 ) ) ;
#2834 = CIRCLE ( 'NONE', #61915, 0.9999999999999981126 ) ;
#2833 = CARTESIAN_POINT ( 'NONE',  ( -11.03890283615240087, 1426.504156864669994, 93.54506299971779981 ) ) ;
#2836 = CARTESIAN_POINT ( 'NONE',  ( 1.136004274065000041, 1516.815173273089840, 211.9874827793370287 ) ) ;
#2837 = LINE ( 'NONE', #28569, #78414 ) ;
#2838 = CARTESIAN_POINT ( 'NONE',  ( -18.32011680670000331, 1412.375216495030145, 259.8063326943979519 ) ) ;
#2839 = CARTESIAN_POINT ( 'NONE',  ( 2.581285063860000228, 1486.431383666189959, 219.6162510183990264 ) ) ;
#2840 = CARTESIAN_POINT ( 'NONE',  ( -26.09332909799999811, 1435.428316942780157, 135.6095828681980038 ) ) ;
#2841 = CARTESIAN_POINT ( 'NONE',  ( 2.516438831412172394, 1448.700965663029820, 154.6256843495723103 ) ) ;
#2842 = CARTESIAN_POINT ( 'NONE',  ( 12.51099983133400073, 1416.825784014559986, 196.0986189223339977 ) ) ;
#2843 = ORIENTED_EDGE ( 'NONE', *, *, #95289, .T. ) ;
#2844 = CARTESIAN_POINT ( 'NONE',  ( -5.386055587696130686, 1432.253251891989976, 154.6059980213289862 ) ) ;
#2845 = CARTESIAN_POINT ( 'NONE',  ( 11.97297233184965570, 1513.029502680773930, 225.6983645998317058 ) ) ;
#2846 = CARTESIAN_POINT ( 'NONE',  ( 5.886744298249999119, 1509.118630028029884, 238.1980421559979959 ) ) ;
#2847 = ORIENTED_EDGE ( 'NONE', *, *, #49017, .T. ) ;
#2848 = ORIENTED_EDGE ( 'NONE', *, *, #54124, .T. ) ;
#2849 = CARTESIAN_POINT ( 'NONE',  ( 9.582368326175020101, 1452.681705851589868, 210.9617576210509924 ) ) ;
#2850 = CARTESIAN_POINT ( 'NONE',  ( 6.308047056989999568, 1423.705631131640075, 194.8804956342990238 ) ) ;
#2851 = EDGE_LOOP ( 'NONE', ( #82408, #92311, #63309, #90861 ) ) ;
#2852 = CARTESIAN_POINT ( 'NONE',  ( -0.3231955925520000328, 1419.319817403729985, 184.6083566393980107 ) ) ;
#2853 = CARTESIAN_POINT ( 'NONE',  ( -8.689678022561432513, 1418.698340087812312, 196.3843397762474012 ) ) ;
#2854 = LINE ( 'NONE', #9023, #17151 ) ;
#2855 = CARTESIAN_POINT ( 'NONE',  ( -3.210018582440000046, 1470.482941419229974, 235.1373499011980073 ) ) ;
#2856 = CARTESIAN_POINT ( 'NONE',  ( 6.455447949027460552, 1508.551704612109916, 202.2941920603649919 ) ) ;
#2857 = VERTEX_POINT ( 'NONE', #4258 ) ;
#2859 = EDGE_CURVE ( 'NONE', #36236, #24424, #73680, .T. ) ;
#2858 = AXIS2_PLACEMENT_3D ( 'NONE', #14026, #56057, #90747 ) ;
#2860 = CARTESIAN_POINT ( 'NONE',  ( 11.15489169059999952, 1425.160568487430055, 144.1681086605980227 ) ) ;
#2861 = EDGE_CURVE ( 'NONE', #93671, #44996, #6366, .T. ) ;
#2862 = CARTESIAN_POINT ( 'NONE',  ( 19.37374569213945463, 1524.382868172863937, 234.3668155954418637 ) ) ;
#2863 = CARTESIAN_POINT ( 'NONE',  ( 10.93679547204000002, 1490.434980368090010, 209.9321327948960061 ) ) ;
#2864 = VERTEX_POINT ( 'NONE', #72042 ) ;
#2865 = CARTESIAN_POINT ( 'NONE',  ( 7.324914918154999732, 1516.685667699390024, 204.5043554653269950 ) ) ;
#2866 = ORIENTED_EDGE ( 'NONE', *, *, #53184, .T. ) ;
#2868 = EDGE_CURVE ( 'NONE', #92807, #71088, #52026, .T. ) ;
#2867 = CARTESIAN_POINT ( 'NONE',  ( 11.86420161318850042, 1432.203304325139925, 149.9807413596300023 ) ) ;
#2869 = CARTESIAN_POINT ( 'NONE',  ( 13.39865035957124029, 1444.421645391301581, 187.7321514735085088 ) ) ;
#2870 = ORIENTED_EDGE ( 'NONE', *, *, #97880, .F. ) ;
#2871 = ORIENTED_EDGE ( 'NONE', *, *, #47610, .T. ) ;
#2872 = CARTESIAN_POINT ( 'NONE',  ( 5.370527602886283169, 1422.356908813907012, 139.1416118586824666 ) ) ;
#2873 = EDGE_CURVE ( 'NONE', #49524, #3437, #29264, .T. ) ;
#2874 = CARTESIAN_POINT ( 'NONE',  ( -4.733060768706960353, 1508.551704408389924, 219.7446302201209960 ) ) ;
#2875 = CARTESIAN_POINT ( 'NONE',  ( 10.88110552090000027, 1508.288216035629830, 234.3544958320979958 ) ) ;
#2876 = ADVANCED_FACE ( 'NONE', ( #80412 ), #17111, .F. ) ;
#2877 = VECTOR ( 'NONE', #103941, 1000.000000000000000 ) ;
#2878 = CARTESIAN_POINT ( 'NONE',  ( -4.629079371760130179, 1468.688288304400203, 218.9163698581939741 ) ) ;
#2879 = CARTESIAN_POINT ( 'NONE',  ( 20.20676118117160058, 1452.207424737969859, 143.0075041318320075 ) ) ;
#2880 = CARTESIAN_POINT ( 'NONE',  ( 3.409543808716749780, 1410.339071755739951, 269.6161397029929958 ) ) ;
#2881 = CARTESIAN_POINT ( 'NONE',  ( -108.8461099330000081, 1385.969494106900129, 297.2525754554590094 ) ) ;
#2882 = CARTESIAN_POINT ( 'NONE',  ( -12.69118497449169958, 1502.259178338380025, 210.4948179440679894 ) ) ;
#2883 = CARTESIAN_POINT ( 'NONE',  ( 9.887380464539999636, 1491.508268245589989, 214.0815257268789935 ) ) ;
#2884 = DIRECTION ( 'NONE',  ( 0.9858563016923833633, 0.000000000000000000, 0.1675928173085483863 ) ) ;
#2885 = CARTESIAN_POINT ( 'NONE',  ( 8.814856031159362004, 1424.907964168706485, 195.6717967497336303 ) ) ;
#2886 = EDGE_CURVE ( 'NONE', #77278, #33852, #29899, .T. ) ;
#2888 = CARTESIAN_POINT ( 'NONE',  ( 10.38075141161009896, 1469.469397341999866, 204.6697731946910039 ) ) ;
#2887 = CARTESIAN_POINT ( 'NONE',  ( -15.03612198640000130, 1503.549707945290038, 208.9024357440380015 ) ) ;
#2889 = CARTESIAN_POINT ( 'NONE',  ( -62.71435643172744534, 1379.746901600607089, 270.6043089139369613 ) ) ;
#2890 = CARTESIAN_POINT ( 'NONE',  ( 17.73489863255730015, 1415.061873231259824, 224.9295571200040058 ) ) ;
#2891 = CARTESIAN_POINT ( 'NONE',  ( -7.573276867445001059, 1513.355826799089755, 201.2778793177070042 ) ) ;
#2892 = ORIENTED_EDGE ( 'NONE', *, *, #104822, .F. ) ;
#2893 = CARTESIAN_POINT ( 'NONE',  ( 28.05448519009999941, 1420.250147135629959, 265.6112251771979800 ) ) ;
#2894 = CARTESIAN_POINT ( 'NONE',  ( 13.20531104009999979, 1434.869042435399933, 149.0170821157980185 ) ) ;
#2895 = CARTESIAN_POINT ( 'NONE',  ( -55.66345240404490369, 1385.088922544829984, 273.0910554044640435 ) ) ;
#2896 = CARTESIAN_POINT ( 'NONE',  ( -19.67623451925548039, 1525.581535527370761, 181.0581612214988638 ) ) ;
#2897 = CARTESIAN_POINT ( 'NONE',  ( -8.848347859410001348, 1384.947984491080206, 199.9153136718090025 ) ) ;
#2898 = CARTESIAN_POINT ( 'NONE',  ( 45.63714000780699820, 1434.626146812550132, 268.9747433262190270 ) ) ;
#2899 = EDGE_CURVE ( 'NONE', #36031, #103217, #14727, .T. ) ;
#2901 = VERTEX_POINT ( 'NONE', #12649 ) ;
#2900 = CARTESIAN_POINT ( 'NONE',  ( 12.69572402884860018, 1421.073347931960143, 203.4319052107520349 ) ) ;
#2902 = CARTESIAN_POINT ( 'NONE',  ( -16.57704819438239952, 1418.510437161299933, 202.8789069828859795 ) ) ;
#2903 = CARTESIAN_POINT ( 'NONE',  ( -24.35236995230000190, 1444.655896658020083, 211.1425131463980165 ) ) ;
#2904 = CARTESIAN_POINT ( 'NONE',  ( -2.319649531331190229, 1449.727814782791029, 154.4137922862332459 ) ) ;
#2905 = CARTESIAN_POINT ( 'NONE',  ( -2.381707907557049975, 1429.261286886310018, 200.0546762301680133 ) ) ;
#2906 = CARTESIAN_POINT ( 'NONE',  ( 18.28372774912679688, 1419.974404435409951, 223.2769049341759739 ) ) ;
#2907 = CARTESIAN_POINT ( 'NONE',  ( -10.93437594629999943, 1442.547277881270020, 185.2874795750979899 ) ) ;
#2908 = EDGE_CURVE ( 'NONE', #11508, #65085, #80, .T. ) ;
#2909 = CARTESIAN_POINT ( 'NONE',  ( 30.40044630675230053, 1510.013553480240034, 213.6863598775470052 ) ) ;
#2910 = CARTESIAN_POINT ( 'NONE',  ( -17.17241001986463189, 1523.382868172864164, 238.6251415217917895 ) ) ;
#2911 = CARTESIAN_POINT ( 'NONE',  ( 12.71481701828757949, 1434.614953001262847, 149.3394185820198743 ) ) ;
#2912 = ADVANCED_FACE ( 'NONE', ( #30547 ), #64736, .T. ) ;
#2913 = CARTESIAN_POINT ( 'NONE',  ( 13.93256980790000021, 1412.742330145629921, 228.1707926741980259 ) ) ;
#2914 = CARTESIAN_POINT ( 'NONE',  ( -6.558658715760000035, 1477.685682757989753, 218.2637888529989993 ) ) ;
#2915 = CARTESIAN_POINT ( 'NONE',  ( -15.88332445569999862, 1459.702822082929970, 228.9589543435980090 ) ) ;
#2916 = CARTESIAN_POINT ( 'NONE',  ( 2.863787855735000054, 1516.788317650260069, 207.4054531903269947 ) ) ;
#2917 = CARTESIAN_POINT ( 'NONE',  ( 41.36157324430000415, 1425.216340838630003, 268.6469744794979988 ) ) ;
#2918 = CARTESIAN_POINT ( 'NONE',  ( -17.99881233489999843, 1409.541592764029929, 221.8083273357979976 ) ) ;
#2919 = CARTESIAN_POINT ( 'NONE',  ( 20.43352477559999869, 1435.211929165099946, 143.2813443149979946 ) ) ;
#2920 = ADVANCED_FACE ( 'NONE', ( #14838 ), #57974, .T. ) ;
#2921 = CARTESIAN_POINT ( 'NONE',  ( 20.06092942580000127, 1488.587903410330000, 190.6166884224980151 ) ) ;
#2922 = CARTESIAN_POINT ( 'NONE',  ( 29.22958591724099975, 1509.933780020319773, 206.4713313096740137 ) ) ;
#2923 = CIRCLE ( 'NONE', #49338, 3.500000000000003109 ) ;
#2924 = CARTESIAN_POINT ( 'NONE',  ( -12.31353720152530151, 1377.792119713679995, 208.8773538342209974 ) ) ;
#2925 = CARTESIAN_POINT ( 'NONE',  ( -15.97706642740000227, 1420.887606515729885, 227.0366021596980204 ) ) ;
#2926 = CARTESIAN_POINT ( 'NONE',  ( 32.22536377336282953, 1523.621879633028811, 216.8351145222429466 ) ) ;
#2927 = CARTESIAN_POINT ( 'NONE',  ( -40.67505929589849956, 1440.823025992459861, 136.6075842068449901 ) ) ;
#2928 = CARTESIAN_POINT ( 'NONE',  ( -7.881523990731260199, 1408.659461760370050, 198.0058231072500234 ) ) ;
#2929 = CARTESIAN_POINT ( 'NONE',  ( -15.42144792929999930, 1415.206394609319887, 209.1184241532129988 ) ) ;
#2930 = CARTESIAN_POINT ( 'NONE',  ( -12.80028686799999882, 1442.828808077900021, 186.6514660660979814 ) ) ;
#2931 = CARTESIAN_POINT ( 'NONE',  ( -27.86688904147829859, 1508.626580732350021, 210.5580440514449947 ) ) ;
#2932 = CARTESIAN_POINT ( 'NONE',  ( -30.80657653509999605, 1436.049661374800053, 136.3951857664980025 ) ) ;
#2933 = DIRECTION ( 'NONE',  ( 0.3892484888175031799, -0.9211327884476211425, 0.000000000000000000 ) ) ;
#2934 = ORIENTED_EDGE ( 'NONE', *, *, #96685, .F. ) ;
#2935 = CARTESIAN_POINT ( 'NONE',  ( 5.963459866581566793, 1510.663752950224307, 216.6350338863308309 ) ) ;
#2936 = CARTESIAN_POINT ( 'NONE',  ( -4.827031846966990614, 1409.081624053799942, 223.3000366672669941 ) ) ;
#2937 = CARTESIAN_POINT ( 'NONE',  ( 33.42844755917185751, 1522.382868172863937, 196.1165140606791226 ) ) ;
#2938 = CARTESIAN_POINT ( 'NONE',  ( 17.10989499766859367, 1517.051704408389924, 222.9504516956734506 ) ) ;
#2939 = FACE_OUTER_BOUND ( 'NONE', #88360, .T. ) ;
#2940 = CARTESIAN_POINT ( 'NONE',  ( -42.28308919219999495, 1455.990853814730144, 268.6218227887980561 ) ) ;
#2941 = CARTESIAN_POINT ( 'NONE',  ( -29.75841426815548019, 1525.320827368860364, 196.2321946361128653 ) ) ;
#2942 = CARTESIAN_POINT ( 'NONE',  ( -2.382436964801009083, 1426.901689560119166, 137.0999999980979567 ) ) ;
#2943 = CARTESIAN_POINT ( 'NONE',  ( -26.47494755039999959, 1509.166824640230061, 216.3301573140479945 ) ) ;
#2944 = CARTESIAN_POINT ( 'NONE',  ( -109.1111611177930030, 1384.583257041720117, 311.2497810013429671 ) ) ;
#2945 = CARTESIAN_POINT ( 'NONE',  ( -30.61862460611610359, 1384.969957910880112, 205.9038405460119918 ) ) ;
#2946 = CARTESIAN_POINT ( 'NONE',  ( -5.992819232552549558, 1405.413060387330006, 198.1520639380683235 ) ) ;
#2947 = CARTESIAN_POINT ( 'NONE',  ( 22.52523981570000089, 1509.699659094630078, 227.7647078266979861 ) ) ;
#2948 = CARTESIAN_POINT ( 'NONE',  ( 14.91982466159999987, 1485.050512577729933, 224.1086942190979983 ) ) ;
#2949 = ADVANCED_FACE ( 'NONE', ( #65276 ), #49574, .T. ) ;
#2950 = AXIS2_PLACEMENT_3D ( 'NONE', #40990, #76253, #75169 ) ;
#2951 = CARTESIAN_POINT ( 'NONE',  ( -26.68246396532270026, 1495.347229232020027, 211.0255316263900056 ) ) ;
#2952 = CIRCLE ( 'NONE', #74470, 11.73460161499999899 ) ;
#2953 = DIRECTION ( 'NONE',  ( -3.469446951953611033E-14, 0.000000000000000000, 1.000000000000000000 ) ) ;
#2954 = CARTESIAN_POINT ( 'NONE',  ( -3.567504847130000378, 1508.690878337329877, 180.4372022099980200 ) ) ;
#2955 = CARTESIAN_POINT ( 'NONE',  ( -2.621457251404222255, 1519.551704408389924, 228.0616540033011574 ) ) ;
#2956 = ADVANCED_FACE ( 'NONE', ( #92651 ), #32751, .F. ) ;
#2957 = LINE ( 'NONE', #64506, #87287 ) ;
#2958 = CARTESIAN_POINT ( 'NONE',  ( -11.53430538779999992, 1415.163755998629995, 195.3861979139979894 ) ) ;
#2959 = CARTESIAN_POINT ( 'NONE',  ( -1.920598319070000004, 1420.567467226830104, 193.8392728795989797 ) ) ;
#2960 = CARTESIAN_POINT ( 'NONE',  ( 23.75575072150000011, 1410.664328360029913, 210.9000785660479949 ) ) ;
#2961 = CARTESIAN_POINT ( 'NONE',  ( -107.1805148838380006, 1391.913060387289988, 307.0819323254360143 ) ) ;
#2962 = CARTESIAN_POINT ( 'NONE',  ( -10.00816683080000047, 1449.847106855290122, 190.9047640032989932 ) ) ;
#2963 = CARTESIAN_POINT ( 'NONE',  ( -5.360093979568320677, 1422.720973808630106, 147.5125564607829745 ) ) ;
#2965 = CARTESIAN_POINT ( 'NONE',  ( -12.26059043289999906, 1378.259319071080199, 207.8536745223389914 ) ) ;
#2964 = FACE_OUTER_BOUND ( 'NONE', #105643, .T. ) ;
#2966 = CARTESIAN_POINT ( 'NONE',  ( -5.093520080700000285, 1391.866578459589846, 203.7174121390089852 ) ) ;
#2967 = CARTESIAN_POINT ( 'NONE',  ( -113.4000000000000057, 1377.418846546390114, 293.0440248834589738 ) ) ;
#2968 = CARTESIAN_POINT ( 'NONE',  ( 234.5897387251999930, 11221.53578756869865, -1757.702084499889907 ) ) ;
#2969 = CARTESIAN_POINT ( 'NONE',  ( 19.30421002850018652, 1493.475027096192434, 199.7216057415594719 ) ) ;
#2970 = CARTESIAN_POINT ( 'NONE',  ( -1.288412296889219766, 1419.848508814950264, 185.1203347260929775 ) ) ;
#2971 = EDGE_CURVE ( 'NONE', #6947, #108856, #31094, .T. ) ;
#2972 = CARTESIAN_POINT ( 'NONE',  ( 7.712490952985000980, 1516.666407245520077, 204.5049844236870058 ) ) ;
#2973 = DIRECTION ( 'NONE',  ( -0.000000000000000000, -1.000000000000000000, -0.000000000000000000 ) ) ;
#2974 = CARTESIAN_POINT ( 'NONE',  ( -16.67081401233100024, 1485.422209799639859, 187.9724624971670153 ) ) ;
#2975 = CARTESIAN_POINT ( 'NONE',  ( -7179.982233247708791, -2339.246371527897281, 8259.998446794346819 ) ) ;
#2976 = CARTESIAN_POINT ( 'NONE',  ( -13.81339225453198516, 1421.071880379611684, 210.6281576511377409 ) ) ;
#2978 = ORIENTED_EDGE ( 'NONE', *, *, #90427, .T. ) ;
#2977 = CARTESIAN_POINT ( 'NONE',  ( -67.97495219347740658, 1379.746072679010013, 279.4294113511920159 ) ) ;
#2979 = VERTEX_POINT ( 'NONE', #83162 ) ;
#2980 = CARTESIAN_POINT ( 'NONE',  ( 29.12655685680000062, 1509.869978479729980, 210.7036736057679889 ) ) ;
#2981 = ORIENTED_EDGE ( 'NONE', *, *, #46007, .F. ) ;
#2982 = DIRECTION ( 'NONE',  ( -1.000000000000000000, -0.000000000000000000, -0.000000000000000000 ) ) ;
#2983 = CARTESIAN_POINT ( 'NONE',  ( -109.1312185580000005, 1384.935967175139922, 311.2646235902590206 ) ) ;
#2984 =( BOUNDED_CURVE ( )  B_SPLINE_CURVE ( 3, ( #106814, #3295, #47486, #37427 ),
 .UNSPECIFIED., .F., .F. ) 
 B_SPLINE_CURVE_WITH_KNOTS ( ( 4, 4 ),
 ( 3.106755518160905005, 3.118534288586135350 ),
 .UNSPECIFIED. ) 
 CURVE ( )  GEOMETRIC_REPRESENTATION_ITEM ( )  RATIONAL_B_SPLINE_CURVE ( ( 1.000000000000000000, 0.9999884384140235172, 0.9999884384140235172, 1.000000000000000000 ) ) 
 REPRESENTATION_ITEM ( '' )  );
#2986 = CARTESIAN_POINT ( 'NONE',  ( 24.61702284729999946, 1442.198266432479841, 213.4925807370779864 ) ) ;
#2985 = CARTESIAN_POINT ( 'NONE',  ( 15.88602804442459870, 1417.757759938499930, 191.3037173568610001 ) ) ;
#2987 = CARTESIAN_POINT ( 'NONE',  ( -0.8945946638535250406, 1417.298095655010002, 235.8147265033050246 ) ) ;
#2988 = EDGE_CURVE ( 'NONE', #20697, #36071, #48476, .T. ) ;
#2989 = CARTESIAN_POINT ( 'NONE',  ( -25.31584570420000091, 1451.871603816930246, 136.1751615687979893 ) ) ;
#2990 = CARTESIAN_POINT ( 'NONE',  ( 8.178501070643639181, 1441.152429762079919, 153.9860758848200248 ) ) ;
#2991 = CARTESIAN_POINT ( 'NONE',  ( 5.659654762769999792, 1409.110699888030013, 230.1372059342980094 ) ) ;
#2992 = CARTESIAN_POINT ( 'NONE',  ( 6.561686423234999843, 1517.069378699710114, 212.5741351528070027 ) ) ;
#2993 = CARTESIAN_POINT ( 'NONE',  ( 41.63894744325380515, 1444.312235791039939, 134.0999999983169744 ) ) ;
#2994 = CARTESIAN_POINT ( 'NONE',  ( 2.487935123032369855, 1509.038615930399828, 204.6345961886270004 ) ) ;
#2995 = CARTESIAN_POINT ( 'NONE',  ( -0.5635418445434529078, 1419.788636389980184, 227.8982600517779815 ) ) ;
#2996 = ORIENTED_EDGE ( 'NONE', *, *, #78745, .F. ) ;
#2997 = CARTESIAN_POINT ( 'NONE',  ( -19.86622907060200305, 1443.388380008240119, 213.1207143647550311 ) ) ;
#2998 = EDGE_CURVE ( 'NONE', #65697, #94153, #105190, .T. ) ;
#2999 = CARTESIAN_POINT ( 'NONE',  ( -11.03495751070000175, 1391.553749705140035, 203.9031261639289880 ) ) ;
#3000 = ORIENTED_EDGE ( 'NONE', *, *, #54836, .F. ) ;
#3001 = EDGE_LOOP ( 'NONE', ( #74480, #135, #9524, #81135 ) ) ;
#3002 = VERTEX_POINT ( 'NONE', #82614 ) ;
#3003 = CARTESIAN_POINT ( 'NONE',  ( -7.316722043595000002, 1511.382498894329956, 215.7022088808070066 ) ) ;
#3004 = CARTESIAN_POINT ( 'NONE',  ( -1.499470402960000115, 1465.333991039530019, 236.0689215525979705 ) ) ;
#3005 = CARTESIAN_POINT ( 'NONE',  ( 21.08599079332655890, 1450.945512302869247, 144.3583723772087808 ) ) ;
#3006 = CARTESIAN_POINT ( 'NONE',  ( -8.298094033859999996, 1384.915121724699929, 218.7036151108189870 ) ) ;
#3007 = CARTESIAN_POINT ( 'NONE',  ( -2.031883580139580037, 1464.998375551469962, 198.3053770173009980 ) ) ;
#3008 = CARTESIAN_POINT ( 'NONE',  ( -18.54137802971740001, 1445.596289520634400, 214.4230706237874813 ) ) ;
#3009 = CARTESIAN_POINT ( 'NONE',  ( -68.43938665331394589, 1379.747307078699578, 279.3521370341155148 ) ) ;
#3010 = CARTESIAN_POINT ( 'NONE',  ( 4.254108446939370403, 1446.519541462919960, 160.4550363066709906 ) ) ;
#3011 = ADVANCED_FACE ( 'NONE', ( #66387 ), #102765, .F. ) ;
#3012 = CARTESIAN_POINT ( 'NONE',  ( -4.811461170099283535, 1516.551188146009054, 218.2487618711105313 ) ) ;
#3013 = ORIENTED_EDGE ( 'NONE', *, *, #19215, .F. ) ;
#3014 = CARTESIAN_POINT ( 'NONE',  ( 0.7350231981660010350, 1516.970035769810011, 206.8242163110469960 ) ) ;
#3016 = ORIENTED_EDGE ( 'NONE', *, *, #24009, .F. ) ;
#3015 = B_SPLINE_CURVE_WITH_KNOTS ( 'NONE', 3,
 ( #84972, #110740, #16106, #42999 ),
 .UNSPECIFIED., .F., .F.,
 ( 4, 4 ),
 ( 0.000000000000000000, 0.0002960034161023847310 ),
 .UNSPECIFIED. ) ;
#3017 = CARTESIAN_POINT ( 'NONE',  ( 24.29942712596140098, 1440.913060387330006, 236.7211978293100003 ) ) ;
#3018 = CARTESIAN_POINT ( 'NONE',  ( -15.81194716269999923, 1509.534088746730049, 183.7661278115980110 ) ) ;
#3019 = EDGE_CURVE ( 'NONE', #74254, #18150, #87284, .T. ) ;
#3020 = ORIENTED_EDGE ( 'NONE', *, *, #23524, .F. ) ;
#3021 = CARTESIAN_POINT ( 'NONE',  ( 25.87535885525390000, 1449.883803224160147, 136.9992940508379888 ) ) ;
#3022 = CARTESIAN_POINT ( 'NONE',  ( -14.55035415250000064, 1409.421169950730018, 191.6335217687980048 ) ) ;
#3023 = CARTESIAN_POINT ( 'NONE',  ( -23.99542451635583262, 1379.613613144763121, 214.7981695600689704 ) ) ;
#3025 = CARTESIAN_POINT ( 'NONE',  ( 7.717505752974999744, 1516.857914730730045, 201.4043401791270185 ) ) ;
#3024 = DIRECTION ( 'NONE',  ( -0.8672669759446620663, -1.225281874271767957E-16, 0.4978433412588753049 ) ) ;
#3026 = CARTESIAN_POINT ( 'NONE',  ( 22.53780194058930064, 1411.035674245950077, 206.1988793083210112 ) ) ;
#3027 = CARTESIAN_POINT ( 'NONE',  ( -1.858949912414051386, 1455.785754466377284, 218.4293971133010359 ) ) ;
#3028 = CARTESIAN_POINT ( 'NONE',  ( 1.356522472024429993, 1410.335674015750101, 232.6399073486850000 ) ) ;
#3029 = CARTESIAN_POINT ( 'NONE',  ( -13.50104314780000081, 1434.968970217379820, 148.5641363387979936 ) ) ;
#3030 = CARTESIAN_POINT ( 'NONE',  ( -6.690645534649999782, 1508.290528910890089, 219.9963685916989959 ) ) ;
#3032 = CARTESIAN_POINT ( 'NONE',  ( 18.25280056480000113, 1432.153207019990077, 210.9297336666290050 ) ) ;
#3031 = CARTESIAN_POINT ( 'NONE',  ( 6.227622670500000623, 1464.007336795129959, 235.2942956369979868 ) ) ;
#3033 = CARTESIAN_POINT ( 'NONE',  ( -3.259101837015000225, 1517.102359858469754, 216.0714209178769920 ) ) ;
#3034 = EDGE_CURVE ( 'NONE', #80762, #8717, #17270, .T. ) ;
#3035 = CARTESIAN_POINT ( 'NONE',  ( -31.34491535884016855, 1525.848196786131666, 217.0523381734421662 ) ) ;
#3036 = ADVANCED_FACE ( 'NONE', ( #102150 ), #41040, .F. ) ;
#3037 = CARTESIAN_POINT ( 'NONE',  ( 5.949235695344720298, 1511.655824793919919, 217.4114490419000276 ) ) ;
#3038 = CARTESIAN_POINT ( 'NONE',  ( -3.246772394788723481, 1512.187213306747481, 177.1492560608742224 ) ) ;
#3039 = CARTESIAN_POINT ( 'NONE',  ( 2.492443650904999863, 1516.793978928989873, 212.3737347995770222 ) ) ;
#3040 = CARTESIAN_POINT ( 'NONE',  ( 3.330134165755000097, 1515.051704408389924, 213.4516374609670208 ) ) ;
#3041 = CARTESIAN_POINT ( 'NONE',  ( -4.853142760347620488, 1483.079447084539879, 199.6457431982469757 ) ) ;
#3043 = ORIENTED_EDGE ( 'NONE', *, *, #45218, .T. ) ;
#3042 = CARTESIAN_POINT ( 'NONE',  ( -75.53845940079999366, 1389.374618531590158, 296.9084575487589746 ) ) ;
#3044 = CARTESIAN_POINT ( 'NONE',  ( -17.50742245788202922, 1524.972383263453139, 237.3784165796199375 ) ) ;
#3045 = CARTESIAN_POINT ( 'NONE',  ( 24.64758684679999945, 1455.655050828230060, 240.2509105760980219 ) ) ;
#3046 = CARTESIAN_POINT ( 'NONE',  ( 29.00779973304128134, 1526.382868172864164, 217.2942086403122630 ) ) ;
#3047 = CARTESIAN_POINT ( 'NONE',  ( -25.94248324348950163, 1509.818991864719919, 222.8344883908499980 ) ) ;
#3048 = CARTESIAN_POINT ( 'NONE',  ( -21.60894078472486868, 1517.051704408389924, 199.6722430288449175 ) ) ;
#3049 = ADVANCED_FACE ( 'NONE', ( #13044 ), #33926, .F. ) ;
#3050 = CARTESIAN_POINT ( 'NONE',  ( -20.89412605160000069, 1454.104942495830073, 223.6452089798980012 ) ) ;
#3052 = CARTESIAN_POINT ( 'NONE',  ( 5.386275313190370007, 1432.307805056000007, 154.6069887461920018 ) ) ;
#3051 = CARTESIAN_POINT ( 'NONE',  ( 10.97117078989999861, 1432.448750475399947, 151.7701039698980026 ) ) ;
#3053 = CARTESIAN_POINT ( 'NONE',  ( -9.173772188490959323, 1450.560542621009972, 208.1432906865220218 ) ) ;
#3054 = CARTESIAN_POINT ( 'NONE',  ( -105.4833704291039993, 1380.472658686770046, 307.8541256062359821 ) ) ;
#3055 = ORIENTED_EDGE ( 'NONE', *, *, #108341, .F. ) ;
#3056 = CARTESIAN_POINT ( 'NONE',  ( -2.877113108595000135, 1516.697242742309982, 204.1252037719370094 ) ) ;
#3057 = CARTESIAN_POINT ( 'NONE',  ( 0.5545655831749999320, 1406.267234724929949, 269.2946136120979759 ) ) ;
#3058 = EDGE_CURVE ( 'NONE', #99066, #109412, #62977, .T. ) ;
#3059 = CARTESIAN_POINT ( 'NONE',  ( 0.7244299515159999814, 1515.369718807090067, 213.4098813832590054 ) ) ;
#3060 = CARTESIAN_POINT ( 'NONE',  ( 38.52648929541060596, 1455.895828382030004, 270.1643681006679572 ) ) ;
#3061 = CARTESIAN_POINT ( 'NONE',  ( 5.519877061429999898, 1440.499830656789982, 154.7645262406979896 ) ) ;
#3062 = CARTESIAN_POINT ( 'NONE',  ( 11.60004869885203682, 1425.894345409931248, 137.5113366366250034 ) ) ;
#3063 = B_SPLINE_CURVE_WITH_KNOTS ( 'NONE', 3,
 ( #18293, #2092, #52486, #79334, #86614, #10462, #88280, #44077, #19395, #77671, #44636, #78777 ),
 .UNSPECIFIED., .F., .F.,
 ( 4, 2, 2, 2, 2, 4 ),
 ( -0.1123552135074580016, -0.09789198044012829836, -0.08346214397256018769, -0.05408911794985069715, -0.02844460996696679400, -2.821931098934138404E-07 ),
 .UNSPECIFIED. ) ;
#3064 = CARTESIAN_POINT ( 'NONE',  ( -36.36844575302269789, 1440.913060387330006, 253.5188197989739933 ) ) ;
#3065 = CARTESIAN_POINT ( 'NONE',  ( -25.71870319980000019, 1450.791960742989886, 136.8495502446980083 ) ) ;
#3066 = CARTESIAN_POINT ( 'NONE',  ( 3.322123243643906765, 1445.528383361184751, 200.7448775392205675 ) ) ;
#3067 = DIRECTION ( 'NONE',  ( 0.8775825618903732028, -4.965288137873349002E-32, 0.4794255386042021172 ) ) ;
#3068 = CARTESIAN_POINT ( 'NONE',  ( 1.459574821760450059, 1450.689303316930136, 154.7904039106100242 ) ) ;
#3069 = AXIS2_PLACEMENT_3D ( 'NONE', #84795, #58524, #49027 ) ;
#3070 = CARTESIAN_POINT ( 'NONE',  ( -1.544604216069999980, 1508.025075525790044, 220.8982248008990155 ) ) ;
#3071 = CARTESIAN_POINT ( 'NONE',  ( -1.546949757679999760, 1416.828040475729949, 228.0209010782980101 ) ) ;
#3072 = VERTEX_POINT ( 'NONE', #38264 ) ;
#3073 = CARTESIAN_POINT ( 'NONE',  ( -22.74199304079999706, 1435.511682894840078, 234.3916895436979928 ) ) ;
#3074 = CARTESIAN_POINT ( 'NONE',  ( 2.315006021250000323, 1485.018218158490072, 198.6293828328989832 ) ) ;
#3075 = CARTESIAN_POINT ( 'NONE',  ( 10.16195519437919970, 1469.411650742470101, 205.1025830150449849 ) ) ;
#3076 = CARTESIAN_POINT ( 'NONE',  ( -1.333808752909999784, 1476.063104645729936, 267.5364536224980156 ) ) ;
#3077 = CARTESIAN_POINT ( 'NONE',  ( 3.092030599670000157, 1499.597189252489898, 201.0134171835890129 ) ) ;
#3078 = CARTESIAN_POINT ( 'NONE',  ( -27.93158978740000009, 1508.017348977630036, 210.2982006691480024 ) ) ;
#3079 = CARTESIAN_POINT ( 'NONE',  ( 7.500055757779999333, 1423.184307743249974, 213.6185429247490219 ) ) ;
#3080 = CARTESIAN_POINT ( 'NONE',  ( -26.69200297127330046, 1384.840286869720103, 224.9839128895910108 ) ) ;
#3081 = VECTOR ( 'NONE', #105652, 999.9999999999998863 ) ;
#3082 = CARTESIAN_POINT ( 'NONE',  ( -18.79647799810000208, 1416.822690122329959, 208.4084635082059833 ) ) ;
#3083 = CARTESIAN_POINT ( 'NONE',  ( -11.10658002539999956, 1483.002145788689859, 204.7825228467889929 ) ) ;
#3084 = CARTESIAN_POINT ( 'NONE',  ( 26.56954545285969616, 1436.266953136529992, 136.6620164141489795 ) ) ;
#3085 = CARTESIAN_POINT ( 'NONE',  ( -10.84999001794609974, 1396.291950387739917, 211.3263223283950083 ) ) ;
#3086 = CARTESIAN_POINT ( 'NONE',  ( -15.81043287432200017, 1421.035995845646084, 227.0411833758840032 ) ) ;
#3087 = CARTESIAN_POINT ( 'NONE',  ( -16.59998697850549831, 1410.444752549930172, 226.4425751357730121 ) ) ;
#3088 = CARTESIAN_POINT ( 'NONE',  ( -45.62036884359999789, 1439.936247324329770, 268.9752023951979822 ) ) ;
#3089 = EDGE_LOOP ( 'NONE', ( #34929, #47856, #37715, #44340, #103281 ) ) ;
#3090 = CARTESIAN_POINT ( 'NONE',  ( -11.33134919748442471, 1502.978141622408202, 207.0767717826675209 ) ) ;
#3091 = CARTESIAN_POINT ( 'NONE',  ( -13.58559797177369965, 1508.489012943990019, 209.9933550906049788 ) ) ;
#3092 = DIRECTION ( 'NONE',  ( 0.000000000000000000, -1.000000000000000000, -0.000000000000000000 ) ) ;
#3094 = CARTESIAN_POINT ( 'NONE',  ( -12.61087486066499785, 1512.195694528090144, 194.0417079242670013 ) ) ;
#3093 = CARTESIAN_POINT ( 'NONE',  ( 11.17341440289999888, 1425.629743028729990, 126.2832056323980083 ) ) ;
#3095 = CARTESIAN_POINT ( 'NONE',  ( -2.562340869413342048, 1522.051704408389924, 196.2891841806521711 ) ) ;
#3096 = CARTESIAN_POINT ( 'NONE',  ( -14.31906343784990021, 1380.323795378649947, 209.9058136714729983 ) ) ;
#3097 = CARTESIAN_POINT ( 'NONE',  ( -2.872700555325000238, 1516.559109716219837, 201.4121646638069763 ) ) ;
#3098 = CARTESIAN_POINT ( 'NONE',  ( 7.897123973650000295, 1424.702922360419961, 211.7415114879590021 ) ) ;
#3100 = CARTESIAN_POINT ( 'NONE',  ( -11.86716023049999968, 1432.353341358199941, 147.6509521729980179 ) ) ;
#3099 = CIRCLE ( 'NONE', #17334, 1.999999999999999556 ) ;
#3101 = CARTESIAN_POINT ( 'NONE',  ( 7.312123808780000012, 1507.578463809529921, 182.6814736750980046 ) ) ;
#3102 = CARTESIAN_POINT ( 'NONE',  ( 7.575166919095000395, 1511.422242621320265, 206.4203055568870013 ) ) ;
#3103 = CARTESIAN_POINT ( 'NONE',  ( -76.47832706378659395, 1379.656496316390076, 293.1148347572179773 ) ) ;
#3104 = CARTESIAN_POINT ( 'NONE',  ( 7.818221670759999853, 1367.736483592530021, 207.6218459616989946 ) ) ;
#3106 = ORIENTED_EDGE ( 'NONE', *, *, #105951, .T. ) ;
#3105 = CARTESIAN_POINT ( 'NONE',  ( 7.892605823620001182, 1452.443926081389918, 214.1248619204189936 ) ) ;
#3107 = VERTEX_POINT ( 'NONE', #106040 ) ;
#3108 = DIRECTION ( 'NONE',  ( 1.000000000000000000, 0.000000000000000000, 0.000000000000000000 ) ) ;
#3109 = FACE_OUTER_BOUND ( 'NONE', #94071, .T. ) ;
#3110 = DIRECTION ( 'NONE',  ( -0.9510565162951566398, 0.000000000000000000, -0.3090169943749383474 ) ) ;
#3111 = CARTESIAN_POINT ( 'NONE',  ( -7.848179713114999956, 1511.193640125469983, 213.6447370295169890 ) ) ;
#3113 = CARTESIAN_POINT ( 'NONE',  ( -113.4000000000000057, 1306.483669372790018, 310.9930631313190474 ) ) ;
#3112 = CARTESIAN_POINT ( 'NONE',  ( -8.737946438520001635, 1383.987033302019881, 218.5474386001390030 ) ) ;
#3114 = ADVANCED_FACE ( 'NONE', ( #29317 ), #55103, .T. ) ;
#3115 = CARTESIAN_POINT ( 'NONE',  ( -32.06267705388219014, 1524.739563915922645, 202.1338641996698016 ) ) ;
#3116 = CARTESIAN_POINT ( 'NONE',  ( 13.15366522099999891, 1428.703228679929907, 223.0784815109979888 ) ) ;
#3117 = CARTESIAN_POINT ( 'NONE',  ( -40.26396339707969219, 1444.186527608570032, 137.1012300132789790 ) ) ;
#3118 = B_SPLINE_CURVE_WITH_KNOTS ( 'NONE', 5,
 ( #70328, #25504, #77046, #59694, #60814, #34479 ),
 .UNSPECIFIED., .F., .F.,
 ( 6, 6 ),
 ( 0.000000000000000000, 1.000000000000000000 ),
 .UNSPECIFIED. ) ;
#3119 = CARTESIAN_POINT ( 'NONE',  ( -2.500000000000000000, 1448.375148597939869, 162.6885153068710110 ) ) ;
#3120 = CARTESIAN_POINT ( 'NONE',  ( 26.79414481833639883, 1435.433178084320161, 135.2874577367330176 ) ) ;
#3121 = FACE_OUTER_BOUND ( 'NONE', #50968, .T. ) ;
#3122 = CARTESIAN_POINT ( 'NONE',  ( -3.804492251863449859, 1406.371137055889903, 269.2897714392109947 ) ) ;
#3123 = CARTESIAN_POINT ( 'NONE',  ( -18.64588652299999794, 1416.828040475229955, 208.5593769277110141 ) ) ;
#3124 = ORIENTED_EDGE ( 'NONE', *, *, #73570, .F. ) ;
#3125 = CARTESIAN_POINT ( 'NONE',  ( 4.095657388320000258, 1423.950325605830130, 183.4778182170979903 ) ) ;
#3126 = CARTESIAN_POINT ( 'NONE',  ( 12.24860663770000002, 1442.680101602390096, 186.9125332272980131 ) ) ;
#3127 = ORIENTED_EDGE ( 'NONE', *, *, #89493, .F. ) ;
#3128 = ORIENTED_EDGE ( 'NONE', *, *, #24699, .T. ) ;
#3129 = CARTESIAN_POINT ( 'NONE',  ( -3.389499785119999942, 1455.558962287190070, 200.3052658018689840 ) ) ;
#3130 = CARTESIAN_POINT ( 'NONE',  ( -2.380813228419999650, 1360.502616939890004, 207.6218459616989946 ) ) ;
#3131 = CIRCLE ( 'NONE', #24488, 0.4999999999999980016 ) ;
#3132 = CARTESIAN_POINT ( 'NONE',  ( -7.325541825264999751, 1516.710692850270107, 214.1269169785269924 ) ) ;
#3133 = CARTESIAN_POINT ( 'NONE',  ( 4.813011385984999890, 1510.693074690949970, 216.6779200322870054 ) ) ;
#3134 = ORIENTED_EDGE ( 'NONE', *, *, #50453, .T. ) ;
#3135 = CARTESIAN_POINT ( 'NONE',  ( 7.901854723500001398, 1423.732064818020035, 212.4548200391890020 ) ) ;
#3136 = CARTESIAN_POINT ( 'NONE',  ( -94.75917112700000189, 1379.224093153639842, 301.3391293692590125 ) ) ;
#3137 = CARTESIAN_POINT ( 'NONE',  ( -105.8293410826149881, 1378.913060387450059, 303.6100817853489957 ) ) ;
#3138 = CARTESIAN_POINT ( 'NONE',  ( -0.01322039564809850132, 1516.939819969850078, 205.0847949345169923 ) ) ;
#3139 = EDGE_CURVE ( 'NONE', #70769, #106306, #40471, .T. ) ;
#3140 = CARTESIAN_POINT ( 'NONE',  ( -41.02245140317685212, 1434.148376033890372, 269.6289973472830184 ) ) ;
#3141 = CARTESIAN_POINT ( 'NONE',  ( 0.7403205670290020635, 1517.139320148880188, 201.3969713189170250 ) ) ;
#3142 = CARTESIAN_POINT ( 'NONE',  ( -9.486449742109998695, 1409.244334512030036, 228.2930016836979803 ) ) ;
#3143 = EDGE_CURVE ( 'NONE', #8260, #27116, #82750, .T. ) ;
#3145 = ORIENTED_EDGE ( 'NONE', *, *, #8545, .T. ) ;
#3144 = CARTESIAN_POINT ( 'NONE',  ( -8.965713971590000497, 1447.579297599270149, 186.2691576776979900 ) ) ;
#3146 = DIRECTION ( 'NONE',  ( 0.000000000000000000, 0.000000000000000000, 1.000000000000000000 ) ) ;
#3147 = CARTESIAN_POINT ( 'NONE',  ( 4.326992699989999913, 1515.158586642790169, 209.1218459614979963 ) ) ;
#3149 = CARTESIAN_POINT ( 'NONE',  ( -3.078458293690000236, 1384.210421809239961, 218.5154548192989807 ) ) ;
#3148 = CIRCLE ( 'NONE', #17389, 1.000000000000000888 ) ;
#3150 = CARTESIAN_POINT ( 'NONE',  ( 15.56138138183905362, 1506.691119442913987, 224.9532563058226913 ) ) ;
#3151 = ADVANCED_FACE ( 'NONE', ( #91438 ), #28602, .F. ) ;
#3152 = CARTESIAN_POINT ( 'NONE',  ( 27.75956368386599848, 1417.581732837509890, 269.7078427950669948 ) ) ;
#3153 = CARTESIAN_POINT ( 'NONE',  ( -4.609996619675000851, 1516.769879638719885, 212.5810025483170023 ) ) ;
#3154 = CARTESIAN_POINT ( 'NONE',  ( -65.39677373169999441, 1379.739124186490017, 273.1945630607590374 ) ) ;
#3155 = CIRCLE ( 'NONE', #72836, 1.999999999999998668 ) ;
#3156 = ADVANCED_FACE ( 'NONE', ( #5221 ), #75032, .T. ) ;
#3157 = CARTESIAN_POINT ( 'NONE',  ( 0.01643980240737619863, 1507.683248503670711, 237.4603286191148754 ) ) ;
#3158 = CARTESIAN_POINT ( 'NONE',  ( -30.95265250778393806, 1524.659148609483054, 221.7851970717786685 ) ) ;
#3159 = CARTESIAN_POINT ( 'NONE',  ( 18.70421975728147501, 1410.928392002681903, 194.6991403882563532 ) ) ;
#3160 = CARTESIAN_POINT ( 'NONE',  ( 0.7533003524100010395, 1516.992029636990083, 209.8620668306199946 ) ) ;
#3161 = ORIENTED_EDGE ( 'NONE', *, *, #108302, .T. ) ;
#3162 = CARTESIAN_POINT ( 'NONE',  ( 0.1179895432987919934, 1424.305365874710105, 227.5542676486180085 ) ) ;
#3163 = CARTESIAN_POINT ( 'NONE',  ( -6.550474571240000543, 1420.442131291729993, 231.7423262060979994 ) ) ;
#3164 = CARTESIAN_POINT ( 'NONE',  ( -102.7364477239999871, 1384.825249911479887, 311.2346497062589492 ) ) ;
#3165 = VERTEX_POINT ( 'NONE', #86883 ) ;
#3166 = CARTESIAN_POINT ( 'NONE',  ( -36.10181457510150693, 1385.203388602290033, 235.7704352495559874 ) ) ;
#3167 = CARTESIAN_POINT ( 'NONE',  ( -4.730384175031817406, 1508.603735226452955, 206.6339107270123066 ) ) ;
#3168 = CARTESIAN_POINT ( 'NONE',  ( 2.816976817413889833, 1488.404750540059922, 235.1213689463969843 ) ) ;
#3169 = CARTESIAN_POINT ( 'NONE',  ( -24.04894046811064712, 1437.994949862434623, 211.5653030982465452 ) ) ;
#3170 = DIRECTION ( 'NONE',  ( -0.9076061524720632212, 0.000000000000000000, 0.4198226673190215696 ) ) ;
#3171 = CARTESIAN_POINT ( 'NONE',  ( -0.1980233633810000171, 1409.427787100730029, 233.0227887172979990 ) ) ;
#3172 = CARTESIAN_POINT ( 'NONE',  ( -0.05438287574095269916, 1420.446865887249942, 182.6846654475669993 ) ) ;
#3174 = CARTESIAN_POINT ( 'NONE',  ( 21.53981368633951377, 1523.542365884048422, 183.9340804168593309 ) ) ;
#3173 = CARTESIAN_POINT ( 'NONE',  ( -5.777745433405000242, 1516.908489800550115, 215.6797558528670038 ) ) ;
#3175 = CARTESIAN_POINT ( 'NONE',  ( -5.789140635075909813, 1391.897372272190069, 215.0545055588169987 ) ) ;
#3176 = CARTESIAN_POINT ( 'NONE',  ( 10.51972982329080075, 1470.321793319200196, 208.5210859618010204 ) ) ;
#3177 = VECTOR ( 'NONE', #85229, 1000.000000000000000 ) ;
#3178 = VERTEX_POINT ( 'NONE', #51640 ) ;
#3179 = CARTESIAN_POINT ( 'NONE',  ( 0.7403205670290020635, 1517.139320148880188, 201.3969713189170250 ) ) ;
#3181 = EDGE_CURVE ( 'NONE', #93757, #70633, #100209, .T. ) ;
#3180 = ADVANCED_FACE ( 'NONE', ( #153 ), #68846, .T. ) ;
#3182 = DIRECTION ( 'NONE',  ( -0.5877852522924562617, 0.000000000000000000, 0.8090169943749596637 ) ) ;
#3183 = ORIENTED_EDGE ( 'NONE', *, *, #94264, .T. ) ;
#3184 = CARTESIAN_POINT ( 'NONE',  ( -0.1710941967680000009, 1506.802866821829866, 231.3049357514979931 ) ) ;
#3185 = B_SPLINE_CURVE_WITH_KNOTS ( 'NONE', 5,
 ( #15559, #100143, #57065, #64360, #30728, #81128, #91190, #99024, #4446, #38573, #82238, #56502 ),
 .UNSPECIFIED., .F., .F.,
 ( 6, 3, 3, 6 ),
 ( 0.000000000000000000, 0.4244931604951553972, 0.5659654508551994478, 1.000000000000000000 ),
 .UNSPECIFIED. ) ;
#3186 = CARTESIAN_POINT ( 'NONE',  ( 4.771249618659999747, 1425.961663979450122, 210.6061160235690295 ) ) ;
#3187 = EDGE_CURVE ( 'NONE', #62493, #65430, #7980, .T. ) ;
#3188 = CARTESIAN_POINT ( 'NONE',  ( 7.946349138541700441, 1511.532396045849964, 203.1959877047910084 ) ) ;
#3189 = CARTESIAN_POINT ( 'NONE',  ( 2.967450459799999773, 1441.849466645390066, 217.8449471930090056 ) ) ;
#3190 = CARTESIAN_POINT ( 'NONE',  ( -26.50966091029689764, 1508.705881461730087, 201.4781748968639761 ) ) ;
#3191 = CARTESIAN_POINT ( 'NONE',  ( 19.39445793089999981, 1410.873186823329888, 196.0569557394979938 ) ) ;
#3192 = FACE_OUTER_BOUND ( 'NONE', #35869, .T. ) ;
#3193 = CARTESIAN_POINT ( 'NONE',  ( -17.73224984459999831, 1423.865196787429795, 226.2326530843979810 ) ) ;
#3194 = CARTESIAN_POINT ( 'NONE',  ( -23.11088550610000070, 1435.448731366229822, 140.2466043785979934 ) ) ;
#3195 = CARTESIAN_POINT ( 'NONE',  ( -4.906228319039999342, 1433.447543843880112, 150.0987928807979870 ) ) ;
#3196 = CARTESIAN_POINT ( 'NONE',  ( -111.2060435952740676, 1390.913060387289988, 303.0232821107484824 ) ) ;
#3198 = CARTESIAN_POINT ( 'NONE',  ( -17.29007009959331143, 1433.653063861127976, 216.8064808204674421 ) ) ;
#3197 = CARTESIAN_POINT ( 'NONE',  ( 0.6901592941706589102, 1408.937161280970031, 231.9235919190410300 ) ) ;
#3199 = CARTESIAN_POINT ( 'NONE',  ( 20.49831092009999978, 1496.178973653789853, 204.1013708937389879 ) ) ;
#3200 = EDGE_LOOP ( 'NONE', ( #15746, #77246, #26481, #24802 ) ) ;
#3201 = DIRECTION ( 'NONE',  ( 0.02616798426500965835, 0.9993150019883683122, -0.02616798426500970692 ) ) ;
#3202 = CARTESIAN_POINT ( 'NONE',  ( 4.987078416414999715, 1508.551704408389924, 212.6094384009469707 ) ) ;
#3203 = CIRCLE ( 'NONE', #6681, 1.999999999999999556 ) ;
#3204 = CARTESIAN_POINT ( 'NONE',  ( -23.95903483410000234, 1435.875769846390085, 211.1525007611679712 ) ) ;
#3205 = CARTESIAN_POINT ( 'NONE',  ( -3.235066836120000122, 1485.183772486390126, 198.0938001695989783 ) ) ;
#3206 = CARTESIAN_POINT ( 'NONE',  ( -18.59896194139999892, 1509.326147591629933, 230.4813394039980210 ) ) ;
#3207 = CARTESIAN_POINT ( 'NONE',  ( -2.389870119416070082, 1525.253996226948402, 242.0501772481331386 ) ) ;
#3208 = CARTESIAN_POINT ( 'NONE',  ( -17.33645362950000290, 1414.996442546130083, 207.8511177337479978 ) ) ;
#3209 = CYLINDRICAL_SURFACE ( 'NONE', #54484, 1.000000000000000888 ) ;
#3210 = CARTESIAN_POINT ( 'NONE',  ( -8.304037367963141847, 1489.233820626979877, 216.5016543136719918 ) ) ;
#3211 = CARTESIAN_POINT ( 'NONE',  ( -21.51338718909140013, 1505.551624535830115, 209.1218323743090082 ) ) ;
#3212 = CARTESIAN_POINT ( 'NONE',  ( -93.31501789313530537, 1383.768231546839843, 309.4758065345690170 ) ) ;
#3213 = FACE_OUTER_BOUND ( 'NONE', #87331, .T. ) ;
#3214 = CARTESIAN_POINT ( 'NONE',  ( -5.171974582749985672, 1391.896122674977278, 214.5527304933138737 ) ) ;
#3215 = CARTESIAN_POINT ( 'NONE',  ( 6.732768143660000426, 1427.455436918209898, 213.9186140547390096 ) ) ;
#3217 = VERTEX_POINT ( 'NONE', #11300 ) ;
#3216 = CARTESIAN_POINT ( 'NONE',  ( 20.60471804940000240, 1508.365513109829863, 189.9195030953979710 ) ) ;
#3218 = B_SPLINE_CURVE_WITH_KNOTS ( 'NONE', 3,
 ( #27078, #69654, #94819, #779, #62355, #77478 ),
 .UNSPECIFIED., .F., .F.,
 ( 4, 2, 4 ),
 ( -0.08353783071465489818, -0.08289724164866060785, -0.08222331866850060567 ),
 .UNSPECIFIED. ) ;
#3219 = CARTESIAN_POINT ( 'NONE',  ( -84.23427087509999467, 1380.672444284130052, 291.6063032490590103 ) ) ;
#3220 = CYLINDRICAL_SURFACE ( 'NONE', #35381, 3.999999999999993339 ) ;
#3221 = ORIENTED_EDGE ( 'NONE', *, *, #85035, .T. ) ;
#3222 = ORIENTED_EDGE ( 'NONE', *, *, #102846, .T. ) ;
#3223 = CARTESIAN_POINT ( 'NONE',  ( 27.68253994085160130, 1507.989615297080036, 207.6661388942010262 ) ) ;
#3224 = CARTESIAN_POINT ( 'NONE',  ( -109.8949053929999877, 1384.921907949040133, 297.0284378280589976 ) ) ;
#3225 = CARTESIAN_POINT ( 'NONE',  ( 12.58542764725278396, 1442.782369552073305, 169.4702723407457370 ) ) ;
#3227 = CARTESIAN_POINT ( 'NONE',  ( 3.493530715499999673E-09, 1465.143864312329924, 238.2947549826980094 ) ) ;
#3226 = CARTESIAN_POINT ( 'NONE',  ( 33.74927008391222216, 1422.757720856681317, 269.5148346472382173 ) ) ;
#3228 = CARTESIAN_POINT ( 'NONE',  ( -19.92516257929999668, 1505.117484763329912, 189.0508382488979748 ) ) ;
#3229 = CARTESIAN_POINT ( 'NONE',  ( -11.37747002660000106, 1433.840278266459791, 151.4434446340980003 ) ) ;
#3230 = CARTESIAN_POINT ( 'NONE',  ( 28.18475875730000269, 1509.897293851330005, 206.0721245515180158 ) ) ;
#3231 = CARTESIAN_POINT ( 'NONE',  ( -19.57242333670000178, 1486.003043799229999, 190.0103911238980174 ) ) ;
#3232 = CARTESIAN_POINT ( 'NONE',  ( 12.57381168289999884, 1409.852089639629867, 190.4288237261979759 ) ) ;
#3233 = CARTESIAN_POINT ( 'NONE',  ( 5.138704292839999965, 1423.280612878629881, 185.3401477795979986 ) ) ;
#3234 = CARTESIAN_POINT ( 'NONE',  ( -24.36523719230000040, 1440.927839248139890, 211.6868766829179833 ) ) ;
#3235 = CARTESIAN_POINT ( 'NONE',  ( 6.070028637900000135, 1440.055554934649763, 154.5780772664979850 ) ) ;
#3236 = DIRECTION ( 'NONE',  ( 1.000000000000000000, 0.000000000000000000, 0.000000000000000000 ) ) ;
#3237 = VECTOR ( 'NONE', #94239, 1000.000000000000000 ) ;
#3238 = CARTESIAN_POINT ( 'NONE',  ( -6.229759787779999947, 1452.550331331829966, 152.9826722968979880 ) ) ;
#3240 = ORIENTED_EDGE ( 'NONE', *, *, #58344, .F. ) ;
#3239 = CYLINDRICAL_SURFACE ( 'NONE', #30010, 0.9999999999999943379 ) ;
#3241 = ORIENTED_EDGE ( 'NONE', *, *, #26966, .F. ) ;
#3242 = CARTESIAN_POINT ( 'NONE',  ( -3.961806501176829975, 1508.551704407889929, 213.6667149433449993 ) ) ;
#3243 = VECTOR ( 'NONE', #20861, 1000.000000000000000 ) ;
#3244 = CARTESIAN_POINT ( 'NONE',  ( -17.92831943059999844, 1489.596456395790028, 195.2426190332990075 ) ) ;
#3245 = CARTESIAN_POINT ( 'NONE',  ( -28.88176192769999773, 1466.008130076530051, 270.2667557415980468 ) ) ;
#3246 = CARTESIAN_POINT ( 'NONE',  ( -7.500000019064998469, 1516.801704408389924, 209.1218459511669892 ) ) ;
#3247 = CARTESIAN_POINT ( 'NONE',  ( 7.549516567449999513E-15, 1441.600846913620217, 155.7224805731980268 ) ) ;
#3248 = CARTESIAN_POINT ( 'NONE',  ( -22.60252397918324618, 1411.062741196104980, 211.6173965618407351 ) ) ;
#3249 = B_SPLINE_CURVE_WITH_KNOTS ( 'NONE', 3,
 ( #35085, #45171, #87150, #51903, #79312, #36748, #70941, #77107, #78191, #93876 ),
 .UNSPECIFIED., .F., .F.,
 ( 4, 3, 3, 4 ),
 ( -157.4228417709999803, -134.4932908349400122, -78.88178533201940468, -29.50720979964130208 ),
 .UNSPECIFIED. ) ;
#3250 = CARTESIAN_POINT ( 'NONE',  ( 4.328687482160760602, 1515.093865522929946, 210.3164017889689887 ) ) ;
#3251 = CARTESIAN_POINT ( 'NONE',  ( -13.27194800760000071, 1421.356218534429900, 229.3113483544979943 ) ) ;
#3252 = CARTESIAN_POINT ( 'NONE',  ( -7.055457375169999601, 1459.495818635790101, 217.3326011958589845 ) ) ;
#3253 = CARTESIAN_POINT ( 'NONE',  ( 7.877099145829999038, 1362.118768394180051, 207.6218459616989946 ) ) ;
#3254 = CARTESIAN_POINT ( 'NONE',  ( -45.16571290676200334, 1435.656948718850117, 266.2028280709869819 ) ) ;
#3255 = ORIENTED_EDGE ( 'NONE', *, *, #26901, .F. ) ;
#3256 = CARTESIAN_POINT ( 'NONE',  ( -8.818304860959999658, 1423.702314450679978, 208.5313052791129849 ) ) ;
#3257 = ORIENTED_EDGE ( 'NONE', *, *, #89991, .F. ) ;
#3258 = CARTESIAN_POINT ( 'NONE',  ( 1.137296650804999976, 1516.908147884120126, 210.8236964273370120 ) ) ;
#3259 = CYLINDRICAL_SURFACE ( 'NONE', #34042, 1.999999999999913181 ) ;
#3260 = CIRCLE ( 'NONE', #56869, 1.999998625699862753 ) ;
#3261 = DIRECTION ( 'NONE',  ( 0.000000000000000000, 4.493040424372315268E-15, -1.000000000000000000 ) ) ;
#3262 = CARTESIAN_POINT ( 'NONE',  ( -4.228066225910000142, 1425.410669922729767, 186.1178616580979792 ) ) ;
#3263 = CARTESIAN_POINT ( 'NONE',  ( 4.163336342339999869E-15, 1416.177402202029953, 209.1218459616989946 ) ) ;
#3264 = ORIENTED_EDGE ( 'NONE', *, *, #59650, .F. ) ;
#3265 = CARTESIAN_POINT ( 'NONE',  ( 3.628818056492709943, 1505.602008419380127, 221.3635114792730292 ) ) ;
#3266 = CARTESIAN_POINT ( 'NONE',  ( 5.778999773775000293, 1516.955859323880077, 201.7887757972170277 ) ) ;
#3267 = ADVANCED_FACE ( 'NONE', ( #108507 ), #46009, .F. ) ;
#3268 = CARTESIAN_POINT ( 'NONE',  ( 9.374255435350001164, 1470.737626183290104, 212.9758214168889765 ) ) ;
#3269 = CARTESIAN_POINT ( 'NONE',  ( -9.907124821256790170, 1439.782531377399891, 207.6975214335770090 ) ) ;
#3270 = ORIENTED_EDGE ( 'NONE', *, *, #22830, .T. ) ;
#3271 = CARTESIAN_POINT ( 'NONE',  ( -12.98904541243399891, 1411.656893195809971, 269.6326585443520116 ) ) ;
#3272 = CARTESIAN_POINT ( 'NONE',  ( 1.715109447055000125, 1516.963431999339946, 209.8570730874349977 ) ) ;
#3273 = CARTESIAN_POINT ( 'NONE',  ( 2.895864789156030294, 1417.780720963150088, 233.2805537130719813 ) ) ;
#3274 = CARTESIAN_POINT ( 'NONE',  ( 8.957671594842102181, 1435.649687873459925, 208.1941622349180250 ) ) ;
#3276 = EDGE_LOOP ( 'NONE', ( #55028, #24641, #38474, #82690, #56008, #92096, #97428 ) ) ;
#3275 = CARTESIAN_POINT ( 'NONE',  ( -4.710894888870413411, 1366.841595974748316, 209.6218459617148824 ) ) ;
#3277 = ORIENTED_EDGE ( 'NONE', *, *, #64427, .F. ) ;
#3278 = CARTESIAN_POINT ( 'NONE',  ( 42.20684054510284255, 1453.921873302082531, 269.0702141739801618 ) ) ;
#3279 = CARTESIAN_POINT ( 'NONE',  ( 2.170280451284099854, 1466.842894365370057, 219.9682480396010078 ) ) ;
#3280 = CARTESIAN_POINT ( 'NONE',  ( -10.71662182846777611, 1438.669127598729347, 152.4922056935914725 ) ) ;
#3281 = VECTOR ( 'NONE', #62003, 1000.000000000000000 ) ;
#3282 = CARTESIAN_POINT ( 'NONE',  ( -37.29571716481897425, 1420.414000716506052, 266.4271095758174965 ) ) ;
#3283 = CARTESIAN_POINT ( 'NONE',  ( -13.36997666210000091, 1416.851343894929869, 221.9096085505980227 ) ) ;
#3284 = CARTESIAN_POINT ( 'NONE',  ( 5.386772287290000349, 1432.443201990170110, 154.6097844173980036 ) ) ;
#3285 = EDGE_CURVE ( 'NONE', #96209, #14911, #48053, .T. ) ;
#3286 = CARTESIAN_POINT ( 'NONE',  ( -14.35483098210000108, 1416.837177098929942, 221.5788728580980091 ) ) ;
#3287 = CARTESIAN_POINT ( 'NONE',  ( 12.72965162820000096, 1416.819756528429934, 223.1305967425979873 ) ) ;
#3288 = CARTESIAN_POINT ( 'NONE',  ( 8.781051467919999354, 1447.572322149110050, 186.1084250623979983 ) ) ;
#3289 = CARTESIAN_POINT ( 'NONE',  ( -2.299656354225000143, 1516.843453247299749, 206.6453952679669896 ) ) ;
#3290 = VERTEX_POINT ( 'NONE', #37586 ) ;
#3291 = CARTESIAN_POINT ( 'NONE',  ( 0.5594537969809989519, 1444.672526988890013, 215.3952916019189843 ) ) ;
#3292 = CARTESIAN_POINT ( 'NONE',  ( 1.488643740577330066, 1472.261774644039861, 182.6335304928790038 ) ) ;
#3293 = VERTEX_POINT ( 'NONE', #73824 ) ;
#3294 = CARTESIAN_POINT ( 'NONE',  ( 6.928690003924570462, 1456.700621706041602, 227.7321335879927346 ) ) ;
#3296 = ADVANCED_FACE ( 'NONE', ( #71789 ), #3304, .T. ) ;
#3295 = CARTESIAN_POINT ( 'NONE',  ( -18.89942244622886491, 1416.835807149959237, 207.5749765851556674 ) ) ;
#3297 = CARTESIAN_POINT ( 'NONE',  ( -15.29528072393560123, 1489.809333300280059, 194.3627042033380121 ) ) ;
#3298 = CARTESIAN_POINT ( 'NONE',  ( -37.25179242459999784, 1388.439297844689918, 234.7543419479590057 ) ) ;
#3299 = CARTESIAN_POINT ( 'NONE',  ( -9.094257307180781069, 1384.874748761890260, 199.9429999480310016 ) ) ;
#3300 = CARTESIAN_POINT ( 'NONE',  ( 22.53878019769999952, 1411.058442714830107, 206.1986153634379946 ) ) ;
#3301 = CARTESIAN_POINT ( 'NONE',  ( 18.43688931543651321, 1444.994950788469851, 161.6100378850028676 ) ) ;
#3302 = CARTESIAN_POINT ( 'NONE',  ( 16.57803282680000123, 1409.491978020829947, 225.2035548608979809 ) ) ;
#3303 = CARTESIAN_POINT ( 'NONE',  ( 32.22536377336271585, 1523.621879633028584, 201.4085774011528542 ) ) ;
#3304 = TOROIDAL_SURFACE ( 'NONE', #110537, 8.432239102140000497, 0.5000000000000000000 ) ;
#3305 = CARTESIAN_POINT ( 'NONE',  ( 0.9110504335954089372, 1450.859124385219957, 181.7304192028629757 ) ) ;
#3306 = DIRECTION ( 'NONE',  ( -1.000000000000000000, 0.000000000000000000, 0.000000000000000000 ) ) ;
#3307 = CIRCLE ( 'NONE', #64056, 26.99999999999999645 ) ;
#3308 = CARTESIAN_POINT ( 'NONE',  ( 2.874588922665000545, 1516.606339319019980, 215.6687976528169770 ) ) ;
#3309 = CARTESIAN_POINT ( 'NONE',  ( 2.485146179491022345, 1524.547395018738143, 242.5342643028157852 ) ) ;
#3310 = ORIENTED_EDGE ( 'NONE', *, *, #50885, .T. ) ;
#3311 = CARTESIAN_POINT ( 'NONE',  ( 3.448830483803564828, 1512.187213306747481, 175.1594891075192209 ) ) ;
#3312 = CARTESIAN_POINT ( 'NONE',  ( -5.102340803919999779, 1483.010473641589897, 199.7820758705289848 ) ) ;
#3313 = AXIS2_PLACEMENT_3D ( 'NONE', #66122, #56597, #100245 ) ;
#3314 = CARTESIAN_POINT ( 'NONE',  ( -12.32904923379281392, 1414.913060387329779, 219.9538042439937726 ) ) ;
#3315 = CIRCLE ( 'NONE', #58754, 2.000000000000075495 ) ;
#3316 = DIRECTION ( 'NONE',  ( 0.5877852522924831291, 0.000000000000000000, 0.8090169943749401238 ) ) ;
#3317 =( BOUNDED_CURVE ( )  B_SPLINE_CURVE ( 3, ( #53153, #105197, #11148, #87861 ),
 .UNSPECIFIED., .F., .F. ) 
 B_SPLINE_CURVE_WITH_KNOTS ( ( 4, 4 ),
 ( 1.916439914372829456, 2.295463455679393583 ),
 .UNSPECIFIED. ) 
 CURVE ( )  GEOMETRIC_REPRESENTATION_ITEM ( )  RATIONAL_B_SPLINE_CURVE ( ( 1.000000000000000000, 0.9880642163529229638, 0.9880642163529229638, 1.000000000000000000 ) ) 
 REPRESENTATION_ITEM ( '' )  );
#3318 = CARTESIAN_POINT ( 'NONE',  ( -35.83299582265050276, 1450.078159482010051, 136.2400848972689857 ) ) ;
#3319 = ADVANCED_FACE ( 'NONE', ( #22819, #101742 ), #68194, .T. ) ;
#3320 = AXIS2_PLACEMENT_3D ( 'NONE', #70591, #45924, #21217 ) ;
#3321 = LINE ( 'NONE', #53729, #4841 ) ;
#3322 = CARTESIAN_POINT ( 'NONE',  ( -7.553102827650000961, 1458.344558659830000, 234.3916895958979865 ) ) ;
#3323 = CARTESIAN_POINT ( 'NONE',  ( -2.904356733534350088, 1464.880529238149848, 184.1795813031409921 ) ) ;
#3324 = CARTESIAN_POINT ( 'NONE',  ( 11.85605537800000064, 1433.090874555759910, 150.3159297862979997 ) ) ;
#3325 = CARTESIAN_POINT ( 'NONE',  ( -42.68574267046690096, 1451.691555868290152, 269.7334229991980123 ) ) ;
#3326 = CARTESIAN_POINT ( 'NONE',  ( -17.98939368576640163, 1410.465184060849879, 195.2754043433779998 ) ) ;
#3327 = B_SPLINE_CURVE_WITH_KNOTS ( 'NONE', 3,
 ( #6516, #74842, #32271, #58038, #92718, #103883, #76476, #101651, #34476, #27183, #50725, #75926, #77041 ),
 .UNSPECIFIED., .F., .F.,
 ( 4, 3, 3, 3, 4 ),
 ( 0.9031056323884600889, 0.9451379527402459235, 0.9933535966189359634, 1.028735865613630063, 1.041569240497630000 ),
 .UNSPECIFIED. ) ;
#3328 = FACE_OUTER_BOUND ( 'NONE', #62628, .T. ) ;
#3329 = CARTESIAN_POINT ( 'NONE',  ( 9.412245003297918799, 1500.377496655100003, 202.5220683207009813 ) ) ;
#3330 = ORIENTED_EDGE ( 'NONE', *, *, #90583, .T. ) ;
#3331 = CYLINDRICAL_SURFACE ( 'NONE', #1911, 0.4999999999999909517 ) ;
#3332 = CARTESIAN_POINT ( 'NONE',  ( -3.059301852550817102, 1525.343727714918259, 176.8478560800957666 ) ) ;
#3333 = CARTESIAN_POINT ( 'NONE',  ( -1255.832924500349918, 1412.219004263330135, 209.0925205239309719 ) ) ;
#3334 = CARTESIAN_POINT ( 'NONE',  ( 8.491925884367525157, 1398.165181957728691, 199.2754951843434412 ) ) ;
#3335 = CARTESIAN_POINT ( 'NONE',  ( 1.914485657349999981, 1482.804926797230110, 235.2460200716980125 ) ) ;
#3336 = AXIS2_PLACEMENT_3D ( 'NONE', #42739, #25909, #50591 ) ;
#3337 = CARTESIAN_POINT ( 'NONE',  ( -17.12202622828511522, 1526.104292489133286, 235.9427193670834697 ) ) ;
#3338 = CARTESIAN_POINT ( 'NONE',  ( -13.79885730810000055, 1508.398156089429904, 232.7146120173979966 ) ) ;
#3339 = CARTESIAN_POINT ( 'NONE',  ( -22.49235462320989853, 1383.850897880320190, 221.9470685874750018 ) ) ;
#3340 = CARTESIAN_POINT ( 'NONE',  ( -4.679790880385569452, 1508.610720271750097, 205.9457817814489715 ) ) ;
#3341 = CARTESIAN_POINT ( 'NONE',  ( 2.499938418426329800, 1420.065636441539937, 97.17118231416419860 ) ) ;
#3342 = CARTESIAN_POINT ( 'NONE',  ( -14.75858115399999981, 1415.739699861750069, 212.8702772705990185 ) ) ;
#3343 = CARTESIAN_POINT ( 'NONE',  ( 1.549411822890000234, 1466.670383311630076, 234.9066445244980059 ) ) ;
#3345 = ORIENTED_EDGE ( 'NONE', *, *, #72188, .T. ) ;
#3344 = CARTESIAN_POINT ( 'NONE',  ( -41.65927775779999820, 1443.915297666309925, 135.6909731803980037 ) ) ;
#3346 = CARTESIAN_POINT ( 'NONE',  ( -1.608997026699999777, 1450.560824856070212, 182.3064528867980130 ) ) ;
#3347 = CARTESIAN_POINT ( 'NONE',  ( -10.88383664749751745, 1390.636386471471496, 203.2482663326153158 ) ) ;
#3348 = CARTESIAN_POINT ( 'NONE',  ( -5.401672965901620493, 1440.924418141449905, 154.8182599540220110 ) ) ;
#3350 = ORIENTED_EDGE ( 'NONE', *, *, #99298, .F. ) ;
#3349 = CARTESIAN_POINT ( 'NONE',  ( -30.90487439922542734, 1525.907212628473644, 216.4335774778784014 ) ) ;
#3351 = CARTESIAN_POINT ( 'NONE',  ( -2.360343982743250191, 1508.551704408389924, 220.0510488555580082 ) ) ;
#3352 = EDGE_LOOP ( 'NONE', ( #106947, #4880, #33350, #100023, #30456 ) ) ;
#3353 = CARTESIAN_POINT ( 'NONE',  ( -11.56183394306549950, 1388.455280331700123, 216.7304925199499905 ) ) ;
#3354 = FACE_OUTER_BOUND ( 'NONE', #40201, .T. ) ;
#3355 = CARTESIAN_POINT ( 'NONE',  ( -4.500000000000000000, 1411.429641636930000, 146.1721969590979882 ) ) ;
#3356 = CARTESIAN_POINT ( 'NONE',  ( -11.86629848740000170, 1432.349867584279991, 149.9824238681979978 ) ) ;
#3357 = CARTESIAN_POINT ( 'NONE',  ( -0.1306346743340009997, 1430.514091579490014, 217.4937112845890113 ) ) ;
#3358 = CARTESIAN_POINT ( 'NONE',  ( 19.68017795844365381, 1509.620912528763256, 186.9948578458423469 ) ) ;
#3359 = CARTESIAN_POINT ( 'NONE',  ( 14.51762396736629945, 1409.420026987000028, 212.6122462860219855 ) ) ;
#3360 = CARTESIAN_POINT ( 'NONE',  ( 2.040878228339999989, 1454.390661367689972, 215.4849015426389940 ) ) ;
#3361 = CARTESIAN_POINT ( 'NONE',  ( -89.02070098190330327, 1385.189645878620240, 291.9514036105480272 ) ) ;
#3362 = DIRECTION ( 'NONE',  ( 1.836970198721029688E-16, 1.000000000000000000, 0.000000000000000000 ) ) ;
#3363 = CARTESIAN_POINT ( 'NONE',  ( -2.372478608332516892, 1522.382868172863937, 174.8996806668726549 ) ) ;
#3364 = CARTESIAN_POINT ( 'NONE',  ( 12.33879830033670011, 1492.074832325789885, 209.1388286321879946 ) ) ;
#3365 = EDGE_LOOP ( 'NONE', ( #58598, #82587, #92902, #20201 ) ) ;
#3366 = EDGE_LOOP ( 'NONE', ( #41879, #9222, #17343, #38774, #60912 ) ) ;
#3367 = B_SPLINE_CURVE_WITH_KNOTS ( 'NONE', 3,
 ( #16187, #25142, #102412, #108618, #49833, #109187 ),
 .UNSPECIFIED., .F., .F.,
 ( 4, 2, 4 ),
 ( -1.285435071109398989E-05, 0.001079388306740562773, 0.002171630964192219470 ),
 .UNSPECIFIED. ) ;
#3368 = CARTESIAN_POINT ( 'NONE',  ( -11.93592535262589927, 1415.651572961190141, 194.9902245485579897 ) ) ;
#3369 = CARTESIAN_POINT ( 'NONE',  ( -1.306867980634530024, 1496.219773069479970, 196.8427661518120146 ) ) ;
#3370 = CARTESIAN_POINT ( 'NONE',  ( 16.41865139929206308, 1468.993348773691878, 269.3709366672832743 ) ) ;
#3371 = DIRECTION ( 'NONE',  ( -0.000000000000000000, -1.000000000000000000, -0.000000000000000000 ) ) ;
#3372 = CARTESIAN_POINT ( 'NONE',  ( 31.32941610406347266, 1525.856065479242716, 201.1886151593328123 ) ) ;
#3373 = CARTESIAN_POINT ( 'NONE',  ( -19.08184036181711818, 1486.257387795368004, 189.3980559289429664 ) ) ;
#3374 = CARTESIAN_POINT ( 'NONE',  ( -11.37387391107785994, 1367.111335829282325, 209.6218459617033432 ) ) ;
#3375 = CARTESIAN_POINT ( 'NONE',  ( 2.890489020090289962, 1507.108937781499890, 235.9439513786750240 ) ) ;
#3376 = CARTESIAN_POINT ( 'NONE',  ( -0.01323705180209850014, 1516.939658295650133, 206.6356258303270010 ) ) ;
#3377 = CIRCLE ( 'NONE', #67716, 10.00000000000000888 ) ;
#3378 = CARTESIAN_POINT ( 'NONE',  ( -12.89606705209609849, 1434.724827189529833, 149.2205627886980039 ) ) ;
#3379 = CARTESIAN_POINT ( 'NONE',  ( -3.156402467807082335, 1454.645949074940972, 199.8283705214046506 ) ) ;
#3380 = CARTESIAN_POINT ( 'NONE',  ( 0.5621803949210000262, 1416.843576337130116, 190.4753774197980078 ) ) ;
#3381 = CARTESIAN_POINT ( 'NONE',  ( 1.968601617930000103, 1498.935401861390119, 197.9561509160990056 ) ) ;
#3382 = AXIS2_PLACEMENT_3D ( 'NONE', #13665, #16278, #50481 ) ;
#3383 = B_SPLINE_CURVE_WITH_KNOTS ( 'NONE', 5,
 ( #71103, #62715, #96835, #77276, #34699, #11714 ),
 .UNSPECIFIED., .F., .F.,
 ( 6, 6 ),
 ( 0.000000000000000000, 1.000000000000000000 ),
 .UNSPECIFIED. ) ;
#3384 = ORIENTED_EDGE ( 'NONE', *, *, #73344, .T. ) ;
#3385 = AXIS2_PLACEMENT_3D ( 'NONE', #2627, #105625, #3182 ) ;
#3386 = CARTESIAN_POINT ( 'NONE',  ( 8.753854055680109880, 1516.720891557477444, 213.2732902691849972 ) ) ;
#3387 = CARTESIAN_POINT ( 'NONE',  ( -25.71796661899999847, 1449.805629481410051, 208.5932933947370032 ) ) ;
#3389 = CARTESIAN_POINT ( 'NONE',  ( -1.421471790896170040, 1507.619497854750080, 232.0556091900969875 ) ) ;
#3388 = CARTESIAN_POINT ( 'NONE',  ( -10.34929248509440036, 1425.419910064279975, 92.74534805534860027 ) ) ;
#3390 = CARTESIAN_POINT ( 'NONE',  ( -1.875976467151887928, 1407.675044305313577, 270.1370780915658543 ) ) ;
#3391 = CARTESIAN_POINT ( 'NONE',  ( -27.24390625379999875, 1427.221042094029826, 244.3119004031979955 ) ) ;
#3392 = CARTESIAN_POINT ( 'NONE',  ( 2.918982678559999933, 1485.831548431689953, 219.6257443891990135 ) ) ;
#3393 = CARTESIAN_POINT ( 'NONE',  ( 1.149726251327802373, 1415.652443921420854, 233.0560295573103815 ) ) ;
#3394 = CARTESIAN_POINT ( 'NONE',  ( 33.52142426879999704, 1450.454466855290093, 136.2569758902980084 ) ) ;
#3395 = ORIENTED_EDGE ( 'NONE', *, *, #68151, .F. ) ;
#3396 = CARTESIAN_POINT ( 'NONE',  ( -0.07152548254896469448, 1397.597842456309991, 196.1220356218829863 ) ) ;
#3397 = CARTESIAN_POINT ( 'NONE',  ( 14.31751620109325174, 1514.209381233404883, 225.6439688837686504 ) ) ;
#3398 = CARTESIAN_POINT ( 'NONE',  ( 5.994894223190000204, 1509.255434487730099, 238.7615784654979905 ) ) ;
#3399 = ORIENTED_EDGE ( 'NONE', *, *, #91858, .T. ) ;
#3400 = VERTEX_POINT ( 'NONE', #50279 ) ;
#3401 = CARTESIAN_POINT ( 'NONE',  ( -6.355004503879999156, 1384.926023117790010, 199.7181650675090054 ) ) ;
#3402 = CARTESIAN_POINT ( 'NONE',  ( 5.145309007309999849, 1422.426130173420006, 194.5914466168989918 ) ) ;
#3403 = ORIENTED_EDGE ( 'NONE', *, *, #51030, .F. ) ;
#3404 = CARTESIAN_POINT ( 'NONE',  ( 0.4901633952960000040, 1417.479174814430053, 184.7651825110980326 ) ) ;
#3405 = PRESENTATION_LAYER_ASSIGNMENT (  '', '', ( #99919 ) ) ;
#3406 = CARTESIAN_POINT ( 'NONE',  ( 10.80134480061129842, 1446.564900598669965, 153.0805715986590201 ) ) ;
#3407 = FACE_BOUND ( 'NONE', #58671, .T. ) ;
#3408 = CARTESIAN_POINT ( 'NONE',  ( -1.478497299709999879, 1479.774927945029958, 235.9387637257979975 ) ) ;
#3409 = CARTESIAN_POINT ( 'NONE',  ( 5.473890272918479738, 1440.659206135580007, 154.7842680422769774 ) ) ;
#3410 = ORIENTED_EDGE ( 'NONE', *, *, #83296, .T. ) ;
#3411 = CARTESIAN_POINT ( 'NONE',  ( 10.81515773970000005, 1424.921120067930133, 144.1684135303979986 ) ) ;
#3412 = CARTESIAN_POINT ( 'NONE',  ( -12.82280136242419921, 1414.971993471370070, 220.5247844368900019 ) ) ;
#3413 = B_SPLINE_CURVE_WITH_KNOTS ( 'NONE', 3,
 ( #73421, #105928, #29207, #99688, #65019, #107557, #63396, #81245, #39809, #97512, #82363, #108100, #90190, #89106, #22980, #57185, #54981, #46580, #80714, #4023, #72331, #106461, #29745, #63933, #98046, #21320, #55524, #4560, #38693, #72869, #30292, #25736, #15130, #6196, #50432, #102450, #40348, #31948, #42015, #57736, #7846, #58816, #48779, #58271, #75080, #83446, #108660, #59938, #41471, #24082, #42560, #91854, #94055, #7305, #109766, #74529, #24620, #66685, #33586, #23544, #15667, #75631, #66142, #100265, #8391, #92394, #49320, #82904, #34158, #6741, #59387, #40899, #25, #92955, #109230, #67779, #16228, #32514, #100791, #49871, #33046, #67234, #16769, #84005, #101330, #101891, #25184, #85102, #84557, #76164, #110311, #93498, #50972, #76713, #68344, #95723, #18431, #104120, #36915, #87895, #52631, #79487, #1131, #52081, #77282, #27408, #27967, #70006, #71109, #86768, #96278, #43671, #43123, #1682, #2795, #579, #35261, #61590, #26865, #61053, #18988, #60486, #11186, #77823 ),
 .UNSPECIFIED., .F., .F.,
 ( 4, 3, 3, 3, 3, 3, 3, 3, 3, 3, 3, 3, 3, 3, 3, 3, 3, 3, 3, 3, 3, 3, 3, 3, 3, 3, 3, 3, 3, 3, 3, 3, 3, 3, 3, 3, 3, 3, 3, 3, 3, 4 ),
 ( 1.527661073586570062E-12, 0.7233976231403740353, 1.453179569883080058, 2.189205328784380011, 2.931232241550089768, 3.681692766877309619, 4.436664690839419833, 5.195519430183240139, 5.957507373442520127, 6.722615321679190181, 7.488461883525279639, 8.253940120566859662, 8.872098166340000702, 9.627621989370730660, 10.37987637255229956, 11.12818954179939901, 11.87201083100580057, 12.60808579036049792, 13.25493342740159974, 13.90338778565579858, 14.62763214506709986, 14.71347576958129899, 15.43831616431399922, 16.16939285698139983, 16.92109434517130140, 17.66675291283500115, 18.41722696808670179, 19.17198454146360120, 19.93209661842169922, 20.69429497015770281, 21.45845625511120147, 22.18300476250000131, 22.94765126354310070, 23.71051285761900118, 24.46875717884919865, 25.22311653746220017, 25.97295705762990181, 26.71776956198449682, 27.45421737720040056, 28.18570414294039850, 28.90920563930189857, 29.42721171550000392 ),
 .UNSPECIFIED. ) ;
#3414 = CARTESIAN_POINT ( 'NONE',  ( 14.23707600319999855, 1463.795787833229952, 224.1834224494979821 ) ) ;
#3415 = ORIENTED_EDGE ( 'NONE', *, *, #94459, .T. ) ;
#3416 = CARTESIAN_POINT ( 'NONE',  ( -3.264778817514999876, 1516.727068157269969, 204.1245957781970048 ) ) ;
#3417 = ORIENTED_EDGE ( 'NONE', *, *, #69223, .T. ) ;
#3418 = CARTESIAN_POINT ( 'NONE',  ( 11.86184899506429957, 1432.039039536349947, 149.9742464043579844 ) ) ;
#3419 = CARTESIAN_POINT ( 'NONE',  ( 12.56175195062177607, 1445.048273880567194, 186.1342204703917673 ) ) ;
#3420 = ORIENTED_EDGE ( 'NONE', *, *, #96056, .T. ) ;
#3421 = ORIENTED_EDGE ( 'NONE', *, *, #105523, .F. ) ;
#3422 = CARTESIAN_POINT ( 'NONE',  ( 2.038847259689249736, 1522.382868172863937, 173.3106345060153046 ) ) ;
#3423 = CARTESIAN_POINT ( 'NONE',  ( -1.725662463192670248, 1484.236887848700007, 182.7463278875050037 ) ) ;
#3424 = CARTESIAN_POINT ( 'NONE',  ( -20.70884933757140089, 1409.636229341499984, 202.4398936187430138 ) ) ;
#3425 = CARTESIAN_POINT ( 'NONE',  ( -7.120274244888039838, 1470.094334173359812, 216.5229890130249828 ) ) ;
#3426 = CARTESIAN_POINT ( 'NONE',  ( 22.49191412916869837, 1452.127625438600035, 139.6794960788859896 ) ) ;
#3427 = CARTESIAN_POINT ( 'NONE',  ( 3.113156245266410327, 1409.286500863440097, 270.3710781324699610 ) ) ;
#3428 = CARTESIAN_POINT ( 'NONE',  ( -0.02549190311316479676, 1475.332589245109830, 220.5468605150740302 ) ) ;
#3429 = DIRECTION ( 'NONE',  ( 4.465978680329379737E-17, 1.000000000000000000, -2.349386720892264891E-16 ) ) ;
#3430 = CARTESIAN_POINT ( 'NONE',  ( -19.53035325068421812, 1509.611020418987209, 231.3334718708714206 ) ) ;
#3431 = FACE_OUTER_BOUND ( 'NONE', #16047, .T. ) ;
#3433 = CARTESIAN_POINT ( 'NONE',  ( 16.04354243109999700, 1471.309244717529964, 194.9556777362979858 ) ) ;
#3432 = CARTESIAN_POINT ( 'NONE',  ( -19.29649804419999981, 1504.799431328789979, 209.3162768295289879 ) ) ;
#3434 = CARTESIAN_POINT ( 'NONE',  ( 12.45034049356619832, 1421.619540909540092, 207.5029415923690124 ) ) ;
#3435 = CARTESIAN_POINT ( 'NONE',  ( 18.00557643216280113, 1423.829347998640060, 225.1846075778630052 ) ) ;
#3436 = CARTESIAN_POINT ( 'NONE',  ( -6.742834623714999864, 1512.383155430620036, 200.7463434866369880 ) ) ;
#3437 = VERTEX_POINT ( 'NONE', #32357 ) ;
#3438 = CARTESIAN_POINT ( 'NONE',  ( 8.518323188990001071, 1421.108130355529966, 243.9198229205979942 ) ) ;
#3439 = CARTESIAN_POINT ( 'NONE',  ( 18.68654020979418817, 1509.565608750526735, 186.8439702850651543 ) ) ;
#3440 = CARTESIAN_POINT ( 'NONE',  ( -55.35242389386650075, 1385.090656389910237, 272.4922876094810249 ) ) ;
#3441 = B_SPLINE_SURFACE_WITH_KNOTS ( 'NONE', 5, 5, ( 
 ( #25923, #43857, #8032, #33234, #60120, #94238 ),
 ( #17513, #51711, #30752, #105829, #55426, #64933 ),
 ( #55974, #72777, #4468, #90098, #37506, #95362 ),
 ( #18623, #39145, #12847, #72237, #99046, #106363 ),
 ( #13381, #29649, #89558, #81154, #98505, #106904 ),
 ( #47028, #35450, #47569, #30191, #64385, #20679 ),
 ( #38597, #107457, #21773, #11752, #81694, #5000 ),
 ( #22324, #1310, #80058, #45923, #73320, #56526 ),
 ( #63836, #69638, #3930, #97948, #46484, #54336 ) ),
 .UNSPECIFIED., .F., .F., .F.,
 ( 6, 3, 6 ),
 ( 6, 6 ),
 ( 10.04884080650000122, 10.52102568589999976, 10.99321056540000008 ),
 ( 0.000000000000000000, 2.000000000000000000 ),
 .UNSPECIFIED. ) ;
#3442 = DIRECTION ( 'NONE',  ( 0.000000000000000000, 1.000000000000000000, 0.000000000000000000 ) ) ;
#3443 = CARTESIAN_POINT ( 'NONE',  ( 4.875706362549999895, 1506.017256195089885, 219.8452990541989891 ) ) ;
#3444 = CARTESIAN_POINT ( 'NONE',  ( -15.41742678890000029, 1415.853057449160133, 210.9644741221289905 ) ) ;
#3446 = ORIENTED_EDGE ( 'NONE', *, *, #70043, .F. ) ;
#3445 = CARTESIAN_POINT ( 'NONE',  ( -15.86086750622509989, 1419.980772078519976, 210.7345574348329933 ) ) ;
#3447 = CARTESIAN_POINT ( 'NONE',  ( -16.78154512266720033, 1418.363846789659874, 203.4619184960750147 ) ) ;
#3448 = CARTESIAN_POINT ( 'NONE',  ( 19.60792669039999936, 1475.100271358290229, 204.3343059087790152 ) ) ;
#3449 = AXIS2_PLACEMENT_3D ( 'NONE', #65561, #99672, #14721 ) ;
#3450 = DIRECTION ( 'NONE',  ( 1.755985294532469921E-16, -1.000000000000000000, 1.338183447452831989E-16 ) ) ;
#3451 = DIRECTION ( 'NONE',  ( -0.5030436214085118873, 0.000000000000000000, 0.8642610224696064547 ) ) ;
#3452 = CARTESIAN_POINT ( 'NONE',  ( 14.12475443283500098, 1513.169116394660023, 224.4178625549669732 ) ) ;
#3453 = CARTESIAN_POINT ( 'NONE',  ( -7.375172166690000530, 1440.187291567539887, 186.1370477051980004 ) ) ;
#3454 = CARTESIAN_POINT ( 'NONE',  ( 6.531016915288740066, 1509.181447638889949, 179.3779377418509853 ) ) ;
#3455 = DIRECTION ( 'NONE',  ( -0.6736849260863841948, 0.000000000000000000, 0.7390186874254148774 ) ) ;
#3456 = CARTESIAN_POINT ( 'NONE',  ( -7.215398911020000305, 1408.913060387329779, 225.6058586963979735 ) ) ;
#3457 = CARTESIAN_POINT ( 'NONE',  ( 16.82235843289999977, 1415.092068029630127, 226.6094184117980319 ) ) ;
#3458 = EDGE_CURVE ( 'NONE', #77864, #90721, #54814, .T. ) ;
#3459 = CARTESIAN_POINT ( 'NONE',  ( -12.74982669920128941, 1462.837610516389304, 224.9934397671993054 ) ) ;
#3460 = CARTESIAN_POINT ( 'NONE',  ( -21.38516915558527742, 1522.906561336852519, 237.8497028174197965 ) ) ;
#3461 = CARTESIAN_POINT ( 'NONE',  ( 1.117840086735000016, 1516.949031626070109, 207.4047068479870006 ) ) ;
#3462 = CARTESIAN_POINT ( 'NONE',  ( 44.15636045789999287, 1429.838460442230144, 267.0405866975980302 ) ) ;
#3463 = CARTESIAN_POINT ( 'NONE',  ( -17.71696417089999898, 1409.531750409229971, 223.2909357272980060 ) ) ;
#3464 = CARTESIAN_POINT ( 'NONE',  ( 17.33494591590000056, 1435.104201471239776, 146.4861191636979925 ) ) ;
#3465 = VECTOR ( 'NONE', #20873, 1000.000000000000000 ) ;
#3466 = CARTESIAN_POINT ( 'NONE',  ( 21.98314659799999760, 1488.582363539229846, 193.7203962354979865 ) ) ;
#3467 = CARTESIAN_POINT ( 'NONE',  ( 29.71786509910646146, 1509.988056437398200, 208.1828936582288065 ) ) ;
#3468 = AXIS2_PLACEMENT_3D ( 'NONE', #34859, #94767, #69046 ) ;
#3469 = CARTESIAN_POINT ( 'NONE',  ( -13.68999425486880028, 1379.602495655479970, 208.0136990666040049 ) ) ;
#3470 = CARTESIAN_POINT ( 'NONE',  ( -1.328227237909999969, 1475.823473844229966, 266.9604901357979543 ) ) ;
#3471 = CYLINDRICAL_SURFACE ( 'NONE', #29822, 1.999999999999999556 ) ;
#3472 = FACE_OUTER_BOUND ( 'NONE', #58106, .T. ) ;
#3473 = CARTESIAN_POINT ( 'NONE',  ( -10.00906774830520085, 1407.931115486439921, 200.5109140070470062 ) ) ;
#3474 = CARTESIAN_POINT ( 'NONE',  ( -16.80706507779999725, 1416.677443236529825, 209.1193462365459936 ) ) ;
#3475 = CARTESIAN_POINT ( 'NONE',  ( -13.40958089250450058, 1414.996442620860080, 220.3303868550709694 ) ) ;
#3476 = CARTESIAN_POINT ( 'NONE',  ( -7.655626746931960547, 1383.726789944049870, 218.9639101100850098 ) ) ;
#3477 = CARTESIAN_POINT ( 'NONE',  ( 13.80590739080000162, 1434.979616766929894, 146.7593012265980121 ) ) ;
#3478 = CARTESIAN_POINT ( 'NONE',  ( 24.08426297012860218, 1411.115209414830133, 209.6325633951909708 ) ) ;
#3479 = DIRECTION ( 'NONE',  ( 1.273732310806389972E-11, 4.864864992887659796E-10, 1.000000000000000000 ) ) ;
#3480 = ORIENTED_EDGE ( 'NONE', *, *, #87025, .F. ) ;
#3481 = CARTESIAN_POINT ( 'NONE',  ( 0.9603421195823178547, 1368.656381476072966, 207.8228078564805230 ) ) ;
#3482 = CARTESIAN_POINT ( 'NONE',  ( -8.449237503979869501, 1409.208114262609797, 221.4678425924969929 ) ) ;
#3483 = CARTESIAN_POINT ( 'NONE',  ( 30.79697748855962303, 1526.178928173327677, 196.3997152352017110 ) ) ;
#3484 = CARTESIAN_POINT ( 'NONE',  ( -5.370514330159649852, 1422.356910281434239, 139.1416123588654727 ) ) ;
#3485 = CARTESIAN_POINT ( 'NONE',  ( -31.61404177300000029, 1466.402308574429981, 266.8259062747980010 ) ) ;
#3487 = AXIS2_PLACEMENT_3D ( 'NONE', #447, #19973, #10478 ) ;
#3486 = CARTESIAN_POINT ( 'NONE',  ( -30.64453888532113268, 1525.163527997504843, 196.6301324186591160 ) ) ;
#3488 = CARTESIAN_POINT ( 'NONE',  ( 3.347801439296141268, 1518.913060387330006, 176.1543725841967500 ) ) ;
#3489 = CARTESIAN_POINT ( 'NONE',  ( 19.30300490008626468, 1526.348417187218047, 233.1578084719440653 ) ) ;
#3490 = CARTESIAN_POINT ( 'NONE',  ( -95.18509927322880060, 1384.609717790749983, 310.0734934036659638 ) ) ;
#3491 = CARTESIAN_POINT ( 'NONE',  ( -46.36155058326189504, 1385.007142338620042, 220.0507881939000185 ) ) ;
#3492 = CARTESIAN_POINT ( 'NONE',  ( -5.436526647126479261, 1374.917605893529981, 214.9039629178479913 ) ) ;
#3493 = CARTESIAN_POINT ( 'NONE',  ( 21.92272425139999825, 1509.678618787829919, 227.7933223883979963 ) ) ;
#3494 = CARTESIAN_POINT ( 'NONE',  ( 15.64624339340000070, 1506.809279343430035, 224.6411995677980258 ) ) ;
#3495 = DIRECTION ( 'NONE',  ( -0.5224574779883525144, -0.7067418228232951183, 0.4770263929453549823 ) ) ;
#3497 = ORIENTED_EDGE ( 'NONE', *, *, #50233, .F. ) ;
#3496 = CARTESIAN_POINT ( 'NONE',  ( 4.324478665330000027, 1515.254593745989951, 208.3983361640229930 ) ) ;
#3498 = CARTESIAN_POINT ( 'NONE',  ( -8.604502001330001093, 1384.928348898680042, 199.8686409361690153 ) ) ;
#3499 = EDGE_CURVE ( 'NONE', #35766, #99633, #74407, .T. ) ;
#3500 = DIRECTION ( 'NONE',  ( 1.000000000000000000, 0.000000000000000000, 0.000000000000000000 ) ) ;
#3501 = EDGE_CURVE ( 'NONE', #90277, #63160, #6599, .T. ) ;
#3502 = EDGE_CURVE ( 'NONE', #33889, #21042, #75482, .T. ) ;
#3503 = CARTESIAN_POINT ( 'NONE',  ( -11.23368485119999960, 1500.117004219489900, 211.0002778243189994 ) ) ;
#3504 = DIRECTION ( 'NONE',  ( -0.8642610224695904675, 0.000000000000000000, 0.5030436214085395319 ) ) ;
#3505 = DIRECTION ( 'NONE',  ( -0.3090169943749447312, -0.000000000000000000, 0.9510565162951544194 ) ) ;
#3506 = EDGE_CURVE ( 'NONE', #83462, #77212, #56914, .T. ) ;
#3507 = CARTESIAN_POINT ( 'NONE',  ( 23.35095090740000146, 1410.223686913330084, 211.6910680449280164 ) ) ;
#3508 = CARTESIAN_POINT ( 'NONE',  ( -4.146782895030730387, 1426.018316030089863, 186.1121555109529879 ) ) ;
#3509 = EDGE_CURVE ( 'NONE', #105125, #50173, #92804, .T. ) ;
#3510 = CARTESIAN_POINT ( 'NONE',  ( 18.80805864981130071, 1458.321402826489930, 220.5644953607610148 ) ) ;
#3511 = CARTESIAN_POINT ( 'NONE',  ( -15.63365311440000127, 1422.686384262629872, 229.4762402829979919 ) ) ;
#3513 = CARTESIAN_POINT ( 'NONE',  ( -11.72666526949699950, 1426.702413974029923, 143.4268556625789870 ) ) ;
#3512 = CARTESIAN_POINT ( 'NONE',  ( -11.77676754959999883, 1432.864147235409973, 150.8103446100980136 ) ) ;
#3514 = CARTESIAN_POINT ( 'NONE',  ( -0.4957217136000000024, 1415.745301206330168, 233.4042774855979872 ) ) ;
#3515 = CARTESIAN_POINT ( 'NONE',  ( 0.3803835583100000362, 1496.712195753129890, 230.6756913771979782 ) ) ;
#3516 = CARTESIAN_POINT ( 'NONE',  ( 1966.823930461590180, 11221.53578756869865, 443.7115846868979929 ) ) ;
#3517 = CYLINDRICAL_SURFACE ( 'NONE', #87453, 1.999999999999998668 ) ;
#3518 = CARTESIAN_POINT ( 'NONE',  ( -9.830395177430000686, 1365.769828494180047, 210.6218459616991936 ) ) ;
#3519 = CARTESIAN_POINT ( 'NONE',  ( -2.490245952555000031, 1516.691389976299888, 204.5134284255869943 ) ) ;
#3520 = CARTESIAN_POINT ( 'NONE',  ( 13.38995414329220068, 1507.947836362450062, 233.1180173837540224 ) ) ;
#3521 = CARTESIAN_POINT ( 'NONE',  ( -16.30638770610000066, 1484.820604609629981, 187.8396872195979768 ) ) ;
#3522 = CARTESIAN_POINT ( 'NONE',  ( 11.23549300526389949, 1502.543211738040100, 212.3416208334529927 ) ) ;
#3523 = AXIS2_PLACEMENT_3D ( 'NONE', #13851, #98969, #13297 ) ;
#3524 = CARTESIAN_POINT ( 'NONE',  ( -13.70181463665861621, 1421.117064391099802, 210.6307364177106649 ) ) ;
#3526 = ORIENTED_EDGE ( 'NONE', *, *, #49371, .T. ) ;
#3525 = CARTESIAN_POINT ( 'NONE',  ( -67.80648804034809984, 1379.745630162259886, 279.2148224231119684 ) ) ;
#3527 = ORIENTED_EDGE ( 'NONE', *, *, #9754, .T. ) ;
#3528 = CARTESIAN_POINT ( 'NONE',  ( 28.32766665009999940, 1509.601337745830051, 212.4145138620280022 ) ) ;
#3529 = ORIENTED_EDGE ( 'NONE', *, *, #6660, .F. ) ;
#3530 = DIRECTION ( 'NONE',  ( -0.6736849260863841948, 0.000000000000000000, 0.7390186874254148774 ) ) ;
#3531 = DIRECTION ( 'NONE',  ( -0.9334681682710679329, 0.3057582888762500062, -0.1874807926378720124 ) ) ;
#3533 = CARTESIAN_POINT ( 'NONE',  ( 1.206391046180000037, 1508.614280349730052, 180.4667425254979776 ) ) ;
#3532 = CARTESIAN_POINT ( 'NONE',  ( 15.76264809293400226, 1413.510787989959908, 191.4348339044099987 ) ) ;
#3534 = CARTESIAN_POINT ( 'NONE',  ( 11.86590139589999815, 1432.348266868109931, 151.0567667964980103 ) ) ;
#3535 = EDGE_CURVE ( 'NONE', #75001, #94600, #101498, .T. ) ;
#3536 = AXIS2_PLACEMENT_3D ( 'NONE', #106492, #105958, #29236 ) ;
#3537 = CARTESIAN_POINT ( 'NONE',  ( -25.15969574395609953, 1451.151030661709910, 137.5686878300720082 ) ) ;
#3538 = CARTESIAN_POINT ( 'NONE',  ( -1.044338232960000168, 1469.645465345889988, 219.1445103612989840 ) ) ;
#3539 = CARTESIAN_POINT ( 'NONE',  ( 5.824346749060000050, 1409.620982476830022, 230.9132778911979926 ) ) ;
#3540 = CARTESIAN_POINT ( 'NONE',  ( 10.04557648923880109, 1482.796278672210065, 212.7028893834429937 ) ) ;
#3541 = CARTESIAN_POINT ( 'NONE',  ( 2.879956924955000108, 1516.827328999679821, 212.3743765858270081 ) ) ;
#3542 = EDGE_CURVE ( 'NONE', #67049, #17568, #84135, .T. ) ;
#3543 = CARTESIAN_POINT ( 'NONE',  ( 40.44958274758150196, 1439.458628678830109, 134.0999999981179940 ) ) ;
#3544 = CARTESIAN_POINT ( 'NONE',  ( -20.55780381099999943, 1485.073231501690088, 207.1087988815990002 ) ) ;
#3545 = EDGE_LOOP ( 'NONE', ( #86504, #13255, #25222, #109789 ) ) ;
#3546 = CARTESIAN_POINT ( 'NONE',  ( 0.1681681984989999989, 1420.473120458229914, 172.2701767054979882 ) ) ;
#3547 = AXIS2_PLACEMENT_3D ( 'NONE', #96990, #88590, #88047 ) ;
#3548 = CARTESIAN_POINT ( 'NONE',  ( -1.731903628061610023, 1431.483103224190017, 200.9088633058729840 ) ) ;
#3549 = ORIENTED_EDGE ( 'NONE', *, *, #64421, .T. ) ;
#3550 = ORIENTED_EDGE ( 'NONE', *, *, #91361, .T. ) ;
#3551 = EDGE_CURVE ( 'NONE', #79909, #47729, #20081, .T. ) ;
#3552 = ORIENTED_EDGE ( 'NONE', *, *, #50922, .F. ) ;
#3553 = CARTESIAN_POINT ( 'NONE',  ( 13.46945357809454613, 1410.756328442758104, 228.3088036694626624 ) ) ;
#3554 = CARTESIAN_POINT ( 'NONE',  ( 32.72609422369145449, 1524.152349020271004, 217.1332896956630520 ) ) ;
#3555 = CARTESIAN_POINT ( 'NONE',  ( 10.56616917823093793, 1451.302389960884284, 152.0481050481907630 ) ) ;
#3556 = CARTESIAN_POINT ( 'NONE',  ( -8.022926871310001928, 1384.932834875369963, 218.7874489595089926 ) ) ;
#3557 = CARTESIAN_POINT ( 'NONE',  ( 9.774667823450000625, 1462.791341090990045, 210.7173602730590005 ) ) ;
#3558 = AXIS2_PLACEMENT_3D ( 'NONE', #22540, #5792, #107690 ) ;
#3559 = CARTESIAN_POINT ( 'NONE',  ( -12.34121275650000094, 1378.648013544750029, 208.9830469583500019 ) ) ;
#3560 = CARTESIAN_POINT ( 'NONE',  ( -63.72440971995120407, 1379.735940357757272, 269.6083204700776719 ) ) ;
#3561 = CARTESIAN_POINT ( 'NONE',  ( 4.237127598589969679, 1446.355009009640071, 163.3939598556469832 ) ) ;
#3562 = CARTESIAN_POINT ( 'NONE',  ( 1.406911967200000113, 1508.853878877429906, 238.2247902776979913 ) ) ;
#3563 = VERTEX_POINT ( 'NONE', #44074 ) ;
#3564 = CARTESIAN_POINT ( 'NONE',  ( 3.445201488374999954, 1516.743010792419909, 207.4064848398570291 ) ) ;
#3565 = ORIENTED_EDGE ( 'NONE', *, *, #91748, .F. ) ;
#3566 = CARTESIAN_POINT ( 'NONE',  ( 31.14199524840240230, 1440.913060387330006, 254.3632966892320155 ) ) ;
#3567 = CARTESIAN_POINT ( 'NONE',  ( -18.89418430779999980, 1508.334383760630089, 187.8348365672979980 ) ) ;
#3568 = ORIENTED_EDGE ( 'NONE', *, *, #9882, .T. ) ;
#3569 = CARTESIAN_POINT ( 'NONE',  ( 25.71819509060329878, 1450.790613536419869, 136.8498688079899921 ) ) ;
#3570 = CARTESIAN_POINT ( 'NONE',  ( -13.62085029079999998, 1409.388710960530034, 191.1271092111979897 ) ) ;
#3571 = CARTESIAN_POINT ( 'NONE',  ( -17.98592010575266187, 1508.456915429008859, 211.9106567536674106 ) ) ;
#3573 = DIRECTION ( 'NONE',  ( 1.836970198721029688E-16, 1.000000000000000000, -1.262177448353620010E-31 ) ) ;
#3572 = CARTESIAN_POINT ( 'NONE',  ( -24.90078896880000059, 1441.036975945570020, 210.4313365108079950 ) ) ;
#3574 = CARTESIAN_POINT ( 'NONE',  ( 22.13036493270980287, 1410.097162861090055, 206.2644002183290013 ) ) ;
#3575 = CARTESIAN_POINT ( 'NONE',  ( 0.0002637436312147029959, 1396.476788460397984, 196.7304488273350387 ) ) ;
#3576 = CYLINDRICAL_SURFACE ( 'NONE', #58477, 0.9999999999999522604 ) ;
#3577 = CARTESIAN_POINT ( 'NONE',  ( -11.87502393270000134, 1433.007271228389982, 149.9804723947979994 ) ) ;
#3578 = CARTESIAN_POINT ( 'NONE',  ( -14.56318188130000024, 1489.452917662129948, 192.4089202742979978 ) ) ;
#3580 = CARTESIAN_POINT ( 'NONE',  ( 0.3086485800401259638, 1457.828016588880018, 228.9774103206889890 ) ) ;
#3579 = CARTESIAN_POINT ( 'NONE',  ( -0.2272535083270984524, 1465.118792751454293, 238.1338994539894145 ) ) ;
#3581 = AXIS2_PLACEMENT_3D ( 'NONE', #29767, #90773, #64504 ) ;
#3582 = B_SPLINE_SURFACE_WITH_KNOTS ( 'NONE', 5, 5, ( 
 ( #34061, #491, #33489, #34614, #51420, #58724 ),
 ( #68800, #76619, #74985, #91755, #109133, #67138 ),
 ( #32416, #84467, #68254, #66595, #100699, #83908 ),
 ( #25645, #93410, #67691, #8848, #101236, #58176 ),
 ( #41919, #50342, #92305, #15575, #101799, #49777 ),
 ( #50874, #7214, #75538, #109672, #24536, #92859 ),
 ( #16135, #7755, #76075, #59293, #110216, #25089 ),
 ( #16675, #85003, #44697, #20017, #3256, #1586 ),
 ( #51983, #94508, #103459, #17783, #27878, #79940 ),
 ( #88337, #71019, #69350, #10522, #53094, #104024 ),
 ( #60387, #26766, #60954, #45255, #95630, #11088 ),
 ( #79390, #37383, #9418, #43580, #36272, #77730 ),
 ( #105139, #1043, #27319, #61500, #70462, #96184 ),
 ( #86124, #54212, #28429, #35165, #95081, #18347 ),
 ( #11629, #62629, #52538, #86671, #9967, #44138 ) ),
 .UNSPECIFIED., .F., .F., .F.,
 ( 6, 3, 3, 3, 6 ),
 ( 6, 6 ),
 ( 10.77847743720000118, 25.90271913459999809, 41.12370487549999609, 56.51454383889999633, 65.55090256170001339 ),
 ( 0.000000000000000000, 2.000000000000000000 ),
 .UNSPECIFIED. ) ;
#3583 = CARTESIAN_POINT ( 'NONE',  ( -6.940473372275000052, 1516.833525648419936, 215.6778681647369922 ) ) ;
#3584 = CARTESIAN_POINT ( 'NONE',  ( -32.80315919379393819, 1523.919943579690425, 217.1667904774563453 ) ) ;
#3585 = CARTESIAN_POINT ( 'NONE',  ( 6.048292005814400518, 1511.681069547209972, 217.7611486164249754 ) ) ;
#3586 = CARTESIAN_POINT ( 'NONE',  ( 2.189546061933858478, 1407.000065118299290, 222.1218459836267698 ) ) ;
#3587 = CARTESIAN_POINT ( 'NONE',  ( -4.996642198295000448, 1516.697242742309982, 211.9989590406970024 ) ) ;
#3588 = CARTESIAN_POINT ( 'NONE',  ( 3.915803383833039941, 1515.051704408389924, 213.4516362061017674 ) ) ;
#3589 = CARTESIAN_POINT ( 'NONE',  ( -2.646473796664690070, 1483.649213716789973, 198.7830764605120066 ) ) ;
#3591 = ORIENTED_EDGE ( 'NONE', *, *, #5748, .T. ) ;
#3590 = CARTESIAN_POINT ( 'NONE',  ( -3.071538966616310429, 1374.913060387290216, 207.4438565765843236 ) ) ;
#3592 = CARTESIAN_POINT ( 'NONE',  ( -17.12670006681592128, 1524.374142163904253, 237.3021637559003523 ) ) ;
#3593 = AXIS2_PLACEMENT_3D ( 'NONE', #48663, #91738, #72750 ) ;
#3594 = CARTESIAN_POINT ( 'NONE',  ( 28.09269446629999933, 1440.913060388880012, 231.9538848061980048 ) ) ;
#3595 = CARTESIAN_POINT ( 'NONE',  ( -11.86652821809999914, 1432.377789890399981, 150.3970469068979980 ) ) ;
#3596 = CARTESIAN_POINT ( 'NONE',  ( -14.68065129330000040, 1415.999375028279928, 204.4212104945090118 ) ) ;
#3597 = CARTESIAN_POINT ( 'NONE',  ( 1.797565579689999860, 1415.903556134429891, 232.4419632246980143 ) ) ;
#3598 = CARTESIAN_POINT ( 'NONE',  ( 12.23993107200000097, 1420.119835428209853, 199.7451907216789948 ) ) ;
#3599 = EDGE_CURVE ( 'NONE', #23842, #58146, #11963, .T. ) ;
#3601 = CARTESIAN_POINT ( 'NONE',  ( 19.01728017970000195, 1456.599257794629921, 225.8866418926980089 ) ) ;
#3600 = FACE_OUTER_BOUND ( 'NONE', #27914, .T. ) ;
#3602 = CARTESIAN_POINT ( 'NONE',  ( -0.2331618352820000184, 1488.813684182529869, 187.9057016649980199 ) ) ;
#3603 = CARTESIAN_POINT ( 'NONE',  ( -106.8758219270079906, 1380.995759212869871, 309.1925272263990223 ) ) ;
#3604 = ORIENTED_EDGE ( 'NONE', *, *, #53028, .T. ) ;
#3605 = CARTESIAN_POINT ( 'NONE',  ( -7.723480117524999855, 1517.086065052259983, 205.0863097070169943 ) ) ;
#3606 = CARTESIAN_POINT ( 'NONE',  ( 2.110812721519999879, 1405.784960767830171, 267.5353002013980017 ) ) ;
#3607 = EDGE_CURVE ( 'NONE', #82900, #104987, #86066, .T. ) ;
#3608 = CARTESIAN_POINT ( 'NONE',  ( -1.466212339980000001, 1515.204044912790096, 213.4476482949990270 ) ) ;
#3609 = B_SPLINE_CURVE_WITH_KNOTS ( 'NONE', 3,
 ( #106022, #37157, #89205, #11951, #10858, #80263, #81338, #13026, #61834, #12500 ),
 .UNSPECIFIED., .F., .F.,
 ( 4, 2, 2, 2, 4 ),
 ( 0.000000000000000000, 0.2500000000000000000, 0.5000000000000000000, 0.7500000000000000000, 1.000000000000000000 ),
 .UNSPECIFIED. ) ;
#3610 = CARTESIAN_POINT ( 'NONE',  ( 38.08045545485799721, 1455.559130441839898, 269.8109766600500166 ) ) ;
#3611 = DIRECTION ( 'NONE',  ( -0.7142107836478398530, 0.4827861023098918847, -0.5067746401878859830 ) ) ;
#3612 = CARTESIAN_POINT ( 'NONE',  ( 21.13734888319999783, 1496.938803861589804, 209.1218459616989946 ) ) ;
#3613 = CARTESIAN_POINT ( 'NONE',  ( -18.83964618864532881, 1526.382868172863937, 232.8185072403850313 ) ) ;
#3614 = TOROIDAL_SURFACE ( 'NONE', #66194, 1.000000000000000000, 1.000000000000000000 ) ;
#3615 = EDGE_CURVE ( 'NONE', #37055, #77021, #38719, .T. ) ;
#3616 = DIRECTION ( 'NONE',  ( -0.7067707787425930865, 0.03085829008194152304, 0.7067692920952404201 ) ) ;
#3617 = CARTESIAN_POINT ( 'NONE',  ( 9.619198284380544806, 1463.334820347890400, 214.5538614071193706 ) ) ;
#3618 = CARTESIAN_POINT ( 'NONE',  ( 3.246115288789999997, 1507.570166992290069, 220.3920571188990039 ) ) ;
#3619 = DIRECTION ( 'NONE',  ( -1.755985294532469921E-16, 1.000000000000000000, -1.338183447452831989E-16 ) ) ;
#3620 = ORIENTED_EDGE ( 'NONE', *, *, #20513, .T. ) ;
#3621 = AXIS2_PLACEMENT_3D ( 'NONE', #4859, #38463, #72639 ) ;
#3622 = CARTESIAN_POINT ( 'NONE',  ( -23.42675388609999843, 1440.913060387330006, 234.3916895593979746 ) ) ;
#3623 = CARTESIAN_POINT ( 'NONE',  ( 20.20959865099491992, 1512.187213306747481, 236.2316688286738611 ) ) ;
#3624 = CARTESIAN_POINT ( 'NONE',  ( -0.2135896670159999899, 1475.319218785530211, 269.4986771182980192 ) ) ;
#3625 = CARTESIAN_POINT ( 'NONE',  ( -4.254265649320910114, 1446.521173488880095, 160.4300573142469943 ) ) ;
#3626 = CARTESIAN_POINT ( 'NONE',  ( -33.14208818188998151, 1524.841055067850220, 197.8283574329105647 ) ) ;
#3627 = CARTESIAN_POINT ( 'NONE',  ( -3.531993496884077377, 1448.289151893011649, 184.8902033554412299 ) ) ;
#3628 = CARTESIAN_POINT ( 'NONE',  ( -39.33111985152770274, 1384.790562297770066, 240.9749358342589858 ) ) ;
#3629 = VECTOR ( 'NONE', #88330, 1000.000000000000227 ) ;
#3630 = CARTESIAN_POINT ( 'NONE',  ( -105.7427259770000063, 1378.913061773969957, 302.9732994362589693 ) ) ;
#3631 = CARTESIAN_POINT ( 'NONE',  ( 17.70437741359999961, 1453.580057579390086, 200.5051001409389926 ) ) ;
#3632 = CARTESIAN_POINT ( 'NONE',  ( 26.48169467979350244, 1435.504490709530046, 135.8310255694130149 ) ) ;
#3633 = EDGE_CURVE ( 'NONE', #32165, #85866, #104172, .T. ) ;
#3634 =( BOUNDED_CURVE ( )  B_SPLINE_CURVE ( 3, ( #36275, #78848, #61504, #11632 ),
 .UNSPECIFIED., .F., .F. ) 
 B_SPLINE_CURVE_WITH_KNOTS ( ( 4, 4 ),
 ( 5.498282993746389735, 7.068394191937580118 ),
 .UNSPECIFIED. ) 
 CURVE ( )  GEOMETRIC_REPRESENTATION_ITEM ( )  RATIONAL_B_SPLINE_CURVE ( ( 1.000000000000000000, 0.8048993128220308657, 0.8048993128220308657, 1.000000000000000000 ) ) 
 REPRESENTATION_ITEM ( '' )  );
#3635 = CARTESIAN_POINT ( 'NONE',  ( -11.00962827163180080, 1396.297525078389981, 210.2710635922789777 ) ) ;
#3636 = EDGE_CURVE ( 'NONE', #72154, #74077, #29398, .T. ) ;
#3637 = B_SPLINE_CURVE_WITH_KNOTS ( 'NONE', 3,
 ( #100646, #92259, #49179, #57031, #109620, #76561, #91158, #109081, #75486, #8239, #59237, #32362, #15529, #76012, #40205 ),
 .UNSPECIFIED., .F., .F.,
 ( 4, 2, 2, 1, 1, 1, 2, 2, 4 ),
 ( 0.000000000000000000, 0.2499999999999727440, 0.3749999999999591438, 0.4374999999999514277, 0.4687499999999488742, 0.4843749999999449329, 0.4921874999999458211, 0.4999999999999468203, 1.000000000000000000 ),
 .UNSPECIFIED. ) ;
#3638 = CARTESIAN_POINT ( 'NONE',  ( -14.74910871950000057, 1422.312372933829920, 229.1172104516980141 ) ) ;
#3639 = CARTESIAN_POINT ( 'NONE',  ( -44.78530908650000697, 1438.258924716540150, 269.6939408608980671 ) ) ;
#3640 = VERTEX_POINT ( 'NONE', #52483 ) ;
#3641 = CARTESIAN_POINT ( 'NONE',  ( -11.32996165527507415, 1502.367014232210977, 207.2237320763624666 ) ) ;
#3642 = FACE_OUTER_BOUND ( 'NONE', #105448, .T. ) ;
#3643 = CARTESIAN_POINT ( 'NONE',  ( -11.76196280667599936, 1425.587142435169881, 146.3421825698729890 ) ) ;
#3645 = CARTESIAN_POINT ( 'NONE',  ( -14.49215846226499949, 1514.088841912139969, 192.6059998857670053 ) ) ;
#3644 = CARTESIAN_POINT ( 'NONE',  ( 11.30143738019999944, 1426.878411159930010, 112.6515547669980037 ) ) ;
#3646 = CARTESIAN_POINT ( 'NONE',  ( -2.487934962309999776, 1508.551704408389924, 204.1347675205190058 ) ) ;
#3647 = CARTESIAN_POINT ( 'NONE',  ( 4.285305835930380169, 1423.903434674070013, 183.8442863319299931 ) ) ;
#3648 = EDGE_CURVE ( 'NONE', #55027, #58309, #2089, .T. ) ;
#3649 = TOROIDAL_SURFACE ( 'NONE', #35, 1.000000000000000000, 1.000000000000000000 ) ;
#3650 = CARTESIAN_POINT ( 'NONE',  ( 1.710012720495000194, 1517.232977404109988, 201.3945188173769907 ) ) ;
#3651 = CARTESIAN_POINT ( 'NONE',  ( 7.436161634030000300, 1426.180031595399896, 212.4856801342990025 ) ) ;
#3652 = CARTESIAN_POINT ( 'NONE',  ( 18.32584137559999959, 1473.764089050990151, 194.8973954003990059 ) ) ;
#3653 = CARTESIAN_POINT ( 'NONE',  ( 2.338461260499999916, 1507.140901839730077, 181.2734692156980145 ) ) ;
#3654 = CARTESIAN_POINT ( 'NONE',  ( -21.12854634993719927, 1507.715432715349834, 209.4790063854959783 ) ) ;
#3655 = CARTESIAN_POINT ( 'NONE',  ( -62.88192661074859302, 1379.821258371850035, 270.0876200625010028 ) ) ;
#3656 = CARTESIAN_POINT ( 'NONE',  ( 7.706598004008788472, 1366.632089620137322, 207.6218459616988241 ) ) ;
#3657 = EDGE_CURVE ( 'NONE', #3107, #87558, #71252, .T. ) ;
#3659 = EDGE_LOOP ( 'NONE', ( #92733, #50325, #24117, #77022 ) ) ;
#3658 = CARTESIAN_POINT ( 'NONE',  ( -16.67901052306879706, 1379.616296946549937, 212.0685361777370304 ) ) ;
#3660 = ORIENTED_EDGE ( 'NONE', *, *, #109695, .T. ) ;
#3661 = CARTESIAN_POINT ( 'NONE',  ( -6.170313909579999923, 1397.182081570829951, 197.8857380438980158 ) ) ;
#3662 = CARTESIAN_POINT ( 'NONE',  ( -0.2817902298945799688, 1499.041747040399741, 236.9809926041430117 ) ) ;
#3663 = CARTESIAN_POINT ( 'NONE',  ( 3.294994957250000134, 1408.913060387329779, 226.6118641217979928 ) ) ;
#3664 = CARTESIAN_POINT ( 'NONE',  ( -7.556166249915000854, 1510.696675236759802, 213.5834717662970093 ) ) ;
#3666 = CARTESIAN_POINT ( 'NONE',  ( 11.71997758784366184, 1414.913060387329779, 198.0465748933708880 ) ) ;
#3665 = CARTESIAN_POINT ( 'NONE',  ( -105.3795479729999869, 1390.980567596649962, 304.2017031079589628 ) ) ;
#3667 = AXIS2_PLACEMENT_3D ( 'NONE', #4462, #79519, #2823 ) ;
#3668 = CARTESIAN_POINT ( 'NONE',  ( 2.931305164040000300, 1429.770167287230151, 184.8385999854980071 ) ) ;
#3669 = CARTESIAN_POINT ( 'NONE',  ( -1.720875739424750028, 1464.150623787119912, 199.3240472289820104 ) ) ;
#3670 = CARTESIAN_POINT ( 'NONE',  ( -41.65407651957470136, 1444.067054679140028, 136.1145617669420176 ) ) ;
#3671 = CARTESIAN_POINT ( 'NONE',  ( -2.500000000000000000, 1448.203018870860205, 169.6830894382590031 ) ) ;
#3672 = CARTESIAN_POINT ( 'NONE',  ( -12.89608512423069975, 1434.724840024559853, 149.2206170422699927 ) ) ;
#3673 = CARTESIAN_POINT ( 'NONE',  ( 1.342110557989999897, 1416.822690122629865, 190.1636845438980004 ) ) ;
#3674 = CARTESIAN_POINT ( 'NONE',  ( -3.827756660372859887, 1405.952650783709942, 267.2292680377810257 ) ) ;
#3675 = CARTESIAN_POINT ( 'NONE',  ( 15.90990255763500016, 1512.830284628050094, 198.1616908427670296 ) ) ;
#3676 = ORIENTED_EDGE ( 'NONE', *, *, #21579, .F. ) ;
#3677 = CARTESIAN_POINT ( 'NONE',  ( -16.81611548244668342, 1526.382868172864164, 183.6985842798727049 ) ) ;
#3678 = CARTESIAN_POINT ( 'NONE',  ( 12.53124724090000086, 1441.827068648660088, 188.3849333394979908 ) ) ;
#3679 = EDGE_LOOP ( 'NONE', ( #18940, #40964, #10687, #106527, #99518 ) ) ;
#3680 = EDGE_CURVE ( 'NONE', #97278, #44414, #58766, .T. ) ;
#3681 = ORIENTED_EDGE ( 'NONE', *, *, #18018, .T. ) ;
#3682 = CARTESIAN_POINT ( 'NONE',  ( -4.360511100030000087, 1454.978814073790090, 200.7714291330290166 ) ) ;
#3683 = DIRECTION ( 'NONE',  ( -1.755985294532469921E-16, 1.000000000000000000, -1.338183447452831989E-16 ) ) ;
#3684 = EDGE_CURVE ( 'NONE', #18150, #15971, #12215, .T. ) ;
#3685 = CARTESIAN_POINT ( 'NONE',  ( 3.263521904354999670, 1516.676340709600026, 214.8942497445370066 ) ) ;
#3686 = CARTESIAN_POINT ( 'NONE',  ( 3.165841356415000085, 1511.802450769970164, 217.0590624235869939 ) ) ;
#3687 = ORIENTED_EDGE ( 'NONE', *, *, #36438, .F. ) ;
#3688 = CARTESIAN_POINT ( 'NONE',  ( -2.961869365206950100, 1509.113818662810218, 179.2106785136219855 ) ) ;
#3689 = CARTESIAN_POINT ( 'NONE',  ( -79.28273665509999546, 1377.156469662599875, 290.5424571711589579 ) ) ;
#3690 = CARTESIAN_POINT ( 'NONE',  ( 18.20160569639999792, 1416.825421875629900, 213.0758509618380003 ) ) ;
#3691 = CARTESIAN_POINT ( 'NONE',  ( -2.878693287274999957, 1516.766397346390022, 205.0941487061870134 ) ) ;
#3692 = VECTOR ( 'NONE', #69071, 1000.000000000000000 ) ;
#3693 = FACE_OUTER_BOUND ( 'NONE', #70319, .T. ) ;
#3694 = B_SPLINE_SURFACE_WITH_KNOTS ( 'NONE', 5, 5, ( 
 ( #309, #110587, #33873, #74800, #42284, #15953 ),
 ( #17600, #76434, #75890, #50686, #51800, #68609 ),
 ( #85939, #9242, #59652, #66412, #108943, #58000 ),
 ( #68064, #17038, #7027, #24898, #100529, #60203 ),
 ( #102177, #110040, #93760, #23808, #102712, #59105 ),
 ( #92134, #51235, #15409, #83732, #41184, #84283 ) ),
 .UNSPECIFIED., .F., .F., .F.,
 ( 6, 6 ),
 ( 6, 6 ),
 ( 4.250940516431700011, 7.082035122218299783 ),
 ( -9.670478295891639110E-06, 0.5000000000000000000 ),
 .UNSPECIFIED. ) ;
#3695 = CARTESIAN_POINT ( 'NONE',  ( -106.7756681249999957, 1385.009182713600012, 297.1165651138589965 ) ) ;
#3696 = CARTESIAN_POINT ( 'NONE',  ( -3.448199307399999913, 1409.033474160629794, 231.3476878950980051 ) ) ;
#3698 = ORIENTED_EDGE ( 'NONE', *, *, #45621, .F. ) ;
#3697 = CARTESIAN_POINT ( 'NONE',  ( -30.61618914730555119, 1525.211473355384669, 196.6453055283535889 ) ) ;
#3699 = CARTESIAN_POINT ( 'NONE',  ( -14.59279134157089963, 1436.244781760590058, 149.8708244536879874 ) ) ;
#3700 = LINE ( 'NONE', #36174, #92569 ) ;
#3701 = CARTESIAN_POINT ( 'NONE',  ( 20.28308613678659711, 1497.601638836400070, 226.7150518706519904 ) ) ;
#3702 = CARTESIAN_POINT ( 'NONE',  ( 16.61094140337936409, 1423.052547370200500, 227.3764671272628277 ) ) ;
#3703 = CARTESIAN_POINT ( 'NONE',  ( 42.28239094362500339, 1436.755401113810194, 269.8809666808659813 ) ) ;
#3704 = CARTESIAN_POINT ( 'NONE',  ( 6.560742225334999844, 1517.028034847769959, 213.1554992345569701 ) ) ;
#3705 = CARTESIAN_POINT ( 'NONE',  ( -65.00001850430001582, 1379.749314314899948, 272.6104031607590059 ) ) ;
#3706 = CARTESIAN_POINT ( 'NONE',  ( 23.55087631299999984, 1411.110694763729953, 207.7642880164279973 ) ) ;
#3707 = CARTESIAN_POINT ( 'NONE',  ( -109.9855944279999989, 1384.926148861439970, 311.4562326602589906 ) ) ;
#3708 = CARTESIAN_POINT ( 'NONE',  ( 13.54784204829999972, 1426.885522674909907, 197.1450391101479909 ) ) ;
#3709 = CARTESIAN_POINT ( 'NONE',  ( -11.60004869885203682, 1422.586199384407792, 135.5999999980976440 ) ) ;
#3710 = CARTESIAN_POINT ( 'NONE',  ( -1.709766532154999963, 1516.959716008189844, 209.1345041580460133 ) ) ;
#3711 = ORIENTED_EDGE ( 'NONE', *, *, #526, .T. ) ;
#3712 = CARTESIAN_POINT ( 'NONE',  ( 4.299342307242959293, 1420.540376342569971, 185.6306603416350072 ) ) ;
#3713 = CARTESIAN_POINT ( 'NONE',  ( -12.88074797900000057, 1417.902816224529943, 228.2418185653980061 ) ) ;
#3714 = DIRECTION ( 'NONE',  ( -5.980589973904019347E-17, 1.000000000000000000, -1.736889445713099699E-16 ) ) ;
#3715 = ORIENTED_EDGE ( 'NONE', *, *, #63601, .F. ) ;
#3716 = CARTESIAN_POINT ( 'NONE',  ( -25.11140045820960154, 1385.255350696510050, 223.7582419935289977 ) ) ;
#3717 = CARTESIAN_POINT ( 'NONE',  ( -2.583034826040000009, 1429.324951399489919, 200.5039866108990054 ) ) ;
#3718 = CIRCLE ( 'NONE', #78837, 7.513264357030008611 ) ;
#3719 = CARTESIAN_POINT ( 'NONE',  ( 7.499999980935000643, 1516.801704408389924, 209.1218459511669892 ) ) ;
#3720 = CARTESIAN_POINT ( 'NONE',  ( -24.91259172930000076, 1441.818365303380006, 210.4560922370480114 ) ) ;
#3721 = CARTESIAN_POINT ( 'NONE',  ( -0.4274041271319999891, 1409.096031326030015, 232.6209024892979755 ) ) ;
#3722 = CARTESIAN_POINT ( 'NONE',  ( 0.04366022373244289601, 1420.445819799160063, 182.6759295617300154 ) ) ;
#3723 = ADVANCED_FACE ( 'NONE', ( #29457 ), #100025, .F. ) ;
#3724 = AXIS2_PLACEMENT_3D ( 'NONE', #5683, #89127, #40366 ) ;
#3726 = CARTESIAN_POINT ( 'NONE',  ( -16.11470690007832118, 1416.382804326506175, 208.7747741149743490 ) ) ;
#3725 = CARTESIAN_POINT ( 'NONE',  ( 2.488360629304999794, 1516.616791731099966, 214.8929950451170043 ) ) ;
#3727 = DIRECTION ( 'NONE',  ( -0.6736849260863839728, 0.000000000000000000, 0.7390186874254150995 ) ) ;
#3728 = CARTESIAN_POINT ( 'NONE',  ( 10.06225300309310100, 1469.716777501389970, 209.4998798077870106 ) ) ;
#3729 = VERTEX_POINT ( 'NONE', #70805 ) ;
#3730 = CARTESIAN_POINT ( 'NONE',  ( -0.01126495432349849946, 1516.939530130779985, 202.1773791897269916 ) ) ;
#3731 = CARTESIAN_POINT ( 'NONE',  ( 10.52443147309969973, 1481.186296556219986, 208.2194658927409989 ) ) ;
#3732 = ORIENTED_EDGE ( 'NONE', *, *, #44116, .F. ) ;
#3733 = CARTESIAN_POINT ( 'NONE',  ( 5.151075264148989419, 1490.744830062189976, 188.9005219498210124 ) ) ;
#3734 = DIRECTION ( 'NONE',  ( 1.988619772330852129E-13, 0.03085824620771311644, -0.9995237709234254808 ) ) ;
#3735 = CARTESIAN_POINT ( 'NONE',  ( 8.788267567532809466, 1511.742575854359984, 202.8686686809350022 ) ) ;
#3736 = CARTESIAN_POINT ( 'NONE',  ( 2.583256299099999875, 1441.752764794789982, 218.3094755959190252 ) ) ;
#3737 = CARTESIAN_POINT ( 'NONE',  ( -27.30178126419649942, 1509.643183905199976, 201.1665203492270280 ) ) ;
#3738 = AXIS2_PLACEMENT_3D ( 'NONE', #51329, #16589, #77104 ) ;
#3739 = EDGE_CURVE ( 'NONE', #68673, #108385, #26617, .T. ) ;
#3740 = CARTESIAN_POINT ( 'NONE',  ( -3.116049926250000102, 1446.579647253840221, 167.4613962610980025 ) ) ;
#3741 = CARTESIAN_POINT ( 'NONE',  ( -29.30029655192934257, 1525.907212628473644, 221.3719603026177367 ) ) ;
#3742 = CARTESIAN_POINT ( 'NONE',  ( -16.81191884579999751, 1435.084986459429956, 146.9484194988980050 ) ) ;
#3743 = CARTESIAN_POINT ( 'NONE',  ( -19.75595884730000051, 1465.302413857089959, 208.1547143399459685 ) ) ;
#3744 = CARTESIAN_POINT ( 'NONE',  ( 18.35614473489999909, 1445.354571529839859, 191.3429017699980079 ) ) ;
#3746 = CARTESIAN_POINT ( 'NONE',  ( -18.93441063164366511, 1438.881150600395131, 210.4529607928175494 ) ) ;
#3745 = FACE_OUTER_BOUND ( 'NONE', #71128, .T. ) ;
#3747 = CARTESIAN_POINT ( 'NONE',  ( -9.903567409750580808, 1472.178920281909996, 211.4406132415489878 ) ) ;
#3748 = ORIENTED_EDGE ( 'NONE', *, *, #10708, .F. ) ;
#3750 = EDGE_CURVE ( 'NONE', #10960, #67163, #71013, .T. ) ;
#3749 = CARTESIAN_POINT ( 'NONE',  ( -105.0536199400000044, 1379.378595376449994, 303.3386746932590086 ) ) ;
#3751 = CARTESIAN_POINT ( 'NONE',  ( -8.899549366109999582, 1508.515584743789987, 219.0073388492789945 ) ) ;
#3752 = CARTESIAN_POINT ( 'NONE',  ( -10.73514660131351839, 1424.973046421745494, 139.1354236205272343 ) ) ;
#3753 = CARTESIAN_POINT ( 'NONE',  ( -24.26965460479999948, 1437.030983368090119, 210.8923187080280002 ) ) ;
#3754 = CARTESIAN_POINT ( 'NONE',  ( -3.082606035640000464, 1484.897200977490229, 198.4345628581990013 ) ) ;
#3755 = CARTESIAN_POINT ( 'NONE',  ( 1.435939366446196575, 1526.382868172863937, 239.4992070516220508 ) ) ;
#3756 = CARTESIAN_POINT ( 'NONE',  ( -2.500000000000000000, 1425.929641636930000, 184.1455913746980002 ) ) ;
#3757 = CARTESIAN_POINT ( 'NONE',  ( 22.59376922909999763, 1497.713060387329961, 210.1004891184930159 ) ) ;
#3758 = CARTESIAN_POINT ( 'NONE',  ( -7.495712400002839004, 1517.016242308364099, 208.8285887136074450 ) ) ;
#3759 = CARTESIAN_POINT ( 'NONE',  ( 3.938385272561739647, 1493.417418013209954, 219.5392876527429848 ) ) ;
#3760 = CARTESIAN_POINT ( 'NONE',  ( -10.29417939532470072, 1490.744234622979775, 212.9867478681659918 ) ) ;
#3761 = CARTESIAN_POINT ( 'NONE',  ( 20.81805062950000362, 1457.016307409189949, 206.8942079858889826 ) ) ;
#3762 = CARTESIAN_POINT ( 'NONE',  ( -92.91140151093370037, 1383.768484979190134, 309.3741002178249460 ) ) ;
#3763 = CARTESIAN_POINT ( 'NONE',  ( -109.6813523066950182, 1383.874575646420226, 311.2769763007889878 ) ) ;
#3764 = CARTESIAN_POINT ( 'NONE',  ( -0.7983437007204670088, 1516.708834472140097, 201.4082439830900171 ) ) ;
#3766 = ORIENTED_EDGE ( 'NONE', *, *, #88002, .F. ) ;
#3765 = CARTESIAN_POINT ( 'NONE',  ( 21.59676349220000091, 1508.920392562430152, 190.9891518189980104 ) ) ;
#3767 = CARTESIAN_POINT ( 'NONE',  ( -106.7756681350000036, 1384.894991215109940, 297.1173194602590115 ) ) ;
#3768 = ADVANCED_FACE ( 'NONE', ( #87002 ), #11419, .F. ) ;
#3769 = CARTESIAN_POINT ( 'NONE',  ( 12.22498599127479935, 1512.125809830880144, 223.8828819965079902 ) ) ;
#3770 = VERTEX_POINT ( 'NONE', #37164 ) ;
#3771 = ORIENTED_EDGE ( 'NONE', *, *, #24131, .F. ) ;
#3772 = CARTESIAN_POINT ( 'NONE',  ( 26.92641998615820143, 1490.346006921080061, 207.6803555114329924 ) ) ;
#3773 = CARTESIAN_POINT ( 'NONE',  ( -109.7179059649999999, 1384.924775326750023, 297.0861727099589871 ) ) ;
#3774 = CARTESIAN_POINT ( 'NONE',  ( 12.75948692019158948, 1442.829946663825012, 169.4538695351947410 ) ) ;
#3776 = CARTESIAN_POINT ( 'NONE',  ( -31.95512683359999428, 1442.955673910089899, 244.1805851163980208 ) ) ;
#3775 = CARTESIAN_POINT ( 'NONE',  ( 38.88871891119339352, 1429.342410219364410, 269.5910596282614051 ) ) ;
#3777 = EDGE_CURVE ( 'NONE', #20783, #98304, #62963, .T. ) ;
#3778 = CARTESIAN_POINT ( 'NONE',  ( 9.723333314712000686, 1436.167293238569982, 210.6196431544800021 ) ) ;
#3779 = CARTESIAN_POINT ( 'NONE',  ( -11.93261574969999828, 1433.458717525199972, 150.0079056965979873 ) ) ;
#3780 = EDGE_CURVE ( 'NONE', #81290, #58486, #53436, .T. ) ;
#3781 = CARTESIAN_POINT ( 'NONE',  ( 26.86205050240000247, 1508.007394640929988, 206.2315947028279766 ) ) ;
#3782 = CARTESIAN_POINT ( 'NONE',  ( -19.05388999639999881, 1486.255215324529900, 189.3722275761979859 ) ) ;
#3783 = CARTESIAN_POINT ( 'NONE',  ( -19.84399396720000297, 1467.318719066990070, 208.1502282180090333 ) ) ;
#3784 = CARTESIAN_POINT ( 'NONE',  ( 13.86092680780000030, 1410.765486841630263, 191.1266656171980003 ) ) ;
#3785 = CARTESIAN_POINT ( 'NONE',  ( 5.031515383899999527, 1423.012122006030040, 184.4169789091980078 ) ) ;
#3786 = CARTESIAN_POINT ( 'NONE',  ( 1.554992009126110020, 1515.071272245649880, 213.4511250689819803 ) ) ;
#3787 = CARTESIAN_POINT ( 'NONE',  ( 16.95499469859999664, 1419.905063748630027, 226.7592642413980002 ) ) ;
#3788 = CARTESIAN_POINT ( 'NONE',  ( -5.864936813312239927, 1477.472823321480064, 219.0780053889600083 ) ) ;
#3789 = AXIS2_PLACEMENT_3D ( 'NONE', #101960, #93560, #7368 ) ;
#3790 = EDGE_CURVE ( 'NONE', #92672, #11723, #41367, .T. ) ;
#3791 = CARTESIAN_POINT ( 'NONE',  ( 34.31402925621353006, 1524.244163922423468, 200.2096061136539618 ) ) ;
#3793 = ORIENTED_EDGE ( 'NONE', *, *, #92766, .T. ) ;
#3792 = CARTESIAN_POINT ( 'NONE',  ( 9.286020759454600352E-09, 1409.388281829009884, 259.9969200755350585 ) ) ;
#3794 = ORIENTED_EDGE ( 'NONE', *, *, #5777, .T. ) ;
#3795 = CARTESIAN_POINT ( 'NONE',  ( -11.85886382813039930, 1431.831096394299948, 149.9589654793649913 ) ) ;
#3796 = CARTESIAN_POINT ( 'NONE',  ( -21.39151623717510020, 1487.103275126709832, 201.9631718257530224 ) ) ;
#3797 = CARTESIAN_POINT ( 'NONE',  ( -10.46129436240000032, 1470.510090683430008, 269.3483239609980160 ) ) ;
#3798 = CARTESIAN_POINT ( 'NONE',  ( 7.516769032520000060, 1422.170349638209927, 195.6959265412990021 ) ) ;
#3800 = AXIS2_PLACEMENT_3D ( 'NONE', #88123, #46679, #72424 ) ;
#3799 = FACE_OUTER_BOUND ( 'NONE', #95481, .T. ) ;
#3801 = CARTESIAN_POINT ( 'NONE',  ( -15.32324661150000011, 1495.926233386129979, 224.3776978810979870 ) ) ;
#3802 = CARTESIAN_POINT ( 'NONE',  ( 0.3404056040617879364, 1450.948218928229835, 181.6983794943430155 ) ) ;
#3803 = CARTESIAN_POINT ( 'NONE',  ( -4.987078435459999071, 1508.551704408389924, 209.1218459616989946 ) ) ;
#3804 = DIRECTION ( 'NONE',  ( -0.6736849260863841948, 0.000000000000000000, 0.7390186874254148774 ) ) ;
#3805 = AXIS2_PLACEMENT_3D ( 'NONE', #47369, #8103, #110024 ) ;
#3806 = CARTESIAN_POINT ( 'NONE',  ( -1.056358525591428288, 1484.867159798215653, 182.1438065072321137 ) ) ;
#3807 = CARTESIAN_POINT ( 'NONE',  ( 6.892224678230459034, 1361.632554499760090, 210.6218459616991936 ) ) ;
#3808 = CARTESIAN_POINT ( 'NONE',  ( -44.63471219002420298, 1432.172276597919790, 266.7236482179810082 ) ) ;
#3809 = ORIENTED_EDGE ( 'NONE', *, *, #19899, .T. ) ;
#3810 = CARTESIAN_POINT ( 'NONE',  ( -3.543446017492749789, 1501.284872974150176, 181.2258732813619986 ) ) ;
#3811 = EDGE_CURVE ( 'NONE', #48668, #45663, #28011, .T. ) ;
#3812 = ORIENTED_EDGE ( 'NONE', *, *, #98933, .F. ) ;
#3813 = ORIENTED_EDGE ( 'NONE', *, *, #46047, .T. ) ;
#3814 = CARTESIAN_POINT ( 'NONE',  ( -5.770820179264999794, 1516.591755933730155, 210.8331571987770019 ) ) ;
#3815 = AXIS2_PLACEMENT_3D ( 'NONE', #40082, #109501, #99974 ) ;
#3816 = CARTESIAN_POINT ( 'NONE',  ( -17.22592475670000312, 1443.913060387330006, 162.9227486557980171 ) ) ;
#3817 = EDGE_CURVE ( 'NONE', #106056, #88894, #75711, .T. ) ;
#3818 = CARTESIAN_POINT ( 'NONE',  ( -22.52564151099999989, 1509.699673122230024, 190.3321270482979912 ) ) ;
#3819 = CARTESIAN_POINT ( 'NONE',  ( -14.69814578489999946, 1425.419041251630006, 189.8691658534980036 ) ) ;
#3820 = CARTESIAN_POINT ( 'NONE',  ( 11.75869035672759999, 1522.051704408389924, 227.2994842695800060 ) ) ;
#3821 = ORIENTED_EDGE ( 'NONE', *, *, #47977, .F. ) ;
#3822 = EDGE_CURVE ( 'NONE', #89306, #3290, #97423, .T. ) ;
#3823 = CARTESIAN_POINT ( 'NONE',  ( 3.259729297834999873, 1517.119374999550018, 201.7846921639870175 ) ) ;
#3824 = CARTESIAN_POINT ( 'NONE',  ( 5.826428076080000906, 1473.811884028689974, 218.9454251420289950 ) ) ;
#3825 = CARTESIAN_POINT ( 'NONE',  ( -13.83457784759895937, 1504.369317328791112, 226.5199076315979312 ) ) ;
#3826 = ORIENTED_EDGE ( 'NONE', *, *, #68263, .F. ) ;
#3827 = AXIS2_PLACEMENT_3D ( 'NONE', #16214, #50418, #79473 ) ;
#3828 = CARTESIAN_POINT ( 'NONE',  ( -13.03876375938340004, 1411.451441007050107, 269.8787200598279696 ) ) ;
#3829 = CARTESIAN_POINT ( 'NONE',  ( -1.554562095370000119, 1427.328278510630071, 123.0297916884979941 ) ) ;
#3830 = CARTESIAN_POINT ( 'NONE',  ( 8.536223301210858594, 1436.502018257360078, 207.9555195538749786 ) ) ;
#3832 = ORIENTED_EDGE ( 'NONE', *, *, #55659, .F. ) ;
#3831 = CARTESIAN_POINT ( 'NONE',  ( -9.657355732020000971, 1366.083296228050131, 207.6218459616989946 ) ) ;
#3833 = ORIENTED_EDGE ( 'NONE', *, *, #97972, .F. ) ;
#3834 = CARTESIAN_POINT ( 'NONE',  ( 45.58493676572534525, 1442.547795422105082, 268.9761766335485618 ) ) ;
#3835 = CARTESIAN_POINT ( 'NONE',  ( 2.993162530245609965, 1466.561220909740086, 219.7621249222650022 ) ) ;
#3836 = CARTESIAN_POINT ( 'NONE',  ( -14.45215659597139890, 1436.253647968190080, 149.9616404399920100 ) ) ;
#3837 = CARTESIAN_POINT ( 'NONE',  ( -0.03623977524627750024, 1409.497123560340015, 185.3062518060349930 ) ) ;
#3838 = AXIS2_PLACEMENT_3D ( 'NONE', #66963, #14317, #56898 ) ;
#3839 = CARTESIAN_POINT ( 'NONE',  ( -17.44754804248470137, 1415.007830321539814, 207.5653879932930295 ) ) ;
#3840 = CARTESIAN_POINT ( 'NONE',  ( -18.30677928060000070, 1435.778268302339939, 226.2504290301980063 ) ) ;
#3841 = CARTESIAN_POINT ( 'NONE',  ( 10.66852226406069981, 1475.487520392919805, 267.5060550787330271 ) ) ;
#3842 = CARTESIAN_POINT ( 'NONE',  ( 11.75715125319999999, 1415.140114695929924, 222.5039781239979959 ) ) ;
#3843 = CARTESIAN_POINT ( 'NONE',  ( -17.37005806175103473, 1422.637693141805130, 226.5733611387645965 ) ) ;
#3844 = CARTESIAN_POINT ( 'NONE',  ( -1.136004312195000088, 1516.815173273089840, 206.2562091229970065 ) ) ;
#3845 = ORIENTED_EDGE ( 'NONE', *, *, #950, .F. ) ;
#3846 = CARTESIAN_POINT ( 'NONE',  ( -38.81202640297369300, 1450.612734557460044, 135.6928040505150079 ) ) ;
#3847 = CARTESIAN_POINT ( 'NONE',  ( -22.45016027724620855, 1451.714353191599685, 219.6156308778561765 ) ) ;
#3848 = ORIENTED_EDGE ( 'NONE', *, *, #109496, .T. ) ;
#3850 = B_SPLINE_CURVE_WITH_KNOTS ( 'NONE', 3,
 ( #45604, #96535, #79746, #63518, #71375, #104375, #9757, #18148, #105487, #28778, #27125, #87592, #62978 ),
 .UNSPECIFIED., .F., .F.,
 ( 4, 3, 3, 3, 4 ),
 ( -7.154418212010000389, -6.085421029112350055, -5.016423846214689952, -3.988585745587499787, -2.933308256780000178 ),
 .UNSPECIFIED. ) ;
#3849 = CARTESIAN_POINT ( 'NONE',  ( 0.2331202188386839735, 1408.921201124740037, 186.4825399812679905 ) ) ;
#3851 = CARTESIAN_POINT ( 'NONE',  ( 15.69795926444620271, 1519.551704408389924, 222.7678737639049871 ) ) ;
#3852 = CARTESIAN_POINT ( 'NONE',  ( 6.372167600494999640, 1511.069621805459974, 216.5183910133270047 ) ) ;
#3853 = CARTESIAN_POINT ( 'NONE',  ( -9.092535821413379793, 1384.806370746179937, 199.9443633485050213 ) ) ;
#3854 = CARTESIAN_POINT ( 'NONE',  ( 19.12232319319999618, 1410.076634111130033, 195.9544771405979873 ) ) ;
#3855 = CARTESIAN_POINT ( 'NONE',  ( 22.77810580590000100, 1410.208903622529988, 207.2750177385480015 ) ) ;
#3856 = CARTESIAN_POINT ( 'NONE',  ( -23.80235451360000098, 1435.328707481769925, 136.9030858810979794 ) ) ;
#3857 = CARTESIAN_POINT ( 'NONE',  ( 32.38845791999494850, 1523.382868172864164, 202.1182848005511801 ) ) ;
#3858 = CARTESIAN_POINT ( 'NONE',  ( 20.28305703155452733, 1455.773760547615893, 223.2321826931089106 ) ) ;
#3859 = CARTESIAN_POINT ( 'NONE',  ( 2.500000000000000000, 1439.466623694439932, 162.9904177469239812 ) ) ;
#3860 = CARTESIAN_POINT ( 'NONE',  ( -4.612507312034999529, 1516.886345593249871, 214.1313240375470173 ) ) ;
#3861 = CARTESIAN_POINT ( 'NONE',  ( 2.700472180933962907, 1524.678541297860875, 241.8613664836760506 ) ) ;
#3862 = ORIENTED_EDGE ( 'NONE', *, *, #70755, .F. ) ;
#3863 = CARTESIAN_POINT ( 'NONE',  ( -17.23909798190000231, 1417.482756323010108, 206.7388844422490024 ) ) ;
#3864 = CARTESIAN_POINT ( 'NONE',  ( -44.79032719779999638, 1444.249662561040168, 269.6864475883979821 ) ) ;
#3865 = CARTESIAN_POINT ( 'NONE',  ( -11.22085813611739979, 1414.913060387329779, 220.6193216859199993 ) ) ;
#3866 = CARTESIAN_POINT ( 'NONE',  ( -20.37344316928624721, 1508.015640753926164, 209.5635218970269023 ) ) ;
#3867 = CARTESIAN_POINT ( 'NONE',  ( -40.23101736414809437, 1444.600352321709806, 137.0308947161730089 ) ) ;
#3868 = VECTOR ( 'NONE', #53553, 1000.000000000000000 ) ;
#3869 = CARTESIAN_POINT ( 'NONE',  ( 11.60004869885203682, 1425.965608304797797, 137.6301247321180483 ) ) ;
#3870 = CARTESIAN_POINT ( 'NONE',  ( -3.274920518576323377E-16, 1418.913060387330006, 172.2701767054979882 ) ) ;
#3871 = CARTESIAN_POINT ( 'NONE',  ( 17.88228687367667646, 1423.788287748384391, 225.8724688183563671 ) ) ;
#3872 = CARTESIAN_POINT ( 'NONE',  ( -12.31045119098629925, 1378.376187953739873, 209.7947064970520046 ) ) ;
#3873 = CARTESIAN_POINT ( 'NONE',  ( -44.01000096382649929, 1448.211628717079975, 269.7085006184129838 ) ) ;
#3874 = CARTESIAN_POINT ( 'NONE',  ( -10.32771419153329973, 1461.601508178220001, 211.2214880053600154 ) ) ;
#3875 = CARTESIAN_POINT ( 'NONE',  ( -109.7216215100000056, 1385.013037790159842, 297.0870309045589579 ) ) ;
#3876 = CARTESIAN_POINT ( 'NONE',  ( -32.06031249785756643, 1524.760046179776054, 202.1360311646459422 ) ) ;
#3877 = ORIENTED_EDGE ( 'NONE', *, *, #58344, .T. ) ;
#3878 = CARTESIAN_POINT ( 'NONE',  ( -3.351006924987864455, 1524.082582765195411, 176.2279596953965779 ) ) ;
#3879 = DIRECTION ( 'NONE',  ( 0.7063774289747313251, 0.04540766091858271930, -0.7063774289747313251 ) ) ;
#3880 = CIRCLE ( 'NONE', #57513, 1.999999999992389865 ) ;
#3881 = CARTESIAN_POINT ( 'NONE',  ( -5.513435705061030312, 1509.038615938849944, 201.6090957135359929 ) ) ;
#3882 = CARTESIAN_POINT ( 'NONE',  ( -2.409586283469999923, 1426.663880916129983, 144.1938086916980239 ) ) ;
#3883 = CARTESIAN_POINT ( 'NONE',  ( 33.93019615848955084, 1522.382868172863937, 220.5829544587961095 ) ) ;
#3884 = CARTESIAN_POINT ( 'NONE',  ( -14.53877746969999940, 1509.420765683830041, 233.9657681612980014 ) ) ;
#3885 = CARTESIAN_POINT ( 'NONE',  ( -19.85258526977679949, 1383.853738160929879, 220.7008533539980135 ) ) ;
#3886 = CARTESIAN_POINT ( 'NONE',  ( -2.847678236428970333, 1430.845636561999981, 201.2564352187889938 ) ) ;
#3887 = CARTESIAN_POINT ( 'NONE',  ( 18.64672481363430379, 1416.851343896850040, 209.6839434896919840 ) ) ;
#3888 = LINE ( 'NONE', #106320, #16463 ) ;
#3889 = CARTESIAN_POINT ( 'NONE',  ( 1.358137423290000090, 1466.377668926530077, 235.0851387380980100 ) ) ;
#3891 = ORIENTED_EDGE ( 'NONE', *, *, #55132, .T. ) ;
#3890 = CARTESIAN_POINT ( 'NONE',  ( -4.554962026871971048, 1508.731359868796062, 212.6094325583298712 ) ) ;
#3892 = CARTESIAN_POINT ( 'NONE',  ( -0.9433386499399999403, 1452.411361074829983, 183.4747736275980117 ) ) ;
#3893 = CIRCLE ( 'NONE', #64637, 1.999999999999999556 ) ;
#3894 = CARTESIAN_POINT ( 'NONE',  ( -17.51956951369999871, 1383.856177979750100, 219.7926916635590260 ) ) ;
#3895 = EDGE_CURVE ( 'NONE', #110498, #7502, #103397, .T. ) ;
#3896 = CARTESIAN_POINT ( 'NONE',  ( 4.001327954560360389, 1508.551704408389924, 204.6458544173759719 ) ) ;
#3898 = VERTEX_POINT ( 'NONE', #40452 ) ;
#3897 = CARTESIAN_POINT ( 'NONE',  ( -18.34590453789999742, 1416.851343897030119, 208.8605687093670156 ) ) ;
#3899 = CARTESIAN_POINT ( 'NONE',  ( 22.14278947725500402, 1473.984036977170035, 210.1089657997129905 ) ) ;
#3900 = ORIENTED_EDGE ( 'NONE', *, *, #100121, .F. ) ;
#3901 = CARTESIAN_POINT ( 'NONE',  ( -10.88641269510000065, 1390.488938065530192, 215.1023730057590058 ) ) ;
#3902 = CARTESIAN_POINT ( 'NONE',  ( 11.74015320060000001, 1428.979986575930070, 144.1938086916980239 ) ) ;
#3903 = FACE_OUTER_BOUND ( 'NONE', #75801, .T. ) ;
#3904 = CARTESIAN_POINT ( 'NONE',  ( -6.404454395499999286, 1464.203453065390022, 200.1263287045289871 ) ) ;
#3905 = CARTESIAN_POINT ( 'NONE',  ( -9.803834995107230554, 1517.151704408390060, 196.6215198571080123 ) ) ;
#3906 = CARTESIAN_POINT ( 'NONE',  ( 2.622430729442982056, 1523.621879633028584, 242.1535192357228254 ) ) ;
#3907 = CARTESIAN_POINT ( 'NONE',  ( 14.85649457888519898, 1409.431860609890009, 210.6024228449819873 ) ) ;
#3908 = FACE_OUTER_BOUND ( 'NONE', #1261, .T. ) ;
#3909 = CARTESIAN_POINT ( 'NONE',  ( -90.62803924738049943, 1385.194695644730018, 292.9449760712819852 ) ) ;
#3910 = CARTESIAN_POINT ( 'NONE',  ( -18.11933796430000143, 1437.050887716040052, 191.5172096114979752 ) ) ;
#3911 = CARTESIAN_POINT ( 'NONE',  ( -68.68489780340000550, 1379.748151576980035, 279.9908545622590168 ) ) ;
#3912 = CIRCLE ( 'NONE', #317, 20.12638776789572503 ) ;
#3913 = CARTESIAN_POINT ( 'NONE',  ( 11.87221919846740015, 1491.806965132240066, 208.7302600617219923 ) ) ;
#3914 = EDGE_CURVE ( 'NONE', #42052, #70558, #6856, .T. ) ;
#3915 = ORIENTED_EDGE ( 'NONE', *, *, #80879, .T. ) ;
#3916 = ORIENTED_EDGE ( 'NONE', *, *, #24375, .F. ) ;
#3917 = DIRECTION ( 'NONE',  ( -0.000000000000000000, -1.000000000000000000, -0.000000000000000000 ) ) ;
#3918 = CARTESIAN_POINT ( 'NONE',  ( -18.69648219331439876, 1441.918081136590217, 210.3870465119969992 ) ) ;
#3919 = CARTESIAN_POINT ( 'NONE',  ( -3.467940602053699806, 1495.562067921990092, 197.2905559617530002 ) ) ;
#3920 = CARTESIAN_POINT ( 'NONE',  ( 29.04422735952528356, 1509.932355432719078, 214.2352895502645822 ) ) ;
#3921 = CARTESIAN_POINT ( 'NONE',  ( -20.18061928985329700, 1494.280760705760031, 190.7832826676969660 ) ) ;
#3922 = CARTESIAN_POINT ( 'NONE',  ( -14.46094609939999920, 1420.539308687509902, 213.8039270598989958 ) ) ;
#3923 = CARTESIAN_POINT ( 'NONE',  ( 31.97146249857578937, 1524.678872986499073, 201.5731023188606912 ) ) ;
#3924 = CARTESIAN_POINT ( 'NONE',  ( -7.878537825433329367, 1522.051704408389924, 218.1850669711710111 ) ) ;
#3925 = CARTESIAN_POINT ( 'NONE',  ( -10.68726663944961963, 1366.700119988787719, 210.6218459617030021 ) ) ;
#3926 = CARTESIAN_POINT ( 'NONE',  ( 31.22294729666619162, 1523.678648413191695, 195.3480975247479705 ) ) ;
#3927 = CARTESIAN_POINT ( 'NONE',  ( -19.39871373709999958, 1468.954201919629895, 192.1830138438979816 ) ) ;
#3928 = CARTESIAN_POINT ( 'NONE',  ( -0.7579263249019989601, 1516.927039499179955, 207.4176752179770347 ) ) ;
#3929 = CARTESIAN_POINT ( 'NONE',  ( -13.16556780021149820, 1435.937898916229869, 150.6367019297510126 ) ) ;
#3930 = CARTESIAN_POINT ( 'NONE',  ( -8.022927361009998037, 1384.932834884869862, 218.7874485825090005 ) ) ;
#3931 = ADVANCED_FACE ( 'NONE', ( #49428 ), #87143, .F. ) ;
#3932 = AXIS2_PLACEMENT_3D ( 'NONE', #72929, #107068, #65081 ) ;
#3933 = CARTESIAN_POINT ( 'NONE',  ( 0.7132214971689999627, 1416.830000968330069, 190.3250594539979943 ) ) ;
#3934 = CARTESIAN_POINT ( 'NONE',  ( 0.7572375962070010402, 1498.197839107489926, 197.8134798819990010 ) ) ;
#3935 = CARTESIAN_POINT ( 'NONE',  ( -3.675448282928950317, 1497.092948350399865, 201.5013805017089794 ) ) ;
#3936 = VERTEX_POINT ( 'NONE', #96380 ) ;
#3937 = CARTESIAN_POINT ( 'NONE',  ( 10.01186952689999821, 1415.800370255129792, 244.5548898179980029 ) ) ;
#3938 = CARTESIAN_POINT ( 'NONE',  ( -21.52036872800000111, 1488.680653138530261, 194.1608577479979942 ) ) ;
#3940 = CARTESIAN_POINT ( 'NONE',  ( -16.99430611709999894, 1409.506514629130152, 195.5583755198979929 ) ) ;
#3939 = CARTESIAN_POINT ( 'NONE',  ( -10.67517646397909914, 1425.711402707339857, 92.74368930566500069 ) ) ;
#3941 = EDGE_CURVE ( 'NONE', #20620, #41312, #69230, .T. ) ;
#3942 = CARTESIAN_POINT ( 'NONE',  ( 2.086548178679999754, 1515.551704408389924, 205.2922258481490303 ) ) ;
#3943 = CARTESIAN_POINT ( 'NONE',  ( -31.20802388730000132, 1430.369980854730102, 248.1710554681980057 ) ) ;
#3944 = CARTESIAN_POINT ( 'NONE',  ( 1.088119754170000064, 1486.968603087390193, 219.9165972894990091 ) ) ;
#3945 = CARTESIAN_POINT ( 'NONE',  ( 2.595924361719925244, 1448.352474427002562, 154.6961829228227145 ) ) ;
#3946 = CARTESIAN_POINT ( 'NONE',  ( -24.07938165869598635, 1410.986708706416493, 208.6133297288818653 ) ) ;
#3947 = ORIENTED_EDGE ( 'NONE', *, *, #888, .T. ) ;
#3948 = CARTESIAN_POINT ( 'NONE',  ( 3.433722984520000132, 1396.093883862429948, 197.4759704522980144 ) ) ;
#3949 = CARTESIAN_POINT ( 'NONE',  ( 14.77683004841523307, 1514.552098284236536, 225.3854720466699462 ) ) ;
#3950 = DIRECTION ( 'NONE',  ( 0.000000000000000000, 1.000000000000000000, 0.000000000000000000 ) ) ;
#3951 = ORIENTED_EDGE ( 'NONE', *, *, #14255, .F. ) ;
#3952 = ORIENTED_EDGE ( 'NONE', *, *, #50407, .F. ) ;
#3953 = CARTESIAN_POINT ( 'NONE',  ( -3.078458355199999996, 1384.777566036459802, 199.6697850883389833 ) ) ;
#3954 = CARTESIAN_POINT ( 'NONE',  ( 7.207469458989999467, 1424.355561564639856, 194.9835187250990032 ) ) ;
#3955 = VERTEX_POINT ( 'NONE', #1792 ) ;
#3956 = AXIS2_PLACEMENT_3D ( 'NONE', #18061, #95892, #34874 ) ;
#3957 = CARTESIAN_POINT ( 'NONE',  ( -1.083446969300000173, 1419.332833902230050, 184.9378854065980136 ) ) ;
#3958 = CARTESIAN_POINT ( 'NONE',  ( -10.57419901610000146, 1462.298693876490006, 208.7178814602820012 ) ) ;
#3959 = CARTESIAN_POINT ( 'NONE',  ( -0.7728793615600000333, 1479.776535910530129, 236.0727651660979802 ) ) ;
#3960 = DIRECTION ( 'NONE',  ( 1.755985294532464991E-16, -1.000000000000000000, 1.338183447452830017E-16 ) ) ;
#3961 = ORIENTED_EDGE ( 'NONE', *, *, #103402, .F. ) ;
#3962 = CARTESIAN_POINT ( 'NONE',  ( 11.15486294749999985, 1425.160588235329897, 144.1660541351980100 ) ) ;
#3963 = CARTESIAN_POINT ( 'NONE',  ( -12.28605913130100014, 1415.088506334920112, 220.9685418577669793 ) ) ;
#3964 = CARTESIAN_POINT ( 'NONE',  ( 15.25203479360000181, 1496.671131138630017, 225.4162514494980201 ) ) ;
#3965 = EDGE_LOOP ( 'NONE', ( #93778, #97741 ) ) ;
#3966 =( BOUNDED_CURVE ( )  B_SPLINE_CURVE ( 3, ( #54667, #63085, #97184, #80398 ),
 .UNSPECIFIED., .F., .F. ) 
 B_SPLINE_CURVE_WITH_KNOTS ( ( 4, 4 ),
 ( 2.226350983651550042, 2.864757500696315073 ),
 .UNSPECIFIED. ) 
 CURVE ( )  GEOMETRIC_REPRESENTATION_ITEM ( )  RATIONAL_B_SPLINE_CURVE ( ( 1.000000000000000000, 0.9663238299975769330, 0.9663238299975769330, 1.000000000000000000 ) ) 
 REPRESENTATION_ITEM ( '' )  );
#3967 = CARTESIAN_POINT ( 'NONE',  ( 1.121383591734999907, 1517.104192383289956, 204.4960559556369901 ) ) ;
#3968 = ORIENTED_EDGE ( 'NONE', *, *, #56195, .T. ) ;
#3969 = CARTESIAN_POINT ( 'NONE',  ( 0.000000000000000000, 1408.913060387329779, 217.9908631324380224 ) ) ;
#3970 = CIRCLE ( 'NONE', #14650, 2.000000000000003553 ) ;
#3971 = CARTESIAN_POINT ( 'NONE',  ( 13.50539683911128108, 1444.074071570348224, 187.9928544899986775 ) ) ;
#3972 = ORIENTED_EDGE ( 'NONE', *, *, #93708, .T. ) ;
#3973 = ORIENTED_EDGE ( 'NONE', *, *, #65486, .F. ) ;
#3974 = CARTESIAN_POINT ( 'NONE',  ( 0.6235920161070117596, 1525.878013734321485, 175.2961586039432120 ) ) ;
#3975 = CARTESIAN_POINT ( 'NONE',  ( -3.644778954545839778, 1508.551704408389924, 219.9243067801160123 ) ) ;
#3976 = CARTESIAN_POINT ( 'NONE',  ( -22.42121221859999736, 1409.696026370929985, 207.7819003571480039 ) ) ;
#3977 = CARTESIAN_POINT ( 'NONE',  ( -7.960864549025298942, 1469.836596664489889, 216.0273995464790175 ) ) ;
#3978 = CARTESIAN_POINT ( 'NONE',  ( 14.98330790116689926, 1452.389831745899983, 147.8685068122100006 ) ) ;
#3979 = CARTESIAN_POINT ( 'NONE',  ( 8.765728093939998189, 1421.055606564249956, 196.4760046562989828 ) ) ;
#3980 = CARTESIAN_POINT ( 'NONE',  ( -18.02257621027557377, 1526.382868172863937, 235.3484976865589147 ) ) ;
#3981 = CARTESIAN_POINT ( 'NONE',  ( -108.2868634315222067, 1380.916857273249434, 298.2057793955574425 ) ) ;
#3982 = CARTESIAN_POINT ( 'NONE',  ( 11.12152504562100042, 1478.725870727130086, 205.8941487266770025 ) ) ;
#3983 = CARTESIAN_POINT ( 'NONE',  ( 0.03647752878835780477, 1409.823935006122611, 233.1203796024890380 ) ) ;
#3984 = CARTESIAN_POINT ( 'NONE',  ( -12.78476385600000143, 1502.707311016190033, 209.0177136757029928 ) ) ;
#3985 = CARTESIAN_POINT ( 'NONE',  ( 12.26636271253249966, 1421.698877206780026, 207.4435041203790036 ) ) ;
#3986 = CARTESIAN_POINT ( 'NONE',  ( -24.07281716570090069, 1508.277182899829995, 222.3373729421060148 ) ) ;
#3987 = CARTESIAN_POINT ( 'NONE',  ( -6.658917469454999960, 1512.371207877090001, 200.8892782097470047 ) ) ;
#3988 = ORIENTED_EDGE ( 'NONE', *, *, #12337, .F. ) ;
#3989 = CARTESIAN_POINT ( 'NONE',  ( 3.804422481160000036, 1422.873164470030133, 234.3916895958979865 ) ) ;
#3990 = CIRCLE ( 'NONE', #54111, 2.000000000000008882 ) ;
#3991 = CARTESIAN_POINT ( 'NONE',  ( 41.66134420550000073, 1443.796851579070108, 135.6885409488979803 ) ) ;
#3992 = CARTESIAN_POINT ( 'NONE',  ( -81.63072053611109880, 1384.989726998269816, 304.8882203442400396 ) ) ;
#3993 = CARTESIAN_POINT ( 'NONE',  ( 4.133200439670000392, 1506.299374241689975, 220.1647597449990030 ) ) ;
#3994 = LINE ( 'NONE', #105332, #99178 ) ;
#3995 = EDGE_LOOP ( 'NONE', ( #51836, #93827, #100561, #103653, #100469 ) ) ;
#3996 = CARTESIAN_POINT ( 'NONE',  ( 2.022791977769999860, 1430.155356877590066, 217.3490746647090077 ) ) ;
#3997 = CARTESIAN_POINT ( 'NONE',  ( 16.55212241053982325, 1524.756004293092246, 237.4472295103155091 ) ) ;
#3998 = CARTESIAN_POINT ( 'NONE',  ( -16.09575332200000020, 1416.289980099749982, 209.1849711052219902 ) ) ;
#3999 = CARTESIAN_POINT ( 'NONE',  ( -0.1852938298213350210, 1430.295842153490185, 199.7081761581629848 ) ) ;
#4000 = CARTESIAN_POINT ( 'NONE',  ( 13.86270800413499948, 1513.875858217480072, 225.8871191791669730 ) ) ;
#4001 = CARTESIAN_POINT ( 'NONE',  ( -19.53786426058999481, 1512.187213306747481, 236.7197124308268030 ) ) ;
#4002 = CARTESIAN_POINT ( 'NONE',  ( 27.79924491104030082, 1510.012621779409983, 222.8077676732789882 ) ) ;
#4003 = CARTESIAN_POINT ( 'NONE',  ( 7.679909121233859715, 1460.810760006640066, 203.1061546417070076 ) ) ;
#4004 = DIRECTION ( 'NONE',  ( 0.9983395709201744461, 0.05760296116452706672, 0.000000000000000000 ) ) ;
#4005 = CARTESIAN_POINT ( 'NONE',  ( 9.414868078959999664, 1419.756125693529839, 230.5038554507980280 ) ) ;
#4006 = CARTESIAN_POINT ( 'NONE',  ( 9.549000552458089430, 1470.075890067440014, 212.3436661921319910 ) ) ;
#4007 = CARTESIAN_POINT ( 'NONE',  ( -19.37374569213905318, 1526.382868172863937, 234.3668155954421479 ) ) ;
#4008 = CARTESIAN_POINT ( 'NONE',  ( -2.494758036134999912, 1516.937508036699910, 207.4208181092269854 ) ) ;
#4009 = CARTESIAN_POINT ( 'NONE',  ( 44.24543032989999602, 1429.800888227629912, 267.6618094214979919 ) ) ;
#4010 = CARTESIAN_POINT ( 'NONE',  ( -18.02631345340000024, 1410.039226335029980, 224.3300098786980072 ) ) ;
#4011 = CARTESIAN_POINT ( 'NONE',  ( 19.94495958220000276, 1435.193444768860218, 143.8622995873980130 ) ) ;
#4012 = CARTESIAN_POINT ( 'NONE',  ( 21.33447918899999962, 1508.013007766330020, 191.0177302433980344 ) ) ;
#4013 = CARTESIAN_POINT ( 'NONE',  ( 29.73445058744768588, 1509.991226363751821, 208.3164907507077714 ) ) ;
#4014 = CARTESIAN_POINT ( 'NONE',  ( -26.93323766929999863, 1469.218382335129945, 266.6753116650979791 ) ) ;
#4015 = CARTESIAN_POINT ( 'NONE',  ( 18.19590854888146580, 1522.382868172863937, 180.0410247165184217 ) ) ;
#4016 = CARTESIAN_POINT ( 'NONE',  ( -40.58566290280030131, 1442.151355276100048, 136.9330292898360142 ) ) ;
#4017 = CARTESIAN_POINT ( 'NONE',  ( 0.2174939161106619889, 1453.161012291630186, 183.2464846872150304 ) ) ;
#4018 = CARTESIAN_POINT ( 'NONE',  ( -15.29352652250000055, 1409.447122101729974, 207.7760784791980200 ) ) ;
#4019 = CYLINDRICAL_SURFACE ( 'NONE', #68164, 0.9999999999999985567 ) ;
#4020 = CARTESIAN_POINT ( 'NONE',  ( 20.64339891394559601, 1523.429859730330236, 179.9837476533122640 ) ) ;
#4021 = CARTESIAN_POINT ( 'NONE',  ( -7.702631097496129620, 1383.525349896430043, 218.9204624055510067 ) ) ;
#4022 = CARTESIAN_POINT ( 'NONE',  ( 2.554632337009709708, 1456.353935948870230, 219.4317766317170140 ) ) ;
#4023 = CARTESIAN_POINT ( 'NONE',  ( -37.65468647916719647, 1436.753545005770093, 134.0999999968539953 ) ) ;
#4024 = DIRECTION ( 'NONE',  ( -0.8775825618903722036, 0.000000000000000000, -0.4794255386042038936 ) ) ;
#4025 = ORIENTED_EDGE ( 'NONE', *, *, #48403, .F. ) ;
#4026 = CARTESIAN_POINT ( 'NONE',  ( 6.288919081391354027, 1510.947107034761302, 216.5507387054137496 ) ) ;
#4027 = CARTESIAN_POINT ( 'NONE',  ( -4.185613592979979813, 1409.059225234809901, 223.5095492053650048 ) ) ;
#4028 = CARTESIAN_POINT ( 'NONE',  ( -11.02808036529999924, 1492.177362994390023, 209.7513178175030077 ) ) ;
#4029 = CARTESIAN_POINT ( 'NONE',  ( -3.660988608500000296, 1468.712036633390198, 189.5324782634990015 ) ) ;
#4030 = CARTESIAN_POINT ( 'NONE',  ( 15.87566433304780311, 1507.597587122909999, 231.8003883547650048 ) ) ;
#4031 = CARTESIAN_POINT ( 'NONE',  ( -27.10654211919999668, 1469.521092463829973, 267.5396841185980179 ) ) ;
#4032 = CARTESIAN_POINT ( 'NONE',  ( 3.347801439296147041, 1523.382868172864164, 176.1543725841967500 ) ) ;
#4033 = CARTESIAN_POINT ( 'NONE',  ( 18.79734767819999774, 1416.844618642430078, 209.8348600039379903 ) ) ;
#4034 = CARTESIAN_POINT ( 'NONE',  ( -27.50473206080000210, 1509.873546795530046, 216.5854941500080031 ) ) ;
#4035 = CARTESIAN_POINT ( 'NONE',  ( -88.81502644064428864, 1384.621400043609810, 308.2893549430740450 ) ) ;
#4036 = CARTESIAN_POINT ( 'NONE',  ( -37.08409534967810117, 1384.983166705460008, 210.3120036977730081 ) ) ;
#4037 = CARTESIAN_POINT ( 'NONE',  ( -12.22358767350790032, 1490.666492278739724, 208.1734027058400045 ) ) ;
#4038 = CARTESIAN_POINT ( 'NONE',  ( 20.61567397870000207, 1508.364961461330040, 227.6869092844980003 ) ) ;
#4039 = CARTESIAN_POINT ( 'NONE',  ( -27.28051563420000036, 1451.961389759230087, 135.3445407374979936 ) ) ;
#4040 = CARTESIAN_POINT ( 'NONE',  ( 33.91369110979979951, 1435.681798629080049, 135.0664268281979901 ) ) ;
#4041 = ADVANCED_FACE ( 'NONE', ( #9601 ), #9961, .T. ) ;
#4043 = ORIENTED_EDGE ( 'NONE', *, *, #59929, .T. ) ;
#4042 = CARTESIAN_POINT ( 'NONE',  ( 2.183428632720000095, 1507.960443100289922, 217.8271517235889974 ) ) ;
#4044 = CARTESIAN_POINT ( 'NONE',  ( -109.4838093930000014, 1384.905744133400049, 311.2841432912590562 ) ) ;
#4045 = DIRECTION ( 'NONE',  ( 1.000000000000000000, 0.000000000000000000, 0.000000000000000000 ) ) ;
#4046 = B_SPLINE_CURVE_WITH_KNOTS ( 'NONE', 3,
 ( #45936, #72249, #3393, #105842, #46498, #38072, #21231, #12861, #82820, #40821, #67152, #41388, #82278 ),
 .UNSPECIFIED., .F., .F.,
 ( 4, 2, 2, 1, 2, 2, 4 ),
 ( 0.000000000000000000, 0.2499999999998752664, 0.3749999999998002709, 0.4374999999998336331, 0.4687499999998503974, 0.4999999999998672173, 1.000000000000000000 ),
 .UNSPECIFIED. ) ;
#4047 = CARTESIAN_POINT ( 'NONE',  ( -11.18708202009999830, 1500.025273076890244, 211.2389607902390196 ) ) ;
#4048 = CARTESIAN_POINT ( 'NONE',  ( -12.22173834910000068, 1416.311719782429918, 194.7110039421980048 ) ) ;
#4049 = CARTESIAN_POINT ( 'NONE',  ( -0.5536948142769980707, 1422.303198269830091, 193.2759312063989796 ) ) ;
#4050 = EDGE_CURVE ( 'NONE', #29796, #77481, #97817, .T. ) ;
#4051 = CARTESIAN_POINT ( 'NONE',  ( 22.29596073799999800, 1409.691652492829917, 210.9314411838980163 ) ) ;
#4052 = CARTESIAN_POINT ( 'NONE',  ( -107.0252682235529988, 1391.913060387289988, 306.7492100420760153 ) ) ;
#4053 = CARTESIAN_POINT ( 'NONE',  ( -18.69626595349999931, 1468.616571719990134, 201.1221850591790030 ) ) ;
#4054 = CARTESIAN_POINT ( 'NONE',  ( -15.95047594089999876, 1421.629085502230055, 227.1824928441980092 ) ) ;
#4056 = CARTESIAN_POINT ( 'NONE',  ( -11.72622114699999862, 1378.269058748980115, 205.1826066712690135 ) ) ;
#4055 = CARTESIAN_POINT ( 'NONE',  ( -11.87124624760000025, 1432.722071916729874, 149.9814472446979892 ) ) ;
#4057 = CARTESIAN_POINT ( 'NONE',  ( 28.25140913253650155, 1508.152706006489780, 209.3868776241489797 ) ) ;
#4058 = CARTESIAN_POINT ( 'NONE',  ( -100.5161172129000136, 1371.894749952189613, 291.3379631701586732 ) ) ;
#4059 = CARTESIAN_POINT ( 'NONE',  ( 16.53242990339596474, 1526.073434386619283, 235.9344106296537120 ) ) ;
#4060 = CARTESIAN_POINT ( 'NONE',  ( -22.99101922890000083, 1415.988654013429823, 211.3100808865079898 ) ) ;
#4061 = B_SPLINE_CURVE_WITH_KNOTS ( 'NONE', 5,
 ( #8258, #49197, #100666, #42423, #101206, #42992, #17185, #109100, #84432, #16100, #77150, #68760, #15545, #110733, #67654, #34023, #454 ),
 .UNSPECIFIED., .F., .F.,
 ( 6, 2, 3, 3, 3, 6 ),
 ( 50.96205257140000100, 60.48206970939999394, 67.46372249629999374, 67.82259044730000141, 68.73290467190000186, 70.00206443017889058 ),
 .UNSPECIFIED. ) ;
#4062 = CARTESIAN_POINT ( 'NONE',  ( 0.05823133897709759782, 1360.390585217549869, 210.6218459616991936 ) ) ;
#4063 = CARTESIAN_POINT ( 'NONE',  ( 4.028630584655000568, 1516.812923327049930, 205.6617440802170051 ) ) ;
#4064 = CARTESIAN_POINT ( 'NONE',  ( -18.97892456421369900, 1485.957843142680076, 189.4647141020179788 ) ) ;
#4065 = EDGE_LOOP ( 'NONE', ( #105815, #40794, #21686, #105689, #86561 ) ) ;
#4066 = CARTESIAN_POINT ( 'NONE',  ( 3.281831459213320201, 1466.303209658950209, 198.5678429405679992 ) ) ;
#4067 = CARTESIAN_POINT ( 'NONE',  ( -11.36636202294226727, 1422.064850992264837, 210.6381225563648911 ) ) ;
#4069 = EDGE_LOOP ( 'NONE', ( #72525, #55858, #37367, #105994, #72756 ) ) ;
#4068 = CARTESIAN_POINT ( 'NONE',  ( -68.16711561486698656, 1379.746493480949994, 279.7015904451550341 ) ) ;
#4070 = ORIENTED_EDGE ( 'NONE', *, *, #85135, .F. ) ;
#4071 = CARTESIAN_POINT ( 'NONE',  ( 28.28536618100000055, 1509.154939139430098, 210.5349106460980124 ) ) ;
#4072 = ORIENTED_EDGE ( 'NONE', *, *, #106151, .T. ) ;
#4073 = CARTESIAN_POINT ( 'NONE',  ( 2.563005697779590086, 1485.055789815510025, 220.6962468248860034 ) ) ;
#4074 = LINE ( 'NONE', #62914, #42142 ) ;
#4076 = CARTESIAN_POINT ( 'NONE',  ( 1.126797019860000137, 1507.655509662929717, 181.0315140402979921 ) ) ;
#4075 = CARTESIAN_POINT ( 'NONE',  ( 15.77284072136830240, 1413.861949724670012, 191.4239925061509950 ) ) ;
#4077 = CARTESIAN_POINT ( 'NONE',  ( 6.594885160195530283, 1463.733219486340204, 209.8009738102450115 ) ) ;
#4078 = CARTESIAN_POINT ( 'NONE',  ( -23.91746435257450187, 1452.077846361179809, 136.8095616623199930 ) ) ;
#4079 = CARTESIAN_POINT ( 'NONE',  ( 10.67939883587730066, 1438.711029782762353, 152.5177852837198600 ) ) ;
#4080 = CARTESIAN_POINT ( 'NONE',  ( 5.754827835269999525, 1409.281567319030046, 230.5672434926979975 ) ) ;
#4081 = CARTESIAN_POINT ( 'NONE',  ( 12.52297189095030028, 1501.145799326159931, 211.3282646751150082 ) ) ;
#4082 =( NAMED_UNIT ( * ) PLANE_ANGLE_UNIT ( ) SI_UNIT ( $, .RADIAN. ) );
#4083 = B_SPLINE_CURVE_WITH_KNOTS ( 'NONE', 3,
 ( #106969, #5060, #39206, #89615, #73383, #22381, #31360, #49840, #26263 ),
 .UNSPECIFIED., .F., .F.,
 ( 4, 1, 2, 2, 4 ),
 ( 0.000000000000000000, 0.2500000000002982614, 0.3750000000003418932, 0.5000000000003855805, 1.000000000000000000 ),
 .UNSPECIFIED. ) ;
#4084 = CARTESIAN_POINT ( 'NONE',  ( 40.38917806159109603, 1448.047423120819985, 134.0999999983369833 ) ) ;
#4085 = CARTESIAN_POINT ( 'NONE',  ( 2.824339754329999952, 1434.323903598489778, 204.0183183669190043 ) ) ;
#4086 = ORIENTED_EDGE ( 'NONE', *, *, #51369, .T. ) ;
#4087 = CARTESIAN_POINT ( 'NONE',  ( -17.51543818720000090, 1417.552356044260023, 206.7803260803289902 ) ) ;
#4088 = CARTESIAN_POINT ( 'NONE',  ( -16.02330256640034634, 1410.858424892926678, 226.7269707842006881 ) ) ;
#4089 = VERTEX_POINT ( 'NONE', #17991 ) ;
#4090 = ORIENTED_EDGE ( 'NONE', *, *, #91097, .F. ) ;
#4091 = ORIENTED_EDGE ( 'NONE', *, *, #25305, .T. ) ;
#4092 = CARTESIAN_POINT ( 'NONE',  ( -6.715925881185000001, 1514.199187793469946, 216.9011106608170110 ) ) ;
#4093 = CARTESIAN_POINT ( 'NONE',  ( 16.20149547506775534, 1514.624327907797579, 194.2555113716582582 ) ) ;
#4094 = CARTESIAN_POINT ( 'NONE',  ( 15.15576445393604033, 1451.146651684196740, 149.6210827369275762 ) ) ;
#4095 = CARTESIAN_POINT ( 'NONE',  ( -8.023454095920000029, 1384.914900298040038, 218.7875189542389762 ) ) ;
#4096 = B_SPLINE_CURVE_WITH_KNOTS ( 'NONE', 3,
 ( #25862, #52214, #60621, #10187, #2379, #26997, #27545, #1252, #35391, #37042 ),
 .UNSPECIFIED., .F., .F.,
 ( 4, 2, 2, 2, 4 ),
 ( 0.000000000000000000, 0.0007406479101618162336, 0.001481295820323632467, 0.002221943730485448701, 0.002962591640647264934 ),
 .UNSPECIFIED. ) ;
#4097 = LINE ( 'NONE', #37131, #3243 ) ;
#4098 = CARTESIAN_POINT ( 'NONE',  ( -68.38408895284545963, 1379.747196019225385, 279.2321024377919798 ) ) ;
#4099 = CARTESIAN_POINT ( 'NONE',  ( 2.024278636110000029, 1464.636130398189835, 199.4774878893790060 ) ) ;
#4100 = CARTESIAN_POINT ( 'NONE',  ( -0.7397222527619999877, 1507.631725827129912, 231.9097525726980109 ) ) ;
#4101 = CARTESIAN_POINT ( 'NONE',  ( 3.747720459029999951, 1415.426091369230107, 191.4590206283980081 ) ) ;
#4102 = CARTESIAN_POINT ( 'NONE',  ( -55.49204166402299876, 1384.646788494520024, 234.8063369579010100 ) ) ;
#4103 = VERTEX_POINT ( 'NONE', #62253 ) ;
#4104 = CARTESIAN_POINT ( 'NONE',  ( 7.321193707744999557, 1516.534976163889951, 206.8301696586770220 ) ) ;
#4105 = EDGE_LOOP ( 'NONE', ( #83933, #6129, #93015, #63228 ) ) ;
#4106 = CARTESIAN_POINT ( 'NONE',  ( 23.86424463509850113, 1440.913060387330006, 235.1402480613069770 ) ) ;
#4107 = CARTESIAN_POINT ( 'NONE',  ( 11.31476318222129862, 1478.684671585819842, 206.0074932402150125 ) ) ;
#4108 = EDGE_LOOP ( 'NONE', ( #11879, #6944, #90929, #2996 ) ) ;
#4109 = CARTESIAN_POINT ( 'NONE',  ( -7.966081143649218710, 1384.918389534460175, 199.4892681243580057 ) ) ;
#4110 = CARTESIAN_POINT ( 'NONE',  ( -16.31417794970000301, 1410.855162238230150, 191.5236355156980039 ) ) ;
#4111 = CARTESIAN_POINT ( 'NONE',  ( -22.75992825160000166, 1415.999881831630091, 212.0429175123080086 ) ) ;
#4113 = LINE ( 'NONE', #31338, #74209 ) ;
#4112 = CARTESIAN_POINT ( 'NONE',  ( -24.36543176699999691, 1441.018317148199912, 211.6908555921579875 ) ) ;
#4114 = CARTESIAN_POINT ( 'NONE',  ( 22.53630099147500232, 1411.012929146719898, 206.1992209292300231 ) ) ;
#4115 = CARTESIAN_POINT ( 'NONE',  ( -20.99191405665301247, 1509.583341913562435, 229.4942967042139799 ) ) ;
#4116 = CARTESIAN_POINT ( 'NONE',  ( 23.58347146439999875, 1410.948704344629959, 266.7402917337980170 ) ) ;
#4117 = DIRECTION ( 'NONE',  ( 0.9991156138703696232, -3.961952592064073292E-33, -0.04204747460233797945 ) ) ;
#4118 = CARTESIAN_POINT ( 'NONE',  ( -22.69876404240115519, 1522.382868172864164, 181.3483716558183119 ) ) ;
#4120 = CARTESIAN_POINT ( 'NONE',  ( -11.60004869885203682, 1424.140773632030005, 136.0101406525482162 ) ) ;
#4119 = CARTESIAN_POINT ( 'NONE',  ( 4.576117726849999734, 1464.329345424329858, 235.6418306423979914 ) ) ;
#4121 = CARTESIAN_POINT ( 'NONE',  ( 0.7538707352880020807, 1516.719999691880048, 216.0603247549969979 ) ) ;
#4122 = CARTESIAN_POINT ( 'NONE',  ( -27.74152896854549866, 1446.393007474169963, 137.1637341980870133 ) ) ;
#4123 = DIRECTION ( 'NONE',  ( 0.8236474686107853049, -0.5669078173018522460, 0.01484500364079644613 ) ) ;
#4124 = CARTESIAN_POINT ( 'NONE',  ( 19.22487415824295098, 1443.387065727409436, 213.3559128720396529 ) ) ;
#4125 = CARTESIAN_POINT ( 'NONE',  ( 6.561995960394999550, 1517.083030555940013, 212.3803205491769859 ) ) ;
#4126 = EDGE_CURVE ( 'NONE', #68079, #18109, #30589, .T. ) ;
#4127 = CARTESIAN_POINT ( 'NONE',  ( -18.05542495219999921, 1416.825784017130218, 209.4840452931509844 ) ) ;
#4128 = CARTESIAN_POINT ( 'NONE',  ( 29.86461515634917774, 1525.960063244516959, 220.9690070206021062 ) ) ;
#4130 = ORIENTED_EDGE ( 'NONE', *, *, #86035, .T. ) ;
#4129 = CARTESIAN_POINT ( 'NONE',  ( -4.720855738540000068, 1427.997322581190019, 206.3545885669889799 ) ) ;
#4131 = CARTESIAN_POINT ( 'NONE',  ( 13.10606020890036838, 1522.051704408389924, 225.8214468947291493 ) ) ;
#4132 = CARTESIAN_POINT ( 'NONE',  ( 29.14244786389999931, 1446.680133728120154, 238.0755343184980006 ) ) ;
#4133 = EDGE_CURVE ( 'NONE', #94093, #78014, #64274, .T. ) ;
#4134 = CARTESIAN_POINT ( 'NONE',  ( 10.47511427260239891, 1482.040461736080033, 210.7458695605469927 ) ) ;
#4135 = CARTESIAN_POINT ( 'NONE',  ( -14.79119396799999997, 1415.837009589480203, 205.0101417669090154 ) ) ;
#4136 = EDGE_CURVE ( 'NONE', #61054, #22898, #54923, .T. ) ;
#4137 = CARTESIAN_POINT ( 'NONE',  ( 8.373664385848250902, 1414.913060387329779, 195.2168834859115236 ) ) ;
#4138 = CARTESIAN_POINT ( 'NONE',  ( 16.81049281788159178, 1526.143142182266047, 182.6472226615215675 ) ) ;
#4140 = CARTESIAN_POINT ( 'NONE',  ( 19.74164165809999716, 1455.376033653930108, 226.0788330262979855 ) ) ;
#4139 = CARTESIAN_POINT ( 'NONE',  ( -21.42362349770000307, 1457.441058934229886, 222.6620133773979830 ) ) ;
#4141 = CARTESIAN_POINT ( 'NONE',  ( -2.793441807180000236, 1486.025323702830065, 182.0741001059980135 ) ) ;
#4142 = EDGE_LOOP ( 'NONE', ( #40394, #38865, #62593, #78516 ) ) ;
#4143 = CARTESIAN_POINT ( 'NONE',  ( -6.559798094425000059, 1516.987478262539980, 204.5068286042669854 ) ) ;
#4144 = CARTESIAN_POINT ( 'NONE',  ( 2.076955596959999983, 1406.811590412529995, 269.6487031941979922 ) ) ;
#4145 = CARTESIAN_POINT ( 'NONE',  ( 1.842963430059999963, 1515.219201257890063, 213.4472514052690144 ) ) ;
#4146 = CARTESIAN_POINT ( 'NONE',  ( 42.89777864911530258, 1451.794179102650105, 270.1114872296610088 ) ) ;
#4147 = DIRECTION ( 'NONE',  ( 0.000000000000000000, -1.000000000000000000, 0.000000000000000000 ) ) ;
#4148 = CARTESIAN_POINT ( 'NONE',  ( -4.500000000000000000, 1411.429641636930000, 137.0999999980979851 ) ) ;
#4149 = DIRECTION ( 'NONE',  ( -5.980589973904019347E-17, 1.000000000000000000, -1.736889445713099699E-16 ) ) ;
#4150 = CARTESIAN_POINT ( 'NONE',  ( -5.931789999490000298, 1459.036866685989935, 218.1324649368089865 ) ) ;
#4151 = CARTESIAN_POINT ( 'NONE',  ( -1.612833274716345411, 1450.726624143510662, 183.2858275704341793 ) ) ;
#4152 = CARTESIAN_POINT ( 'NONE',  ( 2.425481792534780023, 1449.557072643099900, 154.2478782046509878 ) ) ;
#4153 = CARTESIAN_POINT ( 'NONE',  ( -14.44521984438740070, 1416.640375558069991, 221.3789857444529900 ) ) ;
#4154 = CARTESIAN_POINT ( 'NONE',  ( 17.88677872281977344, 1428.781882675516044, 191.8785727744143799 ) ) ;
#4155 = EDGE_CURVE ( 'NONE', #24424, #77584, #66711, .T. ) ;
#4156 = ORIENTED_EDGE ( 'NONE', *, *, #71920, .F. ) ;
#4157 = CARTESIAN_POINT ( 'NONE',  ( 5.773159728049999117E-15, 1422.873164470030133, 234.3916895801979763 ) ) ;
#4158 = CARTESIAN_POINT ( 'NONE',  ( 2.500000000000000000, 1439.615672362369878, 170.5246407132979982 ) ) ;
#4159 = CARTESIAN_POINT ( 'NONE',  ( -0.2158985180920000024, 1475.983168668529743, 267.2349487566980315 ) ) ;
#4160 = CARTESIAN_POINT ( 'NONE',  ( -27.26775404520000023, 1451.960960096730105, 134.9110166487979825 ) ) ;
#4161 = DIRECTION ( 'NONE',  ( 0.07285353650440702655, -0.004327861288661672377, 0.9973332601670652497 ) ) ;
#4162 = CARTESIAN_POINT ( 'NONE',  ( -2.981021339944338155, 1448.268954114771532, 184.4415419840244681 ) ) ;
#4163 = CARTESIAN_POINT ( 'NONE',  ( -26.14268957564699747, 1384.842186362059920, 224.5499447472220140 ) ) ;
#4164 = CARTESIAN_POINT ( 'NONE',  ( -105.1761031979999927, 1379.258906148879987, 302.7941945437589766 ) ) ;
#4165 = CARTESIAN_POINT ( 'NONE',  ( 8.389588760568322812, 1511.399594748087793, 204.5238464867746302 ) ) ;
#4166 = CARTESIAN_POINT ( 'NONE',  ( -6.206590242792029422, 1396.129799296749752, 218.2548821234479988 ) ) ;
#4167 = CARTESIAN_POINT ( 'NONE',  ( -3.328126825706799963, 1508.551704408389924, 204.2788038780209945 ) ) ;
#4168 = CARTESIAN_POINT ( 'NONE',  ( -45.63712941939999723, 1440.913060387330006, 268.9747522934979997 ) ) ;
#4169 = ORIENTED_EDGE ( 'NONE', *, *, #52921, .T. ) ;
#4170 = ADVANCED_FACE ( 'NONE', ( #109599 ), #49705, .T. ) ;
#4171 = CARTESIAN_POINT ( 'NONE',  ( -3.767256085520910514, 1436.652614717099823, 227.2392139179829940 ) ) ;
#4172 = CARTESIAN_POINT ( 'NONE',  ( 2.935740814629999917, 1409.954265555830034, 231.6094213276980156 ) ) ;
#4173 = CARTESIAN_POINT ( 'NONE',  ( -19.91075572344583478, 1526.211523310372513, 233.5136430000777921 ) ) ;
#4175 = CARTESIAN_POINT ( 'NONE',  ( -12.07722023366500075, 1511.957228877180114, 194.2728863314669923 ) ) ;
#4174 = CARTESIAN_POINT ( 'NONE',  ( 11.03988486929999979, 1426.047781454529968, 101.9056521216979974 ) ) ;
#4176 = CARTESIAN_POINT ( 'NONE',  ( -12.37499353609999986, 1445.063428794549964, 151.6327898328030130 ) ) ;
#4177 = CARTESIAN_POINT ( 'NONE',  ( 2.872208710164999790, 1517.145312756229941, 201.7840522196070197 ) ) ;
#4178 = CARTESIAN_POINT ( 'NONE',  ( 7.763749353059999692, 1427.458563954329975, 212.5755154428889853 ) ) ;
#4179 = CARTESIAN_POINT ( 'NONE',  ( -21.47379552819999660, 1487.892728108790152, 202.0847255913190281 ) ) ;
#4180 = CARTESIAN_POINT ( 'NONE',  ( 2.641544985019999903, 1509.028982294729985, 179.6267714488979834 ) ) ;
#4181 = CARTESIAN_POINT ( 'NONE',  ( 7.684243075114999932, 1511.930588878439949, 206.3551010095970071 ) ) ;
#4182 = CARTESIAN_POINT ( 'NONE',  ( -56.99285471647699808, 1379.895685281439910, 259.6123875215530461 ) ) ;
#4183 = CARTESIAN_POINT ( 'NONE',  ( 9.231361398829999843, 1366.659448741839924, 207.6218459616989946 ) ) ;
#4185 = ORIENTED_EDGE ( 'NONE', *, *, #91619, .T. ) ;
#4184 = CARTESIAN_POINT ( 'NONE',  ( 8.768686371710000316, 1452.910156834589998, 212.7670267765590211 ) ) ;
#4186 = ORIENTED_EDGE ( 'NONE', *, *, #47356, .F. ) ;
#4187 = CARTESIAN_POINT ( 'NONE',  ( -13.37869501641699621, 1446.597784270054717, 188.1529856935966336 ) ) ;
#4188 = CARTESIAN_POINT ( 'NONE',  ( -4.487249791936469556, 1509.038615938009798, 212.6094384014929801 ) ) ;
#4189 = CARTESIAN_POINT ( 'NONE',  ( -4.616861546623686863, 1516.666407247929328, 201.4093550276068072 ) ) ;
#4190 = CARTESIAN_POINT ( 'NONE',  ( 3.066583199566000534E-32, 1507.508085020990166, 209.1218459616989946 ) ) ;
#4191 = CARTESIAN_POINT ( 'NONE',  ( 8.486299124169999430, 1519.913060387329779, 230.6230627099979813 ) ) ;
#4192 = CARTESIAN_POINT ( 'NONE',  ( -2.900859510217989268, 1441.812960597777874, 200.7451303979236741 ) ) ;
#4194 = LINE ( 'NONE', #82555, #96942 ) ;
#4193 = CARTESIAN_POINT ( 'NONE',  ( -9.075785912040000625, 1383.961100907409900, 218.5571957096990161 ) ) ;
#4195 = CARTESIAN_POINT ( 'NONE',  ( 2.112541014579999654, 1410.305346947330008, 185.4714011601980133 ) ) ;
#4196 =( LENGTH_UNIT ( ) NAMED_UNIT ( * ) SI_UNIT ( .MILLI., .METRE. ) );
#4197 = DIRECTION ( 'NONE',  ( 0.8775825618903727587, 9.629649721936177897E-33, 0.4794255386042027833 ) ) ;
#4198 = CARTESIAN_POINT ( 'NONE',  ( 41.01675760900570111, 1440.827364353530129, 136.2625528850119849 ) ) ;
#4199 = CARTESIAN_POINT ( 'NONE',  ( 8.051433653212120234, 1396.194222647300194, 216.6959449344469988 ) ) ;
#4200 = CARTESIAN_POINT ( 'NONE',  ( 1.546949757679999760, 1416.828040475729949, 190.2227908450980181 ) ) ;
#4201 = CARTESIAN_POINT ( 'NONE',  ( 11.27689108819999930, 1430.486160747730082, 151.2803084875980062 ) ) ;
#4202 = CYLINDRICAL_SURFACE ( 'NONE', #48337, 12.50000000000001066 ) ;
#4203 = EDGE_LOOP ( 'NONE', ( #36861, #13976, #3900, #60788 ) ) ;
#4204 = CARTESIAN_POINT ( 'NONE',  ( -17.19739463999676232, 1525.960063244516959, 181.9833109756550868 ) ) ;
#4205 = CARTESIAN_POINT ( 'NONE',  ( 12.60696393929999992, 1442.571107480210003, 187.6656753080980025 ) ) ;
#4206 = VERTEX_POINT ( 'NONE', #57562 ) ;
#4207 = VERTEX_POINT ( 'NONE', #99516 ) ;
#4208 = EDGE_CURVE ( 'NONE', #40999, #32037, #63879, .T. ) ;
#4209 = CARTESIAN_POINT ( 'NONE',  ( 11.45399678350000094, 1491.761485200589959, 209.6397955211830038 ) ) ;
#4210 = CARTESIAN_POINT ( 'NONE',  ( -14.05757250470000130, 1460.648840866229875, 232.1449230562979835 ) ) ;
#4211 = CARTESIAN_POINT ( 'NONE',  ( -15.56469051740000076, 1506.798305107229908, 193.1680121121979994 ) ) ;
#4212 = EDGE_CURVE ( 'NONE', #87841, #64698, #103156, .T. ) ;
#4213 = CARTESIAN_POINT ( 'NONE',  ( -29.30029655192942784, 1525.907212628473872, 196.8717316207789736 ) ) ;
#4214 = CARTESIAN_POINT ( 'NONE',  ( -5.775236830874999505, 1516.804776704140068, 214.1294346171470124 ) ) ;
#4215 = CARTESIAN_POINT ( 'NONE',  ( -13.72133526636149981, 1380.332343284469971, 209.6969764857090013 ) ) ;
#4216 = B_SPLINE_SURFACE_WITH_KNOTS ( 'NONE', 2, 5, ( 
 ( #29177, #20211, #54410, #97483, #88542, #52193 ),
 ( #86322, #9606, #77927, #95284, #86874, #20751 ),
 ( #31919, #106434, #22388, #106975, #89622, #66111 ) ),
 .UNSPECIFIED., .F., .F., .F.,
 ( 3, 3 ),
 ( 6, 6 ),
 ( 1.399803019379999958, 2.016961153080000013 ),
 ( 0.000000000000000000, 1.000000000000000000 ),
 .UNSPECIFIED. ) ;
#4217 = ORIENTED_EDGE ( 'NONE', *, *, #64472, .T. ) ;
#4218 = CARTESIAN_POINT ( 'NONE',  ( -14.39828244561829962, 1509.511548947660003, 182.8869702195129889 ) ) ;
#4219 = CARTESIAN_POINT ( 'NONE',  ( -56.57961477790000515, 1375.243914315939946, 252.6055042413589717 ) ) ;
#4220 = CARTESIAN_POINT ( 'NONE',  ( 2.628012963020000203, 1414.971287085229960, 225.5952605496979970 ) ) ;
#4221 = CARTESIAN_POINT ( 'NONE',  ( -1.713317447804999949, 1516.660388280709867, 204.5138242629670060 ) ) ;
#4222 = ORIENTED_EDGE ( 'NONE', *, *, #9770, .F. ) ;
#4223 = DIRECTION ( 'NONE',  ( 1.755985294532469921E-16, -1.000000000000000000, 1.338183447452831989E-16 ) ) ;
#4224 = CARTESIAN_POINT ( 'NONE',  ( -37.99384790316972982, 1427.843275130108395, 269.5760518878157086 ) ) ;
#4225 = CARTESIAN_POINT ( 'NONE',  ( -2.903727783739999957, 1409.519113742730042, 232.3413682034979786 ) ) ;
#4227 = ORIENTED_EDGE ( 'NONE', *, *, #87834, .F. ) ;
#4226 = CARTESIAN_POINT ( 'NONE',  ( -6.940379574320000522, 1431.113060387329824, 191.4151908640980082 ) ) ;
#4228 = CARTESIAN_POINT ( 'NONE',  ( -0.01304059463119639981, 1452.815422809060010, 183.2381944397329789 ) ) ;
#4229 = CARTESIAN_POINT ( 'NONE',  ( -31.46900625217390157, 1440.913060388669919, 242.6984041783090049 ) ) ;
#4230 = CARTESIAN_POINT ( 'NONE',  ( -22.68195036590000058, 1384.853989887049920, 222.0405270882590116 ) ) ;
#4231 = DIRECTION ( 'NONE',  ( 0.4978433412588735285, 0.000000000000000000, 0.8672669759446630655 ) ) ;
#4232 = EDGE_CURVE ( 'NONE', #101078, #99658, #20918, .T. ) ;
#4233 = CARTESIAN_POINT ( 'NONE',  ( 43.48861604073940157, 1436.533985799180073, 270.3367144192989713 ) ) ;
#4234 = CARTESIAN_POINT ( 'NONE',  ( -6.935457963315000640, 1516.627618683580067, 212.5772239474869991 ) ) ;
#4235 = CARTESIAN_POINT ( 'NONE',  ( -67.66215561869999817, 1379.745947391239952, 277.8420489690590216 ) ) ;
#4236 = CARTESIAN_POINT ( 'NONE',  ( 22.61598442209999860, 1409.702807929629898, 208.8472236539830078 ) ) ;
#4237 = CARTESIAN_POINT ( 'NONE',  ( -7.738877702543442538, 1425.750511251113039, 225.8955623955143039 ) ) ;
#4238 = CARTESIAN_POINT ( 'NONE',  ( -31.32995031131179786, 1523.678648413191922, 221.9013357025049231 ) ) ;
#4240 = EDGE_CURVE ( 'NONE', #49508, #63015, #65316, .T. ) ;
#4239 = CARTESIAN_POINT ( 'NONE',  ( -7.714148301377419692, 1516.729697371079965, 209.8385372711610160 ) ) ;
#4241 = CARTESIAN_POINT ( 'NONE',  ( 5.786847739675000213, 1517.104497701820037, 209.8595134730280165 ) ) ;
#4242 = CARTESIAN_POINT ( 'NONE',  ( 28.15443155984639745, 1509.896245780209938, 217.4026704617729990 ) ) ;
#4243 = CARTESIAN_POINT ( 'NONE',  ( -8.414414886229998558, 1415.366749018530072, 230.7044676890980099 ) ) ;
#4244 = CARTESIAN_POINT ( 'NONE',  ( -81.17886098919998972, 1384.990453609069846, 304.9592558327589700 ) ) ;
#4245 = EDGE_CURVE ( 'NONE', #45310, #77584, #107936, .T. ) ;
#4246 = EDGE_LOOP ( 'NONE', ( #1324, #22500, #53830, #103827, #58472 ) ) ;
#4247 = CARTESIAN_POINT ( 'NONE',  ( -25.62888669017269905, 1385.253130175059823, 224.1332055726419981 ) ) ;
#4248 = FACE_OUTER_BOUND ( 'NONE', #102284, .T. ) ;
#4249 = CARTESIAN_POINT ( 'NONE',  ( 49.24962907673571522, 1526.382868172863937, 407.9033880519289710 ) ) ;
#4250 = EDGE_CURVE ( 'NONE', #21185, #25603, #101356, .T. ) ;
#4251 = CARTESIAN_POINT ( 'NONE',  ( -20.32972594443840109, 1508.870366473410058, 229.0186719067029912 ) ) ;
#4252 = CARTESIAN_POINT ( 'NONE',  ( -24.90010528315330163, 1441.007489120919900, 210.4306619437199970 ) ) ;
#4253 = CARTESIAN_POINT ( 'NONE',  ( 11.03115274839999849, 1422.777860647609941, 206.2455307242489937 ) ) ;
#4254 = CARTESIAN_POINT ( 'NONE',  ( 0.5537922756022227722, 1498.600653688011789, 197.8120951424002385 ) ) ;
#4255 = VECTOR ( 'NONE', #76634, 1000.000000000000000 ) ;
#4256 = ADVANCED_FACE ( 'NONE', ( #40182 ), #87121, .T. ) ;
#4258 = CARTESIAN_POINT ( 'NONE',  ( -110.8380420702032580, 1377.913060387289988, 302.6609578876201567 ) ) ;
#4257 = CARTESIAN_POINT ( 'NONE',  ( 3.261635932824999973, 1516.613881697390070, 216.0569793506570022 ) ) ;
#4259 = CARTESIAN_POINT ( 'NONE',  ( -25.82242192641380640, 1450.787213346408635, 136.8648991040845431 ) ) ;
#4260 = CARTESIAN_POINT ( 'NONE',  ( 11.39902737117300013, 1471.112819660780133, 209.6184962109379910 ) ) ;
#4261 = ORIENTED_EDGE ( 'NONE', *, *, #105010, .F. ) ;
#4262 = CARTESIAN_POINT ( 'NONE',  ( 7.716878902974999122, 1516.833976295079992, 201.7919207096969672 ) ) ;
#4263 = CARTESIAN_POINT ( 'NONE',  ( -14.84895963876499891, 1511.957228877180114, 221.1990661657670216 ) ) ;
#4264 = ORIENTED_EDGE ( 'NONE', *, *, #83036, .T. ) ;
#4265 = CARTESIAN_POINT ( 'NONE',  ( -15.91746622356501462, 1512.594959757389915, 220.0895646873669875 ) ) ;
#4266 = ADVANCED_FACE ( 'NONE', ( #31777 ), #65964, .T. ) ;
#4267 = CIRCLE ( 'NONE', #88344, 1.999999999999994893 ) ;
#4268 =( BOUNDED_CURVE ( )  B_SPLINE_CURVE ( 3, ( #41739, #8674, #52376, #75898 ),
 .UNSPECIFIED., .F., .F. ) 
 B_SPLINE_CURVE_WITH_KNOTS ( ( 4, 4 ),
 ( 5.498078030758629886, 7.068189173309639806 ),
 .UNSPECIFIED. ) 
 CURVE ( )  GEOMETRIC_REPRESENTATION_ITEM ( )  RATIONAL_B_SPLINE_CURVE ( ( 1.000000000000000000, 0.8048993259320535998, 0.8048993259320535998, 1.000000000000000000 ) ) 
 REPRESENTATION_ITEM ( '' )  );
#4269 = FACE_OUTER_BOUND ( 'NONE', #9190, .T. ) ;
#4270 = CARTESIAN_POINT ( 'NONE',  ( 8.544339041751733532, 1424.594794760930426, 195.7981282794199842 ) ) ;
#4271 = EDGE_CURVE ( 'NONE', #33840, #61557, #45293, .T. ) ;
#4272 = CARTESIAN_POINT ( 'NONE',  ( 2.744355238500000294, 1442.847804213789914, 217.5784138281389914 ) ) ;
#4273 = CARTESIAN_POINT ( 'NONE',  ( -27.12205470637029947, 1509.520315501660207, 201.2360477619779999 ) ) ;
#4274 = CARTESIAN_POINT ( 'NONE',  ( -3.115733350010000180, 1446.573609257150110, 168.9983159514980002 ) ) ;
#4275 = CARTESIAN_POINT ( 'NONE',  ( -19.63221898369999963, 1426.793815849529892, 223.9042199868979992 ) ) ;
#4276 = CARTESIAN_POINT ( 'NONE',  ( -24.00430195510000075, 1435.335597340879985, 137.4619936623980152 ) ) ;
#4277 = CARTESIAN_POINT ( 'NONE',  ( -5.268918391659049405, 1464.422126824970292, 199.4426748585790108 ) ) ;
#4278 = CARTESIAN_POINT ( 'NONE',  ( 17.67025347690000103, 1478.544842878630106, 189.4270408572980102 ) ) ;
#4280 = CARTESIAN_POINT ( 'NONE',  ( -18.93601566932215974, 1438.893878115886309, 210.4432051349708104 ) ) ;
#4279 = CARTESIAN_POINT ( 'NONE',  ( -105.5774848019999865, 1391.233264612319999, 302.6220608442590105 ) ) ;
#4281 = ADVANCED_FACE ( 'NONE', ( #102821 ), #24028, .F. ) ;
#4282 = DIRECTION ( 'NONE',  ( 0.000000000000000000, -1.000000000000000000, 0.000000000000000000 ) ) ;
#4283 = ORIENTED_EDGE ( 'NONE', *, *, #31051, .F. ) ;
#4284 = CIRCLE ( 'NONE', #32863, 1.999999999999999556 ) ;
#4285 = CARTESIAN_POINT ( 'NONE',  ( -105.5846564840000070, 1377.935450406140035, 304.0481634900589825 ) ) ;
#4286 = CARTESIAN_POINT ( 'NONE',  ( -8.927975590540000894, 1508.479955638390038, 219.0952217288690065 ) ) ;
#4287 = DIRECTION ( 'NONE',  ( 5.980589973904019347E-17, -1.000000000000000000, 1.736889445713099699E-16 ) ) ;
#4288 = EDGE_CURVE ( 'NONE', #37685, #65412, #87722, .T. ) ;
#4289 = CARTESIAN_POINT ( 'NONE',  ( 31.55061275097025586, 1525.712830164893376, 201.2105093847520436 ) ) ;
#4290 = CARTESIAN_POINT ( 'NONE',  ( -2.572869546270000196, 1484.598564647389821, 198.5804750205990103 ) ) ;
#4291 = CARTESIAN_POINT ( 'NONE',  ( -18.52446843519999931, 1509.559949079530043, 231.7134234805980100 ) ) ;
#4292 = CARTESIAN_POINT ( 'NONE',  ( -3.351189091698004940, 1524.075132568163781, 242.0172129272094992 ) ) ;
#4293 = CARTESIAN_POINT ( 'NONE',  ( -12.90241536995782923, 1442.892915964137273, 186.4197113181899397 ) ) ;
#4294 = CARTESIAN_POINT ( 'NONE',  ( -16.81223226430000039, 1414.913060387329779, 207.5743821216680089 ) ) ;
#4295 = CARTESIAN_POINT ( 'NONE',  ( 5.485830631332369478, 1494.971428724189991, 220.2122593298520030 ) ) ;
#4296 = EDGE_CURVE ( 'NONE', #46346, #13675, #23821, .T. ) ;
#4297 = CARTESIAN_POINT ( 'NONE',  ( 16.50821402049999875, 1494.476688022989947, 193.0250027032990090 ) ) ;
#4298 = CARTESIAN_POINT ( 'NONE',  ( -15.41756489359970139, 1415.677402202029953, 209.3686558232799939 ) ) ;
#4299 = CARTESIAN_POINT ( 'NONE',  ( -108.9848104056970044, 1383.828915778130067, 311.1014354137989812 ) ) ;
#4300 = CARTESIAN_POINT ( 'NONE',  ( 0.04106552329005089957, 1516.946282269519997, 201.4020272027410101 ) ) ;
#4302 = ORIENTED_EDGE ( 'NONE', *, *, #103432, .F. ) ;
#4301 = CARTESIAN_POINT ( 'NONE',  ( -18.83362749532000180, 1444.184359083290019, 209.4102611290639970 ) ) ;
#4303 = FACE_OUTER_BOUND ( 'NONE', #46274, .T. ) ;
#4304 = CARTESIAN_POINT ( 'NONE',  ( 13.70533112961760125, 1512.850289816029772, 224.4308539454270033 ) ) ;
#4305 = VERTEX_POINT ( 'NONE', #28905 ) ;
#4306 = ORIENTED_EDGE ( 'NONE', *, *, #42966, .T. ) ;
#4307 = DIRECTION ( 'NONE',  ( -0.9942586961433765858, 0.000000000000000000, -0.1070030146457237041 ) ) ;
#4308 = CARTESIAN_POINT ( 'NONE',  ( -109.8956305769999915, 1384.931289674369964, 297.0283802634589847 ) ) ;
#4309 = CARTESIAN_POINT ( 'NONE',  ( 13.42980330897129271, 1443.474176595161225, 169.3652270005678133 ) ) ;
#4311 = CARTESIAN_POINT ( 'NONE',  ( -36.81312676959999663, 1443.228346179749906, 254.5659337120980013 ) ) ;
#4310 = CARTESIAN_POINT ( 'NONE',  ( 28.45946923949786012, 1418.491042720496353, 269.4551673254863431 ) ) ;
#4312 = CARTESIAN_POINT ( 'NONE',  ( -20.32961525440000017, 1499.106861559730078, 190.3279599699980054 ) ) ;
#4313 = CARTESIAN_POINT ( 'NONE',  ( -11.91439454699999878, 1433.379825245419852, 150.0311634427979754 ) ) ;
#4314 = LINE ( 'NONE', #13774, #71436 ) ;
#4315 = CARTESIAN_POINT ( 'NONE',  ( 11.63970458439030153, 1426.761200432619944, 137.2142808755380088 ) ) ;
#4316 = CARTESIAN_POINT ( 'NONE',  ( -1.725662463192670248, 1484.236887848700007, 182.7463278875050037 ) ) ;
#4317 = FACE_OUTER_BOUND ( 'NONE', #25471, .T. ) ;
#4318 = CARTESIAN_POINT ( 'NONE',  ( -1.130521170243829809, 1515.098624608320051, 213.4504088227829754 ) ) ;
#4319 = CARTESIAN_POINT ( 'NONE',  ( 16.66094735743510213, 1410.867388111209948, 226.5061907891179942 ) ) ;
#4320 = CARTESIAN_POINT ( 'NONE',  ( -10.91165881471389909, 1480.298603070810032, 213.5307502733419938 ) ) ;
#4321 = CARTESIAN_POINT ( 'NONE',  ( 3.107265622092247881, 1362.633694524574594, 209.6218459617148824 ) ) ;
#4322 = CARTESIAN_POINT ( 'NONE',  ( 32.59719044532401711, 1523.982201850120191, 201.1951351303495130 ) ) ;
#4323 = EDGE_CURVE ( 'NONE', #104484, #82244, #102171, .T. ) ;
#4325 = ORIENTED_EDGE ( 'NONE', *, *, #69514, .T. ) ;
#4324 = CARTESIAN_POINT ( 'NONE',  ( 1.482666866830270077E-09, 1410.677261243919929, 256.9622107588730273 ) ) ;
#4326 = EDGE_LOOP ( 'NONE', ( #107604, #1626, #83708, #46078 ) ) ;
#4327 = CARTESIAN_POINT ( 'NONE',  ( -11.86428414876309922, 1432.209070943210008, 149.9808888289879860 ) ) ;
#4328 = ADVANCED_FACE ( 'NONE', ( #37307 ), #105058, .F. ) ;
#4329 = CARTESIAN_POINT ( 'NONE',  ( 9.763688521220180050, 1493.202298044959889, 188.2888330414619986 ) ) ;
#4330 = CARTESIAN_POINT ( 'NONE',  ( -28.03279905679999828, 1464.673443976430008, 270.1137655723980515 ) ) ;
#4331 = CARTESIAN_POINT ( 'NONE',  ( 8.765535317279999461, 1421.152484001810080, 196.5454161687989938 ) ) ;
#4332 = CARTESIAN_POINT ( 'NONE',  ( -123.8569892972382007, 1368.558218059088176, 298.5091666679096534 ) ) ;
#4333 = DIRECTION ( 'NONE',  ( 0.7882878497005212370, 0.000000000000000000, -0.6153066438894746470 ) ) ;
#4334 = CARTESIAN_POINT ( 'NONE',  ( 0.2178157486290130118, 1452.982786607829894, 183.2541296479709843 ) ) ;
#4335 = CARTESIAN_POINT ( 'NONE',  ( -12.29554385710000020, 1419.827449229430158, 228.7908442235979862 ) ) ;
#4336 = CARTESIAN_POINT ( 'NONE',  ( -30.29107790644756903, 1523.847233649538339, 222.4926083870301454 ) ) ;
#4337 = CARTESIAN_POINT ( 'NONE',  ( -6.617556317490000062, 1459.313145877689976, 217.6703565655190005 ) ) ;
#4338 = CARTESIAN_POINT ( 'NONE',  ( 9.790769103959343411, 1362.302375259238488, 207.6218459616987673 ) ) ;
#4339 = CARTESIAN_POINT ( 'NONE',  ( -44.47864120876400307, 1432.224334038000052, 266.4559105170700377 ) ) ;
#4340 = ORIENTED_EDGE ( 'NONE', *, *, #37161, .T. ) ;
#4341 = CARTESIAN_POINT ( 'NONE',  ( -3.538009167994560222, 1496.111029204799934, 181.4461849933530004 ) ) ;
#4342 = CIRCLE ( 'NONE', #82972, 6.988489866870006395 ) ;
#4343 = ORIENTED_EDGE ( 'NONE', *, *, #104951, .T. ) ;
#4344 = ORIENTED_EDGE ( 'NONE', *, *, #78141, .T. ) ;
#4345 = CARTESIAN_POINT ( 'NONE',  ( 3.462948796544999652, 1516.956048353049937, 211.4063724288770061 ) ) ;
#4346 = EDGE_CURVE ( 'NONE', #91400, #14236, #53213, .T. ) ;
#4347 = CARTESIAN_POINT ( 'NONE',  ( -8.759590148488889838, 1447.855092709829933, 212.1632990431340033 ) ) ;
#4348 = CARTESIAN_POINT ( 'NONE',  ( -17.59976141832330043, 1419.797097700060021, 206.6695233765389901 ) ) ;
#4349 = CARTESIAN_POINT ( 'NONE',  ( -8.015707256689999838, 1470.460698177329732, 184.9071038282980055 ) ) ;
#4350 = B_SPLINE_CURVE_WITH_KNOTS ( 'NONE', 3,
 ( #14924, #82143, #55873, #65924, #13819, #65375, #98394, #39601, #73772, #107896, #37954, #38485, #106790, #72663, #55318, #13269, #12742, #91098, #73206, #49119, #99479, #23334, #64832, #46925, #56966, #30080, #100046, #4886, #14376, #82704, #81043, #89994, #4357, #106252, #29538, #107350, #63725, #47459, #97835, #39027, #30646, #8182, #17109, #32833, #40697, #92201, #76504, #15474, #77073, #51299, #33945, #110653, #7642, #24428, #93298, #16560, #83801, #41254, #68679, #101682, #32301, #66485, #92747, #50754, #84891, #58616, #16024, #17670, #102786, #109565, #26081, #93839, #60272, #382, #68139, #23873, #74869, #7098, #59719, #109018, #84351, #102250, #24971, #100592, #42349, #25529, #94390, #50223, #33380, #41796, #75956, #110107, #49669, #85436, #67576, #83251, #59178, #58069, #67027, #75428, #8734, #42917, #34503, #6547, #101133, #63476, #97595, #52431, #9853, #38773, #70352, #928, #20866, #64015, #104464, #72949, #44575, #78719, #35051, #38226, #36168, #107085, #98126, #30374, #47195, #4102, #103342, #43471, #86557, #29829, #9308, #52982, #13009, #4635, #89188, #72409, #87114, #44021, #69233, #61394, #55061, #10404, #95515, #94967, #55612, #2035, #81321, #89735, #21402, #12481, #64564, #98683, #18236, #29281, #18785, #106540, #78157, #51872, #86008, #69795, #46663, #77616, #26644, #60842, #1468, #80796, #35602, #103913, #27213, #57809, #57269, #40427, #74052, #39333, #81875, #73506, #82444, #92472, #65653, #23626, #6279, #15207, #109847, #41544, #75700, #107641, #99770, #23059, #66219, #47740, #74603, #65103, #5177, #66766, #30925, #99215, #14113, #33124, #82987, #22493, #100338, #91396, #15742, #5742, #49943, #56694, #91933, #90830, #49398, #84081, #14673, #39885, #21944, #109304, #48304, #83524, #108181, #6818, #100866, #108739, #32030, #48861, #40977, #75157, #31472, #32590, #24157, #58347, #7379, #67311, #56137, #90272, #13554, #51597, #76241, #68971, #25257, #18510, #68417, #60568, #653, #26373, #50504, #103072, #52707, #60009, #85180, #101408, #77896, #33668, #52156, #76792, #94688, #35336, #51047, #58896, #110388, #17961, #67860, #95246, #69525, #86289, #86842, #7923, #43745, #10134, #101971, #1203, #59460, #16300, #103645, #44306, #84626, #109, #34784, #9573, #42639, #34231, #35901, #78449, #16845, #42093, #8466, #26943, #61132, #1763, #24700, #93029, #93570, #102519, #25811, #94130, #17401, #9029, #85730, #43200, #77351, #89590, #45420, #20176, #79562, #45957, #46516, #11258 ),
 .UNSPECIFIED., .F., .F.,
 ( 4, 3, 3, 3, 3, 3, 3, 3, 3, 3, 3, 3, 3, 3, 3, 3, 3, 3, 3, 3, 3, 3, 3, 3, 3, 3, 3, 3, 3, 3, 3, 3, 3, 3, 3, 3, 3, 3, 3, 3, 3, 3, 3, 3, 3, 3, 3, 3, 3, 3, 3, 3, 3, 3, 3, 3, 3, 3, 3, 3, 3, 3, 3, 3, 3, 3, 3, 3, 3, 3, 3, 3, 3, 3, 3, 3, 3, 3, 3, 3, 3, 3, 3, 3, 3, 3, 3, 3, 3, 3, 3, 3, 3, 3, 3, 3, 3, 3, 3, 3, 3, 4 ),
 ( 8.528903892709999823, 10.11079874316899918, 11.96402179552659994, 13.55545591726709986, 14.93540995916639957, 15.39383910902119901, 16.53784965764519654, 17.65533335631520018, 18.74952487047229965, 19.85344026384639804, 20.89947257251949964, 21.93049568398669891, 22.94770232675979571, 23.95212381599139917, 24.93878849665829733, 25.91622982162849809, 26.88014850494499797, 27.58084801746479542, 28.63695919667589607, 29.71615375306799933, 30.81911651081409786, 31.94529991305369521, 33.12652436437380032, 34.29236762325579946, 35.45927563792669446, 36.61824151545220474, 37.81245501749270232, 38.92511934700599596, 40.01843177764789772, 41.08438201573959958, 41.39509552361419509, 42.90409533968830402, 44.42289876441959962, 45.95738695247120376, 47.50856733623960082, 49.07757088809649559, 50.66567512639480242, 52.27433300125469628, 53.93242794869799894, 55.59996648682680132, 57.29321361784219846, 59.01465425201970305, 60.78527615218369817, 62.58728134439490276, 64.44454181919989821, 65.53909258080051359, 67.04475135045599643, 68.62894058153921151, 70.27967536058729081, 72.01761458325029253, 73.87891071221881134, 75.94929923628670565, 78.63951486550050163, 80.97143900281349715, 82.94603025408429176, 84.75425470534629824, 86.41460430148269722, 88.01672707843430032, 89.54556736663739969, 90.91108773679130195, 93.82957164518428783, 96.80547043545971064, 99.57405818404620845, 102.2141381765199952, 104.7420692361749985, 107.1759481923769926, 109.5308444734030076, 111.7884715630940065, 113.9994590479840042, 116.1473335953590009, 117.6367619673870024, 119.0967884077180088, 120.5520899153760013, 122.0392533098840175, 123.4344489772180253, 124.8001882596219900, 126.1366051610670098, 127.4449720650600142, 128.7132937358369986, 129.9615380000630012, 131.2054675357509836, 132.4493970714400177, 133.6727958913919565, 135.0110548064769773, 136.6141698558100188, 138.3143900939450077, 139.6965082775570011, 140.9764010850390150, 142.1130208664269787, 143.2066028786510117, 144.2502205449540043, 144.8160795074840053, 146.1142711068380038, 147.4422065578220042, 148.8126880694590000, 150.2044901557419792, 151.6094053898760023, 153.0744782599189762, 154.4631086672829952, 155.8325814729020067, 157.1697943162390061, 157.4696968700480113 ),
 .UNSPECIFIED. ) ;
#4351 = LINE ( 'NONE', #91087, #37570 ) ;
#4352 = B_SPLINE_SURFACE_WITH_KNOTS ( 'NONE', 5, 5, ( 
 ( #24216, #49997, #41596, #75751, #109897, #67367 ),
 ( #84678, #90883, #14170, #24753, #58950, #93082 ),
 ( #16355, #7976, #42144, #110445, #69581, #103698 ),
 ( #18565, #61188, #93619, #16897, #104255, #95305 ),
 ( #43796, #60622, #76852, #85228, #35955, #43254 ),
 ( #77401, #10188, #94183, #34835, #35392, #26998 ) ),
 .UNSPECIFIED., .F., .F., .F.,
 ( 6, 6 ),
 ( 6, 6 ),
 ( 5.770254232290000118, 6.424361107539999338 ),
 ( 0.000000000000000000, 2.000000000000000000 ),
 .UNSPECIFIED. ) ;
#4353 = EDGE_LOOP ( 'NONE', ( #61123, #106543, #39984, #54937 ) ) ;
#4354 = CARTESIAN_POINT ( 'NONE',  ( 2.291514297774999598, 1517.194972660189933, 201.3955140066269962 ) ) ;
#4355 = ADVANCED_FACE ( 'NONE', ( #57438 ), #32207, .T. ) ;
#4356 = CARTESIAN_POINT ( 'NONE',  ( 1.110223024629999949E-15, 1377.913060387289988, 209.1218459616989946 ) ) ;
#4357 = CARTESIAN_POINT ( 'NONE',  ( -24.53717461995699978, 1384.543544838199978, 203.1111072970969929 ) ) ;
#4358 = EDGE_LOOP ( 'NONE', ( #50228, #35588, #67697, #74405 ) ) ;
#4359 = CARTESIAN_POINT ( 'NONE',  ( -26.95138969526639983, 1414.522592307069999, 270.1541509808739647 ) ) ;
#4360 = CARTESIAN_POINT ( 'NONE',  ( 3.460649750935970381, 1417.553534582059910, 232.5463249240959840 ) ) ;
#4361 = CARTESIAN_POINT ( 'NONE',  ( 9.634266010251048229, 1434.809772052239850, 207.3359404128959795 ) ) ;
#4362 = EDGE_CURVE ( 'NONE', #93315, #20179, #49242, .T. ) ;
#4364 = ORIENTED_EDGE ( 'NONE', *, *, #57291, .F. ) ;
#4363 = CARTESIAN_POINT ( 'NONE',  ( -8.968861126993214583, 1364.620492801554747, 207.6218459616988241 ) ) ;
#4365 = ORIENTED_EDGE ( 'NONE', *, *, #2554, .F. ) ;
#4366 = CARTESIAN_POINT ( 'NONE',  ( 45.62325630519739406, 1441.755915269380012, 268.9751291415536230 ) ) ;
#4367 = CARTESIAN_POINT ( 'NONE',  ( 11.39903530061180170, 1471.112746094619979, 209.6182361319149834 ) ) ;
#4368 = CARTESIAN_POINT ( 'NONE',  ( -13.45539595447709935, 1436.151332559189996, 150.5285823830119796 ) ) ;
#4369 = CARTESIAN_POINT ( 'NONE',  ( -19.75056259240000145, 1465.177823603190063, 209.1218459616989946 ) ) ;
#4370 = CARTESIAN_POINT ( 'NONE',  ( 0.7559394982620020187, 1516.972341476009888, 210.2438793621770117 ) ) ;
#4371 = CARTESIAN_POINT ( 'NONE',  ( -18.49337492746660061, 1415.724942517919999, 207.5698429335219828 ) ) ;
#4372 = CARTESIAN_POINT ( 'NONE',  ( -14.56134018280000042, 1420.166564076130044, 221.4975583820979921 ) ) ;
#4373 = CARTESIAN_POINT ( 'NONE',  ( 11.53430538779999992, 1415.163755998629995, 222.8574940093980103 ) ) ;
#4374 = EDGE_CURVE ( 'NONE', #105852, #62493, #63928, .T. ) ;
#4375 = CARTESIAN_POINT ( 'NONE',  ( 7.717016619025000246, 1511.440441732939917, 205.8449389055269876 ) ) ;
#4376 = VERTEX_POINT ( 'NONE', #6456 ) ;
#4377 = CARTESIAN_POINT ( 'NONE',  ( 4.995994787574999485, 1516.665179208830068, 206.6322283937570035 ) ) ;
#4378 = ORIENTED_EDGE ( 'NONE', *, *, #31531, .F. ) ;
#4379 = LINE ( 'NONE', #98415, #97351 ) ;
#4380 = CARTESIAN_POINT ( 'NONE',  ( -12.86122366611309964, 1416.830086716310007, 196.3807296669870084 ) ) ;
#4381 = EDGE_LOOP ( 'NONE', ( #1303, #84850, #25958, #73510, #92359 ) ) ;
#4382 = CARTESIAN_POINT ( 'NONE',  ( 7.356817058030821421, 1456.556113374074812, 227.5920619859562350 ) ) ;
#4383 = ADVANCED_FACE ( 'NONE', ( #64178 ), #47800, .T. ) ;
#4384 = CARTESIAN_POINT ( 'NONE',  ( 25.15894589063669784, 1451.153250808739813, 137.5682474387959928 ) ) ;
#4385 = CARTESIAN_POINT ( 'NONE',  ( 13.29661090509999966, 1415.048591087029763, 197.5746719060980183 ) ) ;
#4386 = CARTESIAN_POINT ( 'NONE',  ( -2.694739704345539888, 1517.151704408390060, 212.0779207114006510 ) ) ;
#4387 = CARTESIAN_POINT ( 'NONE',  ( 21.35641278199999959, 1409.658842758330138, 204.9228439656180285 ) ) ;
#4388 = B_SPLINE_CURVE_WITH_KNOTS ( 'NONE', 5,
 ( #32962, #32430, #90110, #76090, #88222, #34630 ),
 .UNSPECIFIED., .F., .F.,
 ( 6, 6 ),
 ( -1.999999982688239974, 0.000000000000000000 ),
 .UNSPECIFIED. ) ;
#4389 = CARTESIAN_POINT ( 'NONE',  ( -4.220676207128734703, 1446.230049502166139, 170.5366217123670083 ) ) ;
#4390 = CARTESIAN_POINT ( 'NONE',  ( -24.67107306660000177, 1435.359038600570102, 135.9357527513979846 ) ) ;
#4391 = CARTESIAN_POINT ( 'NONE',  ( -24.00203106780000084, 1421.760869654530097, 210.4932335677079891 ) ) ;
#4392 = CARTESIAN_POINT ( 'NONE',  ( 30.31940284289302667, 1523.456924617338245, 222.4933038711250219 ) ) ;
#4393 = CARTESIAN_POINT ( 'NONE',  ( 1.000433738244750126, 1452.575225918920069, 183.3871588569680284 ) ) ;
#4394 = EDGE_CURVE ( 'NONE', #92844, #75158, #90445, .T. ) ;
#4395 = CARTESIAN_POINT ( 'NONE',  ( 2.500000000000000000, 1439.450741841849776, 162.6867541768519914 ) ) ;
#4396 = CARTESIAN_POINT ( 'NONE',  ( -6.939219520934999608, 1516.783701990830195, 214.9027072062869763 ) ) ;
#4397 = ORIENTED_EDGE ( 'NONE', *, *, #51664, .F. ) ;
#4398 = CARTESIAN_POINT ( 'NONE',  ( 7.708877363402839578, 1516.528409826940106, 206.8600011716279994 ) ) ;
#4399 = CARTESIAN_POINT ( 'NONE',  ( -3.739222493130000213, 1474.769836386989937, 198.3144648466990247 ) ) ;
#4400 = FACE_OUTER_BOUND ( 'NONE', #92039, .T. ) ;
#4401 = EDGE_CURVE ( 'NONE', #39734, #98871, #3148, .T. ) ;
#4402 = FACE_OUTER_BOUND ( 'NONE', #81841, .T. ) ;
#4403 = CARTESIAN_POINT ( 'NONE',  ( -38.26793863361420733, 1448.575033566829916, 136.4135971887010044 ) ) ;
#4404 = CARTESIAN_POINT ( 'NONE',  ( 11.18796758460170615, 1425.276586956789288, 138.5633102189376018 ) ) ;
#4405 = CARTESIAN_POINT ( 'NONE',  ( 2.567982850141544926, 1417.735512785670153, 233.8238498394635201 ) ) ;
#4406 = CARTESIAN_POINT ( 'NONE',  ( -2.141398646916960136, 1471.330659375019877, 183.6643496123579951 ) ) ;
#4407 = CARTESIAN_POINT ( 'NONE',  ( 7.271052316819548444, 1517.051704408389924, 192.9032753742981470 ) ) ;
#4408 = DIRECTION ( 'NONE',  ( -7.436362843295819681E-17, 1.000000000000000000, -1.457576885956999882E-16 ) ) ;
#4409 = CARTESIAN_POINT ( 'NONE',  ( 36.09585466289570377, 1440.913060387229962, 253.0262047010989761 ) ) ;
#4410 = CARTESIAN_POINT ( 'NONE',  ( -109.7017504620000068, 1385.317244295069941, 297.1054320267589901 ) ) ;
#4411 = CARTESIAN_POINT ( 'NONE',  ( 8.452187789688819564, 1498.645326028860154, 200.1952072007560162 ) ) ;
#4412 = ORIENTED_EDGE ( 'NONE', *, *, #61891, .T. ) ;
#4413 = EDGE_CURVE ( 'NONE', #43546, #93315, #18458, .T. ) ;
#4414 = AXIS2_PLACEMENT_3D ( 'NONE', #92463, #60002, #33658 ) ;
#4415 = CARTESIAN_POINT ( 'NONE',  ( 10.55222728675549959, 1481.276343967989988, 208.5110256208110115 ) ) ;
#4416 = DIRECTION ( 'NONE',  ( 0.9990834534827314206, 0.04280481766341149436, 2.370275682555253978E-05 ) ) ;
#4417 = CARTESIAN_POINT ( 'NONE',  ( -2.183147893290000585, 1442.593045501889947, 200.4930349953090172 ) ) ;
#4418 = CARTESIAN_POINT ( 'NONE',  ( 1.734605482469999904, 1474.701058102730030, 235.0720776984979921 ) ) ;
#4420 = EDGE_CURVE ( 'NONE', #61381, #25667, #44294, .T. ) ;
#4419 = VECTOR ( 'NONE', #35940, 999.9999999999998863 ) ;
#4421 = CARTESIAN_POINT ( 'NONE',  ( 0.000000000000000000, 1398.755125754900064, 209.1218459616989946 ) ) ;
#4422 = CARTESIAN_POINT ( 'NONE',  ( -17.92485939079999824, 1509.539010270229937, 231.4769768637980007 ) ) ;
#4423 = CARTESIAN_POINT ( 'NONE',  ( -45.92082474586209884, 1383.818659492949791, 252.9957497693810069 ) ) ;
#4424 = CARTESIAN_POINT ( 'NONE',  ( 21.03123203779729877, 1507.789098030329797, 226.0655639048319756 ) ) ;
#4425 = CARTESIAN_POINT ( 'NONE',  ( 1.363639811660000145, 1415.765555525229956, 232.8698637559979829 ) ) ;
#4426 = CARTESIAN_POINT ( 'NONE',  ( -11.48593466557120024, 1501.387652528300123, 208.6966813591159848 ) ) ;
#4427 = CARTESIAN_POINT ( 'NONE',  ( 1.586086858110000053, 1465.659878105630014, 235.1389441440979908 ) ) ;
#4429 = ORIENTED_EDGE ( 'NONE', *, *, #64747, .F. ) ;
#4428 = CARTESIAN_POINT ( 'NONE',  ( -4.487249791936469556, 1509.038615938009798, 212.6094384014929801 ) ) ;
#4430 = CARTESIAN_POINT ( 'NONE',  ( -0.9209488051710000844, 1450.858101657689758, 181.8220196252979974 ) ) ;
#4431 = CARTESIAN_POINT ( 'NONE',  ( -39.64173303379999425, 1383.033670297620120, 212.5860353986090274 ) ) ;
#4432 = CARTESIAN_POINT ( 'NONE',  ( -3.544886644340000448, 1474.831256732490147, 198.2487847239990231 ) ) ;
#4434 = VERTEX_POINT ( 'NONE', #49028 ) ;
#4433 = CARTESIAN_POINT ( 'NONE',  ( -22.69876404240057965, 1522.382868172863937, 236.8953202675781426 ) ) ;
#4435 = CARTESIAN_POINT ( 'NONE',  ( -9.609618950303881135, 1464.248441293520273, 228.1966055971730043 ) ) ;
#4436 = ORIENTED_EDGE ( 'NONE', *, *, #58396, .F. ) ;
#4437 = PRODUCT_DEFINITION_SHAPE ( 'NONE', 'NONE',  #110840 ) ;
#4438 = CARTESIAN_POINT ( 'NONE',  ( -11.41029669623840093, 1391.349546573489988, 213.9346477860329969 ) ) ;
#4439 = CARTESIAN_POINT ( 'NONE',  ( -18.04214300190000131, 1416.520646107730045, 209.4829339742140064 ) ) ;
#4440 = CARTESIAN_POINT ( 'NONE',  ( 3.487585849186794817, 1508.611350403810775, 213.8000011204408963 ) ) ;
#4441 = CARTESIAN_POINT ( 'NONE',  ( -5.670189958209999936, 1463.356297375389886, 200.9627545900790153 ) ) ;
#4442 = CARTESIAN_POINT ( 'NONE',  ( -18.11157280723839946, 1509.545530446499924, 231.7129765844609892 ) ) ;
#4443 = CARTESIAN_POINT ( 'NONE',  ( 19.50214312291780416, 1509.609062993781436, 186.8947548611758407 ) ) ;
#4444 = CARTESIAN_POINT ( 'NONE',  ( 12.10652582572050129, 1409.335829585050078, 200.3615976011700184 ) ) ;
#4445 = FACE_OUTER_BOUND ( 'NONE', #2323, .T. ) ;
#4446 = CARTESIAN_POINT ( 'NONE',  ( 1.506876827590000190, 1419.080345689929800, 184.9340756889980071 ) ) ;
#4447 = CARTESIAN_POINT ( 'NONE',  ( 3995.588063464740117, 778.1435596157219834, 210.2211552457290225 ) ) ;
#4448 = CARTESIAN_POINT ( 'NONE',  ( -68.33454988889999981, 1379.748399532440089, 279.2380605676589767 ) ) ;
#4449 = CARTESIAN_POINT ( 'NONE',  ( -2.647176844829699949, 1448.931638480319862, 183.9391811989769678 ) ) ;
#4450 = EDGE_LOOP ( 'NONE', ( #106162, #109811, #97788, #44855 ) ) ;
#4451 = EDGE_LOOP ( 'NONE', ( #99966, #90579, #89723, #10007 ) ) ;
#4452 = CIRCLE ( 'NONE', #31287, 1.000000000000000000 ) ;
#4453 = CARTESIAN_POINT ( 'NONE',  ( -7.507423057800870048, 1508.880864719049896, 215.2619752906269923 ) ) ;
#4454 = CARTESIAN_POINT ( 'NONE',  ( -18.74447803847540328, 1442.135375080380072, 209.4108418761609869 ) ) ;
#4455 = CARTESIAN_POINT ( 'NONE',  ( -12.48153481890000016, 1434.603604361780071, 150.3555482973980020 ) ) ;
#4456 = CARTESIAN_POINT ( 'NONE',  ( 12.89015451259809986, 1420.977333543979967, 203.3411088897940147 ) ) ;
#4457 = CARTESIAN_POINT ( 'NONE',  ( -20.45011936773050110, 1503.010088104919987, 190.5302468752080074 ) ) ;
#4458 = CARTESIAN_POINT ( 'NONE',  ( -15.77822988280000160, 1420.228048065240046, 210.6636264438090222 ) ) ;
#4459 = CARTESIAN_POINT ( 'NONE',  ( -109.3962244350000077, 1384.944647467069899, 311.2791233102589672 ) ) ;
#4460 = CARTESIAN_POINT ( 'NONE',  ( -0.8791753874670000801, 1462.362773244929940, 182.9702177369979950 ) ) ;
#4461 = CARTESIAN_POINT ( 'NONE',  ( -10.78183993585174427, 1367.738238001941909, 208.3718459617010978 ) ) ;
#4462 = CARTESIAN_POINT ( 'NONE',  ( -5.242935297045000276, 1514.496907775670024, 217.7778693727470056 ) ) ;
#4463 = CARTESIAN_POINT ( 'NONE',  ( -20.04223814320000230, 1488.365800429130104, 192.0903004145979764 ) ) ;
#4464 = CARTESIAN_POINT ( 'NONE',  ( 4.026614479655000522, 1516.699825673279975, 207.4075116849170115 ) ) ;
#4465 = CARTESIAN_POINT ( 'NONE',  ( -9.901327976855469615, 1447.905481077269997, 209.8160867571170058 ) ) ;
#4466 = CARTESIAN_POINT ( 'NONE',  ( -11.93818408299999945, 1433.480074519959999, 149.8972116839979947 ) ) ;
#4467 = CARTESIAN_POINT ( 'NONE',  ( -13.79088340914820066, 1435.084318818310066, 149.2846745635849857 ) ) ;
#4468 = CARTESIAN_POINT ( 'NONE',  ( -8.034992631979999800, 1385.326470000059999, 218.7648172177289894 ) ) ;
#4469 = B_SPLINE_SURFACE_WITH_KNOTS ( 'NONE', 2, 5, ( 
 ( #30931, #5182, #32595, #55616, #13013, #81325 ),
 ( #73511, #65108, #99220, #22498, #59465, #76246 ),
 ( #93034, #17406, #77356, #84631, #114, #67316 ) ),
 .UNSPECIFIED., .F., .F., .F.,
 ( 3, 3 ),
 ( 6, 6 ),
 ( 1.399803019469999965, 2.016961153420000041 ),
 ( 0.000000000000000000, 1.000000000000000000 ),
 .UNSPECIFIED. ) ;
#4470 = CARTESIAN_POINT ( 'NONE',  ( 0.7133821232520000111, 1416.822694190629818, 190.3253679279979735 ) ) ;
#4471 = CARTESIAN_POINT ( 'NONE',  ( 0.2116392608170009904, 1497.592233828489952, 197.6910041071990065 ) ) ;
#4472 = CARTESIAN_POINT ( 'NONE',  ( -16.46632221292249909, 1492.699621139769988, 229.6814607386230023 ) ) ;
#4473 = ORIENTED_EDGE ( 'NONE', *, *, #96434, .T. ) ;
#4474 = CARTESIAN_POINT ( 'NONE',  ( -2.034726938789999869E-09, 1411.425360646529953, 255.2684106118979912 ) ) ;
#4475 = CARTESIAN_POINT ( 'NONE',  ( -27.39969416010000103, 1508.129222247830057, 204.7535242178479962 ) ) ;
#4477 = CARTESIAN_POINT ( 'NONE',  ( -1.514738108749209999, 1507.606285622480073, 232.0384771855580084 ) ) ;
#4476 = CARTESIAN_POINT ( 'NONE',  ( -10.66340896497400159, 1425.717702253409925, 91.95185177473790361 ) ) ;
#4478 = CARTESIAN_POINT ( 'NONE',  ( -4.375890055962693204, 1407.803708330174459, 270.1335399949743987 ) ) ;
#4479 = CARTESIAN_POINT ( 'NONE',  ( -20.03573726089999596, 1421.675448602630013, 240.3194873213979861 ) ) ;
#4480 = CARTESIAN_POINT ( 'NONE',  ( -0.8226521178380009625, 1486.661073111190035, 220.2963016106990040 ) ) ;
#4481 = CARTESIAN_POINT ( 'NONE',  ( -12.98226713004480004, 1414.913060387349788, 219.9156686614909972 ) ) ;
#4482 = CARTESIAN_POINT ( 'NONE',  ( 28.25319277509999694, 1450.638438602809856, 136.4121326236979996 ) ) ;
#4483 = ORIENTED_EDGE ( 'NONE', *, *, #87792, .F. ) ;
#4484 = CARTESIAN_POINT ( 'NONE',  ( -0.006135675924780000130, 1395.974572295429880, 197.4936679463980056 ) ) ;
#4485 = CARTESIAN_POINT ( 'NONE',  ( 14.16490606602967084, 1514.105081316843780, 225.7087563701193460 ) ) ;
#4486 = DIRECTION ( 'NONE',  ( -1.755985294532469921E-16, 1.000000000000000000, -1.338183447452831989E-16 ) ) ;
#4487 = ORIENTED_EDGE ( 'NONE', *, *, #6990, .F. ) ;
#4488 = VERTEX_POINT ( 'NONE', #80957 ) ;
#4489 = CIRCLE ( 'NONE', #24113, 1.000000000000000888 ) ;
#4490 = CARTESIAN_POINT ( 'NONE',  ( -2.274251696913569793E-15, 1384.485850024879937, 199.6505477045689929 ) ) ;
#4491 = CARTESIAN_POINT ( 'NONE',  ( -22.92752184622879952, 1409.723336632170231, 208.9617817198769671 ) ) ;
#4492 = ORIENTED_EDGE ( 'NONE', *, *, #36509, .T. ) ;
#4493 = CARTESIAN_POINT ( 'NONE',  ( 4.369728359379250193, 1508.879004046169939, 205.0024669094390219 ) ) ;
#4494 = CARTESIAN_POINT ( 'NONE',  ( 7.359652137679999484, 1491.427741686289892, 211.7193136839289878 ) ) ;
#4495 = CARTESIAN_POINT ( 'NONE',  ( -4.707600842899999805, 1479.769858085930082, 235.1404652853979940 ) ) ;
#4496 = CARTESIAN_POINT ( 'NONE',  ( 2.895368129540000002, 1444.422959043590026, 200.6322053094490059 ) ) ;
#4497 = VERTEX_POINT ( 'NONE', #81486 ) ;
#4498 = CARTESIAN_POINT ( 'NONE',  ( 10.81509838440000060, 1424.921163249430037, 144.1641696251980136 ) ) ;
#4499 = CARTESIAN_POINT ( 'NONE',  ( -13.15726445900019925, 1415.090956648730071, 220.8192894451659924 ) ) ;
#4500 = CARTESIAN_POINT ( 'NONE',  ( 14.44508776610000034, 1485.704772158630021, 225.7184853347980038 ) ) ;
#4501 = CARTESIAN_POINT ( 'NONE',  ( 4.612507273904999039, 1516.886345593249871, 204.1123678647870179 ) ) ;
#4502 = EDGE_LOOP ( 'NONE', ( #30495, #1703, #91330, #94161 ) ) ;
#4503 = CARTESIAN_POINT ( 'NONE',  ( 8.235190278047509693, 1482.696351514019852, 217.6054839274150083 ) ) ;
#4504 = EDGE_CURVE ( 'NONE', #18765, #44739, #106843, .T. ) ;
#4505 = DIRECTION ( 'NONE',  ( -0.1402804634174202869, 0.9901118076173992533, 0.000000000000000000 ) ) ;
#4506 = ORIENTED_EDGE ( 'NONE', *, *, #50041, .T. ) ;
#4507 = ORIENTED_EDGE ( 'NONE', *, *, #75832, .F. ) ;
#4508 = CARTESIAN_POINT ( 'NONE',  ( 2.180465155517681275, 1524.667648926078527, 173.9851435850430050 ) ) ;
#4509 = EDGE_CURVE ( 'NONE', #26609, #67105, #69280, .T. ) ;
#4510 = CARTESIAN_POINT ( 'NONE',  ( 16.89233068642487723, 1526.349684470114653, 234.8971439265459935 ) ) ;
#4511 = CARTESIAN_POINT ( 'NONE',  ( -22.51439127229999926, 1409.699280255230178, 208.1503399454410328 ) ) ;
#4512 = CARTESIAN_POINT ( 'NONE',  ( -14.35493914170010044, 1513.426431439620046, 193.9549492499340033 ) ) ;
#4513 = CARTESIAN_POINT ( 'NONE',  ( 12.79875861287509942, 1452.466117888040117, 149.2463358307309989 ) ) ;
#4514 = CARTESIAN_POINT ( 'NONE',  ( 10.39122783130000016, 1420.703789618900146, 197.9464487691990087 ) ) ;
#4515 = DIRECTION ( 'NONE',  ( 3.828568698926946970E-16, 0.000000000000000000, -1.000000000000000000 ) ) ;
#4516 = CARTESIAN_POINT ( 'NONE',  ( -6.418176471656730442, 1494.502784414770076, 198.6080641912510032 ) ) ;
#4517 = CARTESIAN_POINT ( 'NONE',  ( -18.70459388414779767, 1509.566239243649989, 231.7064163625079800 ) ) ;
#4518 = DIRECTION ( 'NONE',  ( 0.000000000000000000, 1.000000000000000000, 0.000000000000000000 ) ) ;
#4520 = CARTESIAN_POINT ( 'NONE',  ( 0.000000000000000000, 1384.913060387289988, 209.1218459572589836 ) ) ;
#4519 = CARTESIAN_POINT ( 'NONE',  ( -16.71917355490290191, 1412.654832539980134, 191.6875434529309814 ) ) ;
#4521 = DIRECTION ( 'NONE',  ( 5.980589973904019347E-17, -1.000000000000000000, 1.736889445713099699E-16 ) ) ;
#4522 = CARTESIAN_POINT ( 'NONE',  ( -24.02854066789229748, 1507.902906607559999, 222.3115874531950169 ) ) ;
#4523 = CARTESIAN_POINT ( 'NONE',  ( -7.466890204824999877, 1513.600111798330090, 202.4729951676269764 ) ) ;
#4524 = VERTEX_POINT ( 'NONE', #74233 ) ;
#4525 = CARTESIAN_POINT ( 'NONE',  ( 19.62446893450000118, 1438.771933937429822, 214.3676144197979738 ) ) ;
#4526 = CARTESIAN_POINT ( 'NONE',  ( -101.2221464535970057, 1384.943467076989918, 310.9552930315260255 ) ) ;
#4527 = EDGE_CURVE ( 'NONE', #73491, #86829, #88950, .T. ) ;
#4528 = VECTOR ( 'NONE', #7696, 1000.000000000000000 ) ;
#4529 = CARTESIAN_POINT ( 'NONE',  ( -9.481266696980000575, 1388.680743057909922, 201.1014716156689985 ) ) ;
#4530 = CARTESIAN_POINT ( 'NONE',  ( -15.69169271700000046, 1415.996555271789930, 210.3616365314589984 ) ) ;
#4532 = ORIENTED_EDGE ( 'NONE', *, *, #99080, .F. ) ;
#4531 = FACE_OUTER_BOUND ( 'NONE', #69074, .T. ) ;
#4533 = CARTESIAN_POINT ( 'NONE',  ( 3.880613242430000387, 1429.881321868690065, 216.9307363606289982 ) ) ;
#4534 = CARTESIAN_POINT ( 'NONE',  ( 16.64685887467730296, 1523.847248782568840, 237.7436681237527125 ) ) ;
#4535 = CARTESIAN_POINT ( 'NONE',  ( -14.00886230499999918, 1416.826388551330183, 221.8518116138980076 ) ) ;
#4536 = CARTESIAN_POINT ( 'NONE',  ( -2.282423313820620248, 1429.314140543729991, 200.0277053824169968 ) ) ;
#4537 = CARTESIAN_POINT ( 'NONE',  ( 11.87063484783499945, 1512.258183966700017, 225.5052044994669700 ) ) ;
#4538 = CARTESIAN_POINT ( 'NONE',  ( 1.047411759368620077, 1450.818007791970103, 181.4574043003410111 ) ) ;
#4539 = CARTESIAN_POINT ( 'NONE',  ( 3.587171487853899610, 1458.048446730460000, 200.0260115809859940 ) ) ;
#4540 = CARTESIAN_POINT ( 'NONE',  ( -4.159508860199999880, 1408.913060387329779, 226.9541261483979895 ) ) ;
#4541 = CARTESIAN_POINT ( 'NONE',  ( 4.446767511710000065, 1419.755698973330027, 231.8271342798979902 ) ) ;
#4542 = CARTESIAN_POINT ( 'NONE',  ( -21.19880661588985760, 1524.382868172863937, 233.5487980989313144 ) ) ;
#4543 = CARTESIAN_POINT ( 'NONE',  ( 2.282622912365000367, 1516.861367446839949, 206.8218623544969716 ) ) ;
#4544 = CARTESIAN_POINT ( 'NONE',  ( 45.69700908059999733, 1436.916749176230041, 266.4179775685979621 ) ) ;
#4545 = CARTESIAN_POINT ( 'NONE',  ( -18.78014126040000065, 1409.733562993129908, 222.2006764194979951 ) ) ;
#4546 = ADVANCED_FACE ( 'NONE', ( #51214 ), #93203, .T. ) ;
#4547 = CARTESIAN_POINT ( 'NONE',  ( 14.60160452979999945, 1435.005028509159956, 148.0399068081979976 ) ) ;
#4548 = CARTESIAN_POINT ( 'NONE',  ( -0.7136739638169999900, 1418.680438739629835, 228.0000072166980090 ) ) ;
#4549 = CARTESIAN_POINT ( 'NONE',  ( -16.10803554549259786, 1409.475565386449944, 193.1216181386560038 ) ) ;
#4550 = CARTESIAN_POINT ( 'NONE',  ( 12.45685414969999805, 1416.832348306829999, 223.4765384881980026 ) ) ;
#4551 = CARTESIAN_POINT ( 'NONE',  ( -14.21117982910179833, 1416.454926512799830, 203.1643232870270026 ) ) ;
#4552 = CARTESIAN_POINT ( 'NONE',  ( -40.49282606110470084, 1439.396725205129769, 135.6940988356820128 ) ) ;
#4553 = EDGE_CURVE ( 'NONE', #23910, #49801, #58521, .T. ) ;
#4554 = CARTESIAN_POINT ( 'NONE',  ( 0.2139245209313919704, 1455.148420693890102, 183.1612303901350174 ) ) ;
#4555 = CARTESIAN_POINT ( 'NONE',  ( -9.354904844460000035, 1409.239740863030192, 221.4829250259980142 ) ) ;
#4556 = CARTESIAN_POINT ( 'NONE',  ( 2.382436964801011303, 1426.901689560120076, 137.0999999980980135 ) ) ;
#4557 = CARTESIAN_POINT ( 'NONE',  ( -4.325231581420000637, 1515.225841049890050, 208.0340196748790049 ) ) ;
#4558 = CARTESIAN_POINT ( 'NONE',  ( -28.26636407291830011, 1509.425358601070229, 210.9265341182299949 ) ) ;
#4559 = CARTESIAN_POINT ( 'NONE',  ( 13.50093264849999919, 1434.968966241960061, 149.0260858328979907 ) ) ;
#4560 = CARTESIAN_POINT ( 'NONE',  ( -39.02661178205909920, 1437.758897876949959, 134.0999999974839909 ) ) ;
#4561 = CARTESIAN_POINT ( 'NONE',  ( 8.565457501751716052, 1437.263446294652567, 210.3368058788049666 ) ) ;
#4562 = ORIENTED_EDGE ( 'NONE', *, *, #60333, .F. ) ;
#4563 = CARTESIAN_POINT ( 'NONE',  ( 3.132736840369999776, 1477.411600225689881, 199.0056338034989949 ) ) ;
#4564 = CARTESIAN_POINT ( 'NONE',  ( -6.087041179825980031, 1409.125624549270015, 222.8042030212700126 ) ) ;
#4565 = CARTESIAN_POINT ( 'NONE',  ( -12.23036328449999921, 1490.675422890390109, 208.1371813544890017 ) ) ;
#4566 = CARTESIAN_POINT ( 'NONE',  ( -9.784003721936180398, 1438.410133247240083, 210.7787260446129949 ) ) ;
#4567 = DIRECTION ( 'NONE',  ( 0.8200914087126649488, -0.4884709562386962411, 0.2980708074718669276 ) ) ;
#4568 = CARTESIAN_POINT ( 'NONE',  ( 31.76117549946924612, 1416.371467029696760, 269.3206785931494665 ) ) ;
#4569 = CARTESIAN_POINT ( 'NONE',  ( 19.70592387150000135, 1434.997135647629875, 210.0287612964809796 ) ) ;
#4570 = CARTESIAN_POINT ( 'NONE',  ( 2.407253779970412566, 1523.313115944345554, 243.1783812783781116 ) ) ;
#4571 = CARTESIAN_POINT ( 'NONE',  ( -90.82321950335810357, 1384.617696737160259, 308.9652747753909807 ) ) ;
#4572 = CARTESIAN_POINT ( 'NONE',  ( -43.37668113294960648, 1384.998540390349945, 216.4009036113180002 ) ) ;
#4573 = CARTESIAN_POINT ( 'NONE',  ( -17.06401309437957892, 1526.329757971584741, 237.1783921619734770 ) ) ;
#4574 = CARTESIAN_POINT ( 'NONE',  ( -24.74145858110844642, 1444.127034557292745, 210.7303339034181988 ) ) ;
#4575 = CARTESIAN_POINT ( 'NONE',  ( -27.01382318160000295, 1450.681613999719957, 136.4483333615980030 ) ) ;
#4576 = DIRECTION ( 'NONE',  ( 0.000000000000000000, 1.000000000000000000, 0.000000000000000000 ) ) ;
#4578 = ORIENTED_EDGE ( 'NONE', *, *, #83626, .T. ) ;
#4577 = CYLINDRICAL_SURFACE ( 'NONE', #87806, 2.000000000000003109 ) ;
#4579 = CARTESIAN_POINT ( 'NONE',  ( -109.9850615409999932, 1384.906745092810070, 311.4561455232590106 ) ) ;
#4581 = CARTESIAN_POINT ( 'NONE',  ( 5.098960260437297443, 1422.101870575426801, 138.2838502392716862 ) ) ;
#4580 = VECTOR ( 'NONE', #40352, 999.9999999999998863 ) ;
#4582 = CARTESIAN_POINT ( 'NONE',  ( -11.24237508680000097, 1500.135314328090089, 210.9525305401789979 ) ) ;
#4583 = B_SPLINE_CURVE_WITH_KNOTS ( 'NONE', 3,
 ( #10826, #104323, #103775, #45553, #36568, #86415, #95377, #95924, #104877, #1323 ),
 .UNSPECIFIED., .F., .F.,
 ( 4, 2, 2, 2, 4 ),
 ( 0.000000000000000000, 0.5154127766764070584, 1.031119021958050164, 1.547502715879019997, 2.064659070031829913 ),
 .UNSPECIFIED. ) ;
#4584 = CARTESIAN_POINT ( 'NONE',  ( 3.487592431604999987, 1508.551704408389924, 204.1347675156769981 ) ) ;
#4585 = CARTESIAN_POINT ( 'NONE',  ( 0.003688949178799999940, 1466.041018883930064, 235.8553854185979901 ) ) ;
#4586 = CARTESIAN_POINT ( 'NONE',  ( 21.08090099129999828, 1409.649221671529858, 214.5855264853080087 ) ) ;
#4587 = B_SPLINE_SURFACE_WITH_KNOTS ( 'NONE', 5, 1, ( 
 ( #31429, #39285 ),
 ( #65611, #55561 ),
 ( #22451, #73460 ),
 ( #74559, #56652 ),
 ( #31984, #4593 ),
 ( #30876, #99723 ) ),
 .UNSPECIFIED., .F., .F., .F.,
 ( 6, 6 ),
 ( 2, 2 ),
 ( 0.000000000000000000, 3.708546873389999998 ),
 ( 0.000000000000000000, 14.00000000000000000 ),
 .UNSPECIFIED. ) ;
#4588 = CARTESIAN_POINT ( 'NONE',  ( 2.487935123020000194, 1509.038615934189920, 213.6090957346689834 ) ) ;
#4589 = CARTESIAN_POINT ( 'NONE',  ( -20.38158083214809935, 1465.353255672800060, 211.0002992862519875 ) ) ;
#4590 = CARTESIAN_POINT ( 'NONE',  ( -15.59773506849999869, 1422.361982635230106, 227.8242805376979732 ) ) ;
#4592 = CARTESIAN_POINT ( 'NONE',  ( -11.73701141503820011, 1426.696005490819971, 144.1689084034089774 ) ) ;
#4591 = CARTESIAN_POINT ( 'NONE',  ( -3.385932610363147077, 1511.683921178999071, 201.1181467729594203 ) ) ;
#4593 = CARTESIAN_POINT ( 'NONE',  ( 20.21058018289999936, 1475.708866082789882, 208.1563043901110177 ) ) ;
#4594 = CARTESIAN_POINT ( 'NONE',  ( -31.23437356469425907, 1523.382868172864164, 222.8968241038848248 ) ) ;
#4595 = CARTESIAN_POINT ( 'NONE',  ( 17.84338787571943996, 1523.481610426287716, 237.8836641337660467 ) ) ;
#4596 = CARTESIAN_POINT ( 'NONE',  ( -1.828265859660000103, 1416.270454245330029, 233.1889656714979822 ) ) ;
#4597 = CARTESIAN_POINT ( 'NONE',  ( 8.653423937779999520, 1367.169888897630017, 210.6218459616991936 ) ) ;
#4598 = CARTESIAN_POINT ( 'NONE',  ( -4.041472511874999896, 1516.858649670339901, 205.0922732913970208 ) ) ;
#4599 = CARTESIAN_POINT ( 'NONE',  ( -10.40111706681060078, 1485.527135515960026, 184.6835754761009696 ) ) ;
#4600 = ORIENTED_EDGE ( 'NONE', *, *, #107012, .F. ) ;
#4601 = CARTESIAN_POINT ( 'NONE',  ( 11.66537932461100091, 1501.769425689289847, 211.4581373967929778 ) ) ;
#4602 = CARTESIAN_POINT ( 'NONE',  ( -10.66799487405013558, 1422.348300139214871, 210.6394755018355909 ) ) ;
#4604 = ORIENTED_EDGE ( 'NONE', *, *, #53075, .F. ) ;
#4603 = CARTESIAN_POINT ( 'NONE',  ( -68.34061848820969942, 1379.747312853899984, 279.8872088319540126 ) ) ;
#4605 = ORIENTED_EDGE ( 'NONE', *, *, #8081, .T. ) ;
#4606 = CARTESIAN_POINT ( 'NONE',  ( 28.08128577580000140, 1509.609363975330098, 213.5608712337979966 ) ) ;
#4607 = ORIENTED_EDGE ( 'NONE', *, *, #90717, .T. ) ;
#4608 = CARTESIAN_POINT ( 'NONE',  ( 2.061035136763549769, 1485.227510182900005, 220.8012168559289989 ) ) ;
#4609 = CARTESIAN_POINT ( 'NONE',  ( 1.326919697849999968, 1414.988015876730060, 191.7691690367979902 ) ) ;
#4611 = CARTESIAN_POINT ( 'NONE',  ( 15.73512419572140075, 1409.471149252580062, 192.7531534643019882 ) ) ;
#4610 = CARTESIAN_POINT ( 'NONE',  ( 15.79333902952730107, 1414.567926746569810, 191.4021969136939845 ) ) ;
#4612 = CARTESIAN_POINT ( 'NONE',  ( -4.612671377915000370, 1516.783665406140017, 209.8782801844560026 ) ) ;
#4613 =( BOUNDED_CURVE ( )  B_SPLINE_CURVE ( 3, ( #71939, #89242, #97646, #20915 ),
 .UNSPECIFIED., .F., .T. ) 
 B_SPLINE_CURVE_WITH_KNOTS ( ( 4, 4 ),
 ( 0.8490841261708470533, 1.097941757445210165 ),
 .UNSPECIFIED. ) 
 CURVE ( )  GEOMETRIC_REPRESENTATION_ITEM ( )  RATIONAL_B_SPLINE_CURVE ( ( 1.000000000000000000, 0.9948458117537219980, 0.9948458117537219980, 1.000000000000000000 ) ) 
 REPRESENTATION_ITEM ( '' )  );
#4614 = CARTESIAN_POINT ( 'NONE',  ( -24.99671999555539870, 1451.592871286339914, 137.2106111822299965 ) ) ;
#4615 = CARTESIAN_POINT ( 'NONE',  ( -11.63668813159999971, 1425.864839735429769, 144.1681848196979843 ) ) ;
#4616 = CARTESIAN_POINT ( 'NONE',  ( 13.06456701529999975, 1409.369285120729955, 227.4078810651980120 ) ) ;
#4617 = CARTESIAN_POINT ( 'NONE',  ( -16.53125420670000167, 1418.541487540729804, 202.7561987471289910 ) ) ;
#4618 = DIRECTION ( 'NONE',  ( 1.000000000000000000, 0.000000000000000000, 0.000000000000000000 ) ) ;
#4620 = AXIS2_PLACEMENT_3D ( 'NONE', #57541, #83814, #52323 ) ;
#4619 = CARTESIAN_POINT ( 'NONE',  ( 41.25063694425699623, 1441.159963067259923, 134.0999999980680002 ) ) ;
#4621 = CARTESIAN_POINT ( 'NONE',  ( -40.14620926511650367, 1442.319073519450058, 136.9682662247859923 ) ) ;
#4622 = ORIENTED_EDGE ( 'NONE', *, *, #51179, .T. ) ;
#4623 = CARTESIAN_POINT ( 'NONE',  ( 11.69993711075939835, 1435.514582224059950, 225.6365368809329937 ) ) ;
#4624 = CARTESIAN_POINT ( 'NONE',  ( -16.81464677261302754, 1526.382868172863937, 234.5384874912344344 ) ) ;
#4625 = ORIENTED_EDGE ( 'NONE', *, *, #80622, .F. ) ;
#4626 = VERTEX_POINT ( 'NONE', #85345 ) ;
#4627 = CARTESIAN_POINT ( 'NONE',  ( -6.390054486374999954, 1513.333000339850059, 216.6179291409569885 ) ) ;
#4628 = CARTESIAN_POINT ( 'NONE',  ( -0.06979896196049999169, 1450.915497820830069, 181.2403767423980128 ) ) ;
#4629 = CARTESIAN_POINT ( 'NONE',  ( -16.87622493273829960, 1508.451388730329882, 209.8247102120089949 ) ) ;
#4630 = CARTESIAN_POINT ( 'NONE',  ( -18.98492718470860297, 1508.490463703670002, 210.0727590967670153 ) ) ;
#4631 = CARTESIAN_POINT ( 'NONE',  ( -63.44223337645949101, 1379.735152652233410, 269.0017066445272462 ) ) ;
#4632 = CARTESIAN_POINT ( 'NONE',  ( 1.910178218220000002, 1465.721278390790076, 198.6655444000990087 ) ) ;
#4633 = CARTESIAN_POINT ( 'NONE',  ( 28.24318409530000196, 1508.132100788830030, 208.6373738428400202 ) ) ;
#4634 = CARTESIAN_POINT ( 'NONE',  ( 3.236790408180000078, 1414.913060387329779, 192.7926995017980119 ) ) ;
#4635 = CARTESIAN_POINT ( 'NONE',  ( -57.67880930100110248, 1384.659099901070249, 239.1381722207320024 ) ) ;
#4636 = EDGE_LOOP ( 'NONE', ( #19188, #39513, #92344, #51745 ) ) ;
#4637 = CARTESIAN_POINT ( 'NONE',  ( 7.708770007014999592, 1516.524310051880093, 206.8307984429870032 ) ) ;
#4638 = ORIENTED_EDGE ( 'NONE', *, *, #56372, .T. ) ;
#4639 = DIRECTION ( 'NONE',  ( 0.9510565162951518658, 0.000000000000000000, -0.3090169943749528914 ) ) ;
#4640 = B_SPLINE_CURVE_WITH_KNOTS ( 'NONE', 3,
 ( #21411, #99223, #80803, #81328, #72417, #6287, #13562, #97603, #39341, #55620 ),
 .UNSPECIFIED., .F., .F.,
 ( 4, 2, 2, 2, 4 ),
 ( 2.797157557069881010E-17, 0.0007406479101618366166, 0.001481295820323645261, 0.002221943730485453905, 0.002962591640647262332 ),
 .UNSPECIFIED. ) ;
#4641 = CARTESIAN_POINT ( 'NONE',  ( 19.34500396569999836, 1467.214498603729908, 226.4572167402979801 ) ) ;
#4642 = ORIENTED_EDGE ( 'NONE', *, *, #48019, .F. ) ;
#4643 = CARTESIAN_POINT ( 'NONE',  ( -0.4702569809430000025, 1450.896638651699959, 181.9239822119980090 ) ) ;
#4644 = CARTESIAN_POINT ( 'NONE',  ( -16.23065921520000288, 1409.981629652129868, 191.7102031687979888 ) ) ;
#4645 = CARTESIAN_POINT ( 'NONE',  ( -17.97472709737555263, 1508.456906073600294, 211.9276151093460783 ) ) ;
#4646 = CARTESIAN_POINT ( 'NONE',  ( -24.39257549919999946, 1441.120364142740073, 211.3418877072379871 ) ) ;
#4647 = CARTESIAN_POINT ( 'NONE',  ( 22.52918858713469774, 1410.933109781309895, 206.2006944076529749 ) ) ;
#4648 = CARTESIAN_POINT ( 'NONE',  ( -5.910253173700709795, 1511.600194708689969, 200.4926261112069881 ) ) ;
#4649 = CARTESIAN_POINT ( 'NONE',  ( 45.67178753498799182, 1438.934170743232244, 266.1885948232590522 ) ) ;
#4650 = CARTESIAN_POINT ( 'NONE',  ( -13.19898084229999924, 1434.900407900599930, 147.1505653820979944 ) ) ;
#4651 = CARTESIAN_POINT ( 'NONE',  ( -20.38673671613278771, 1525.878013734320575, 182.1228282333744914 ) ) ;
#4653 = CARTESIAN_POINT ( 'NONE',  ( -11.60004869885203682, 1425.464090738186542, 136.9270719929736515 ) ) ;
#4652 = CARTESIAN_POINT ( 'NONE',  ( 2.994687017620000447, 1464.609795535930061, 236.6065848807980103 ) ) ;
#4654 = CARTESIAN_POINT ( 'NONE',  ( 5.005700201405000271, 1516.732530461250008, 216.0598116305469887 ) ) ;
#4655 = CARTESIAN_POINT ( 'NONE',  ( -113.4000000000000057, 1378.913060387289988, 304.2218459572590064 ) ) ;
#4656 = CARTESIAN_POINT ( 'NONE',  ( -0.1235785668905619999, 1507.996910569370129, 180.6531142414899875 ) ) ;
#4657 = EDGE_CURVE ( 'NONE', #83547, #40664, #20996, .T. ) ;
#4658 = CARTESIAN_POINT ( 'NONE',  ( 2.419940912470191829, 1516.533504771425442, 216.8308567494544832 ) ) ;
#4659 = CARTESIAN_POINT ( 'NONE',  ( 3.266349474065000091, 1516.797038924770050, 213.1501537103870021 ) ) ;
#4660 = AXIS2_PLACEMENT_3D ( 'NONE', #7664, #67596, #110128 ) ;
#4661 = CARTESIAN_POINT ( 'NONE',  ( 4.082779675200349345, 1515.071395204220153, 212.7082060777060235 ) ) ;
#4662 = DIRECTION ( 'NONE',  ( 1.755985294532464991E-16, -1.000000000000000000, 1.338183447452830017E-16 ) ) ;
#4664 = ORIENTED_EDGE ( 'NONE', *, *, #17540, .F. ) ;
#4663 = CARTESIAN_POINT ( 'NONE',  ( 0.000000000000000000, 1395.913060387330006, 201.1218459616980283 ) ) ;
#4665 = CARTESIAN_POINT ( 'NONE',  ( -2.273033093151318962, 1525.821544997590308, 177.3097463090895474 ) ) ;
#4666 = CARTESIAN_POINT ( 'NONE',  ( 24.96471540929999833, 1444.223829899530074, 217.4975133951479904 ) ) ;
#4667 = EDGE_CURVE ( 'NONE', #106739, #71879, #51778, .T. ) ;
#4668 = CARTESIAN_POINT ( 'NONE',  ( -11.30178248569999866, 1432.341675826490018, 151.5222233993980012 ) ) ;
#4669 = CARTESIAN_POINT ( 'NONE',  ( -14.70081393560000116, 1415.677402184240009, 205.6533923404689688 ) ) ;
#4670 = CARTESIAN_POINT ( 'NONE',  ( 9.549927530160001510, 1420.582634806009992, 197.0246874367990131 ) ) ;
#4671 = CARTESIAN_POINT ( 'NONE',  ( 12.37689147640000087, 1445.074465208020001, 186.3522911324980100 ) ) ;
#4672 = B_SPLINE_CURVE_WITH_KNOTS ( 'NONE', 5,
 ( #70814, #96528, #29312, #54008, #55095, #71368, #38258, #11427, #88139, #72442, #37172, #105481 ),
 .UNSPECIFIED., .F., .F.,
 ( 6, 3, 3, 6 ),
 ( 0.000000000000000000, 0.2399281645681053676, 0.6199640824044998499, 1.000000000000000000 ),
 .UNSPECIFIED. ) ;
#4674 = CARTESIAN_POINT ( 'NONE',  ( 2.500000000000000000, 1432.287109468649987, 157.4934292187979850 ) ) ;
#4673 = CARTESIAN_POINT ( 'NONE',  ( -23.87373140470000266, 1444.795516104289845, 213.3892174405480091 ) ) ;
#4675 = CARTESIAN_POINT ( 'NONE',  ( -2.950048403249999840, 1486.007024737429902, 182.1215898259980293 ) ) ;
#4676 = ORIENTED_EDGE ( 'NONE', *, *, #55094, .F. ) ;
#4677 = CARTESIAN_POINT ( 'NONE',  ( 6.547881374914999775, 1516.647534046129977, 205.6658385469270058 ) ) ;
#4678 = CARTESIAN_POINT ( 'NONE',  ( 0.8822908926409999131, 1406.271154717829859, 269.2944284930979961 ) ) ;
#4679 = CARTESIAN_POINT ( 'NONE',  ( -1.477486471839999815, 1515.342042115489903, 213.3960819243490050 ) ) ;
#4680 = AXIS2_PLACEMENT_3D ( 'NONE', #79873, #11559, #20478 ) ;
#4681 = CARTESIAN_POINT ( 'NONE',  ( 24.33107475527064167, 1437.296842069204786, 213.0379144650110845 ) ) ;
#4682 = CARTESIAN_POINT ( 'NONE',  ( 3.106494988410000158, 1471.641399328589841, 189.2364613132990030 ) ) ;
#4683 = CARTESIAN_POINT ( 'NONE',  ( 5.059013353549999259, 1501.257177412389865, 229.8390314845989906 ) ) ;
#4684 = CARTESIAN_POINT ( 'NONE',  ( -7.748343491022634311, 1439.118950628315588, 205.0759599076347399 ) ) ;
#4685 = CARTESIAN_POINT ( 'NONE',  ( -0.8755637974877499285, 1450.882485025779943, 155.3353162938959997 ) ) ;
#4686 = CARTESIAN_POINT ( 'NONE',  ( -1.699825449855114634, 1451.801988038905392, 184.1305289709272586 ) ) ;
#4687 = CARTESIAN_POINT ( 'NONE',  ( -19.75226155591039401, 1486.000263447242787, 190.2095123751601022 ) ) ;
#4688 = CARTESIAN_POINT ( 'NONE',  ( -14.17422268755229986, 1415.724942524879907, 221.1012049180340000 ) ) ;
#4689 = LINE ( 'NONE', #73007, #76490 ) ;
#4690 = CARTESIAN_POINT ( 'NONE',  ( -20.74408967690000338, 1436.077466332870017, 224.8635562271979893 ) ) ;
#4691 = CARTESIAN_POINT ( 'NONE',  ( -26.86204968941349946, 1508.007394745769943, 212.0120970035400205 ) ) ;
#4692 = CARTESIAN_POINT ( 'NONE',  ( 2.710683911340000307, 1440.403613791419957, 159.2736478902979798 ) ) ;
#4693 = CARTESIAN_POINT ( 'NONE',  ( -3.744984048050000069, 1475.448291240629942, 269.2893923236980527 ) ) ;
#4694 = CARTESIAN_POINT ( 'NONE',  ( 19.64992912776053657, 1517.051704408389924, 207.6921549199338983 ) ) ;
#4695 = DIRECTION ( 'NONE',  ( 0.000000000000000000, 1.000000000000000000, 0.000000000000000000 ) ) ;
#4696 = CARTESIAN_POINT ( 'NONE',  ( -40.12232014923479539, 1384.787011377809904, 242.3469171355359890 ) ) ;
#4697 = DIRECTION ( 'NONE',  ( -0.9417419115949662300, -0.2378257470769920556, 0.2378257470769920556 ) ) ;
#4698 = CARTESIAN_POINT ( 'NONE',  ( 12.27851265883290033, 1491.806146454400050, 208.1629158539130060 ) ) ;
#4699 = CARTESIAN_POINT ( 'NONE',  ( -19.92151515271921980, 1526.208281990535852, 184.7237256173605431 ) ) ;
#4700 = CARTESIAN_POINT ( 'NONE',  ( 7.924501696547047835, 1511.889619706852500, 206.0091653069858069 ) ) ;
#4701 = CARTESIAN_POINT ( 'NONE',  ( -5.283839841746620358, 1396.097576142400158, 218.8113393475669852 ) ) ;
#4702 = CARTESIAN_POINT ( 'NONE',  ( -15.05376510940000045, 1421.406871761930233, 227.2858920301979992 ) ) ;
#4703 = CARTESIAN_POINT ( 'NONE',  ( 19.47931728987103739, 1455.585788024227668, 225.7017591050554017 ) ) ;
#4704 = ORIENTED_EDGE ( 'NONE', *, *, #86424, .F. ) ;
#4705 = DIRECTION ( 'NONE',  ( 0.9417419115949662300, -0.2378257470769920556, 0.2378257470769920556 ) ) ;
#4706 = CARTESIAN_POINT ( 'NONE',  ( -7.513187957268617545, 1510.663752939659162, 215.0853058208080313 ) ) ;
#4707 = FACE_OUTER_BOUND ( 'NONE', #68624, .T. ) ;
#4709 = CARTESIAN_POINT ( 'NONE',  ( -11.59188839696499862, 1512.902436350919970, 192.6803903701670038 ) ) ;
#4708 = CARTESIAN_POINT ( 'NONE',  ( 10.97133660469999938, 1425.661190073130001, 112.6510004812979986 ) ) ;
#4710 = CARTESIAN_POINT ( 'NONE',  ( -9286.692186988937465, 54.07981494722830718, 5933.209537134458515 ) ) ;
#4711 = CARTESIAN_POINT ( 'NONE',  ( -7.405436629479999588, 1451.940595730289942, 201.5764829818989767 ) ) ;
#4712 = CARTESIAN_POINT ( 'NONE',  ( -1.708721022705000037, 1516.531533746980131, 201.8006767011069940 ) ) ;
#4713 = CARTESIAN_POINT ( 'NONE',  ( 8.454790768000000512, 1428.363638924389988, 213.4109941084990112 ) ) ;
#4714 = CARTESIAN_POINT ( 'NONE',  ( 20.33643750519999926, 1475.138452888789971, 218.0161091832190152 ) ) ;
#4715 = CARTESIAN_POINT ( 'NONE',  ( 5.458328288009999696, 1507.507604181929992, 182.0472652214980087 ) ) ;
#4716 = CARTESIAN_POINT ( 'NONE',  ( -20.59684415639999955, 1507.762623716630060, 190.3921826403979765 ) ) ;
#4717 = CARTESIAN_POINT ( 'NONE',  ( -75.76943313550691528, 1379.211134910969804, 293.7650760281990188 ) ) ;
#4718 = CARTESIAN_POINT ( 'NONE',  ( 8.726849315049442168, 1367.111769039830051, 210.6218459616987957 ) ) ;
#4720 = ORIENTED_EDGE ( 'NONE', *, *, #106335, .T. ) ;
#4719 = CARTESIAN_POINT ( 'NONE',  ( 16.99888975204404673, 1410.874132688714326, 191.9700510342732684 ) ) ;
#4721 = ORIENTED_EDGE ( 'NONE', *, *, #51473, .T. ) ;
#4722 = CARTESIAN_POINT ( 'NONE',  ( -12.08430580090000106, 1397.963661761730009, 203.2737820671979705 ) ) ;
#4723 = CARTESIAN_POINT ( 'NONE',  ( 2.927202511967800014, 1410.063496054050120, 231.5773537391340255 ) ) ;
#4724 = CARTESIAN_POINT ( 'NONE',  ( -1.383992982630000146, 1414.983773852929744, 226.4898643104980067 ) ) ;
#4725 = CARTESIAN_POINT ( 'NONE',  ( 7.019973835868021340E-09, 1395.913060387101041, 220.3433455203826838 ) ) ;
#4726 = CARTESIAN_POINT ( 'NONE',  ( -14.75025451881061755, 1435.013611857857086, 147.9283386685173411 ) ) ;
#4727 = LINE ( 'NONE', #73050, #1617 ) ;
#4729 = CARTESIAN_POINT ( 'NONE',  ( -1.357842376853849897, 1411.328796458540182, 185.5617438169070113 ) ) ;
#4728 = CARTESIAN_POINT ( 'NONE',  ( -104.4930944259999990, 1390.118374325210198, 304.1821532511589794 ) ) ;
#4730 = FACE_OUTER_BOUND ( 'NONE', #16698, .T. ) ;
#4731 = CARTESIAN_POINT ( 'NONE',  ( -1.879441947317239903, 1463.200433190200101, 199.5207160416179875 ) ) ;
#4732 = CARTESIAN_POINT ( 'NONE',  ( 12.45715143159750049, 1427.088322622419810, 206.6492473361469990 ) ) ;
#4733 = CARTESIAN_POINT ( 'NONE',  ( 9.026700659202800736, 1396.228279763480032, 202.7331491456050117 ) ) ;
#4734 = CARTESIAN_POINT ( 'NONE',  ( 0.5624690339869999889, 1416.828040475229955, 190.4759594386979984 ) ) ;
#4735 = DIRECTION ( 'NONE',  ( -0.9455185755993177343, 0.000000000000000000, 0.3255681544571540909 ) ) ;
#4736 = CARTESIAN_POINT ( 'NONE',  ( 41.65674243270000687, 1443.992462215730029, 135.6790809909979885 ) ) ;
#4737 = VERTEX_POINT ( 'NONE', #58525 ) ;
#4738 = CARTESIAN_POINT ( 'NONE',  ( -113.4000000000000057, 1377.913060387289988, 304.2218459572590064 ) ) ;
#4739 = CARTESIAN_POINT ( 'NONE',  ( 12.57940213210000024, 1442.756379237810052, 186.9445026950980093 ) ) ;
#4740 = ORIENTED_EDGE ( 'NONE', *, *, #95366, .F. ) ;
#4741 = ORIENTED_EDGE ( 'NONE', *, *, #16575, .T. ) ;
#4742 = CARTESIAN_POINT ( 'NONE',  ( -17.03470032699999948, 1420.297131032510151, 203.9213209310090065 ) ) ;
#4743 = CARTESIAN_POINT ( 'NONE',  ( 8.988338641399998608, 1366.896325247149889, 207.6218459616989946 ) ) ;
#4744 = CARTESIAN_POINT ( 'NONE',  ( -109.8576740279066115, 1385.955398400293006, 311.3643922957008385 ) ) ;
#4745 = CYLINDRICAL_SURFACE ( 'NONE', #5170, 2.000000000000003553 ) ;
#4746 = CARTESIAN_POINT ( 'NONE',  ( -5.001338666445000136, 1516.911981270829983, 214.9058546054269812 ) ) ;
#4747 = DIRECTION ( 'NONE',  ( 0.000000000000000000, 1.000000000000000000, 0.000000000000000000 ) ) ;
#4748 = AXIS2_PLACEMENT_3D ( 'NONE', #78412, #102486, #43707 ) ;
#4749 = ORIENTED_EDGE ( 'NONE', *, *, #61669, .T. ) ;
#4750 = CARTESIAN_POINT ( 'NONE',  ( -18.45894773530089950, 1508.542100887300194, 210.6804767572419905 ) ) ;
#4751 = CARTESIAN_POINT ( 'NONE',  ( -2.948549143151390162, 1509.071337496469823, 179.3632791091939964 ) ) ;
#4752 = CARTESIAN_POINT ( 'NONE',  ( -56.57961477790000515, 1379.628839295709895, 252.6055042428589843 ) ) ;
#4753 = CARTESIAN_POINT ( 'NONE',  ( 4.988721302020000081, 1414.971262582530017, 225.1457994249980175 ) ) ;
#4754 = CARTESIAN_POINT ( 'NONE',  ( 0.7360974386200019870, 1517.045004075700035, 205.0794574309270217 ) ) ;
#4755 = VERTEX_POINT ( 'NONE', #32752 ) ;
#4756 = CARTESIAN_POINT ( 'NONE',  ( -20.84357928160000029, 1509.537325856430016, 229.6909426013980067 ) ) ;
#4757 = CARTESIAN_POINT ( 'NONE',  ( -35.24250836817223842, 1424.318067564319335, 269.5348774294620284 ) ) ;
#4758 = CARTESIAN_POINT ( 'NONE',  ( -0.5133638609530000174, 1410.311096994530089, 233.1717005261980091 ) ) ;
#4760 = ORIENTED_EDGE ( 'NONE', *, *, #92439, .F. ) ;
#4759 = CARTESIAN_POINT ( 'NONE',  ( -8.099819236969999281, 1497.713060387329961, 188.5692696260980199 ) ) ;
#4761 = CARTESIAN_POINT ( 'NONE',  ( 2.500000000000000000, 1420.168334228329968, 149.0935893383980044 ) ) ;
#4762 = CARTESIAN_POINT ( 'NONE',  ( -33.00779162925590526, 1440.913060389950033, 246.6090774808910169 ) ) ;
#4763 = CARTESIAN_POINT ( 'NONE',  ( -67.10855885389999287, 1384.077638385570026, 292.1367942583589752 ) ) ;
#4764 = CARTESIAN_POINT ( 'NONE',  ( -0.2830760018822799928, 1465.096848926169969, 236.9997508814410025 ) ) ;
#4765 = B_SPLINE_CURVE_WITH_KNOTS ( 'NONE', 3,
 ( #96116, #54697, #61443, #26696 ),
 .UNSPECIFIED., .F., .F.,
 ( 4, 4 ),
 ( -128.3330504390000044, -82.60381054909998966 ),
 .UNSPECIFIED. ) ;
#4766 = CARTESIAN_POINT ( 'NONE',  ( 27.88456862112260026, 1417.385368265699753, 269.9356247533810347 ) ) ;
#4767 = CARTESIAN_POINT ( 'NONE',  ( -7.323034312095000331, 1516.609912606490070, 212.5765947784269940 ) ) ;
#4768 = CARTESIAN_POINT ( 'NONE',  ( -50.74207601739999518, 1379.687644451550113, 241.2614600171590098 ) ) ;
#4769 = CARTESIAN_POINT ( 'NONE',  ( 23.53857934830000076, 1410.839771826630113, 207.7860714048179887 ) ) ;
#4770 = CARTESIAN_POINT ( 'NONE',  ( -30.51923195337130679, 1524.059547553518769, 221.8697090587693879 ) ) ;
#4771 = CARTESIAN_POINT ( 'NONE',  ( -11.60004869885203682, 1425.691647225251245, 137.2114480028974413 ) ) ;
#4772 = CARTESIAN_POINT ( 'NONE',  ( 4.625789976465000564, 1517.104192383289956, 210.2432295619669844 ) ) ;
#4773 = CARTESIAN_POINT ( 'NONE',  ( 4.240641006030480220, 1420.805731536519943, 185.5174961375570319 ) ) ;
#4774 = CARTESIAN_POINT ( 'NONE',  ( -1.715370464160000052, 1415.379143890329942, 233.0965786315979926 ) ) ;
#4775 = CARTESIAN_POINT ( 'NONE',  ( -86.93157266469999911, 1384.741940548570028, 307.7299721360590183 ) ) ;
#4776 = ORIENTED_EDGE ( 'NONE', *, *, #43168, .T. ) ;
#4778 = B_SPLINE_CURVE_WITH_KNOTS ( 'NONE', 3,
 ( #95144, #52049, #36331, #61561, #68864, #17847, #18405, #95695, #26266, #94573, #78912, #9477, #86739, #59906, #87297, #43641, #16737, #52603, #18962, #99495, #26833, #552, #104088, #60456, #102968, #104643, #77793, #1102, #51486, #85069, #50944, #35231, #69419, #94027, #10591 ),
 .UNSPECIFIED., .F., .F.,
 ( 4, 2, 2, 1, 1, 2, 2, 2, 1, 2, 2, 1, 1, 1, 2, 2, 2, 1, 2, 2, 4 ),
 ( 0.000000000000000000, 0.1250000000000932032, 0.1875000000001283418, 0.2187500000001456890, 0.2343750000001545153, 0.2421875000001469658, 0.2500000000001393885, 0.3125000000000572320, 0.3437500000000050515, 0.3593749999999903411, 0.3749999999999756306, 0.4062499999999467093, 0.4218749999999321654, 0.4296874999999362177, 0.4335937499999382161, 0.4374999999999402145, 0.4687499999999615308, 0.4843749999999613642, 0.4921874999999606426, 0.4999999999999599209, 1.000000000000000000 ),
 .UNSPECIFIED. ) ;
#4777 = CARTESIAN_POINT ( 'NONE',  ( -26.43298866905689692, 1385.249642334559894, 224.7510168897049994 ) ) ;
#4779 = CARTESIAN_POINT ( 'NONE',  ( -9.862951377749247683, 1519.551704408389924, 228.3939896778649654 ) ) ;
#4780 = FACE_OUTER_BOUND ( 'NONE', #40171, .T. ) ;
#4781 = CARTESIAN_POINT ( 'NONE',  ( 17.04532911661897288, 1517.151704408390060, 221.2898363890541589 ) ) ;
#4782 = CARTESIAN_POINT ( 'NONE',  ( -107.2902847454959954, 1391.913060387289988, 307.3027153792770036 ) ) ;
#4783 = CARTESIAN_POINT ( 'NONE',  ( 11.64657740540000042, 1421.681747358590201, 203.4365565939590113 ) ) ;
#4784 = CARTESIAN_POINT ( 'NONE',  ( -0.1681676274470000065, 1420.473121337229941, 182.7663689088979879 ) ) ;
#4786 = CARTESIAN_POINT ( 'NONE',  ( 25.07506534592078395, 1507.939511209920283, 220.0842285648270718 ) ) ;
#4785 = CARTESIAN_POINT ( 'NONE',  ( -2.484577695354999616, 1517.170512887980067, 216.4602579296269766 ) ) ;
#4787 = CARTESIAN_POINT ( 'NONE',  ( 1.779428963082609894, 1456.357349037730046, 198.6855221610310309 ) ) ;
#4788 = CARTESIAN_POINT ( 'NONE',  ( 10.03573453041540020, 1469.254327712470058, 209.6255595403590064 ) ) ;
#4789 = VERTEX_POINT ( 'NONE', #26554 ) ;
#4790 = CARTESIAN_POINT ( 'NONE',  ( -3.261007169695000041, 1516.596789218710001, 201.7991362452670216 ) ) ;
#4791 = CARTESIAN_POINT ( 'NONE',  ( 10.19252854585250212, 1480.675633674519986, 206.4352025249530129 ) ) ;
#4792 = ORIENTED_EDGE ( 'NONE', *, *, #110593, .F. ) ;
#4793 = CARTESIAN_POINT ( 'NONE',  ( 0.000000000000000000, 1395.913060387330006, 201.1218459616980283 ) ) ;
#4794 = CIRCLE ( 'NONE', #67414, 1.999999999999951594 ) ;
#4795 = CARTESIAN_POINT ( 'NONE',  ( 20.94619202359999832, 1453.740811735230182, 222.3286468221979817 ) ) ;
#4796 = CARTESIAN_POINT ( 'NONE',  ( 8.429635107905490088, 1437.624008729415664, 153.4535873770691126 ) ) ;
#4797 = CARTESIAN_POINT ( 'NONE',  ( 8.488400859335269999, 1511.451532973539770, 203.7397716954870077 ) ) ;
#4798 = CARTESIAN_POINT ( 'NONE',  ( 2.380213422489999786, 1443.039342964089883, 217.6985620011490141 ) ) ;
#4799 = CARTESIAN_POINT ( 'NONE',  ( -28.15442856212169787, 1509.896234822020006, 200.8410265843269826 ) ) ;
#4800 = CARTESIAN_POINT ( 'NONE',  ( -3.116758655539999534, 1446.591766556430002, 170.5446539902980021 ) ) ;
#4801 = CARTESIAN_POINT ( 'NONE',  ( -18.94750420209999930, 1425.709852022430141, 224.6216987348980183 ) ) ;
#4802 = CARTESIAN_POINT ( 'NONE',  ( -23.79554767710000007, 1435.472948733359999, 138.9787834592980005 ) ) ;
#4803 = CARTESIAN_POINT ( 'NONE',  ( -105.5084658100000041, 1391.296568505289997, 303.1147108145589755 ) ) ;
#4804 = CARTESIAN_POINT ( 'NONE',  ( 15.46929474969999951, 1508.458304026830092, 186.6659617994979783 ) ) ;
#4806 = CARTESIAN_POINT ( 'NONE',  ( 28.79939865120000064, 1509.589074241529943, 209.5214322619669929 ) ) ;
#4805 = CARTESIAN_POINT ( 'NONE',  ( 0.004826507542732910543, 1408.913229183870044, 232.2214716291990158 ) ) ;
#4807 = CARTESIAN_POINT ( 'NONE',  ( -10.02128875133539943, 1472.300851888030138, 210.8937131631379884 ) ) ;
#4808 = ORIENTED_EDGE ( 'NONE', *, *, #14876, .F. ) ;
#4809 = CARTESIAN_POINT ( 'NONE',  ( -21.12212911287049977, 1512.187213306747481, 182.4210318429776976 ) ) ;
#4810 = CARTESIAN_POINT ( 'NONE',  ( -14.48383822919999986, 1508.489289363889839, 215.9967763605189930 ) ) ;
#4811 = FACE_OUTER_BOUND ( 'NONE', #61858, .T. ) ;
#4812 = EDGE_CURVE ( 'NONE', #110694, #92620, #72829, .T. ) ;
#4813 = CARTESIAN_POINT ( 'NONE',  ( -17.73225504275565712, 1524.152349020271004, 237.7705388627552452 ) ) ;
#4814 = CARTESIAN_POINT ( 'NONE',  ( -12.29727565780000020, 1497.713060387329961, 227.1658498148980243 ) ) ;
#4815 = FACE_OUTER_BOUND ( 'NONE', #54864, .T. ) ;
#4816 = CARTESIAN_POINT ( 'NONE',  ( -2.865545859819519148, 1525.651285554128663, 241.1072462093984825 ) ) ;
#4817 = CIRCLE ( 'NONE', #97849, 2.000055855578698250 ) ;
#4818 = CARTESIAN_POINT ( 'NONE',  ( -12.86841135482259801, 1442.875644955115831, 186.3777548099945420 ) ) ;
#4819 = CARTESIAN_POINT ( 'NONE',  ( 3.827327205999999649, 1416.243718512830128, 162.3415388335980083 ) ) ;
#4820 = CARTESIAN_POINT ( 'NONE',  ( 6.225981071277309375, 1494.795956435949847, 219.7811113419710125 ) ) ;
#4821 = DIRECTION ( 'NONE',  ( 0.000000000000000000, 0.000000000000000000, -1.000000000000000000 ) ) ;
#4822 = CARTESIAN_POINT ( 'NONE',  ( -15.05902623708989907, 1415.677402202029953, 207.6815266051810056 ) ) ;
#4823 = CARTESIAN_POINT ( 'NONE',  ( -9.544116702023510257, 1460.067049166229936, 210.4863253896969866 ) ) ;
#4824 = CARTESIAN_POINT ( 'NONE',  ( 0.02465969127001850156, 1516.941612417570013, 201.4021494659330074 ) ) ;
#4826 = ORIENTED_EDGE ( 'NONE', *, *, #85308, .T. ) ;
#4825 = CARTESIAN_POINT ( 'NONE',  ( 6.870558963890000648, 1491.940207589490001, 213.3945113296690010 ) ) ;
#4827 = B_SPLINE_CURVE_WITH_KNOTS ( 'NONE', 5,
 ( #71566, #97257, #53076, #1022, #87214, #10504 ),
 .UNSPECIFIED., .F., .F.,
 ( 6, 6 ),
 ( 0.000000000000000000, 1.000000000000000000 ),
 .UNSPECIFIED. ) ;
#4828 = CARTESIAN_POINT ( 'NONE',  ( -113.4000000000000057, 1379.423458858030017, 303.3195241032590275 ) ) ;
#4829 = CARTESIAN_POINT ( 'NONE',  ( 13.03156809012940087, 1512.406412987999829, 224.3505518485380037 ) ) ;
#4830 = ORIENTED_EDGE ( 'NONE', *, *, #2384, .F. ) ;
#4831 = ORIENTED_EDGE ( 'NONE', *, *, #70025, .F. ) ;
#4832 = CARTESIAN_POINT ( 'NONE',  ( 18.07834331186310095, 1415.943166310999914, 209.4111036143110027 ) ) ;
#4833 = DIRECTION ( 'NONE',  ( 0.4090087482554252696, 0.000000000000000000, -0.9125304618753996566 ) ) ;
#4834 = CARTESIAN_POINT ( 'NONE',  ( -1.658081806242819971E-15, 1375.886883438980021, 209.1218459572589836 ) ) ;
#4836 = CARTESIAN_POINT ( 'NONE',  ( -5.301749019849999911, 1468.084175535429949, 248.5896189551980058 ) ) ;
#4835 = CARTESIAN_POINT ( 'NONE',  ( 38.71733486712167860, 1429.045209714008251, 269.5881714454281450 ) ) ;
#4837 = CARTESIAN_POINT ( 'NONE',  ( -20.14880953469999980, 1505.117035552629886, 189.2730550177980149 ) ) ;
#4838 = CARTESIAN_POINT ( 'NONE',  ( -11.89516891659999942, 1433.269307931430149, 149.9552190595979937 ) ) ;
#4839 = FACE_OUTER_BOUND ( 'NONE', #39781, .T. ) ;
#4840 = CARTESIAN_POINT ( 'NONE',  ( 11.68956516707849858, 1426.727195071810002, 140.7743839025759769 ) ) ;
#4841 = VECTOR ( 'NONE', #104644, 1000.000000000000000 ) ;
#4842 = DIRECTION ( 'NONE',  ( 0.000000000000000000, 1.000000000000000000, -1.836970198721029688E-16 ) ) ;
#4843 = CARTESIAN_POINT ( 'NONE',  ( -25.58021156830000109, 1438.607539758289931, 137.7510881711980062 ) ) ;
#4844 = CARTESIAN_POINT ( 'NONE',  ( -24.49620807289999647, 1440.956473104630049, 210.9946877109179866 ) ) ;
#4845 = CARTESIAN_POINT ( 'NONE',  ( -19.37182493330903554, 1526.345556099435726, 185.3206052367970358 ) ) ;
#4846 = CARTESIAN_POINT ( 'NONE',  ( -11.12097504240020029, 1480.502194893749902, 213.0088585123340010 ) ) ;
#4847 = CARTESIAN_POINT ( 'NONE',  ( -2.252062897235808769, 1361.698003988630035, 210.6218459617142003 ) ) ;
#4848 = CARTESIAN_POINT ( 'NONE',  ( 34.18677586421183179, 1522.382868172863937, 198.4504086008745389 ) ) ;
#4850 = ORIENTED_EDGE ( 'NONE', *, *, #13319, .T. ) ;
#4849 = CARTESIAN_POINT ( 'NONE',  ( 5.854860788615310809E-11, 1411.443096976360039, 255.0304971312720284 ) ) ;
#4851 = ORIENTED_EDGE ( 'NONE', *, *, #79634, .T. ) ;
#4852 = CYLINDRICAL_SURFACE ( 'NONE', #83731, 1.999999999999999556 ) ;
#4853 = EDGE_CURVE ( 'NONE', #91781, #5224, #285, .T. ) ;
#4854 = ADVANCED_FACE ( 'NONE', ( #25430 ), #17830, .T. ) ;
#4855 = CARTESIAN_POINT ( 'NONE',  ( -18.76196770059999963, 1505.911165295990031, 222.6390480598990109 ) ) ;
#4856 = CARTESIAN_POINT ( 'NONE',  ( -19.98019444420000212, 1468.125272135429896, 269.6585770649980418 ) ) ;
#4857 = CARTESIAN_POINT ( 'NONE',  ( -19.16951723229999871, 1456.627470220629903, 228.8719212425980061 ) ) ;
#4858 = CARTESIAN_POINT ( 'NONE',  ( 0.000000000000000000, 1524.340287715038357, 209.1218459616979999 ) ) ;
#4859 = CARTESIAN_POINT ( 'NONE',  ( -14.22993178683297266, 1512.187213306747481, 236.2420368605362455 ) ) ;
#4861 = EDGE_CURVE ( 'NONE', #45216, #1907, #3850, .T. ) ;
#4860 = CARTESIAN_POINT ( 'NONE',  ( 0.2432523447182529941, 1451.431949927530013, 182.6146734826490103 ) ) ;
#4862 = DIRECTION ( 'NONE',  ( 0.5032920991128869703, 0.8641163480518950779, 0.000000000000000000 ) ) ;
#4863 = EDGE_CURVE ( 'NONE', #29539, #30233, #56757, .T. ) ;
#4864 = CARTESIAN_POINT ( 'NONE',  ( -16.17567622148224871, 1459.146940454415244, 230.7169173019193806 ) ) ;
#4865 = CARTESIAN_POINT ( 'NONE',  ( -4.803286822639999620, 1458.496532453990085, 218.2603857696190062 ) ) ;
#4866 = CARTESIAN_POINT ( 'NONE',  ( 10.51115150389377639, 1366.987070946261611, 210.6218459617030021 ) ) ;
#4867 = CARTESIAN_POINT ( 'NONE',  ( -43.33566613482280161, 1430.149811106979996, 269.0393173100790136 ) ) ;
#4868 = ORIENTED_EDGE ( 'NONE', *, *, #109812, .F. ) ;
#4869 = CARTESIAN_POINT ( 'NONE',  ( -11.15738487964140013, 1390.939238811560017, 203.8452351040699853 ) ) ;
#4870 = ORIENTED_EDGE ( 'NONE', *, *, #37390, .F. ) ;
#4871 = CIRCLE ( 'NONE', #67483, 1.000000000000000888 ) ;
#4872 = ORIENTED_EDGE ( 'NONE', *, *, #81477, .T. ) ;
#4873 = CARTESIAN_POINT ( 'NONE',  ( 7.339749335215000059, 1517.224900789629828, 210.8312305431869902 ) ) ;
#4874 = CARTESIAN_POINT ( 'NONE',  ( -8.594767888845639803, 1448.338307337700144, 212.2585178878949819 ) ) ;
#4876 = DIRECTION ( 'NONE',  ( 0.8090169943749507819, -0.000000000000000000, 0.5877852522924685852 ) ) ;
#4875 = CARTESIAN_POINT ( 'NONE',  ( 3.461360093275000160, 1516.874084700499907, 212.3753080308970311 ) ) ;
#4877 = CARTESIAN_POINT ( 'NONE',  ( -2.780728806079999949, 1455.446097032029911, 184.5837736821980002 ) ) ;
#4878 = VECTOR ( 'NONE', #9392, 1000.000000000000000 ) ;
#4879 = CARTESIAN_POINT ( 'NONE',  ( -2.487880308650109118, 1449.152950345517183, 183.0833625634865029 ) ) ;
#4880 = ORIENTED_EDGE ( 'NONE', *, *, #70826, .T. ) ;
#4881 = CARTESIAN_POINT ( 'NONE',  ( -26.80800901980000006, 1435.516554886219865, 135.8282728032980060 ) ) ;
#4882 = ADVANCED_FACE ( 'NONE', ( #87017 ), #67009, .F. ) ;
#4883 = CARTESIAN_POINT ( 'NONE',  ( -3.261007169695000041, 1516.596789218710001, 201.7991362452670216 ) ) ;
#4884 = DIRECTION ( 'NONE',  ( 0.6742693640212154005, 0.000000000000000000, 0.7384854939282328168 ) ) ;
#4885 = ADVANCED_FACE ( 'NONE', ( #56738 ), #76863, .T. ) ;
#4886 = CARTESIAN_POINT ( 'NONE',  ( -22.47842407610009730, 1384.538925626759919, 202.4009993073999851 ) ) ;
#4887 = CARTESIAN_POINT ( 'NONE',  ( -44.70567049325760678, 1435.628793295649984, 269.9105676632909763 ) ) ;
#4888 = DIRECTION ( 'NONE',  ( -6.123233995736769734E-17, -1.000000000000000000, -1.124819836996399911E-32 ) ) ;
#4889 = CARTESIAN_POINT ( 'NONE',  ( -1.233882608030000050, 1397.950738654029919, 196.1137546483980145 ) ) ;
#4891 = ORIENTED_EDGE ( 'NONE', *, *, #57291, .T. ) ;
#4890 = CARTESIAN_POINT ( 'NONE',  ( -8.126618747047817948, 1364.913278222060626, 208.3718459617061285 ) ) ;
#4892 = EDGE_LOOP ( 'NONE', ( #85187, #54785, #37181, #64258, #94394 ) ) ;
#4893 = EDGE_CURVE ( 'NONE', #106524, #26498, #73231, .T. ) ;
#4894 = CARTESIAN_POINT ( 'NONE',  ( 45.63712937690380755, 1440.913060387330006, 268.9747523971630017 ) ) ;
#4895 = CARTESIAN_POINT ( 'NONE',  ( -1.978433376304360003, 1467.924323865460110, 220.0703243356560108 ) ) ;
#4896 = CARTESIAN_POINT ( 'NONE',  ( 19.40350356789999964, 1457.232592156389956, 208.1907244810240059 ) ) ;
#4897 = CARTESIAN_POINT ( 'NONE',  ( -1.654395288670000186, 1485.634623599329871, 182.1583419804979940 ) ) ;
#4898 = CARTESIAN_POINT ( 'NONE',  ( -5.775625115495000017, 1516.745833913490060, 209.8771724060850090 ) ) ;
#4899 = EDGE_CURVE ( 'NONE', #81284, #7253, #83585, .T. ) ;
#4900 = CARTESIAN_POINT ( 'NONE',  ( -68.78495875209999610, 1379.747964692090136, 280.2437115059590269 ) ) ;
#4901 = CARTESIAN_POINT ( 'NONE',  ( -32.85805783624297760, 1523.678648413191695, 217.1983043299907763 ) ) ;
#4902 = CARTESIAN_POINT ( 'NONE',  ( 32.02808312589922224, 1512.187213306747481, 219.9649204700462235 ) ) ;
#4903 = CARTESIAN_POINT ( 'NONE',  ( 12.54660221610000193, 1415.996778984329922, 223.0356910586980064 ) ) ;
#4904 = CARTESIAN_POINT ( 'NONE',  ( 7.548872300095000654, 1510.418062979259958, 203.9404357814470075 ) ) ;
#4905 = ORIENTED_EDGE ( 'NONE', *, *, #45967, .T. ) ;
#4906 =( BOUNDED_CURVE ( )  B_SPLINE_CURVE ( 3, ( #98180, #56187, #20910, #55115 ),
 .UNSPECIFIED., .F., .F. ) 
 B_SPLINE_CURVE_WITH_KNOTS ( ( 4, 4 ),
 ( 4.424142070125560267, 5.579787944456629845 ),
 .UNSPECIFIED. ) 
 CURVE ( )  GEOMETRIC_REPRESENTATION_ITEM ( )  RATIONAL_B_SPLINE_CURVE ( ( 1.000000000000000000, 0.8917691661789544089, 0.8917691661789544089, 1.000000000000000000 ) ) 
 REPRESENTATION_ITEM ( '' )  );
#4907 = CARTESIAN_POINT ( 'NONE',  ( -4.625359562974999506, 1517.025470194390209, 206.6416589153869836 ) ) ;
#4908 = ORIENTED_EDGE ( 'NONE', *, *, #95207, .T. ) ;
#4909 = CARTESIAN_POINT ( 'NONE',  ( -36.37832866295120482, 1451.642701157629745, 135.6928041510159915 ) ) ;
#4910 = CARTESIAN_POINT ( 'NONE',  ( 32.02808312589916540, 1512.187213306747481, 198.2787714533495489 ) ) ;
#4911 = ORIENTED_EDGE ( 'NONE', *, *, #104138, .T. ) ;
#4912 = CARTESIAN_POINT ( 'NONE',  ( 8.469983976807428760, 1456.145527513871912, 227.1991206335947595 ) ) ;
#4913 = DIRECTION ( 'NONE',  ( 0.7414773880254664773, 0.000000000000000000, -0.6709778558543730842 ) ) ;
#4914 = CARTESIAN_POINT ( 'NONE',  ( -4.090588468780437914, 1440.341105203780216, 185.3471663033907362 ) ) ;
#4915 = CARTESIAN_POINT ( 'NONE',  ( -9.100602447694548403, 1384.657749302420143, 199.9536881146249812 ) ) ;
#4916 = CARTESIAN_POINT ( 'NONE',  ( 19.57944302010000115, 1410.092255016530089, 196.9053163625980005 ) ) ;
#4917 = FACE_OUTER_BOUND ( 'NONE', #83327, .T. ) ;
#4918 = CARTESIAN_POINT ( 'NONE',  ( -18.69816095120789612, 1522.382868172863937, 183.3860352823957953 ) ) ;
#4919 = CARTESIAN_POINT ( 'NONE',  ( 24.51476220920747195, 1444.144828869601270, 213.4463787509066606 ) ) ;
#4920 = AXIS2_PLACEMENT_3D ( 'NONE', #49390, #14667, #75694 ) ;
#4921 = SPHERICAL_SURFACE ( 'NONE', #19321, 2.000000000000000000 ) ;
#4922 = CARTESIAN_POINT ( 'NONE',  ( 5.006329581384999727, 1516.755758396839838, 215.6722354023569892 ) ) ;
#4923 = VERTEX_POINT ( 'NONE', #73551 ) ;
#4924 = CARTESIAN_POINT ( 'NONE',  ( 7.710967333700570414, 1516.608222572569957, 207.8710650191239893 ) ) ;
#4925 = CARTESIAN_POINT ( 'NONE',  ( -7.889297536996000559, 1517.051704408390378, 206.4074150262267722 ) ) ;
#4926 = CARTESIAN_POINT ( 'NONE',  ( -3.090336956749999864, 1448.965793307639842, 184.6975808967980015 ) ) ;
#4927 = CARTESIAN_POINT ( 'NONE',  ( 0.3740406207303079711, 1452.976564550639978, 183.2744760995269928 ) ) ;
#4928 = B_SPLINE_CURVE_WITH_KNOTS ( 'NONE', 3,
 ( #87832, #44164, #9443, #104610 ),
 .UNSPECIFIED., .F., .F.,
 ( 4, 4 ),
 ( 0.000000000000000000, 0.0002220129587134778832 ),
 .UNSPECIFIED. ) ;
#4929 = CARTESIAN_POINT ( 'NONE',  ( -40.26304726651319754, 1444.203404886970020, 137.0983463635160149 ) ) ;
#4930 = CARTESIAN_POINT ( 'NONE',  ( -5.432410439650000811, 1391.426148861440197, 209.1218459572589836 ) ) ;
#4931 = CARTESIAN_POINT ( 'NONE',  ( -16.66231036550740541, 1523.604703353109699, 180.4882076302515372 ) ) ;
#4932 = CARTESIAN_POINT ( 'NONE',  ( 18.00000152313205248, 1424.173982496956569, 225.4517810533038471 ) ) ;
#4933 = CARTESIAN_POINT ( 'NONE',  ( 2.234923440975000286, 1512.341036988540054, 216.7210731169070073 ) ) ;
#4934 = CARTESIAN_POINT ( 'NONE',  ( -21.83863729849021951, 1523.580204110583736, 183.2673815993471464 ) ) ;
#4935 = CARTESIAN_POINT ( 'NONE',  ( 36.96116112992849878, 1440.913060387089899, 254.5581055479269708 ) ) ;
#4936 = CARTESIAN_POINT ( 'NONE',  ( -11.33279196814429923, 1470.495430824379810, 210.3432187421609854 ) ) ;
#4937 = CARTESIAN_POINT ( 'NONE',  ( 11.36889272073800150, 1499.667877637589982, 204.5284518008890302 ) ) ;
#4938 = ORIENTED_EDGE ( 'NONE', *, *, #54341, .T. ) ;
#4939 = ORIENTED_EDGE ( 'NONE', *, *, #76019, .F. ) ;
#4940 = CARTESIAN_POINT ( 'NONE',  ( -2.487935123034410445, 1508.909942010395071, 213.6124651809371642 ) ) ;
#4941 = CIRCLE ( 'NONE', #44375, 10.71315034250000053 ) ;
#4942 = ADVANCED_FACE ( 'NONE', ( #21986 ), #50009, .F. ) ;
#4943 = CARTESIAN_POINT ( 'NONE',  ( 18.19590854888146580, 1501.977400791986611, 180.0410247165184217 ) ) ;
#4944 = CARTESIAN_POINT ( 'NONE',  ( -1.232506167737122516, 1409.632636740825774, 185.7525785795714341 ) ) ;
#4945 = CARTESIAN_POINT ( 'NONE',  ( 11.47870337641239935, 1502.276891194350128, 211.2824957803889845 ) ) ;
#4946 = VECTOR ( 'NONE', #52550, 1000.000000000000114 ) ;
#4947 = CARTESIAN_POINT ( 'NONE',  ( 15.06903345039999920, 1410.389868239730049, 191.5311856341979819 ) ) ;
#4948 = CARTESIAN_POINT ( 'NONE',  ( -30.61443310237114446, 1523.382868172864164, 221.8243310972803783 ) ) ;
#4949 = CARTESIAN_POINT ( 'NONE',  ( -40.03127858458480404, 1383.828107059689955, 241.8368436171929829 ) ) ;
#4950 = CIRCLE ( 'NONE', #81842, 33.13701971169416538 ) ;
#4951 = CARTESIAN_POINT ( 'NONE',  ( -4.538868782924999401, 1511.336728379370243, 201.0216414995070124 ) ) ;
#4952 = CARTESIAN_POINT ( 'NONE',  ( 16.19492434978379691, 1409.478599607480191, 224.1775087544979783 ) ) ;
#4953 = CARTESIAN_POINT ( 'NONE',  ( -11.46596297259700137, 1501.319154807139739, 208.6783501317359821 ) ) ;
#4954 = CARTESIAN_POINT ( 'NONE',  ( 2.281074820099999734, 1464.713448700129902, 235.8689246865980067 ) ) ;
#4956 = ORIENTED_EDGE ( 'NONE', *, *, #72866, .T. ) ;
#4955 = CARTESIAN_POINT ( 'NONE',  ( 32.38114538885255200, 1523.604703353109699, 216.1203639561429100 ) ) ;
#4957 = CARTESIAN_POINT ( 'NONE',  ( -0.6004483790419999911, 1452.607490234929855, 183.3312902083980021 ) ) ;
#4958 = EDGE_CURVE ( 'NONE', #94153, #88502, #4871, .T. ) ;
#4959 = CARTESIAN_POINT ( 'NONE',  ( -22.77753075879999756, 1378.937177693190051, 211.3942171327190067 ) ) ;
#4960 = CARTESIAN_POINT ( 'NONE',  ( 3.704457720059250114, 1508.551704408389924, 204.4495214305590025 ) ) ;
#4962 = ORIENTED_EDGE ( 'NONE', *, *, #64747, .T. ) ;
#4961 = CARTESIAN_POINT ( 'NONE',  ( -31.88717309313515713, 1525.425665131969481, 217.0217438353934369 ) ) ;
#4963 = CARTESIAN_POINT ( 'NONE',  ( 20.81805316561590047, 1457.016391092229924, 206.8941893600089941 ) ) ;
#4964 = EDGE_LOOP ( 'NONE', ( #95945, #97531, #89699, #54523 ) ) ;
#4965 = CARTESIAN_POINT ( 'NONE',  ( -12.48191901824699990, 1389.982499505159922, 213.9369507849619936 ) ) ;
#4966 = CARTESIAN_POINT ( 'NONE',  ( -4.329415264797339624, 1515.068899375750107, 206.1637497075489875 ) ) ;
#4967 = DIRECTION ( 'NONE',  ( 0.02616798426500960631, -0.9993150019883682011, -0.02616798426500960631 ) ) ;
#4968 = CARTESIAN_POINT ( 'NONE',  ( -11.60004869885203505, 1426.591398205465111, 134.9942363669703695 ) ) ;
#4969 = CARTESIAN_POINT ( 'NONE',  ( 1.484157417262786494, 1526.349684470114653, 178.3401290187298684 ) ) ;
#4970 = CARTESIAN_POINT ( 'NONE',  ( 2.620401159596264851, 1523.462669333490567, 242.1631858338582788 ) ) ;
#4971 = VECTOR ( 'NONE', #79904, 1000.000000000000227 ) ;
#4972 = CARTESIAN_POINT ( 'NONE',  ( 6.463161920097060253, 1409.138758974899929, 195.6150904016829770 ) ) ;
#4973 = DIRECTION ( 'NONE',  ( -4.137698748469999823E-18, -2.750577543510000101E-14, -1.000000000000000000 ) ) ;
#4974 = CARTESIAN_POINT ( 'NONE',  ( -108.9665184055720033, 1385.242083167919873, 297.1409723503389841 ) ) ;
#4975 = CARTESIAN_POINT ( 'NONE',  ( 0.000000000000000000, 1402.913060387289988, 209.1218459616989946 ) ) ;
#4976 = CARTESIAN_POINT ( 'NONE',  ( -67.96433663839999895, 1379.748578009009861, 278.4994408155590122 ) ) ;
#4977 = FACE_OUTER_BOUND ( 'NONE', #60016, .T. ) ;
#4978 = VERTEX_POINT ( 'NONE', #51094 ) ;
#4979 = ORIENTED_EDGE ( 'NONE', *, *, #69903, .F. ) ;
#4980 = EDGE_CURVE ( 'NONE', #42879, #48892, #80009, .T. ) ;
#4981 = CARTESIAN_POINT ( 'NONE',  ( 17.07724394729159911, 1524.330813522192102, 237.1903650275838800 ) ) ;
#4982 = CARTESIAN_POINT ( 'NONE',  ( -12.12507211471189805, 1416.051481378869994, 194.8051867232880170 ) ) ;
#4983 = CARTESIAN_POINT ( 'NONE',  ( -11.84681311729999820, 1434.711927244070012, 151.1872562620980034 ) ) ;
#4984 = EDGE_CURVE ( 'NONE', #6840, #23910, #66807, .T. ) ;
#4985 = CARTESIAN_POINT ( 'NONE',  ( -8.184993690210469467E-10, 1468.121328536410147, 248.6278164530129970 ) ) ;
#4986 = CARTESIAN_POINT ( 'NONE',  ( -20.15323670362180053, 1493.393816397240016, 190.8089475466459817 ) ) ;
#4987 = CARTESIAN_POINT ( 'NONE',  ( -15.33731769819999968, 1420.146962874850033, 211.9565886041989984 ) ) ;
#4988 = CARTESIAN_POINT ( 'NONE',  ( -109.8240211180000045, 1384.930942008709962, 311.3852198412590155 ) ) ;
#4989 = CARTESIAN_POINT ( 'NONE',  ( 0.1648048234879999907, 1483.385634709730084, 181.9489519295979676 ) ) ;
#4990 = CARTESIAN_POINT ( 'NONE',  ( -11.03646466085811895, 1367.416071951358845, 208.3718459617010978 ) ) ;
#4991 = CARTESIAN_POINT ( 'NONE',  ( -45.88148358874209976, 1440.468640267019964, 266.4123968719909499 ) ) ;
#4992 = CARTESIAN_POINT ( 'NONE',  ( 13.92249237623939884, 1452.656259886599855, 223.1400375642430163 ) ) ;
#4993 = B_SPLINE_CURVE_WITH_KNOTS ( 'NONE', 5,
 ( #19595, #71146, #87935, #54882, #49107, #71715, #12295, #96876, #2291, #80620, #5433, #45927, #45388, #105267, #20145, #80062, #54342, #70594 ),
 .UNSPECIFIED., .F., .F.,
 ( 6, 3, 3, 3, 3, 6 ),
 ( 0.000000000000000000, 0.2202946003694152555, 0.3397378414386151846, 0.5088681883646077875, 0.8372692437405104826, 1.000000000000000000 ),
 .UNSPECIFIED. ) ;
#4994 = ADVANCED_FACE ( 'NONE', ( #101454 ), #25875, .T. ) ;
#4995 = CARTESIAN_POINT ( 'NONE',  ( -7.727327152855000492, 1517.232977404109988, 207.4118332116069894 ) ) ;
#4996 = AXIS2_PLACEMENT_3D ( 'NONE', #84298, #24379, #23278 ) ;
#4997 = CARTESIAN_POINT ( 'NONE',  ( -9.178648612314900035, 1447.470203629239904, 211.6527240042640017 ) ) ;
#4998 = DIRECTION ( 'NONE',  ( -1.755985294532469921E-16, 1.000000000000000000, -1.338183447452831989E-16 ) ) ;
#4999 = CARTESIAN_POINT ( 'NONE',  ( -13.52518119320440171, 1435.051496296169944, 149.4677306140820008 ) ) ;
#5000 = CARTESIAN_POINT ( 'NONE',  ( -8.859600949860000796, 1385.023751217870085, 218.6831814923290267 ) ) ;
#5001 = CARTESIAN_POINT ( 'NONE',  ( -14.44139730133570154, 1379.629733965419973, 208.1340535457149770 ) ) ;
#5002 = DIRECTION ( 'NONE',  ( 0.000000000000000000, 1.000000000000000000, 0.000000000000000000 ) ) ;
#5003 = EDGE_CURVE ( 'NONE', #34701, #14678, #26360, .T. ) ;
#5004 = ORIENTED_EDGE ( 'NONE', *, *, #54592, .F. ) ;
#5005 = CARTESIAN_POINT ( 'NONE',  ( 32.79493994350000463, 1434.501496568570019, 248.1152222124979971 ) ) ;
#5006 = CARTESIAN_POINT ( 'NONE',  ( -2.795964621609999590, 1422.864594294989956, 191.4386244948990168 ) ) ;
#5008 = CARTESIAN_POINT ( 'NONE',  ( -1.325823302270159987, 1507.620489792419903, 232.0621709551870140 ) ) ;
#5007 = CARTESIAN_POINT ( 'NONE',  ( -2.484903766530000002, 1458.411121269429941, 182.9125316254979907 ) ) ;
#5009 = CARTESIAN_POINT ( 'NONE',  ( 21.91250632045888125, 1506.380977038693800, 207.4373042671960548 ) ) ;
#5010 = CARTESIAN_POINT ( 'NONE',  ( -3.773954403609999897, 1421.529510570530192, 216.2239751100380261 ) ) ;
#5011 = CARTESIAN_POINT ( 'NONE',  ( 7.565983030562289713, 1517.051704408389924, 209.5600921240870207 ) ) ;
#5012 = CARTESIAN_POINT ( 'NONE',  ( -4.967560240179940578, 1452.739589361249955, 152.0866475748709945 ) ) ;
#5013 = CARTESIAN_POINT ( 'NONE',  ( -18.95839814150000180, 1416.827520077830059, 207.7798181853180211 ) ) ;
#5014 = VERTEX_POINT ( 'NONE', #91978 ) ;
#5015 = DIRECTION ( 'NONE',  ( 1.755985294532464991E-16, -1.000000000000000000, 1.338183447452830017E-16 ) ) ;
#5016 = DIRECTION ( 'NONE',  ( -1.000000000000000000, 0.000000000000000000, 0.000000000000000000 ) ) ;
#5017 = FACE_OUTER_BOUND ( 'NONE', #44553, .T. ) ;
#5018 = ORIENTED_EDGE ( 'NONE', *, *, #103442, .T. ) ;
#5019 = VERTEX_POINT ( 'NONE', #68457 ) ;
#5020 = EDGE_CURVE ( 'NONE', #101781, #28929, #94173, .T. ) ;
#5021 = CARTESIAN_POINT ( 'NONE',  ( 9.331306786325548330, 1452.122598230650055, 210.5717110549620088 ) ) ;
#5022 = CARTESIAN_POINT ( 'NONE',  ( 5.450648847440000111, 1423.857684999099774, 194.2417023985990170 ) ) ;
#5023 = ORIENTED_EDGE ( 'NONE', *, *, #28403, .F. ) ;
#5024 = CARTESIAN_POINT ( 'NONE',  ( -20.98459803374076671, 1522.051704408389924, 201.4854660376508377 ) ) ;
#5025 = CARTESIAN_POINT ( 'NONE',  ( 7.675506710379999653, 1490.901593261789913, 210.2162091181089920 ) ) ;
#5026 = VECTOR ( 'NONE', #83048, 1000.000000000000114 ) ;
#5027 = EDGE_CURVE ( 'NONE', #38078, #23627, #85342, .T. ) ;
#5028 = CONICAL_SURFACE ( 'NONE', #96245, 0.9999999999999857891, 0.7853981633970000820 ) ;
#5029 = CARTESIAN_POINT ( 'NONE',  ( -6.753454085369999582, 1489.056761658230016, 234.9017483617980133 ) ) ;
#5030 = CARTESIAN_POINT ( 'NONE',  ( 0.2645430705366629831, 1443.121743617909942, 200.2023352529839997 ) ) ;
#5031 = ORIENTED_EDGE ( 'NONE', *, *, #64741, .T. ) ;
#5032 = AXIS2_PLACEMENT_3D ( 'NONE', #93054, #16327, #84651 ) ;
#5033 = CARTESIAN_POINT ( 'NONE',  ( 45.63691652665460197, 1441.836777326350102, 268.9749693829069770 ) ) ;
#5034 = CARTESIAN_POINT ( 'NONE',  ( -12.73594778875919964, 1416.524489948229984, 221.9712528552830122 ) ) ;
#5035 = CARTESIAN_POINT ( 'NONE',  ( 0.05678182167189999713, 1418.511462927230014, 184.6660934127980340 ) ) ;
#5036 = CARTESIAN_POINT ( 'NONE',  ( -6.557909920764999789, 1516.908489800550115, 203.3441005368270282 ) ) ;
#5037 = VERTEX_POINT ( 'NONE', #42683 ) ;
#5038 = CARTESIAN_POINT ( 'NONE',  ( 7.375496855036300481, 1483.107846205720080, 218.3651359022439919 ) ) ;
#5039 = CARTESIAN_POINT ( 'NONE',  ( 12.91984442206437578, 1442.902292219558149, 187.0613185807262084 ) ) ;
#5040 = VERTEX_POINT ( 'NONE', #84123 ) ;
#5041 = ORIENTED_EDGE ( 'NONE', *, *, #63813, .F. ) ;
#5042 = CARTESIAN_POINT ( 'NONE',  ( -11.41699241967629952, 1481.865938852530235, 208.5945336717069836 ) ) ;
#5043 = CARTESIAN_POINT ( 'NONE',  ( 4.554961988741982992, 1508.731359868795835, 205.6342593440040503 ) ) ;
#5044 = CARTESIAN_POINT ( 'NONE',  ( 12.89273669479999995, 1508.859229393329997, 233.8778408584979900 ) ) ;
#5045 = CARTESIAN_POINT ( 'NONE',  ( -14.75568483658040009, 1513.870294662259994, 194.1736459919410152 ) ) ;
#5046 = CARTESIAN_POINT ( 'NONE',  ( 21.41738597313630166, 1452.165148788659963, 141.3889158671639734 ) ) ;
#5047 = CARTESIAN_POINT ( 'NONE',  ( 12.23993107200000097, 1420.119835428209853, 199.7451907216789948 ) ) ;
#5048 = CARTESIAN_POINT ( 'NONE',  ( 0.3127569488372759499, 1475.234939895219895, 220.5412273341300136 ) ) ;
#5049 = CARTESIAN_POINT ( 'NONE',  ( -109.3435511536187903, 1382.472266926233942, 297.4003323660738261 ) ) ;
#5050 = CARTESIAN_POINT ( 'NONE',  ( -18.95791602736232306, 1509.575124649889176, 231.6168982108185901 ) ) ;
#5051 = CARTESIAN_POINT ( 'NONE',  ( 0.02347612988675716952, 1409.045439741765676, 232.3809737551641774 ) ) ;
#5053 = CARTESIAN_POINT ( 'NONE',  ( 17.01808896600000054, 1507.624369720630057, 193.6805215186979865 ) ) ;
#5052 = CARTESIAN_POINT ( 'NONE',  ( -16.83010722181489882, 1416.063878291570290, 191.5921218490719866 ) ) ;
#5054 = CARTESIAN_POINT ( 'NONE',  ( 10.79561051538090055, 1423.418703670030027, 206.7986195382829919 ) ) ;
#5055 = PRESENTATION_LAYER_ASSIGNMENT (  '', '', ( #24767 ) ) ;
#5056 = CARTESIAN_POINT ( 'NONE',  ( -25.38913556476300215, 1509.752285549599947, 222.9524089379939653 ) ) ;
#5057 = CARTESIAN_POINT ( 'NONE',  ( -7.743766119884999632, 1514.370494773840164, 202.8627129457869955 ) ) ;
#5058 = ORIENTED_EDGE ( 'NONE', *, *, #73390, .F. ) ;
#5059 = CARTESIAN_POINT ( 'NONE',  ( 5.998951827550000004, 1470.912646799889899, 213.0429767062390169 ) ) ;
#5060 = CARTESIAN_POINT ( 'NONE',  ( -16.76711878018801372, 1417.195629503265309, 207.2570596610230780 ) ) ;
#5061 = CARTESIAN_POINT ( 'NONE',  ( -92.03063779543769840, 1384.964829711410175, 309.3299059855730206 ) ) ;
#5062 = CARTESIAN_POINT ( 'NONE',  ( -8.618443112799999639, 1386.703020315259892, 200.0643205304990033 ) ) ;
#5063 = CARTESIAN_POINT ( 'NONE',  ( 8.799694164910118133, 1425.068530136420122, 210.2036770632330160 ) ) ;
#5065 = ORIENTED_EDGE ( 'NONE', *, *, #74029, .T. ) ;
#5064 = CARTESIAN_POINT ( 'NONE',  ( -16.50454912150300046, 1419.915473451730122, 209.2650646900050049 ) ) ;
#5066 = CARTESIAN_POINT ( 'NONE',  ( 3.663504462200000145, 1429.509591348389904, 216.7335040807589905 ) ) ;
#5067 = CARTESIAN_POINT ( 'NONE',  ( -1.639582970820000041, 1434.541746329560056, 150.4377894671980016 ) ) ;
#5068 = CARTESIAN_POINT ( 'NONE',  ( -16.52561552909999776, 1416.917924532109964, 208.4225654288269993 ) ) ;
#5069 = CARTESIAN_POINT ( 'NONE',  ( -21.38516915557943321, 1522.382868172863937, 237.8497028174240313 ) ) ;
#5070 = CARTESIAN_POINT ( 'NONE',  ( 14.37690900153499918, 1514.216506490359961, 225.6932579665669891 ) ) ;
#5071 = DIRECTION ( 'NONE',  ( -5.980589973904019347E-17, 1.000000000000000000, -1.736889445713099699E-16 ) ) ;
#5072 = CARTESIAN_POINT ( 'NONE',  ( 2.357442550764540012, 1458.086361592170306, 199.7974089473029835 ) ) ;
#5073 = FACE_OUTER_BOUND ( 'NONE', #35074, .T. ) ;
#5074 = CARTESIAN_POINT ( 'NONE',  ( 2.938302457570000303, 1419.757091722530049, 232.0470454606980013 ) ) ;
#5075 = EDGE_CURVE ( 'NONE', #8045, #31574, #41588, .T. ) ;
#5076 = CARTESIAN_POINT ( 'NONE',  ( -3.469833849039999683E-16, 1426.566393376330097, 144.1938086916980239 ) ) ;
#5077 = CARTESIAN_POINT ( 'NONE',  ( 10.80134480061119895, 1441.261220175989820, 153.0805715986579969 ) ) ;
#5078 = CARTESIAN_POINT ( 'NONE',  ( -18.59938032009999986, 1409.727296728430019, 222.5591327112979911 ) ) ;
#5079 = CARTESIAN_POINT ( 'NONE',  ( 29.30029655192931770, 1525.907212628473872, 221.3719603026171114 ) ) ;
#5080 = CARTESIAN_POINT ( 'NONE',  ( 20.59733728950000042, 1508.015129919730043, 189.9429528794979944 ) ) ;
#5081 = CARTESIAN_POINT ( 'NONE',  ( 1.955657237439999863, 1459.028687623489986, 202.4574169284290122 ) ) ;
#5082 = CARTESIAN_POINT ( 'NONE',  ( 20.49599333844834348, 1525.960063244517187, 184.3798832129035077 ) ) ;
#5083 = CARTESIAN_POINT ( 'NONE',  ( 0.008119676858140530140, 1515.178500008189985, 204.7953747115290071 ) ) ;
#5084 = CARTESIAN_POINT ( 'NONE',  ( 12.52897032537950217, 1427.032053915000006, 206.3112042049379795 ) ) ;
#5085 = CARTESIAN_POINT ( 'NONE',  ( 32.02808312589922224, 1512.187213306747481, 221.9649204700462235 ) ) ;
#5086 = CARTESIAN_POINT ( 'NONE',  ( -6.194271847559999600, 1415.931669658129977, 226.1787850318980020 ) ) ;
#5087 = CARTESIAN_POINT ( 'NONE',  ( 0.2104582539746929770, 1457.090827936239975, 183.0778992351330032 ) ) ;
#5088 = CARTESIAN_POINT ( 'NONE',  ( -9.160204422789998802, 1409.232941774529991, 221.2278796158979901 ) ) ;
#5089 = CARTESIAN_POINT ( 'NONE',  ( 8.727114281347018832, 1428.313213898079994, 213.1854654111380114 ) ) ;
#5090 = CARTESIAN_POINT ( 'NONE',  ( 18.88880210473194765, 1524.667648926078982, 179.4140113511355423 ) ) ;
#5091 = ADVANCED_FACE ( 'NONE', ( #92518 ), #32995, .F. ) ;
#5092 = CARTESIAN_POINT ( 'NONE',  ( 3.629220049600000220, 1485.493215689190038, 199.0019176958990101 ) ) ;
#5093 = CARTESIAN_POINT ( 'NONE',  ( 11.87527449220000086, 1433.007027006299950, 149.0256347040979961 ) ) ;
#5094 = DIRECTION ( 'NONE',  ( 0.9536973727975270876, 0.1200132783607290032, -0.2757863922244979671 ) ) ;
#5095 = CARTESIAN_POINT ( 'NONE',  ( 11.97824860639999933, 1442.481624454889925, 187.4134949571979973 ) ) ;
#5096 = ORIENTED_EDGE ( 'NONE', *, *, #71920, .T. ) ;
#5097 = CARTESIAN_POINT ( 'NONE',  ( -16.49279218151803050, 1525.408327360769363, 181.2883303505538493 ) ) ;
#5098 = CARTESIAN_POINT ( 'NONE',  ( 9.293015197429999930, 1478.078892413390122, 202.6398356817990134 ) ) ;
#5099 = CARTESIAN_POINT ( 'NONE',  ( -10.35541825330239973, 1409.274679561159928, 219.9120658599189824 ) ) ;
#5100 = CARTESIAN_POINT ( 'NONE',  ( -11.04294906800000042, 1491.966910088589884, 207.3598305497890237 ) ) ;
#5101 = CARTESIAN_POINT ( 'NONE',  ( -15.41079858738659958, 1501.813619937609928, 192.8668813100890134 ) ) ;
#5102 = CARTESIAN_POINT ( 'NONE',  ( 43.55237166414823236, 1430.623344126982829, 269.0332385863825948 ) ) ;
#5103 = CIRCLE ( 'NONE', #103491, 1.999999999999997780 ) ;
#5104 = CARTESIAN_POINT ( 'NONE',  ( -19.62842490763629399, 1495.540557520950642, 189.3275510559486179 ) ) ;
#5105 = CARTESIAN_POINT ( 'NONE',  ( -12.30373392569999957, 1378.362863315840059, 209.9037182927540073 ) ) ;
#5106 = CARTESIAN_POINT ( 'NONE',  ( -107.0634112298879899, 1384.587327643060007, 311.2343609292589690 ) ) ;
#5107 = CARTESIAN_POINT ( 'NONE',  ( -54.03892782705099762, 1385.034468983960096, 232.0668901380410034 ) ) ;
#5108 = CARTESIAN_POINT ( 'NONE',  ( 17.84338787571921614, 1523.481610426287716, 180.3600277896298110 ) ) ;
#5109 = CARTESIAN_POINT ( 'NONE',  ( -4.301731299663230423, 1508.551704408389924, 204.9156561448070022 ) ) ;
#5110 = CIRCLE ( 'NONE', #99897, 1.000000000000059064 ) ;
#5111 = CARTESIAN_POINT ( 'NONE',  ( -27.54194134069999933, 1451.798912744530071, 135.7745631451980159 ) ) ;
#5112 = CARTESIAN_POINT ( 'NONE',  ( 1.488474718485413906, 1526.348417187221685, 178.3303222095514400 ) ) ;
#5113 = CARTESIAN_POINT ( 'NONE',  ( -15.91558000873799905, 1409.468827912599863, 225.2516522794149978 ) ) ;
#5115 = VERTEX_POINT ( 'NONE', #95839 ) ;
#5114 = CARTESIAN_POINT ( 'NONE',  ( 0.5122327485485929088, 1410.651863534059885, 185.0574092668310016 ) ) ;
#5116 = CARTESIAN_POINT ( 'NONE',  ( -9.845241469799999479, 1507.507259092430104, 182.3675330799979974 ) ) ;
#5117 = CARTESIAN_POINT ( 'NONE',  ( 10.82166596142770132, 1471.344689967329941, 210.9651955021979859 ) ) ;
#5118 = DIRECTION ( 'NONE',  ( -0.8236474686107847498, 0.5669078173018529121, -0.01484500364079613562 ) ) ;
#5119 = CARTESIAN_POINT ( 'NONE',  ( -109.4871642380000054, 1384.813187038689875, 311.2830328522589980 ) ) ;
#5120 = DIRECTION ( 'NONE',  ( -0.8907681516580484571, 1.273087901431153894E-31, 0.4544580288560254311 ) ) ;
#5121 = CARTESIAN_POINT ( 'NONE',  ( -1.088650671229999922, 1420.780442655370052, 193.7338955114989858 ) ) ;
#5122 = EDGE_CURVE ( 'NONE', #37608, #21803, #92536, .T. ) ;
#5123 = CARTESIAN_POINT ( 'NONE',  ( 22.68241477640000170, 1411.065318295730094, 214.3862589840079806 ) ) ;
#5124 = CARTESIAN_POINT ( 'NONE',  ( -1.984486858693230493, 1410.354035999710050, 186.2309706543619825 ) ) ;
#5125 = CARTESIAN_POINT ( 'NONE',  ( -13.38188607319999868, 1469.919367367889890, 192.0112524093990203 ) ) ;
#5126 = PLANE ( 'NONE',  #57157 ) ;
#5128 = CARTESIAN_POINT ( 'NONE',  ( 16.19188814560000012, 1409.478493580929808, 223.7357041228979995 ) ) ;
#5127 = CARTESIAN_POINT ( 'NONE',  ( -2.957486053519140956, 1512.146863357693292, 201.2343373090091347 ) ) ;
#5129 = CARTESIAN_POINT ( 'NONE',  ( 24.65388594573819958, 1430.511875713700192, 208.0202360571709903 ) ) ;
#5130 = CARTESIAN_POINT ( 'NONE',  ( -113.4000000000000057, 1368.558218059089995, 292.3061701549589770 ) ) ;
#5131 = EDGE_CURVE ( 'NONE', #36118, #72991, #2370, .T. ) ;
#5132 = DIRECTION ( 'NONE',  ( -1.836970198721029688E-16, -1.000000000000000000, 0.000000000000000000 ) ) ;
#5133 = CARTESIAN_POINT ( 'NONE',  ( -0.9888743217240001382, 1417.038468317130310, 234.0372654507980030 ) ) ;
#5134 = CARTESIAN_POINT ( 'NONE',  ( 8.726849315049999944, 1367.111769039820047, 210.6218459616991936 ) ) ;
#5135 = EDGE_CURVE ( 'NONE', #85592, #22264, #60356, .T. ) ;
#5136 = CARTESIAN_POINT ( 'NONE',  ( 2.285487581364999965, 1517.001127920769704, 205.0775242521070254 ) ) ;
#5137 = CIRCLE ( 'NONE', #60636, 1.000000000000000888 ) ;
#5138 = CARTESIAN_POINT ( 'NONE',  ( -3.344054220715769965, 1485.138363243759841, 183.2114304489670076 ) ) ;
#5139 = CARTESIAN_POINT ( 'NONE',  ( -9081.484824850398581, 5182.767774292099602, -1567.708540563249926 ) ) ;
#5140 = CARTESIAN_POINT ( 'NONE',  ( 14.35483100429999936, 1416.837177087930058, 196.6648189961979938 ) ) ;
#5142 = VERTEX_POINT ( 'NONE', #5076 ) ;
#5141 = CARTESIAN_POINT ( 'NONE',  ( -68.16062186043509996, 1379.746616918160043, 279.7065836077829886 ) ) ;
#5143 = EDGE_CURVE ( 'NONE', #94751, #77737, #27812, .T. ) ;
#5144 = EDGE_LOOP ( 'NONE', ( #76940, #42317, #64742, #2628, #47320 ) ) ;
#5145 = CARTESIAN_POINT ( 'NONE',  ( 26.91098882550000226, 1508.590122467729998, 215.2366165824080042 ) ) ;
#5146 = ORIENTED_EDGE ( 'NONE', *, *, #42524, .F. ) ;
#5147 = CARTESIAN_POINT ( 'NONE',  ( -1.270117472468459852, 1486.209137599609903, 220.9629115624290137 ) ) ;
#5148 = CARTESIAN_POINT ( 'NONE',  ( -18.68355584089999866, 1410.903490300429894, 196.1540984432980110 ) ) ;
#5150 = CARTESIAN_POINT ( 'NONE',  ( 1.361079355559999815, 1508.999526997630028, 179.4746003585979963 ) ) ;
#5149 = CARTESIAN_POINT ( 'NONE',  ( -11.59426166675470071, 1425.891398669320097, 141.1919140291859947 ) ) ;
#5151 = CARTESIAN_POINT ( 'NONE',  ( 2.881325373965000214, 1517.003078582959688, 210.2407492406470055 ) ) ;
#5152 = CARTESIAN_POINT ( 'NONE',  ( -25.43901382002360023, 1451.305424502000051, 136.9267323982909659 ) ) ;
#5153 = CARTESIAN_POINT ( 'NONE',  ( -11.63663615270000129, 1425.864876078829866, 144.1644678891980220 ) ) ;
#5154 = CARTESIAN_POINT ( 'NONE',  ( 11.56026858080000075, 1410.250182171229881, 229.1792121341979964 ) ) ;
#5155 = CARTESIAN_POINT ( 'NONE',  ( 7.231901239322829689, 1483.532524091059940, 217.6548318471419918 ) ) ;
#5156 = PRODUCT_CONTEXT ( 'NONE', #93479, 'mechanical' ) ;
#5157 = CARTESIAN_POINT ( 'NONE',  ( 39.33777287878179862, 1438.052711710340191, 134.0999999977100003 ) ) ;
#5158 = CARTESIAN_POINT ( 'NONE',  ( -39.81703491479910184, 1441.203410251259811, 136.8482318521629963 ) ) ;
#5159 = ORIENTED_EDGE ( 'NONE', *, *, #5131, .F. ) ;
#5160 = CARTESIAN_POINT ( 'NONE',  ( 4.677562605459999467, 1434.889072344290071, 228.7640133631989841 ) ) ;
#5161 = CARTESIAN_POINT ( 'NONE',  ( -17.00631957490619683, 1410.874949912819375, 226.2321320020102462 ) ) ;
#5162 = VERTEX_POINT ( 'NONE', #106445 ) ;
#5163 = VERTEX_POINT ( 'NONE', #29188 ) ;
#5164 = CARTESIAN_POINT ( 'NONE',  ( -5.706397885535000825, 1514.325389163589989, 216.7730352073269842 ) ) ;
#5165 = CARTESIAN_POINT ( 'NONE',  ( 16.31974134803240872, 1514.485057798524167, 194.4298416830750682 ) ) ;
#5166 = CARTESIAN_POINT ( 'NONE',  ( 0.2078300974330000161, 1450.905802800400124, 181.2506496984979947 ) ) ;
#5167 = CARTESIAN_POINT ( 'NONE',  ( -3.212068473500000465, 1485.523016082529921, 182.9307348487979823 ) ) ;
#5168 = DIRECTION ( 'NONE',  ( -5.980589973904019347E-17, 1.000000000000000000, -1.736889445713099699E-16 ) ) ;
#5169 = ADVANCED_FACE ( 'NONE', ( #29728 ), #52169, .T. ) ;
#5170 = AXIS2_PLACEMENT_3D ( 'NONE', #62071, #47861, #81434 ) ;
#5171 = CARTESIAN_POINT ( 'NONE',  ( -3.487592469391230132, 1509.038615938009798, 204.6345961782960217 ) ) ;
#5172 = CARTESIAN_POINT ( 'NONE',  ( -68.07264245651541046, 1379.746555617447939, 278.5801731380780097 ) ) ;
#5173 = CARTESIAN_POINT ( 'NONE',  ( -1.347198969329999940, 1464.928942339390005, 198.6034036249990038 ) ) ;
#5174 = CARTESIAN_POINT ( 'NONE',  ( -2.258825589925000266, 1511.942942747529969, 201.5330432499970073 ) ) ;
#5175 = ADVANCED_FACE ( 'NONE', ( #72852 ), #46562, .F. ) ;
#5176 = CARTESIAN_POINT ( 'NONE',  ( 11.61528297179999925, 1414.971352895729979, 197.1579143274979913 ) ) ;
#5177 = CARTESIAN_POINT ( 'NONE',  ( -74.59470942271289573, 1384.765139218380000, 274.7532847296519662 ) ) ;
#5178 = ORIENTED_EDGE ( 'NONE', *, *, #63092, .T. ) ;
#5179 = DIRECTION ( 'NONE',  ( -1.755985294532469921E-16, 1.000000000000000000, -1.338183447452831989E-16 ) ) ;
#5180 = CARTESIAN_POINT ( 'NONE',  ( 3.255809864005000165, 1516.837969789639828, 208.3644199470059846 ) ) ;
#5181 = ORIENTED_EDGE ( 'NONE', *, *, #70326, .T. ) ;
#5182 = CARTESIAN_POINT ( 'NONE',  ( 11.24049413620000060, 1414.988015881329829, 222.4824404014979962 ) ) ;
#5183 = AXIS2_PLACEMENT_3D ( 'NONE', #103286, #110608, #16514 ) ;
#5184 = CARTESIAN_POINT ( 'NONE',  ( 19.25108290950000267, 1467.194595399430000, 227.2294850399980248 ) ) ;
#5185 = EDGE_LOOP ( 'NONE', ( #86439, #100951, #9561, #15847 ) ) ;
#5186 = CARTESIAN_POINT ( 'NONE',  ( 0.06655362833503029873, 1450.915384491239820, 181.8858670609800186 ) ) ;
#5187 = CARTESIAN_POINT ( 'NONE',  ( -15.83337727950000229, 1409.465974096930040, 192.3897112323980139 ) ) ;
#5188 = DIRECTION ( 'NONE',  ( 0.9751355587651674428, 0.000000000000000000, 0.2216092101690377847 ) ) ;
#5189 = CARTESIAN_POINT ( 'NONE',  ( -10.11189522083689951, 1462.195248612440082, 207.9445251505729857 ) ) ;
#5190 = CARTESIAN_POINT ( 'NONE',  ( -5.450781814275990733, 1434.502290401799883, 217.0838862464160002 ) ) ;
#5191 = CARTESIAN_POINT ( 'NONE',  ( -5.652025646554889704, 1510.855104182140167, 201.5207535327680262 ) ) ;
#5192 = CARTESIAN_POINT ( 'NONE',  ( -2.164025747320000193, 1508.926860436930156, 179.8555707243980066 ) ) ;
#5193 = CARTESIAN_POINT ( 'NONE',  ( -6.178095865712184498, 1510.835436358435118, 201.6599032209836082 ) ) ;
#5194 = CARTESIAN_POINT ( 'NONE',  ( -21.38516915558021125, 1522.906561336852519, 180.3939891059724516 ) ) ;
#5196 = CARTESIAN_POINT ( 'NONE',  ( -11.60004869885203505, 1423.252811911736217, 137.0073056665461309 ) ) ;
#5195 = CARTESIAN_POINT ( 'NONE',  ( 15.48256451790000021, 1460.897023939530072, 229.7631170700979908 ) ) ;
#5197 = CARTESIAN_POINT ( 'NONE',  ( 16.16632277704800558, 1511.187213306747708, 236.8966194768523508 ) ) ;
#5198 = B_SPLINE_CURVE_WITH_KNOTS ( 'NONE', 3,
 ( #220, #42750, #69637, #18622, #51154, #763, #1878, #9149, #27061, #78562, #50602, #60119, #61247, #95361, #102621, #18080, #43313, #103181, #77461, #85850, #94805, #26483, #60679, #52275, #34892 ),
 .UNSPECIFIED., .F., .F.,
 ( 4, 3, 3, 3, 3, 3, 3, 3, 4 ),
 ( -7.454989583650000640, -7.295847338557649664, -6.603480943530409597, -5.920148531335569508, -5.256832802792740011, -4.983278890925820548, -4.387781186674780010, -3.607420121254749645, -3.058675454859999476 ),
 .UNSPECIFIED. ) ;
#5199 = VECTOR ( 'NONE', #47929, 1000.000000000000000 ) ;
#5200 = CARTESIAN_POINT ( 'NONE',  ( -5.778999811904999895, 1516.955859323880077, 216.4549161051170074 ) ) ;
#5201 = AXIS2_PLACEMENT_3D ( 'NONE', #49841, #85612, #75601 ) ;
#5202 = CARTESIAN_POINT ( 'NONE',  ( 0.03632882829513719297, 1486.486083103770170, 181.8024630677937523 ) ) ;
#5203 = CARTESIAN_POINT ( 'NONE',  ( -0.1417130572052019977, 1507.672022827310002, 180.7972791130320047 ) ) ;
#5204 = AXIS2_PLACEMENT_3D ( 'NONE', #24042, #8355, #68860 ) ;
#5205 = CARTESIAN_POINT ( 'NONE',  ( 18.70435367232109058, 1445.431086849344638, 214.8978195684285879 ) ) ;
#5206 = CARTESIAN_POINT ( 'NONE',  ( -5.772727946874999461, 1516.691414181030041, 212.5791125756269935 ) ) ;
#5207 = CARTESIAN_POINT ( 'NONE',  ( 18.59896181469999732, 1509.326147590929850, 187.7623525226980234 ) ) ;
#5208 = CARTESIAN_POINT ( 'NONE',  ( 19.37374569213924502, 1526.382868172863937, 183.8768763279539655 ) ) ;
#5210 = ORIENTED_EDGE ( 'NONE', *, *, #75298, .T. ) ;
#5209 = CARTESIAN_POINT ( 'NONE',  ( -113.4000000000000057, 1386.449969320030050, 311.2218459572590064 ) ) ;
#5211 = CARTESIAN_POINT ( 'NONE',  ( -7.649966233313090669, 1508.551704408389924, 219.0282755267929815 ) ) ;
#5212 = CARTESIAN_POINT ( 'NONE',  ( 3.115880663340000023, 1508.551704408389924, 219.3718645306990140 ) ) ;
#5213 = CARTESIAN_POINT ( 'NONE',  ( -10.96572839600000115, 1432.076500672689917, 151.7663020546979737 ) ) ;
#5214 = CARTESIAN_POINT ( 'NONE',  ( 19.22285271143139695, 1456.937641708669844, 224.8075632610019738 ) ) ;
#5215 = CARTESIAN_POINT ( 'NONE',  ( -109.9659341548349971, 1384.416896023069967, 311.4329124691320203 ) ) ;
#5216 = CARTESIAN_POINT ( 'NONE',  ( 3.218260586992740091, 1432.346978324299926, 155.4230415804039751 ) ) ;
#5217 = CARTESIAN_POINT ( 'NONE',  ( 7.345629923129999739, 1422.263538441430001, 195.5717800564989943 ) ) ;
#5218 = B_SPLINE_CURVE_WITH_KNOTS ( 'NONE', 5,
 ( #98225, #73606, #22587, #29913, #39979, #56237 ),
 .UNSPECIFIED., .F., .F.,
 ( 6, 6 ),
 ( 4.250950522270000143, 7.082025451739999866 ),
 .UNSPECIFIED. ) ;
#5219 = CARTESIAN_POINT ( 'NONE',  ( -5.489226993980830471, 1448.625211997490169, 211.5470588731079715 ) ) ;
#5221 = FACE_OUTER_BOUND ( 'NONE', #39014, .T. ) ;
#5220 = CARTESIAN_POINT ( 'NONE',  ( -21.84276879380000125, 1457.439937068030076, 221.7697786318980206 ) ) ;
#5222 = CARTESIAN_POINT ( 'NONE',  ( 19.41979707700000191, 1457.606582239089903, 210.0704631242259950 ) ) ;
#5223 = CIRCLE ( 'NONE', #83939, 0.9999999999999930056 ) ;
#5224 = VERTEX_POINT ( 'NONE', #21848 ) ;
#5225 = CARTESIAN_POINT ( 'NONE',  ( -1.714334285315000095, 1516.699825673279975, 205.0952314524469955 ) ) ;
#5226 = CARTESIAN_POINT ( 'NONE',  ( 4.982688416889999417, 1406.041084510129849, 267.2248725163979657 ) ) ;
#5227 = CARTESIAN_POINT ( 'NONE',  ( -32.85805783624300602, 1523.678648413191695, 217.1983043299907763 ) ) ;
#5228 = DIRECTION ( 'NONE',  ( 0.9996573249755517088, 0.02617694830808742559, 0.000000000000000000 ) ) ;
#5229 = CARTESIAN_POINT ( 'NONE',  ( 21.88093256148639654, 1429.722962281219907, 218.2777509189953093 ) ) ;
#5230 = CARTESIAN_POINT ( 'NONE',  ( -1.551161424019060098, 1463.265709907049995, 199.4650991780359846 ) ) ;
#5231 = DIRECTION ( 'NONE',  ( -1.755985294532469921E-16, 1.000000000000000000, -1.338183447452831989E-16 ) ) ;
#5232 = CARTESIAN_POINT ( 'NONE',  ( -2.298816264069999615, 1486.462377070590037, 220.8289805453990198 ) ) ;
#5233 = CARTESIAN_POINT ( 'NONE',  ( -1.462738481218180064, 1450.687750463569955, 155.0630832256589997 ) ) ;
#5234 = CARTESIAN_POINT ( 'NONE',  ( -1.598127250451339076, 1450.771782104136264, 183.3389037459045880 ) ) ;
#5235 = CARTESIAN_POINT ( 'NONE',  ( -19.84652166835276432, 1485.605575737134131, 190.5233726884732732 ) ) ;
#5236 = CARTESIAN_POINT ( 'NONE',  ( -14.30082345506849961, 1416.007771869980161, 221.2306877730480039 ) ) ;
#5237 = CARTESIAN_POINT ( 'NONE',  ( -3.906019471690000078, 1515.551703594190030, 210.6105386114290070 ) ) ;
#5238 = CARTESIAN_POINT ( 'NONE',  ( -25.65427092280000210, 1434.769004650220268, 243.9198229650980068 ) ) ;
#5239 = CARTESIAN_POINT ( 'NONE',  ( -26.98839749300549684, 1508.001257810110019, 211.5020470289859986 ) ) ;
#5240 = CARTESIAN_POINT ( 'NONE',  ( -19.64992913029231403, 1519.551704408389924, 210.5515370058381279 ) ) ;
#5241 = CARTESIAN_POINT ( 'NONE',  ( -6.177389037570000241, 1475.457658709629868, 269.0307152584979917 ) ) ;
#5242 = DIRECTION ( 'NONE',  ( -0.000000000000000000, -1.000000000000000000, -0.000000000000000000 ) ) ;
#5244 = CARTESIAN_POINT ( 'NONE',  ( -18.60876427879999895, 1443.367094472220060, 192.4891415986979837 ) ) ;
#5243 = B_SPLINE_CURVE_WITH_KNOTS ( 'NONE', 3,
 ( #14043, #91320, #39819, #71818, #29217, #39259, #54993, #5104, #73980, #108110, #72342, #98611 ),
 .UNSPECIFIED., .F., .F.,
 ( 4, 2, 2, 2, 2, 4 ),
 ( 0.000000000000000000, 0.2500000000000155431, 0.3750000000000233147, 0.5000000000000310862, 0.7500000000000155431, 1.000000000000000000 ),
 .UNSPECIFIED. ) ;
#5245 = CARTESIAN_POINT ( 'NONE',  ( -6.524649951413074689, 1486.518242610188963, 182.3718320799524975 ) ) ;
#5246 = CARTESIAN_POINT ( 'NONE',  ( -29.34764347683880104, 1384.830841659480029, 227.3863593227910087 ) ) ;
#5247 = CARTESIAN_POINT ( 'NONE',  ( -31.18497486287767728, 1524.152349020271004, 221.8763673812615878 ) ) ;
#5248 = CARTESIAN_POINT ( 'NONE',  ( -17.21411445179911581, 1414.941240495250440, 207.5657464664730583 ) ) ;
#5249 = B_SPLINE_SURFACE_WITH_KNOTS ( 'NONE', 5, 5, ( 
 ( #89479, #64859, #64302, #14404, #12774, #98967 ),
 ( #79980, #71628, #29565, #46951, #46405, #21694 ),
 ( #63749, #37980, #97863, #72693, #98422, #8208 ),
 ( #14952, #25555, #32334, #108485, #42374, #76529 ),
 ( #24454, #59747, #32862, #67601, #102275, #74357 ),
 ( #25002, #16586, #23902, #41826, #67054, #16051 ),
 ( #75457, #33972, #50254, #84383, #7670, #7127 ),
 ( #75982, #40176, #31768, #50783, #110133, #92228 ),
 ( #101160, #58642, #93323, #59205, #110681, #68168 ) ),
 .UNSPECIFIED., .F., .F., .F.,
 ( 6, 3, 6 ),
 ( 6, 6 ),
 ( 0.000000000000000000, 3.172668598669999618, 4.759002897999999426 ),
 ( 0.000000000000000000, 14.00000000000000000 ),
 .UNSPECIFIED. ) ;
#5250 = CARTESIAN_POINT ( 'NONE',  ( -105.4205408459999944, 1379.023436635359985, 302.8723641076589956 ) ) ;
#5251 = CARTESIAN_POINT ( 'NONE',  ( 31.65139097221404541, 1525.320849883639767, 216.1854601993777294 ) ) ;
#5252 = CARTESIAN_POINT ( 'NONE',  ( -1.270728281904929924, 1414.996443537369942, 226.4582996361970118 ) ) ;
#5253 = CARTESIAN_POINT ( 'NONE',  ( -22.18770510819999942, 1409.852309958130036, 204.0989260225280191 ) ) ;
#5254 =( BOUNDED_CURVE ( )  B_SPLINE_CURVE ( 3, ( #58994, #16391, #50586, #84716 ),
 .UNSPECIFIED., .F., .T. ) 
 B_SPLINE_CURVE_WITH_KNOTS ( ( 4, 4 ),
 ( 0.5395807524025459934, 1.539014399144550405 ),
 .UNSPECIFIED. ) 
 CURVE ( )  GEOMETRIC_REPRESENTATION_ITEM ( )  RATIONAL_B_SPLINE_CURVE ( ( 1.000000000000000000, 0.9184788592068002799, 0.9184788592068002799, 1.000000000000000000 ) ) 
 REPRESENTATION_ITEM ( '' )  );
#5255 = CARTESIAN_POINT ( 'NONE',  ( 12.74090128278689882, 1421.413457440939965, 206.2481278393109960 ) ) ;
#5256 = VECTOR ( 'NONE', #59809, 1000.000000000000000 ) ;
#5257 = CARTESIAN_POINT ( 'NONE',  ( 19.68098305160793515, 1455.410563046006473, 226.0042006104999075 ) ) ;
#5258 = EDGE_CURVE ( 'NONE', #49199, #29269, #2470, .T. ) ;
#5259 = ORIENTED_EDGE ( 'NONE', *, *, #33197, .F. ) ;
#5260 = CARTESIAN_POINT ( 'NONE',  ( -8.919353607585813748, 1410.596373793224302, 230.1706237015127954 ) ) ;
#5261 = CARTESIAN_POINT ( 'NONE',  ( -7.550503362009299835, 1510.480349264700180, 214.6730346447039892 ) ) ;
#5262 = CARTESIAN_POINT ( 'NONE',  ( 10.75631864651809977, 1451.138109684059827, 190.3409053450899933 ) ) ;
#5264 = CARTESIAN_POINT ( 'NONE',  ( -11.75640701316500092, 1511.791180387469922, 193.9413991097669907 ) ) ;
#5263 = CARTESIAN_POINT ( 'NONE',  ( 11.63658902509999926, 1425.864914507529875, 144.1610765019980249 ) ) ;
#5265 = CARTESIAN_POINT ( 'NONE',  ( 27.65015272131789814, 1446.921108212359968, 137.0757173949590140 ) ) ;
#5266 = CARTESIAN_POINT ( 'NONE',  ( -6.942973667334999988, 1516.833844030519913, 201.7931697622170191 ) ) ;
#5267 = CARTESIAN_POINT ( 'NONE',  ( 7.984273842250000364, 1426.916635774389988, 211.9701635203690273 ) ) ;
#5268 = CARTESIAN_POINT ( 'NONE',  ( -21.44637799630000075, 1506.412602296789828, 216.0243671510289971 ) ) ;
#5269 = CARTESIAN_POINT ( 'NONE',  ( 15.90990255763500016, 1512.830284628050094, 198.1616908427670296 ) ) ;
#5270 = CARTESIAN_POINT ( 'NONE',  ( -18.88624094756929850, 1419.246025400399958, 205.9308376352330185 ) ) ;
#5271 = CARTESIAN_POINT ( 'NONE',  ( -86.54208378602990592, 1379.132636796130100, 301.6681089792259627 ) ) ;
#5272 = CIRCLE ( 'NONE', #35641, 2.000000000000001776 ) ;
#5273 = CARTESIAN_POINT ( 'NONE',  ( 7.445922712490000706, 1367.935115748530052, 207.6218459616989946 ) ) ;
#5275 = ORIENTED_EDGE ( 'NONE', *, *, #78745, .T. ) ;
#5274 = CARTESIAN_POINT ( 'NONE',  ( -14.05185835220319923, 1379.611218837149863, 211.6671715642569893 ) ) ;
#5276 = ORIENTED_EDGE ( 'NONE', *, *, #70145, .F. ) ;
#5277 = EDGE_CURVE ( 'NONE', #88595, #59778, #46067, .T. ) ;
#5278 = CARTESIAN_POINT ( 'NONE',  ( -10.60671173099999898, 1397.919176979029999, 200.8919131671280240 ) ) ;
#5279 = CARTESIAN_POINT ( 'NONE',  ( -21.99779390299999804, 1409.845345892729711, 211.9582520095080156 ) ) ;
#5280 = CARTESIAN_POINT ( 'NONE',  ( -1.052431931479999916, 1415.163755984229965, 226.8636908286979974 ) ) ;
#5281 = CARTESIAN_POINT ( 'NONE',  ( -13.18815759610568605, 1444.720196239782808, 169.3929182581312887 ) ) ;
#5282 = CARTESIAN_POINT ( 'NONE',  ( 47.22425680062420383, 1578.884105819039860, 226.9120406781360089 ) ) ;
#5283 = CARTESIAN_POINT ( 'NONE',  ( 2.329920886069499986, 1515.492270357839971, 204.9835198734710104 ) ) ;
#5285 = CARTESIAN_POINT ( 'NONE',  ( 16.92682308619999887, 1419.037090534729941, 226.7348578532979957 ) ) ;
#5284 = CARTESIAN_POINT ( 'NONE',  ( -8.407635077709999294, 1384.019446811960051, 218.5970489128289955 ) ) ;
#5286 = CARTESIAN_POINT ( 'NONE',  ( 3.219365683689999980, 1429.769570239930090, 184.9205627192980330 ) ) ;
#5287 = CARTESIAN_POINT ( 'NONE',  ( -11.30589511670000036, 1414.913060387329779, 196.4146731187979924 ) ) ;
#5288 = EDGE_CURVE ( 'NONE', #86711, #1325, #81140, .T. ) ;
#5289 = CARTESIAN_POINT ( 'NONE',  ( -40.04713527513419535, 1448.341380581330213, 135.9090988750369888 ) ) ;
#5290 = CARTESIAN_POINT ( 'NONE',  ( 10.99103875765120009, 1396.296875918300202, 210.4629671561480109 ) ) ;
#5291 = CARTESIAN_POINT ( 'NONE',  ( 1.350316101520000256, 1416.274718424630009, 190.2409646149980063 ) ) ;
#5292 = CARTESIAN_POINT ( 'NONE',  ( 11.55624295700000026, 1430.790237445429966, 151.0224672601980274 ) ) ;
#5293 = CARTESIAN_POINT ( 'NONE',  ( 7.380526832584999752, 1511.503799556579906, 202.6426608137470282 ) ) ;
#5294 = ORIENTED_EDGE ( 'NONE', *, *, #58517, .T. ) ;
#5295 = CARTESIAN_POINT ( 'NONE',  ( 3.961598046809999829, 1423.998203942029932, 183.4328845819979961 ) ) ;
#5296 = CARTESIAN_POINT ( 'NONE',  ( 21.55808780551086556, 1523.844782250846038, 234.2610829425819361 ) ) ;
#5297 = VERTEX_POINT ( 'NONE', #66123 ) ;
#5298 = ORIENTED_EDGE ( 'NONE', *, *, #43218, .F. ) ;
#5299 = CARTESIAN_POINT ( 'NONE',  ( 11.13894495610000135, 1491.363598464389952, 209.7173500882680059 ) ) ;
#5300 = DIRECTION ( 'NONE',  ( 0.000000000000000000, 1.000000000000000000, 0.000000000000000000 ) ) ;
#5301 = CARTESIAN_POINT ( 'NONE',  ( -109.8944536047824130, 1385.812234818686193, 311.3867069332368374 ) ) ;
#5302 = CARTESIAN_POINT ( 'NONE',  ( -29.86461515634922037, 1525.960063244517187, 197.2746849027940641 ) ) ;
#5303 = CARTESIAN_POINT ( 'NONE',  ( 0.7538707352880020807, 1516.719999691880048, 216.0603247549969979 ) ) ;
#5304 = CARTESIAN_POINT ( 'NONE',  ( -13.19407264773069954, 1379.711643100160245, 208.4819402826470025 ) ) ;
#5305 = ORIENTED_EDGE ( 'NONE', *, *, #93194, .F. ) ;
#5306 = CARTESIAN_POINT ( 'NONE',  ( -11.97066799919999980, 1502.729030670490147, 208.4344832896910020 ) ) ;
#5307 = CARTESIAN_POINT ( 'NONE',  ( 2.500000000000000000, 1448.507635988019956, 160.4651386227409944 ) ) ;
#5308 = CARTESIAN_POINT ( 'NONE',  ( -55.86512536059999690, 1374.936376805820146, 252.9328197391589867 ) ) ;
#5309 = EDGE_CURVE ( 'NONE', #38904, #24522, #90458, .T. ) ;
#5310 = CARTESIAN_POINT ( 'NONE',  ( 5.061321880549999541, 1415.087745006229852, 225.4285409366979991 ) ) ;
#5311 = CARTESIAN_POINT ( 'NONE',  ( 4.997573787194999895, 1516.742629295279812, 205.6633194342169872 ) ) ;
#5312 = ORIENTED_EDGE ( 'NONE', *, *, #10943, .T. ) ;
#5313 = CARTESIAN_POINT ( 'NONE',  ( 4.037050997585000189, 1516.939819969850078, 209.1086255745840106 ) ) ;
#5314 = CIRCLE ( 'NONE', #33914, 22.86690257359991207 ) ;
#5315 = CARTESIAN_POINT ( 'NONE',  ( -20.10853138519999916, 1509.039643839130122, 229.5731426189979913 ) ) ;
#5316 = CARTESIAN_POINT ( 'NONE',  ( -29.84310692597631842, 1419.462045361091214, 269.4691403088048105 ) ) ;
#5317 = CARTESIAN_POINT ( 'NONE',  ( 6.527830543224999893, 1512.220794350770120, 216.8989209840169963 ) ) ;
#5319 = ORIENTED_EDGE ( 'NONE', *, *, #102056, .T. ) ;
#5318 = CARTESIAN_POINT ( 'NONE',  ( -4.884981308350000102E-15, 1408.913060387329779, 191.3838116191980134 ) ) ;
#5320 = CARTESIAN_POINT ( 'NONE',  ( -0.01271949248029489998, 1452.441493942580109, 183.1886361936269907 ) ) ;
#5321 = CARTESIAN_POINT ( 'NONE',  ( -33.18846733439090002, 1440.913060389980046, 247.0360926224090292 ) ) ;
#5322 = CARTESIAN_POINT ( 'NONE',  ( -89.66120661540000469, 1384.333980646620148, 308.7172663300589761 ) ) ;
#5323 = CARTESIAN_POINT ( 'NONE',  ( -0.1242689031270829830, 1466.391594368360074, 235.6938023998040137 ) ) ;
#5324 = CARTESIAN_POINT ( 'NONE',  ( 7.478702110549999560, 1409.021897787929902, 270.4228357812979766 ) ) ;
#5325 = CARTESIAN_POINT ( 'NONE',  ( 5.785582913545000316, 1516.981965530290154, 213.1542438721070027 ) ) ;
#5326 = CARTESIAN_POINT ( 'NONE',  ( -54.30030265850000859, 1379.725094345220214, 248.9924859156590173 ) ) ;
#5327 = CARTESIAN_POINT ( 'NONE',  ( 23.71731968020000281, 1410.130348990129960, 209.4170045476479913 ) ) ;
#5328 = CARTESIAN_POINT ( 'NONE',  ( -20.13259047659999723, 1508.866004122629874, 188.8141438244979895 ) ) ;
#5329 = CARTESIAN_POINT ( 'NONE',  ( -7.262210027532643331, 1423.020617356984985, 139.1422465717866146 ) ) ;
#5330 = CARTESIAN_POINT ( 'NONE',  ( -7.708877905894440552, 1516.528429087750055, 211.1705659669590034 ) ) ;
#5331 = CARTESIAN_POINT ( 'NONE',  ( 4.045182479925000685, 1517.057265928030120, 210.8256255754569963 ) ) ;
#5332 = CARTESIAN_POINT ( 'NONE',  ( -3.271537981817990381, 1454.292002020450127, 199.1638778446669846 ) ) ;
#5333 = CARTESIAN_POINT ( 'NONE',  ( 15.10324330609999954, 1409.440477264029823, 192.5109551743979921 ) ) ;
#5334 = CARTESIAN_POINT ( 'NONE',  ( -109.9987472809999929, 1384.922094923150098, 311.2741087182590149 ) ) ;
#5336 = ORIENTED_EDGE ( 'NONE', *, *, #103310, .T. ) ;
#5335 = CARTESIAN_POINT ( 'NONE',  ( -26.83711809360000089, 1388.514028352690048, 223.1242661799589939 ) ) ;
#5337 = CARTESIAN_POINT ( 'NONE',  ( -40.64111485381250333, 1385.178332084029762, 243.2412163901340136 ) ) ;
#5338 = VECTOR ( 'NONE', #14091, 1000.000000000000000 ) ;
#5339 = DIRECTION ( 'NONE',  ( 0.000000000000000000, 1.000000000000000000, 1.036208156316812031E-12 ) ) ;
#5340 = CARTESIAN_POINT ( 'NONE',  ( 0.1366081833359999997, 1416.109320291729773, 233.5463589650980225 ) ) ;
#5341 = PRODUCT_DEFINITION_SHAPE ( 'NONE', 'NONE',  #93161 ) ;
#5342 = CARTESIAN_POINT ( 'NONE',  ( -20.76201028965770234, 1508.885069966210040, 228.4351800535669952 ) ) ;
#5343 = CARTESIAN_POINT ( 'NONE',  ( 7.550503318189189628, 1510.480349263560129, 203.5706572562480119 ) ) ;
#5344 = CARTESIAN_POINT ( 'NONE',  ( 12.89505355770000072, 1420.989633701210096, 203.4267449422790150 ) ) ;
#5345 = DIRECTION ( 'NONE',  ( 1.755985294532469921E-16, -1.000000000000000000, 1.338183447452831989E-16 ) ) ;
#5347 = CARTESIAN_POINT ( 'NONE',  ( -7.968704128189949998, 1384.504568802437689, 199.5050640420236618 ) ) ;
#5346 = CARTESIAN_POINT ( 'NONE',  ( -1.125509888415000104, 1517.203017563489766, 216.4609531728469847 ) ) ;
#5348 = CARTESIAN_POINT ( 'NONE',  ( -4.772433264290000032, 1461.586210710390105, 228.1254610687989839 ) ) ;
#5349 = CARTESIAN_POINT ( 'NONE',  ( 31.81407709660777883, 1522.382868172863937, 221.9534378623329474 ) ) ;
#5350 = ORIENTED_EDGE ( 'NONE', *, *, #15257, .T. ) ;
#5351 = CARTESIAN_POINT ( 'NONE',  ( -6.942344729965000738, 1516.810037859429940, 201.4055938791270250 ) ) ;
#5352 = CARTESIAN_POINT ( 'NONE',  ( 10.51581569650209858, 1481.161035245299900, 208.1366864954699736 ) ) ;
#5353 = VERTEX_POINT ( 'NONE', #67760 ) ;
#5354 = VECTOR ( 'NONE', #11730, 1000.000000000000114 ) ;
#5355 = CARTESIAN_POINT ( 'NONE',  ( 21.83550407203919974, 1523.678648413191695, 234.9693198511250785 ) ) ;
#5356 = CARTESIAN_POINT ( 'NONE',  ( 19.44861509849999948, 1455.533462210330072, 225.7267910435979843 ) ) ;
#5357 = CARTESIAN_POINT ( 'NONE',  ( 10.93222784191639896, 1461.420118457989929, 209.9621245680470167 ) ) ;
#5358 = CARTESIAN_POINT ( 'NONE',  ( 7.551708674585110082, 1510.523965798400013, 203.3918062713489974 ) ) ;
#5359 = CARTESIAN_POINT ( 'NONE',  ( 2.395822483399999925, 1441.661856669790041, 218.7568551047190226 ) ) ;
#5360 = CARTESIAN_POINT ( 'NONE',  ( 16.20463669235772386, 1421.461506550293507, 227.3035140667420251 ) ) ;
#5361 = DIRECTION ( 'NONE',  ( 0.000000000000000000, 1.000000000000000000, -0.000000000000000000 ) ) ;
#5362 = CARTESIAN_POINT ( 'NONE',  ( -19.24690813209999973, 1426.102494106830136, 224.1205169862979858 ) ) ;
#5363 = CARTESIAN_POINT ( 'NONE',  ( -25.00976051679999657, 1436.598010167069788, 137.9330532114979917 ) ) ;
#5364 = CARTESIAN_POINT ( 'NONE',  ( -108.3356498620000110, 1388.869567454079970, 298.1379939792590221 ) ) ;
#5365 = CARTESIAN_POINT ( 'NONE',  ( 19.35574166329999812, 1498.080849027529894, 189.0919305048980164 ) ) ;
#5367 = CARTESIAN_POINT ( 'NONE',  ( -18.45403838167598209, 1436.531269343617168, 212.9422139639101772 ) ) ;
#5366 = CARTESIAN_POINT ( 'NONE',  ( 20.39893125378086580, 1526.069472839386208, 185.1113182959254857 ) ) ;
#5368 = CARTESIAN_POINT ( 'NONE',  ( -29.82636534510967508, 1462.376341263100585, 269.4689657811763368 ) ) ;
#5369 = ORIENTED_EDGE ( 'NONE', *, *, #109924, .F. ) ;
#5370 = CARTESIAN_POINT ( 'NONE',  ( -105.4154991850000016, 1378.862308729909955, 303.3418524678589847 ) ) ;
#5371 = CARTESIAN_POINT ( 'NONE',  ( -15.53181541920000086, 1508.521255623489878, 214.8366523089289899 ) ) ;
#5372 = DIRECTION ( 'NONE',  ( -1.755985294532469921E-16, 1.000000000000000000, -1.338183447452831989E-16 ) ) ;
#5373 = CARTESIAN_POINT ( 'NONE',  ( 32.10254378951870535, 1525.211473355384896, 201.2198347410968893 ) ) ;
#5374 = CARTESIAN_POINT ( 'NONE',  ( -0.9776412681320001408, 1475.513060387329915, 230.7453403689980007 ) ) ;
#5375 = AXIS2_PLACEMENT_3D ( 'NONE', #34462, #94922, #43974 ) ;
#5376 = CARTESIAN_POINT ( 'NONE',  ( 1.461235200690810032, 1494.741996085649816, 181.6529089755349844 ) ) ;
#5377 = CARTESIAN_POINT ( 'NONE',  ( -32.38114538885259464, 1523.604703353109699, 202.1233279672532888 ) ) ;
#5378 = CARTESIAN_POINT ( 'NONE',  ( -13.24008678843756925, 1444.663275562806803, 186.6390711729250711 ) ) ;
#5379 = B_SPLINE_SURFACE_WITH_KNOTS ( 'NONE', 5, 5, ( 
 ( #2759, #36879, #88393, #10586, #28488, #71074 ),
 ( #78338, #27376, #44757, #61558, #35785, #2213 ),
 ( #79991, #62680, #80548, #37441, #105758, #71638 ),
 ( #104082, #29043, #78905, #46416, #3863, #37991 ),
 ( #100092, #108495, #6033, #39641, #82741, #91687 ),
 ( #64868, #81622, #65413, #74367, #29574, #107939 ) ),
 .UNSPECIFIED., .F., .F., .F.,
 ( 6, 6 ),
 ( 6, 6 ),
 ( 22.07912247049999976, 26.44584043820000119 ),
 ( 0.000000000000000000, 0.5000000000000000000 ),
 .UNSPECIFIED. ) ;
#5380 = CARTESIAN_POINT ( 'NONE',  ( -13.72878287234173555, 1517.051704408389924, 226.2713469440930112 ) ) ;
#5381 = CARTESIAN_POINT ( 'NONE',  ( 3.582189414718509823, 1494.866532486610140, 220.1463443050500075 ) ) ;
#5382 = B_SPLINE_CURVE_WITH_KNOTS ( 'NONE', 3,
 ( #109925, #57883, #33204, #67394, #56217, #23698, #90347, #49479, #13627, #56772, #31551, #5255, #73587, #107718, #90910, #14193, #74133, #108265, #65728, #23141, #57346, #91470, #14750, #6358, #40507 ),
 .UNSPECIFIED., .F., .F.,
 ( 4, 3, 3, 3, 3, 3, 3, 3, 4 ),
 ( -25.30278126027359775, -25.08579948689999739, -24.77235297171529993, -24.14468077163109783, -23.20356205636220182, -22.54016880708680048, -21.81726924789879973, -20.86314243152489922, -19.77745610209999683 ),
 .UNSPECIFIED. ) ;
#5383 = CARTESIAN_POINT ( 'NONE',  ( -1.810647825301244129, 1415.577673978943039, 233.0806231791490291 ) ) ;
#5384 = CARTESIAN_POINT ( 'NONE',  ( -103.9411501300010059, 1383.761452288409828, 310.9608569221110201 ) ) ;
#5385 = CARTESIAN_POINT ( 'NONE',  ( -9.599657450428111360, 1460.198427500139815, 210.0868860100479765 ) ) ;
#5386 = CARTESIAN_POINT ( 'NONE',  ( -0.4165852338731970139, 1516.813354641049955, 201.4055070984510110 ) ) ;
#5388 = ORIENTED_EDGE ( 'NONE', *, *, #73718, .T. ) ;
#5387 = CARTESIAN_POINT ( 'NONE',  ( -14.72054864259999896, 1409.427113273230134, 225.7256316435980068 ) ) ;
#5389 = CARTESIAN_POINT ( 'NONE',  ( -109.9987472819999965, 1383.757409383979848, 311.0847451122589860 ) ) ;
#5390 = CARTESIAN_POINT ( 'NONE',  ( 14.92122229814569856, 1514.080593477150160, 223.9397791912049911 ) ) ;
#5391 = ORIENTED_EDGE ( 'NONE', *, *, #14745, .T. ) ;
#5392 = VERTEX_POINT ( 'NONE', #7827 ) ;
#5393 = CARTESIAN_POINT ( 'NONE',  ( 16.49832412793039893, 1414.913057855109855, 209.6477601274349922 ) ) ;
#5394 = CARTESIAN_POINT ( 'NONE',  ( 12.86976130269999885, 1508.080714966730056, 233.3011978812979805 ) ) ;
#5396 = CARTESIAN_POINT ( 'NONE',  ( -10.01186952459999802, 1466.025750520630027, 244.5548898232979980 ) ) ;
#5395 = CARTESIAN_POINT ( 'NONE',  ( 3.694265505850000242, 1454.607279123389844, 217.7787218116090173 ) ) ;
#5397 = CARTESIAN_POINT ( 'NONE',  ( 8.958374100104808946, 1436.656241311369968, 210.3666130420500053 ) ) ;
#5398 = CARTESIAN_POINT ( 'NONE',  ( -11.90032380669999945, 1433.331458429630175, 150.1435198483980287 ) ) ;
#5399 = CARTESIAN_POINT ( 'NONE',  ( 7.868158389100000427, 1422.937290482379922, 214.1570520181289794 ) ) ;
#5400 = FACE_OUTER_BOUND ( 'NONE', #11486, .T. ) ;
#5401 = CARTESIAN_POINT ( 'NONE',  ( -25.47645757409999945, 1436.566927373820135, 137.1740747294979883 ) ) ;
#5402 = CARTESIAN_POINT ( 'NONE',  ( -1.345088944733920044, 1515.083299843980058, 213.4508101154519863 ) ) ;
#5403 = CARTESIAN_POINT ( 'NONE',  ( -4.500000000000000000, 1448.210448412289907, 183.1418046154980175 ) ) ;
#5404 = CARTESIAN_POINT ( 'NONE',  ( 12.86636877496950149, 1428.376440794390192, 223.7743079858460078 ) ) ;
#5405 = CARTESIAN_POINT ( 'NONE',  ( 5.604365146370000161, 1361.139420828410039, 207.6218459616989946 ) ) ;
#5406 = CARTESIAN_POINT ( 'NONE',  ( -1.365576857718376003, 1509.093805881863091, 239.1218459691334033 ) ) ;
#5408 = ORIENTED_EDGE ( 'NONE', *, *, #45670, .T. ) ;
#5407 = CARTESIAN_POINT ( 'NONE',  ( 1.395903919076789877E-08, 1408.640860330559917, 261.6452554441709708 ) ) ;
#5409 = VERTEX_POINT ( 'NONE', #41998 ) ;
#5410 = ADVANCED_FACE ( 'NONE', ( #101873 ), #50955, .F. ) ;
#5411 = CARTESIAN_POINT ( 'NONE',  ( 16.50400130224771544, 1525.907212628473644, 236.2546788475581820 ) ) ;
#5412 = CARTESIAN_POINT ( 'NONE',  ( 13.71656619866890026, 1499.109475169520010, 227.7998406596679786 ) ) ;
#5413 = CARTESIAN_POINT ( 'NONE',  ( -14.72002262839999887, 1469.537467531630227, 269.3627926194980091 ) ) ;
#5414 = CARTESIAN_POINT ( 'NONE',  ( -0.9686567332709090650, 1473.830917872273858, 219.3200354843431228 ) ) ;
#5415 = CARTESIAN_POINT ( 'NONE',  ( -124.5778210737999672, 1377.418846546389204, 315.3996670310588115 ) ) ;
#5417 = CARTESIAN_POINT ( 'NONE',  ( 33.93383603481760247, 1451.270696425840015, 135.9469434958280090 ) ) ;
#5416 = B_SPLINE_CURVE_WITH_KNOTS ( 'NONE', 3,
 ( #51264, #44532, #43429, #42875, #1994, #36129 ),
 .UNSPECIFIED., .F., .F.,
 ( 4, 2, 4 ),
 ( 0.000000000000000000, 0.5000000000000000000, 1.000000000000000000 ),
 .UNSPECIFIED. ) ;
#5418 = AXIS2_PLACEMENT_3D ( 'NONE', #37414, #12197, #105733 ) ;
#5419 = CARTESIAN_POINT ( 'NONE',  ( 0.3830348160098190347, 1450.899684516809884, 181.3422595746110062 ) ) ;
#5420 = CARTESIAN_POINT ( 'NONE',  ( -8.369575833189999869, 1384.742689880740045, 199.7789889385390154 ) ) ;
#5421 = EDGE_CURVE ( 'NONE', #89175, #36972, #105152, .T. ) ;
#5422 = CARTESIAN_POINT ( 'NONE',  ( 17.94074846905810006, 1431.033909182950083, 205.7008688429760070 ) ) ;
#5423 = CARTESIAN_POINT ( 'NONE',  ( -6.210220977990000613, 1458.870741700389772, 216.9690521252790063 ) ) ;
#5424 = CARTESIAN_POINT ( 'NONE',  ( 11.96845083018959421, 1365.600286352959529, 209.6218459617033432 ) ) ;
#5425 = CARTESIAN_POINT ( 'NONE',  ( -39.67050070681160179, 1422.888949612689885, 266.6045514581650195 ) ) ;
#5426 = CIRCLE ( 'NONE', #7185, 2.000000000000009770 ) ;
#5427 = VERTEX_POINT ( 'NONE', #83987 ) ;
#5428 = CARTESIAN_POINT ( 'NONE',  ( -24.24612263075051288, 1442.627844462843541, 211.5705962792871446 ) ) ;
#5429 = EDGE_LOOP ( 'NONE', ( #19653, #94004, #43352, #4868, #80229 ) ) ;
#5430 = ORIENTED_EDGE ( 'NONE', *, *, #24009, .T. ) ;
#5431 = CARTESIAN_POINT ( 'NONE',  ( 2.494757998004999866, 1516.937508036699910, 210.8228737931069929 ) ) ;
#5432 = CARTESIAN_POINT ( 'NONE',  ( -8.794092324118190973, 1447.789040521789957, 212.1549648291330072 ) ) ;
#5433 = CARTESIAN_POINT ( 'NONE',  ( -105.5320588160000028, 1381.208403848540001, 299.1971426474589748 ) ) ;
#5435 =( LENGTH_UNIT ( ) NAMED_UNIT ( * ) SI_UNIT ( .MILLI., .METRE. ) );
#5434 = CARTESIAN_POINT ( 'NONE',  ( -7.323034312095000331, 1516.609912606490070, 212.5765947784269940 ) ) ;
#5436 = CARTESIAN_POINT ( 'NONE',  ( -16.51001495079999870, 1425.424181616729811, 190.9332292383980132 ) ) ;
#5437 = CARTESIAN_POINT ( 'NONE',  ( -1.992696810621175540, 1450.242131535874478, 182.8294641353408281 ) ) ;
#5438 = ORIENTED_EDGE ( 'NONE', *, *, #46699, .T. ) ;
#5439 = CARTESIAN_POINT ( 'NONE',  ( -26.41196673809999851, 1435.620866968539985, 136.0816445379979882 ) ) ;
#5440 = CARTESIAN_POINT ( 'NONE',  ( 5.778372563615000068, 1516.932669162149978, 202.1763558832970205 ) ) ;
#5441 = DIRECTION ( 'NONE',  ( -0.001183870442918495778, 0.9989952321583787098, 0.04480094391417914490 ) ) ;
#5442 = CARTESIAN_POINT ( 'NONE',  ( 2.294541319819646041, 1508.993187694497465, 238.4785069940606661 ) ) ;
#5443 = CARTESIAN_POINT ( 'NONE',  ( -43.48865640085159612, 1435.886059616880175, 270.3367133951149981 ) ) ;
#5444 = CARTESIAN_POINT ( 'NONE',  ( -17.29393938232498229, 1523.621879633028811, 180.8572348224460882 ) ) ;
#5445 = CARTESIAN_POINT ( 'NONE',  ( -4.717969115980000794, 1396.259831671730126, 198.0836446571979934 ) ) ;
#5447 = ORIENTED_EDGE ( 'NONE', *, *, #74822, .T. ) ;
#5446 = CARTESIAN_POINT ( 'NONE',  ( -8.000269850835890040, 1364.913076074710261, 209.6218459617148824 ) ) ;
#5448 = ORIENTED_EDGE ( 'NONE', *, *, #6645, .F. ) ;
#5449 = CARTESIAN_POINT ( 'NONE',  ( 0.4364087686210000316, 1450.897820657319926, 181.2764007302979792 ) ) ;
#5450 = CARTESIAN_POINT ( 'NONE',  ( 32.26066749790219745, 1465.087609890807016, 269.3103000282806647 ) ) ;
#5451 = LINE ( 'NONE', #23883, #107492 ) ;
#5452 = CARTESIAN_POINT ( 'NONE',  ( -3.669386717783980068, 1517.051704642929963, 215.6629163041010031 ) ) ;
#5453 = AXIS2_PLACEMENT_3D ( 'NONE', #71828, #2406, #2953 ) ;
#5454 = CARTESIAN_POINT ( 'NONE',  ( -0.03560127825697149279, 1409.432827519930242, 185.3548041051600137 ) ) ;
#5455 = CARTESIAN_POINT ( 'NONE',  ( 2.493697040924999886, 1516.977201124959947, 210.2401991861970032 ) ) ;
#5456 = CARTESIAN_POINT ( 'NONE',  ( 2.372478608332516892, 1522.382868172863937, 174.8996806668726549 ) ) ;
#5457 = CARTESIAN_POINT ( 'NONE',  ( 2.596345137909159551, 1439.736139237240195, 157.6563016627050047 ) ) ;
#5458 = CARTESIAN_POINT ( 'NONE',  ( 0.000000000000000000, 1445.052233488290085, 126.8032249175980155 ) ) ;
#5459 = DIRECTION ( 'NONE',  ( -1.000000000000000000, 0.000000000000000000, 0.000000000000000000 ) ) ;
#5460 = CARTESIAN_POINT ( 'NONE',  ( 8.558300736974999268, 1511.397837225850026, 204.0148718853070022 ) ) ;
#5461 = CARTESIAN_POINT ( 'NONE',  ( 5.770820141135000192, 1516.591755933730155, 207.4105347035570048 ) ) ;
#5462 = ORIENTED_EDGE ( 'NONE', *, *, #43482, .F. ) ;
#5463 = CARTESIAN_POINT ( 'NONE',  ( -7.544775971906443779, 1425.914422796234476, 205.6924955586506485 ) ) ;
#5464 = CARTESIAN_POINT ( 'NONE',  ( -10.07154961049999820, 1473.228064888090103, 207.4129456781890326 ) ) ;
#5465 = CARTESIAN_POINT ( 'NONE',  ( -23.83497567388974048, 1446.573076643067225, 213.8261868645313655 ) ) ;
#5466 = ORIENTED_EDGE ( 'NONE', *, *, #9215, .T. ) ;
#5468 = AXIS2_PLACEMENT_3D ( 'NONE', #29059, #96820, #20089 ) ;
#5467 = CARTESIAN_POINT ( 'NONE',  ( 18.22805055419890152, 1459.311389626190021, 227.8763770136359881 ) ) ;
#5469 = CARTESIAN_POINT ( 'NONE',  ( -2.860398500404036870, 1367.969949366576884, 210.0987907617960104 ) ) ;
#5470 = CARTESIAN_POINT ( 'NONE',  ( -4.114495368158031852, 1440.063097891708139, 185.4396243348899986 ) ) ;
#5471 = CARTESIAN_POINT ( 'NONE',  ( -2.922186645726760013, 1413.437602691799839, 186.4765809533099912 ) ) ;
#5472 = CARTESIAN_POINT ( 'NONE',  ( 22.33897096189999942, 1410.187224096529917, 206.2328832085579791 ) ) ;
#5473 = CARTESIAN_POINT ( 'NONE',  ( 7.627638999635267147, 1513.425324099864838, 215.5670651928058703 ) ) ;
#5474 = CARTESIAN_POINT ( 'NONE',  ( -14.08481621004247231, 1379.673254536278591, 211.5737053288229106 ) ) ;
#5475 = CARTESIAN_POINT ( 'NONE',  ( 4.163336342339999869E-15, 1416.181292664740113, 209.1218459616989946 ) ) ;
#5476 = CARTESIAN_POINT ( 'NONE',  ( 4.247461698663549612, 1441.373656070180004, 161.5375685151940104 ) ) ;
#5477 = CARTESIAN_POINT ( 'NONE',  ( 4.987078416394999714, 1508.551704408389924, 209.1218459511669892 ) ) ;
#5478 = DIRECTION ( 'NONE',  ( 1.836970198721029688E-16, 1.000000000000000000, 0.000000000000000000 ) ) ;
#5479 = CARTESIAN_POINT ( 'NONE',  ( -7.715625241105000143, 1516.786099423779888, 215.6766101314970001 ) ) ;
#5480 = ORIENTED_EDGE ( 'NONE', *, *, #3607, .F. ) ;
#5481 = CARTESIAN_POINT ( 'NONE',  ( 7.709070221419720426, 1516.535774777470124, 206.6432696383980101 ) ) ;
#5482 = CARTESIAN_POINT ( 'NONE',  ( -7.595213676849999374, 1473.705021973730027, 270.1248737330980134 ) ) ;
#5483 = CARTESIAN_POINT ( 'NONE',  ( 0.3641805758275279969, 1424.317995888269934, 227.5054904079770211 ) ) ;
#5484 = EDGE_CURVE ( 'NONE', #26374, #63089, #67216, .T. ) ;
#5485 = CARTESIAN_POINT ( 'NONE',  ( -6.037828305847510180, 1422.573108036489884, 122.8777291217150065 ) ) ;
#5486 = EDGE_CURVE ( 'NONE', #81391, #100544, #1368, .T. ) ;
#5487 = CARTESIAN_POINT ( 'NONE',  ( 1.029697549479999807, 1474.120255407390005, 219.4685556096990240 ) ) ;
#5488 = CARTESIAN_POINT ( 'NONE',  ( 11.60004869885015211, 1426.082545937270424, 138.9242053348294519 ) ) ;
#5489 = CARTESIAN_POINT ( 'NONE',  ( 2.790610563364870789, 1417.787132752280741, 234.0645936422330919 ) ) ;
#5490 = CARTESIAN_POINT ( 'NONE',  ( -2.500000000000000000, 1432.241594156859946, 157.4925871266979982 ) ) ;
#5491 = ADVANCED_FACE ( 'NONE', ( #33568 ), #41967, .F. ) ;
#5492 = CARTESIAN_POINT ( 'NONE',  ( -106.4840262270000011, 1379.607751643809934, 300.2526974370589983 ) ) ;
#5493 = FACE_OUTER_BOUND ( 'NONE', #7590, .T. ) ;
#5494 = B_SPLINE_SURFACE_WITH_KNOTS ( 'NONE', 5, 5, ( 
 ( #3735, #88267, #86601, #12101, #44063, #2078, #36758, #45737, #35646 ),
 ( #46295, #80422, #18829, #37867, #3188, #11560, #78201, #37316, #27252 ),
 ( #61434, #97205, #53024, #103382, #61990, #54139, #10449, #1514, #44622 ),
 ( #71511, #53585, #105630, #28915, #78763, #104511, #105067, #96106, #19381 ),
 ( #26687, #36208, #27806, #87731, #2631, #11009, #45180, #73122, #5358 ),
 ( #99399, #4797, #22124, #65286, #5917, #107819, #99953, #89907, #38942 ) ),
 .UNSPECIFIED., .F., .F., .F.,
 ( 6, 6 ),
 ( 6, 3, 6 ),
 ( 4.238752792101340816, 5.659133035208659734 ),
 ( 0.000000000000000000, 0.5000000000000000000, 1.002061266618659907 ),
 .UNSPECIFIED. ) ;
#5496 = EDGE_CURVE ( 'NONE', #33774, #83258, #42473, .T. ) ;
#5495 = CARTESIAN_POINT ( 'NONE',  ( 32.33429827083980257, 1440.913060383199991, 244.9699483744109898 ) ) ;
#5497 = CARTESIAN_POINT ( 'NONE',  ( 5.923682464646780943, 1517.151704408390060, 194.3813127491490036 ) ) ;
#5498 = B_SPLINE_CURVE_WITH_KNOTS ( 'NONE', 3,
 ( #43797, #104806, #43255, #44929, #105362, #103128 ),
 .UNSPECIFIED., .F., .F.,
 ( 4, 2, 4 ),
 ( -1.285435071108283616E-05, 0.001079388306740611128, 0.002171630964192305339 ),
 .UNSPECIFIED. ) ;
#5499 = CARTESIAN_POINT ( 'NONE',  ( 13.05081502930000070, 1422.960060114630096, 222.0524190261979811 ) ) ;
#5500 = VERTEX_POINT ( 'NONE', #52062 ) ;
#5501 = ORIENTED_EDGE ( 'NONE', *, *, #56826, .F. ) ;
#5502 = FACE_OUTER_BOUND ( 'NONE', #99984, .T. ) ;
#5503 = CARTESIAN_POINT ( 'NONE',  ( -19.10636532737555626, 1485.521373224806439, 189.6418533252866894 ) ) ;
#5504 = CARTESIAN_POINT ( 'NONE',  ( -0.9810412822912069064, 1409.219255427743292, 186.0188850891012464 ) ) ;
#5505 = CARTESIAN_POINT ( 'NONE',  ( -113.4000000000000057, 1379.913060387289988, 304.2218459572590064 ) ) ;
#5506 = DIRECTION ( 'NONE',  ( -1.755985294532469921E-16, 1.000000000000000000, -1.338183447452831989E-16 ) ) ;
#5507 = AXIS2_PLACEMENT_3D ( 'NONE', #74613, #107651, #66229 ) ;
#5508 = B_SPLINE_CURVE_WITH_KNOTS ( 'NONE', 3,
 ( #93820, #15463, #17097, #110643 ),
 .UNSPECIFIED., .F., .F.,
 ( 4, 4 ),
 ( 0.7259150538130000330, 23.36254398669999688 ),
 .UNSPECIFIED. ) ;
#5509 = CARTESIAN_POINT ( 'NONE',  ( -10.46250751532009993, 1491.356802638789986, 212.5409670664860187 ) ) ;
#5510 = CARTESIAN_POINT ( 'NONE',  ( -1.452443133548009913, 1508.551704408389924, 220.0823312915929932 ) ) ;
#5511 = CARTESIAN_POINT ( 'NONE',  ( -53.52129292230850410, 1383.806223322539836, 268.5146929885909799 ) ) ;
#5512 = CARTESIAN_POINT ( 'NONE',  ( -4.487249019397720140, 1509.038644351750008, 206.6339222935139901 ) ) ;
#5513 = CARTESIAN_POINT ( 'NONE',  ( -13.90890181880000043, 1453.165958253930057, 194.3940701926979955 ) ) ;
#5514 = ADVANCED_FACE ( 'NONE', ( #44212 ), #90706, .T. ) ;
#5515 = CARTESIAN_POINT ( 'NONE',  ( -11.72999038033949937, 1501.913969227260168, 208.8343572913619823 ) ) ;
#5516 = CARTESIAN_POINT ( 'NONE',  ( 2.157288638769999878, 1464.754106553530164, 235.9996813455979918 ) ) ;
#5518 = ORIENTED_EDGE ( 'NONE', *, *, #24049, .F. ) ;
#5517 = LINE ( 'NONE', #28515, #65828 ) ;
#5519 = CARTESIAN_POINT ( 'NONE',  ( -0.3328288701460000443, 1452.976686003830082, 183.2631395458980137 ) ) ;
#5520 = CARTESIAN_POINT ( 'NONE',  ( -25.42483392789999641, 1381.467239109759930, 204.6897922305890063 ) ) ;
#5521 = CARTESIAN_POINT ( 'NONE',  ( -3.790930610359999786, 1476.560235432990112, 199.4766108674189979 ) ) ;
#5523 = ORIENTED_EDGE ( 'NONE', *, *, #44607, .T. ) ;
#5522 = CARTESIAN_POINT ( 'NONE',  ( -10.22078085839999950, 1448.827725591389935, 207.2905425509590032 ) ) ;
#5524 = CARTESIAN_POINT ( 'NONE',  ( -9.771943666833310616, 1448.872252160599828, 190.8346857363359845 ) ) ;
#5525 = ORIENTED_EDGE ( 'NONE', *, *, #219, .F. ) ;
#5526 = EDGE_CURVE ( 'NONE', #51148, #42643, #78925, .T. ) ;
#5527 = AXIS2_PLACEMENT_3D ( 'NONE', #70412, #34010, #44643 ) ;
#5528 = CARTESIAN_POINT ( 'NONE',  ( -8.237282586322759670, 1385.788991056809891, 218.6757492481600025 ) ) ;
#5529 = FACE_OUTER_BOUND ( 'NONE', #43506, .T. ) ;
#5530 = CARTESIAN_POINT ( 'NONE',  ( -9.941476446395858702, 1461.322233705820054, 211.0754656163810239 ) ) ;
#5531 = CARTESIAN_POINT ( 'NONE',  ( -11.60004869884828338, 1426.567386193286893, 135.1569321345708090 ) ) ;
#5532 = CARTESIAN_POINT ( 'NONE',  ( -107.8192228660000040, 1380.324541384940176, 298.6453595191590011 ) ) ;
#5533 = CARTESIAN_POINT ( 'NONE',  ( -15.12493481535974738, 1420.059538282757785, 212.5153262450139096 ) ) ;
#5534 = APPLICATION_CONTEXT ( 'automotive_design' ) ;
#5535 = AXIS2_PLACEMENT_3D ( 'NONE', #104140, #79506, #94628 ) ;
#5536 = CARTESIAN_POINT ( 'NONE',  ( -3.885780586189999829E-16, 1420.943991414029824, 179.3023655596979893 ) ) ;
#5537 = CARTESIAN_POINT ( 'NONE',  ( 2.955851087435179991, 1409.016280981779801, 194.4300961132470036 ) ) ;
#5538 = CARTESIAN_POINT ( 'NONE',  ( 18.03390783410000253, 1424.747035879229998, 225.0015027529979932 ) ) ;
#5539 = FACE_OUTER_BOUND ( 'NONE', #71299, .T. ) ;
#5540 = CARTESIAN_POINT ( 'NONE',  ( -19.64105509870000077, 1485.638507108129943, 190.1260793311979853 ) ) ;
#5541 = CARTESIAN_POINT ( 'NONE',  ( 11.86561512750000169, 1432.302095436430136, 149.9824189746979926 ) ) ;
#5542 = CARTESIAN_POINT ( 'NONE',  ( -4.115857443736018695, 1425.929640604822680, 186.1083528362279651 ) ) ;
#5543 = EDGE_LOOP ( 'NONE', ( #5031, #21279, #102810, #92614 ) ) ;
#5544 = EDGE_LOOP ( 'NONE', ( #6050, #1024, #106130, #95629 ) ) ;
#5545 = CARTESIAN_POINT ( 'NONE',  ( -7.512750272569109988, 1509.038617475950105, 214.6350457578409987 ) ) ;
#5546 = CARTESIAN_POINT ( 'NONE',  ( 19.03157125241660097, 1457.060517503149867, 226.1452829519230079 ) ) ;
#5547 = B_SPLINE_CURVE_WITH_KNOTS ( 'NONE', 3,
 ( #94936, #62479, #26615, #69767, #45113, #87651 ),
 .UNSPECIFIED., .F., .F.,
 ( 4, 2, 4 ),
 ( 0.000000000000000000, 0.5000000000000000000, 1.000000000000000000 ),
 .UNSPECIFIED. ) ;
#5548 = CARTESIAN_POINT ( 'NONE',  ( 18.69816095120750532, 1526.382868172863937, 183.3860352823955679 ) ) ;
#5549 = VECTOR ( 'NONE', #36638, 1000.000000000000114 ) ;
#5550 = DIRECTION ( 'NONE',  ( 0.000000000000000000, 0.000000000000000000, -1.000000000000000000 ) ) ;
#5551 = CARTESIAN_POINT ( 'NONE',  ( -20.32074529087200077, 1498.819556202739932, 190.6518178786860176 ) ) ;
#5552 = EDGE_CURVE ( 'NONE', #6840, #89045, #108619, .T. ) ;
#5553 = DIRECTION ( 'NONE',  ( -0.9417419115949053898, -0.3363363969979660806, -9.559255346349042767E-16 ) ) ;
#5554 = FACE_OUTER_BOUND ( 'NONE', #89313, .T. ) ;
#5555 = CARTESIAN_POINT ( 'NONE',  ( -1.465047864650000031, 1483.408900079630030, 182.5218640156980143 ) ) ;
#5556 = CARTESIAN_POINT ( 'NONE',  ( -7.954225986665955261, 1360.049804075227485, 208.3718459617010978 ) ) ;
#5557 = CARTESIAN_POINT ( 'NONE',  ( -46.16552303099769716, 1440.463954059739990, 266.9715276195660181 ) ) ;
#5558 = CARTESIAN_POINT ( 'NONE',  ( -19.52413277859999852, 1426.414269502929756, 225.5212833970979887 ) ) ;
#5559 = CARTESIAN_POINT ( 'NONE',  ( 13.89554995500000167, 1452.733480491630189, 223.3956528723979886 ) ) ;
#5560 = CARTESIAN_POINT ( 'NONE',  ( 2.477975315464999717, 1516.839862955080207, 207.9852983471170091 ) ) ;
#5561 = CARTESIAN_POINT ( 'NONE',  ( -9.853487827760540441, 1447.709311025530042, 210.2834318627940036 ) ) ;
#5562 = CYLINDRICAL_SURFACE ( 'NONE', #30522, 2.000000000000003109 ) ;
#5563 = CARTESIAN_POINT ( 'NONE',  ( -13.64440718200000013, 1435.322370893529978, 149.8642038458980323 ) ) ;
#5564 = FILL_AREA_STYLE ('',( #31856 ) ) ;
#5565 = CARTESIAN_POINT ( 'NONE',  ( -14.25270368724149961, 1379.587364531829962, 207.9005521859079977 ) ) ;
#5566 = CARTESIAN_POINT ( 'NONE',  ( 7.346206468657319633, 1425.063440261549886, 212.5639244028189978 ) ) ;
#5567 = ORIENTED_EDGE ( 'NONE', *, *, #29783, .F. ) ;
#5568 = CARTESIAN_POINT ( 'NONE',  ( 36.81312681789999885, 1440.913060384859818, 254.5659338001980529 ) ) ;
#5569 = CARTESIAN_POINT ( 'NONE',  ( 4.500000000000000000, 1426.966631815929986, 170.4008037693979816 ) ) ;
#5571 = CARTESIAN_POINT ( 'NONE',  ( -17.63079341550000123, 1410.452321969430159, 194.5845618450980226 ) ) ;
#5570 = CARTESIAN_POINT ( 'NONE',  ( 0.4937778921180000502, 1478.160124056830000, 182.1794214162979983 ) ) ;
#5572 =( BOUNDED_CURVE ( )  B_SPLINE_CURVE ( 3, ( #41935, #7770, #50892, #77746 ),
 .UNSPECIFIED., .F., .T. ) 
 B_SPLINE_CURVE_WITH_KNOTS ( ( 4, 4 ),
 ( 1.036306020146634088, 2.105308394323555099 ),
 .UNSPECIFIED. ) 
 CURVE ( )  GEOMETRIC_REPRESENTATION_ITEM ( )  RATIONAL_B_SPLINE_CURVE ( ( 1.000000000000000000, 0.9070152250226227730, 0.9070152250226227730, 1.000000000000000000 ) ) 
 REPRESENTATION_ITEM ( '' )  );
#5573 = CARTESIAN_POINT ( 'NONE',  ( -27.08076141661259939, 1414.294488336634686, 269.9731936574717110 ) ) ;
#5574 = CARTESIAN_POINT ( 'NONE',  ( -22.49770453780000068, 1429.484910292730092, 225.2498666484979992 ) ) ;
#5575 = CARTESIAN_POINT ( 'NONE',  ( -4.638300726919323935, 1378.093220027633151, 214.4059711397904096 ) ) ;
#5576 = CARTESIAN_POINT ( 'NONE',  ( -0.9757794191400900319, 1452.878985419150013, 152.5158834087430080 ) ) ;
#5577 = CARTESIAN_POINT ( 'NONE',  ( 28.27349493010000003, 1451.471014347730033, 136.1137886329979949 ) ) ;
#5578 = ORIENTED_EDGE ( 'NONE', *, *, #33188, .F. ) ;
#5579 = CARTESIAN_POINT ( 'NONE',  ( -107.8301892023879986, 1378.913060387359792, 300.1602841119429854 ) ) ;
#5580 = CARTESIAN_POINT ( 'NONE',  ( 2.098309414416280126E-05, 1407.650889052649973, 270.1377145618209283 ) ) ;
#5581 = CARTESIAN_POINT ( 'NONE',  ( -0.04885444012580000134, 1508.952077801630139, 238.8419334758980028 ) ) ;
#5582 = CARTESIAN_POINT ( 'NONE',  ( -32.37018134260392799, 1511.187213306747708, 218.0712926453366833 ) ) ;
#5583 = EDGE_LOOP ( 'NONE', ( #76471, #6925, #47180, #75560, #86734, #55615 ) ) ;
#5584 = ORIENTED_EDGE ( 'NONE', *, *, #89323, .T. ) ;
#5585 = CARTESIAN_POINT ( 'NONE',  ( 10.08587585095050088, 1452.694239366880083, 210.2353006364240002 ) ) ;
#5586 = CARTESIAN_POINT ( 'NONE',  ( -24.07954513569999833, 1411.114689535729894, 209.5888749416580197 ) ) ;
#5587 = EDGE_CURVE ( 'NONE', #95653, #19317, #64329, .T. ) ;
#5588 = ORIENTED_EDGE ( 'NONE', *, *, #102639, .F. ) ;
#5589 = CARTESIAN_POINT ( 'NONE',  ( -0.2612701254520000127, 1416.813004075730078, 227.4660694200979947 ) ) ;
#5590 = CARTESIAN_POINT ( 'NONE',  ( -113.4000000000000057, 1391.413060387289988, 304.2218459572590064 ) ) ;
#5591 = ADVANCED_FACE ( 'NONE', ( #97354 ), #73829, .T. ) ;
#5592 = CARTESIAN_POINT ( 'NONE',  ( -21.10399601188239416, 1436.465560437122576, 144.1929280529386972 ) ) ;
#5593 = CARTESIAN_POINT ( 'NONE',  ( 2.487922177595819573, 1508.551704408389924, 213.9544573010300326 ) ) ;
#5594 = ORIENTED_EDGE ( 'NONE', *, *, #22009, .T. ) ;
#5595 = CARTESIAN_POINT ( 'NONE',  ( 44.34415660218949284, 1449.868985015139742, 268.8027473384019572 ) ) ;
#5596 = CARTESIAN_POINT ( 'NONE',  ( -13.15726442530000107, 1416.237488680629895, 221.8313562556980116 ) ) ;
#5597 = CARTESIAN_POINT ( 'NONE',  ( -0.1147355858779999932, 1419.163093610929991, 184.6463452042980009 ) ) ;
#5598 = CARTESIAN_POINT ( 'NONE',  ( 2.866857893004999713, 1516.951766529250108, 205.0784797119270024 ) ) ;
#5599 = CLOSED_SHELL ( 'NONE', ( #96938, #24061, #27007, #21181, #95044, #42222, #31748, #84990, #66105, #15986, #78832, #105611, #9693, #47464, #96441, #57134, #95527, #73378, #69362, #41149, #59645, #20154, #8989, #60806, #56963, #71224, #11391, #50751, #23310, #57672, #99363, #78459, #69555, #48000, #55987, #66999, #61806, #19362, #102319, #70587, #83469, #22197, #76059, #10075, #16727, #19263, #92537, #84237, #101278, #4328, #28941, #65806, #64116, #32565, #58366, #101310, #48745, #27494, #21540, #48765, #2318, #72324, #52788, #93107, #13462, #91394, #72125, #63168, #87992, #41597, #48623, #30912, #13186, #49423, #47605, #30257, #9196, #16734, #20439, #27756, #81449, #110377, #27011, #108348, #63755, #15866, #35213, #36382, #107664, #109982, #87124, #26759, #13816, #5175, #104836, #102164, #76276, #74830, #30311, #52793, #37664, #98830, #102964, #54643, #88843, #84779, #99574, #82543, #2221, #3768, #21272, #66596, #76262, #21664, #19989, #80982, #771, #15078, #88570, #77472, #85641, #58210, #97263, #97920, #32326, #620, #79124, #103589, #66134, #70497, #95510, #74653, #22326, #24667, #80630, #42693, #100116, #12589, #83130, #108285, #28154, #25589, #73272, #42319, #82177 ) ) ;
#5600 = VERTEX_POINT ( 'NONE', #39660 ) ;
#5601 = CARTESIAN_POINT ( 'NONE',  ( 11.06169707739279851, 1480.845630662619897, 213.2313991462129934 ) ) ;
#5602 = CARTESIAN_POINT ( 'NONE',  ( 13.51299049401507091, 1444.004812340696390, 188.0184190261968524 ) ) ;
#5603 = ORIENTED_EDGE ( 'NONE', *, *, #74145, .F. ) ;
#5604 = VERTEX_POINT ( 'NONE', #39085 ) ;
#5605 = CARTESIAN_POINT ( 'NONE',  ( -10.51230281979400161, 1480.112285530560030, 208.7110773518720066 ) ) ;
#5606 = CYLINDRICAL_SURFACE ( 'NONE', #96725, 2.999999999999995115 ) ;
#5607 = CARTESIAN_POINT ( 'NONE',  ( -13.18795888012849993, 1512.495155157840145, 193.8533315336999863 ) ) ;
#5608 = CARTESIAN_POINT ( 'NONE',  ( 4.724549302593670674, 1452.748075490200108, 152.1309929677310038 ) ) ;
#5609 = CARTESIAN_POINT ( 'NONE',  ( -1.651001239120279923E-05, 1410.239988154289904, 269.6149086386799922 ) ) ;
#5610 = CARTESIAN_POINT ( 'NONE',  ( -1.212018553542939969, 1475.694787048319995, 220.4957529374679837 ) ) ;
#5611 = CARTESIAN_POINT ( 'NONE',  ( -109.0700496325590194, 1382.022296823163288, 297.5851204363052602 ) ) ;
#5612 = CARTESIAN_POINT ( 'NONE',  ( 10.99716211064770022, 1478.798203161799847, 205.9204684199630151 ) ) ;
#5613 = CARTESIAN_POINT ( 'NONE',  ( -6.896890933126118993E-05, 1408.913065613199933, 231.7784170915439859 ) ) ;
#5615 = CARTESIAN_POINT ( 'NONE',  ( 17.27619071350000013, 1507.625766668030110, 193.9878102724979954 ) ) ;
#5614 = CARTESIAN_POINT ( 'NONE',  ( 29.79244380917030455, 1525.556090473947052, 196.8434936746641881 ) ) ;
#5616 = CARTESIAN_POINT ( 'NONE',  ( 11.24378212487630080, 1426.078668191249790, 206.4971785593209859 ) ) ;
#5617 = CIRCLE ( 'NONE', #12732, 2.000000000000001776 ) ;
#5618 = CARTESIAN_POINT ( 'NONE',  ( -24.02956139221189957, 1507.932518080230011, 222.3125113693119772 ) ) ;
#5619 = EDGE_CURVE ( 'NONE', #37975, #94335, #103323, .T. ) ;
#5620 = CARTESIAN_POINT ( 'NONE',  ( 4.882003189570000679, 1430.559178934629927, 150.0077195948979920 ) ) ;
#5621 = ORIENTED_EDGE ( 'NONE', *, *, #12480, .F. ) ;
#5622 = FACE_OUTER_BOUND ( 'NONE', #26224, .T. ) ;
#5623 = CARTESIAN_POINT ( 'NONE',  ( -5.614653854145000622, 1512.956339156650074, 214.7364997862470091 ) ) ;
#5624 = CARTESIAN_POINT ( 'NONE',  ( -90.41568981223930734, 1384.968564493010035, 308.8481792632660472 ) ) ;
#5625 = ADVANCED_FACE ( 'NONE', ( #81100 ), #13324, .T. ) ;
#5626 = CARTESIAN_POINT ( 'NONE',  ( -8.184850705000000559, 1385.671368857289963, 199.6841148114490068 ) ) ;
#5627 = CARTESIAN_POINT ( 'NONE',  ( 10.47394328510990036, 1422.444227279350116, 210.3705285485489753 ) ) ;
#5629 = ORIENTED_EDGE ( 'NONE', *, *, #50004, .T. ) ;
#5628 = CARTESIAN_POINT ( 'NONE',  ( 10.94161034597069992, 1423.824721436569689, 203.2068899696880067 ) ) ;
#5630 = EDGE_CURVE ( 'NONE', #22363, #63746, #55100, .T. ) ;
#5631 = CARTESIAN_POINT ( 'NONE',  ( 3.346088552949999961, 1429.638897950889941, 216.8836957388089672 ) ) ;
#5632 = VECTOR ( 'NONE', #96233, 1000.000000000000114 ) ;
#5633 = CARTESIAN_POINT ( 'NONE',  ( 14.45097768893499968, 1514.857962383129916, 224.3693530530669875 ) ) ;
#5634 = DIRECTION ( 'NONE',  ( -0.3679048462383226470, -0.7071067811868645414, -0.6038592750913974738 ) ) ;
#5635 = CARTESIAN_POINT ( 'NONE',  ( -12.78690713350000152, 1416.828040475229955, 195.5394874918979724 ) ) ;
#5636 = CARTESIAN_POINT ( 'NONE',  ( 20.14739811709999984, 1469.497636830730016, 271.1218459616979999 ) ) ;
#5637 = CARTESIAN_POINT ( 'NONE',  ( 0.5697990016583959205, 1450.893162567740092, 181.2939912002310052 ) ) ;
#5638 = VECTOR ( 'NONE', #55237, 1000.000000000000000 ) ;
#5639 = CARTESIAN_POINT ( 'NONE',  ( 6.701030630508360453, 1458.780274625029961, 201.5154958855920029 ) ) ;
#5640 = CARTESIAN_POINT ( 'NONE',  ( -109.6028426828606541, 1386.884535610056219, 297.2361425596885738 ) ) ;
#5641 = CARTESIAN_POINT ( 'NONE',  ( 15.40374502139999890, 1422.106951872629907, 227.8157797934979953 ) ) ;
#5642 = EDGE_CURVE ( 'NONE', #83952, #99467, #48065, .T. ) ;
#5643 = DIRECTION ( 'NONE',  ( 0.000000000000000000, 0.000000000000000000, 1.000000000000000000 ) ) ;
#5644 = CARTESIAN_POINT ( 'NONE',  ( 9.064548041611230289, 1441.200071122209920, 153.7187301893350195 ) ) ;
#5645 = CARTESIAN_POINT ( 'NONE',  ( -17.68297954760000223, 1410.894413715530163, 225.3003200628979812 ) ) ;
#5646 = FACE_OUTER_BOUND ( 'NONE', #74460, .T. ) ;
#5647 = VECTOR ( 'NONE', #2639, 1000.000000000000114 ) ;
#5648 = CARTESIAN_POINT ( 'NONE',  ( -1.544578923920000069, 1422.347071476030123, 228.2660149837979873 ) ) ;
#5649 = ADVANCED_FACE ( 'NONE', ( #90044, #31250 ), #73264, .F. ) ;
#5650 = CARTESIAN_POINT ( 'NONE',  ( 31.03138121380739989, 1441.878430465370002, 137.2367898306910092 ) ) ;
#5651 = CARTESIAN_POINT ( 'NONE',  ( 0.000000000000000000, 1522.051704408389924, 233.8211094035767985 ) ) ;
#5652 = CARTESIAN_POINT ( 'NONE',  ( -1.538891143356439777E-07, 1406.985163805290085, 196.1207725567600164 ) ) ;
#5653 = CARTESIAN_POINT ( 'NONE',  ( -14.61445746615800090, 1417.481753922669895, 203.2535310402599862 ) ) ;
#5654 = FACE_OUTER_BOUND ( 'NONE', #94713, .T. ) ;
#5655 = CARTESIAN_POINT ( 'NONE',  ( -3.954003734500000089, 1416.825421876529845, 227.3234521733980102 ) ) ;
#5656 = DIRECTION ( 'NONE',  ( -0.000000000000000000, -1.000000000000000000, -0.000000000000000000 ) ) ;
#5657 = CARTESIAN_POINT ( 'NONE',  ( -13.35131665876559914, 1408.061408147960037, 210.5533457943919871 ) ) ;
#5658 = CARTESIAN_POINT ( 'NONE',  ( -13.25708502290000013, 1414.913060387329779, 199.5091795105679751 ) ) ;
#5659 = CARTESIAN_POINT ( 'NONE',  ( -0.3534367268244609783, 1484.221040251851036, 198.4322127960935802 ) ) ;
#5660 = CARTESIAN_POINT ( 'NONE',  ( 13.80577029839999881, 1434.979611850010087, 147.2734062573980225 ) ) ;
#5661 = DIRECTION ( 'NONE',  ( -0.2495203814060049652, -0.1962602150479464402, -0.9482729075811118236 ) ) ;
#5662 = CARTESIAN_POINT ( 'NONE',  ( 8.745088717699999847, 1441.583345737160016, 186.1462670829980084 ) ) ;
#5663 = ORIENTED_EDGE ( 'NONE', *, *, #26368, .F. ) ;
#5665 = EDGE_CURVE ( 'NONE', #365, #93138, #21166, .T. ) ;
#5664 = CARTESIAN_POINT ( 'NONE',  ( -16.48227125551525418, 1525.651285554130027, 181.5607879932552464 ) ) ;
#5666 = CARTESIAN_POINT ( 'NONE',  ( 3.160865630554719807, 1370.358795681657284, 206.6712751011299360 ) ) ;
#5667 = CARTESIAN_POINT ( 'NONE',  ( -105.3305948020004763, 1381.132964647196104, 308.7816990702884254 ) ) ;
#5668 = DIRECTION ( 'NONE',  ( -5.980589973904019347E-17, 1.000000000000000000, -1.736889445713099699E-16 ) ) ;
#5669 = EDGE_CURVE ( 'NONE', #86466, #77021, #79780, .T. ) ;
#5670 = CARTESIAN_POINT ( 'NONE',  ( 20.52383114756580085, 1473.184610000140083, 208.7461008354759997 ) ) ;
#5671 = CARTESIAN_POINT ( 'NONE',  ( 15.67984159504549879, 1509.462706413110027, 234.0183160927130075 ) ) ;
#5672 = CARTESIAN_POINT ( 'NONE',  ( 41.65685823593407378, 1426.928113394742468, 269.0850263944785752 ) ) ;
#5673 = CARTESIAN_POINT ( 'NONE',  ( 9.217027833218040200, 1427.824330594879939, 211.8044439908819925 ) ) ;
#5674 = CARTESIAN_POINT ( 'NONE',  ( -14.31906252709999983, 1380.323795378420073, 209.9058135456940022 ) ) ;
#5675 = DIRECTION ( 'NONE',  ( -0.9211327884476214756, -0.3892484888175026247, 0.000000000000000000 ) ) ;
#5676 = CARTESIAN_POINT ( 'NONE',  ( -49.73786273469480790, 1385.018151718609943, 224.8464017876140133 ) ) ;
#5677 = MECHANICAL_DESIGN_GEOMETRIC_PRESENTATION_REPRESENTATION (  '', ( #53993 ), #19966 ) ;
#5678 = CARTESIAN_POINT ( 'NONE',  ( -17.07724394728933248, 1524.330813522192102, 237.1903650275824589 ) ) ;
#5679 = CARTESIAN_POINT ( 'NONE',  ( -3.890622774867280143, 1508.551704408389924, 204.5662182099170252 ) ) ;
#5680 = EDGE_CURVE ( 'NONE', #8387, #93417, #107924, .T. ) ;
#5681 = CARTESIAN_POINT ( 'NONE',  ( -28.91692647416590134, 1509.557647291290095, 208.7049441970110308 ) ) ;
#5682 = CARTESIAN_POINT ( 'NONE',  ( -15.80103170504700039, 1409.464838628420011, 225.2833922138719913 ) ) ;
#5684 = EDGE_LOOP ( 'NONE', ( #12010, #46230, #77091 ) ) ;
#5683 = CARTESIAN_POINT ( 'NONE',  ( 32.28466283162156714, 1512.187213306747481, 219.1752493337713190 ) ) ;
#5685 = CARTESIAN_POINT ( 'NONE',  ( -14.35518634559999818, 1509.483852653929944, 182.9676329983980168 ) ) ;
#5686 = CARTESIAN_POINT ( 'NONE',  ( 10.93373778070590063, 1471.043189543029939, 209.8922278286480037 ) ) ;
#5687 = PLANE ( 'NONE',  #110541 ) ;
#5688 = SURFACE_SIDE_STYLE ('',( #90215 ) ) ;
#5689 = CARTESIAN_POINT ( 'NONE',  ( -11.24049419400000005, 1414.988017874730076, 195.7612516212979870 ) ) ;
#5690 = CARTESIAN_POINT ( 'NONE',  ( 0.2042600169000000077, 1465.101704582730235, 237.0131066117980083 ) ) ;
#5691 = CARTESIAN_POINT ( 'NONE',  ( 22.49646906260000279, 1410.193735020430040, 214.3055066545979912 ) ) ;
#5692 = CARTESIAN_POINT ( 'NONE',  ( -2.667363771992699473, 1417.233457082500081, 186.2697805505230235 ) ) ;
#5693 = CARTESIAN_POINT ( 'NONE',  ( -20.36852751908510228, 1464.956532905599943, 210.9458057460080056 ) ) ;
#5694 = CARTESIAN_POINT ( 'NONE',  ( -16.36294508339999965, 1422.940422817830040, 227.7580329737979810 ) ) ;
#5695 = CARTESIAN_POINT ( 'NONE',  ( 10.52384291159865626, 1498.970202591990983, 202.0357653132980431 ) ) ;
#5696 = CARTESIAN_POINT ( 'NONE',  ( 26.50595462180590189, 1469.329495983640072, 208.3089406750970056 ) ) ;
#5697 = CARTESIAN_POINT ( 'NONE',  ( -113.4000000000000057, 1340.114449826970031, 286.9633900369479989 ) ) ;
#5698 = CARTESIAN_POINT ( 'NONE',  ( 22.68380688229993680, 1509.726051394556407, 190.0734992207788991 ) ) ;
#5699 = CARTESIAN_POINT ( 'NONE',  ( -23.65270513040000111, 1430.813106381330044, 211.2966596496080172 ) ) ;
#5700 = CARTESIAN_POINT ( 'NONE',  ( 8.251048879700000782, 1367.474174444410210, 210.6218459616991936 ) ) ;
#5701 = VECTOR ( 'NONE', #54056, 1000.000000000000000 ) ;
#5702 = CARTESIAN_POINT ( 'NONE',  ( -2.879642191334999879, 1516.812046502680005, 205.6755161564470313 ) ) ;
#5703 = CYLINDRICAL_SURFACE ( 'NONE', #55438, 2.000000000000003997 ) ;
#5704 = CARTESIAN_POINT ( 'NONE',  ( 0.8265244082521410185, 1408.941923255679967, 231.1644249228330068 ) ) ;
#5705 = CARTESIAN_POINT ( 'NONE',  ( -4.228853213262760313, 1441.542194655879939, 165.2229178842150077 ) ) ;
#5707 = VERTEX_POINT ( 'NONE', #6604 ) ;
#5706 = CARTESIAN_POINT ( 'NONE',  ( -68.62400269330709079, 1379.747572044880144, 280.2354522863200259 ) ) ;
#5708 = ORIENTED_EDGE ( 'NONE', *, *, #60246, .F. ) ;
#5709 = ADVANCED_FACE ( 'NONE', ( #57583 ), #67562, .T. ) ;
#5710 = CARTESIAN_POINT ( 'NONE',  ( -8.799867317537470868, 1381.167308713387229, 217.8608335803399143 ) ) ;
#5711 = ORIENTED_EDGE ( 'NONE', *, *, #24212, .T. ) ;
#5712 = CARTESIAN_POINT ( 'NONE',  ( 18.31941652029302858, 1519.551704408389924, 203.8280657238408651 ) ) ;
#5713 = CARTESIAN_POINT ( 'NONE',  ( 11.27432879130000032, 1501.460240645189742, 207.0864724315690069 ) ) ;
#5715 = CARTESIAN_POINT ( 'NONE',  ( 15.94138077806149845, 1410.571769083230038, 191.5578847893440013 ) ) ;
#5714 = CARTESIAN_POINT ( 'NONE',  ( -10.37251529557829954, 1441.250888918300006, 153.2543604180100090 ) ) ;
#5716 = CARTESIAN_POINT ( 'NONE',  ( 7.339749335215000059, 1517.224900789629828, 210.8312305431869902 ) ) ;
#5717 = EDGE_CURVE ( 'NONE', #63851, #10428, #85098, .T. ) ;
#5718 = CIRCLE ( 'NONE', #61218, 2.000000000000003553 ) ;
#5719 = CARTESIAN_POINT ( 'NONE',  ( -106.5054120343349808, 1378.913060387289988, 306.4287628433619943 ) ) ;
#5720 = CARTESIAN_POINT ( 'NONE',  ( 10.81507089421240053, 1424.921187596799882, 144.1620444706739761 ) ) ;
#5721 = DIRECTION ( 'NONE',  ( 0.000000000000000000, 0.000000000000000000, 1.000000000000000000 ) ) ;
#5722 = CARTESIAN_POINT ( 'NONE',  ( 37.66742087362709412, 1450.649596001800091, 134.0999999985879754 ) ) ;
#5723 =( BOUNDED_CURVE ( )  B_SPLINE_CURVE ( 3, ( #68525, #85853, #223, #61250 ),
 .UNSPECIFIED., .F., .T. ) 
 B_SPLINE_CURVE_WITH_KNOTS ( ( 4, 4 ),
 ( 4.177675889938866405, 5.247004472095339267 ),
 .UNSPECIFIED. ) 
 CURVE ( )  GEOMETRIC_REPRESENTATION_ITEM ( )  RATIONAL_B_SPLINE_CURVE ( ( 1.000000000000000000, 0.9069598259872098112, 0.9069598259872098112, 1.000000000000000000 ) ) 
 REPRESENTATION_ITEM ( '' )  );
#5724 = DIRECTION ( 'NONE',  ( 0.03489949670246857150, 0.9993908270190969834, 0.000000000000000000 ) ) ;
#5725 = ORIENTED_EDGE ( 'NONE', *, *, #76427, .F. ) ;
#5726 = CARTESIAN_POINT ( 'NONE',  ( -18.92738905869999755, 1503.346139545890082, 222.1981867166989844 ) ) ;
#5727 = CARTESIAN_POINT ( 'NONE',  ( -18.37766962349999744, 1457.945728469830101, 227.9374886095980060 ) ) ;
#5728 = VERTEX_POINT ( 'NONE', #22826 ) ;
#5729 = ORIENTED_EDGE ( 'NONE', *, *, #107778, .F. ) ;
#5730 = CARTESIAN_POINT ( 'NONE',  ( -5.986375141904999531, 1514.050458741980037, 216.7582919984769774 ) ) ;
#5731 = CARTESIAN_POINT ( 'NONE',  ( -3.218260648026030069, 1432.346989537609943, 155.4230417355269935 ) ) ;
#5732 = EDGE_CURVE ( 'NONE', #4376, #7383, #3637, .T. ) ;
#5733 = CARTESIAN_POINT ( 'NONE',  ( 2.775567936913962086, 1367.641464887947222, 209.1220808601200076 ) ) ;
#5734 = CARTESIAN_POINT ( 'NONE',  ( -21.12854636069999970, 1507.715431485890122, 209.4790061967080135 ) ) ;
#5735 = CARTESIAN_POINT ( 'NONE',  ( -2.500000000000000000, 1439.621710174999862, 168.1588803299280244 ) ) ;
#5736 = AXIS2_PLACEMENT_3D ( 'NONE', #42697, #18022, #34285 ) ;
#5737 = CARTESIAN_POINT ( 'NONE',  ( -2.470168522031893854, 1523.481610118013577, 242.8787258960506961 ) ) ;
#5738 = CARTESIAN_POINT ( 'NONE',  ( 36.37832868398670172, 1435.767865609760065, 135.3769914889309973 ) ) ;
#5739 = CARTESIAN_POINT ( 'NONE',  ( -0.02154542468749880146, 1464.515732093790120, 199.1359198071390040 ) ) ;
#5740 = CARTESIAN_POINT ( 'NONE',  ( 30.04019103850634664, 1524.756004293092019, 222.3084691776629711 ) ) ;
#5741 = CARTESIAN_POINT ( 'NONE',  ( 9.959064829120000795, 1415.087818611729972, 195.3775652628979742 ) ) ;
#5742 = CARTESIAN_POINT ( 'NONE',  ( -78.64846761883408988, 1384.787391290499954, 281.2434142473900351 ) ) ;
#5743 = ORIENTED_EDGE ( 'NONE', *, *, #42395, .F. ) ;
#5744 = CARTESIAN_POINT ( 'NONE',  ( 7.716878902974999122, 1516.833976295079992, 201.7919207096969672 ) ) ;
#5745 = CARTESIAN_POINT ( 'NONE',  ( 0.7402208603880020554, 1516.992029636990083, 208.3685455796920110 ) ) ;
#5746 = ORIENTED_EDGE ( 'NONE', *, *, #79495, .T. ) ;
#5747 = CARTESIAN_POINT ( 'NONE',  ( 34.44779686536719510, 1440.913060387330006, 260.0104300309679957 ) ) ;
#5748 = EDGE_CURVE ( 'NONE', #95283, #62471, #72986, .T. ) ;
#5749 = CARTESIAN_POINT ( 'NONE',  ( -0.002357574298573597137, 1451.791738093121467, 154.0465204539138142 ) ) ;
#5750 = VERTEX_POINT ( 'NONE', #67088 ) ;
#5751 = CARTESIAN_POINT ( 'NONE',  ( -15.06280282045160135, 1422.388303761650150, 229.4662100962750060 ) ) ;
#5752 = CARTESIAN_POINT ( 'NONE',  ( 8.413641089779510196, 1428.393608785230072, 213.4913874550600212 ) ) ;
#5753 = PLANE ( 'NONE',  #77812 ) ;
#5754 = CARTESIAN_POINT ( 'NONE',  ( -1.491506560153236904, 1511.187213306747708, 242.6732489767341576 ) ) ;
#5755 = CARTESIAN_POINT ( 'NONE',  ( -12.61812115819999924, 1416.825245919430245, 222.0544627597980138 ) ) ;
#5756 = ADVANCED_FACE ( 'NONE', ( #110165 ), #110817, .T. ) ;
#5757 = CARTESIAN_POINT ( 'NONE',  ( -20.61690376153225301, 1509.299818264167243, 229.2235484916167820 ) ) ;
#5758 = CARTESIAN_POINT ( 'NONE',  ( 0.5565654927739999147, 1405.991402147929875, 266.9610393333979914 ) ) ;
#5759 = CARTESIAN_POINT ( 'NONE',  ( -5.912224502460420084, 1510.631883423287263, 201.5996445015462371 ) ) ;
#5760 = CARTESIAN_POINT ( 'NONE',  ( -21.61975802671013369, 1524.130440953581001, 183.7557183496595599 ) ) ;
#5762 = CARTESIAN_POINT ( 'NONE',  ( -24.20882859423510070, 1435.739118765830199, 210.8967395777180229 ) ) ;
#5761 = CARTESIAN_POINT ( 'NONE',  ( 14.93370170679999909, 1461.288361491829846, 230.0893540134979958 ) ) ;
#5763 = CARTESIAN_POINT ( 'NONE',  ( 2.472529913803022783, 1523.678648413191695, 175.3762130535718597 ) ) ;
#5764 = CARTESIAN_POINT ( 'NONE',  ( 2.291676273424999799, 1516.534976163889951, 216.4430396779769978 ) ) ;
#5765 = VERTEX_POINT ( 'NONE', #28239 ) ;
#5766 = CARTESIAN_POINT ( 'NONE',  ( -0.5533431911963668792, 1486.379993417803689, 181.7748704520617480 ) ) ;
#5767 = CARTESIAN_POINT ( 'NONE',  ( -0.08976027792670869532, 1508.421112912959870, 180.3398118522160019 ) ) ;
#5768 = CARTESIAN_POINT ( 'NONE',  ( 18.25525582808161218, 1446.597240889685281, 216.0033427005020030 ) ) ;
#5769 = CARTESIAN_POINT ( 'NONE',  ( 1.135185044044999980, 1516.778853242349896, 212.5689744308569971 ) ) ;
#5770 = CARTESIAN_POINT ( 'NONE',  ( 18.55970574510000048, 1508.848287786029914, 188.2531264885979851 ) ) ;
#5771 = CARTESIAN_POINT ( 'NONE',  ( -17.19739463999606599, 1525.960063244516959, 236.2603809477411971 ) ) ;
#5773 = ORIENTED_EDGE ( 'NONE', *, *, #71836, .F. ) ;
#5772 = CARTESIAN_POINT ( 'NONE',  ( -106.4193210029999932, 1386.474088513239849, 311.3161121332589687 ) ) ;
#5774 = B_SPLINE_CURVE_WITH_KNOTS ( 'NONE', 3,
 ( #44237, #19561, #86775, #52088, #2257, #78950, #20116, #104127, #45898, #27973, #103571, #62157, #52638, #28528, #54308, #10064, #78381 ),
 .UNSPECIFIED., .F., .F.,
 ( 4, 2, 2, 1, 1, 1, 1, 1, 2, 2, 4 ),
 ( 0.000000000000000000, 0.2500000000000363598, 0.5000000000000727196, 0.6250000000000900391, 0.6875000000000995870, 0.7187500000001053602, 0.7343750000001072475, 0.7421875000001063594, 0.7460937500001042499, 0.7500000000001021405, 1.000000000000000000 ),
 .UNSPECIFIED. ) ;
#5775 = CARTESIAN_POINT ( 'NONE',  ( -8.371350849009999706, 1384.898375639480037, 199.7750114592789998 ) ) ;
#5776 = DIRECTION ( 'NONE',  ( 0.000000000000000000, 0.000000000000000000, 1.000000000000000000 ) ) ;
#5777 = EDGE_CURVE ( 'NONE', #86539, #59011, #70285, .T. ) ;
#5778 = CARTESIAN_POINT ( 'NONE',  ( -11.85676285999999990, 1431.648968933459855, 150.3599054133979962 ) ) ;
#5779 = CARTESIAN_POINT ( 'NONE',  ( -15.85591190879999779, 1415.880081504350073, 209.4912631162540038 ) ) ;
#5780 = CARTESIAN_POINT ( 'NONE',  ( -65.55053502199999116, 1379.787846393009886, 274.7583384239589464 ) ) ;
#5781 = CARTESIAN_POINT ( 'NONE',  ( 9.400735431060539327, 1432.346466415740224, 153.1462980661239897 ) ) ;
#5782 = ADVANCED_FACE ( 'NONE', ( #2519 ), #11991, .T. ) ;
#5783 = CARTESIAN_POINT ( 'NONE',  ( 17.19739463999641416, 1525.960063244516959, 181.9833109756548879 ) ) ;
#5784 = CARTESIAN_POINT ( 'NONE',  ( -12.22894430393720100, 1440.615615687460149, 224.1155035949470005 ) ) ;
#5785 = ADVANCED_FACE ( 'NONE', ( #19260 ), #69405, .T. ) ;
#5787 = CARTESIAN_POINT ( 'NONE',  ( -9.459818323764448422, 1424.144492356367664, 137.0999999969407099 ) ) ;
#5786 = CARTESIAN_POINT ( 'NONE',  ( -23.17373061810000223, 1444.794561936630089, 216.5813394841780166 ) ) ;
#5788 = CARTESIAN_POINT ( 'NONE',  ( 20.79738390328718367, 1512.187213306747481, 181.2030061003470394 ) ) ;
#5789 = VERTEX_POINT ( 'NONE', #97104 ) ;
#5790 = CARTESIAN_POINT ( 'NONE',  ( -6.948321743994999800, 1517.049325831759916, 205.0875650164470017 ) ) ;
#5791 = CARTESIAN_POINT ( 'NONE',  ( 9.883432818870000247, 1406.823613192530047, 269.0083561828979555 ) ) ;
#5792 = DIRECTION ( 'NONE',  ( 0.000000000000000000, 1.000000000000000000, 0.000000000000000000 ) ) ;
#5793 = CARTESIAN_POINT ( 'NONE',  ( 19.26869546180000015, 1410.873740538630045, 195.8008840898980054 ) ) ;
#5794 = ADVANCED_FACE ( 'NONE', ( #95992 ), #12143, .F. ) ;
#5795 = CARTESIAN_POINT ( 'NONE',  ( 24.00668311305575742, 1435.609311454352110, 213.8188581933794410 ) ) ;
#5796 = CARTESIAN_POINT ( 'NONE',  ( -24.10313149040000269, 1452.071361778829896, 136.4709151672980170 ) ) ;
#5797 = DIRECTION ( 'NONE',  ( -0.000000000000000000, -0.000000000000000000, 1.000000000000000000 ) ) ;
#5798 = CARTESIAN_POINT ( 'NONE',  ( -6.997399759229028682, 1439.698082657984287, 203.8640865756502194 ) ) ;
#5799 = CARTESIAN_POINT ( 'NONE',  ( -2.437740576677990489, 1449.518193424200035, 155.3362125304199992 ) ) ;
#5800 = CARTESIAN_POINT ( 'NONE',  ( -12.72147812920000121, 1445.025642375379903, 185.9027152744980071 ) ) ;
#5801 = CARTESIAN_POINT ( 'NONE',  ( -19.75663087343670909, 1485.988119119562953, 190.2206659241704756 ) ) ;
#5802 = CARTESIAN_POINT ( 'NONE',  ( -14.34456629294319896, 1416.134159100620082, 221.2755357109419947 ) ) ;
#5803 = CARTESIAN_POINT ( 'NONE',  ( -12.03392632030000087, 1501.178862756489934, 213.6370645969589930 ) ) ;
#5804 = CARTESIAN_POINT ( 'NONE',  ( -7.707668447030600056, 1409.182218100520004, 196.2912339717319981 ) ) ;
#5805 = EDGE_CURVE ( 'NONE', #83932, #72812, #42512, .T. ) ;
#5806 = FACE_OUTER_BOUND ( 'NONE', #14080, .T. ) ;
#5807 = CARTESIAN_POINT ( 'NONE',  ( 2.499999998570000326, 1439.824558940259976, 159.3162087218979934 ) ) ;
#5808 = CARTESIAN_POINT ( 'NONE',  ( -6.106286103040000413, 1474.752488639329840, 269.6381986971979927 ) ) ;
#5809 = CARTESIAN_POINT ( 'NONE',  ( -4.244916217095670241, 1446.427620833529772, 161.9653756394929758 ) ) ;
#5810 = CARTESIAN_POINT ( 'NONE',  ( -108.6616353267809956, 1383.758284946439971, 311.0749865448200353 ) ) ;
#5811 = EDGE_CURVE ( 'NONE', #86293, #63851, #29000, .T. ) ;
#5812 = DIRECTION ( 'NONE',  ( 1.755985294532469921E-16, -1.000000000000000000, 1.338183447452831989E-16 ) ) ;
#5813 = CARTESIAN_POINT ( 'NONE',  ( -56.61892686578349299, 1384.709670891599899, 274.9079990654900030 ) ) ;
#5814 = CARTESIAN_POINT ( 'NONE',  ( -30.01999388067554619, 1525.848198008145346, 221.1300202120172003 ) ) ;
#5815 = AXIS2_PLACEMENT_3D ( 'NONE', #89895, #106692, #108911 ) ;
#5816 = CARTESIAN_POINT ( 'NONE',  ( 16.93613030662569940, 1507.562497965019929, 193.6637058848310176 ) ) ;
#5817 = CARTESIAN_POINT ( 'NONE',  ( -106.0599097820000054, 1379.082397735959830, 301.3386546664589787 ) ) ;
#5818 = CARTESIAN_POINT ( 'NONE',  ( 7.508706873624496403, 1508.884207225577484, 203.6084103738515978 ) ) ;
#5819 = CARTESIAN_POINT ( 'NONE',  ( -18.44228220140000118, 1409.721884562830155, 196.7777138713979923 ) ) ;
#5820 = CARTESIAN_POINT ( 'NONE',  ( -15.49718189712599958, 1421.634728641663969, 227.2930083201289904 ) ) ;
#5821 = CARTESIAN_POINT ( 'NONE',  ( -37.09487445649999415, 1421.897761927629972, 269.8322594516980075 ) ) ;
#5822 = ORIENTED_EDGE ( 'NONE', *, *, #86219, .T. ) ;
#5823 = CARTESIAN_POINT ( 'NONE',  ( -2.336386348569962745, 1410.372884070141026, 232.7140726396572745 ) ) ;
#5824 = CARTESIAN_POINT ( 'NONE',  ( -13.58963604942879932, 1508.337642800850062, 209.7220322380239850 ) ) ;
#5825 = CARTESIAN_POINT ( 'NONE',  ( -16.83568192233699889, 1418.884533542789995, 201.2565368160369985 ) ) ;
#5827 = CARTESIAN_POINT ( 'NONE',  ( -12.88197598446049952, 1379.383856360359914, 211.4143069029759943 ) ) ;
#5826 = CARTESIAN_POINT ( 'NONE',  ( -16.42987258731520228, 1416.947447175220077, 208.7386071577110158 ) ) ;
#5828 = DIRECTION ( 'NONE',  ( 0.000000000000000000, -1.000000000000000000, 1.836970198721029688E-16 ) ) ;
#5829 = CARTESIAN_POINT ( 'NONE',  ( 7.768471907389999487, 1409.184341404130009, 189.0606530832980070 ) ) ;
#5830 = FACE_OUTER_BOUND ( 'NONE', #11616, .T. ) ;
#5831 = CARTESIAN_POINT ( 'NONE',  ( 1.125509850285000280, 1517.203017563489766, 201.7827387294869936 ) ) ;
#5832 = CARTESIAN_POINT ( 'NONE',  ( 7.788969440409999834, 1427.187801883110069, 212.3321831630789802 ) ) ;
#5833 = B_SPLINE_CURVE_WITH_KNOTS ( 'NONE', 3,
 ( #104519, #78771, #4277, #2086, #105638, #28923, #96115, #96681, #18836, #29454, #45187, #53032, #89373, #46844, #80429, #70959 ),
 .UNSPECIFIED., .F., .F.,
 ( 4, 3, 3, 3, 3, 4 ),
 ( -19.57721055789999909, -18.83699752252369919, -17.50138789245909976, -16.16248386776419821, -14.82273906699520083, -13.48402717865840117 ),
 .UNSPECIFIED. ) ;
#5834 = CARTESIAN_POINT ( 'NONE',  ( -12.61716434588512037, 1398.287096944733094, 212.2535635707003507 ) ) ;
#5835 = CARTESIAN_POINT ( 'NONE',  ( 15.19327421213499996, 1512.300546902530186, 196.2658363013669884 ) ) ;
#5836 = FACE_BOUND ( 'NONE', #97963, .T. ) ;
#5837 = CARTESIAN_POINT ( 'NONE',  ( -11.18060534273650042, 1378.990352783300068, 211.8621521335040256 ) ) ;
#5838 = CARTESIAN_POINT ( 'NONE',  ( 20.04660124756710005, 1509.276552014090157, 229.7844253363949747 ) ) ;
#5840 = ORIENTED_EDGE ( 'NONE', *, *, #18175, .T. ) ;
#5839 = CARTESIAN_POINT ( 'NONE',  ( 9.296940999030001151, 1453.078838425589993, 212.1081469227889897 ) ) ;
#5841 = ORIENTED_EDGE ( 'NONE', *, *, #83719, .T. ) ;
#5842 = CARTESIAN_POINT ( 'NONE',  ( 0.01233345008840000014, 1396.097901039130193, 221.0480490693979903 ) ) ;
#5843 = CARTESIAN_POINT ( 'NONE',  ( -19.17428229720000132, 1409.582641083130056, 220.3285384914979943 ) ) ;
#5844 = ORIENTED_EDGE ( 'NONE', *, *, #34494, .T. ) ;
#5845 = CARTESIAN_POINT ( 'NONE',  ( -13.51602633418888821, 1443.948650972781479, 169.3503399069581121 ) ) ;
#5846 = CARTESIAN_POINT ( 'NONE',  ( 21.56377605174612100, 1509.708111594535012, 229.5989167562945852 ) ) ;
#5847 = CARTESIAN_POINT ( 'NONE',  ( -7.618904794935000169, 1511.873873588870083, 211.7469127400270281 ) ) ;
#5849 = CARTESIAN_POINT ( 'NONE',  ( 17.17836974400000116, 1416.259463228930144, 226.4421905685979937 ) ) ;
#5848 = FACE_OUTER_BOUND ( 'NONE', #28299, .T. ) ;
#5850 = CARTESIAN_POINT ( 'NONE',  ( 1.034090463059999854, 1410.308950726829835, 185.1959119782980281 ) ) ;
#5851 = CARTESIAN_POINT ( 'NONE',  ( -3.676358388133539989, 1464.513658476559840, 199.1740838259549946 ) ) ;
#5852 = CARTESIAN_POINT ( 'NONE',  ( 3.839962655360000365, 1424.367742364450123, 191.5388040513990120 ) ) ;
#5853 = CARTESIAN_POINT ( 'NONE',  ( 10.69511309515409891, 1396.286541966780078, 206.2627936616379998 ) ) ;
#5854 = CARTESIAN_POINT ( 'NONE',  ( 14.39446395561900083, 1416.321686235030029, 196.9169130221449961 ) ) ;
#5855 = CARTESIAN_POINT ( 'NONE',  ( 11.52956870459999905, 1428.865126643429903, 150.2645387300980246 ) ) ;
#5856 = CARTESIAN_POINT ( 'NONE',  ( 16.90742456150000095, 1442.831169986189934, 162.4348202098979925 ) ) ;
#5857 = ORIENTED_EDGE ( 'NONE', *, *, #43955, .T. ) ;
#5858 = CARTESIAN_POINT ( 'NONE',  ( 13.11860189580039915, 1435.347307412770078, 150.3412794832900090 ) ) ;
#5859 = CARTESIAN_POINT ( 'NONE',  ( 1.930489070153026399, 1450.295778691457372, 181.9128711244939325 ) ) ;
#5860 = ORIENTED_EDGE ( 'NONE', *, *, #36766, .F. ) ;
#5861 = VERTEX_POINT ( 'NONE', #25590 ) ;
#5862 = CARTESIAN_POINT ( 'NONE',  ( -9.975542809210001138, 1421.165924026620132, 193.6282031886989898 ) ) ;
#5863 = CARTESIAN_POINT ( 'NONE',  ( 4.501691961449999724, 1368.956319095359959, 207.6218459616989946 ) ) ;
#5864 = CARTESIAN_POINT ( 'NONE',  ( -108.4554037492093812, 1388.504189957043081, 310.3907579481389121 ) ) ;
#5865 = CARTESIAN_POINT ( 'NONE',  ( -6.553524415734999664, 1516.882690742909972, 216.0660777183969969 ) ) ;
#5866 = CARTESIAN_POINT ( 'NONE',  ( -13.86945421516830024, 1379.876352634179966, 208.3687925243430072 ) ) ;
#5867 = ORIENTED_EDGE ( 'NONE', *, *, #25998, .F. ) ;
#5868 = CARTESIAN_POINT ( 'NONE',  ( -12.03574695270000028, 1503.040364855890175, 208.3824768740459774 ) ) ;
#5869 = CARTESIAN_POINT ( 'NONE',  ( 2.500000000000000000, 1448.626811758040049, 158.8049822478760120 ) ) ;
#5870 = CARTESIAN_POINT ( 'NONE',  ( -55.15130194409999831, 1374.936376805820146, 253.2598301361589961 ) ) ;
#5871 = CARTESIAN_POINT ( 'NONE',  ( 7.710610402995000001, 1516.594591938570147, 205.6677260153969939 ) ) ;
#5872 = ORIENTED_EDGE ( 'NONE', *, *, #100359, .T. ) ;
#5873 = CARTESIAN_POINT ( 'NONE',  ( -3.255809902135000211, 1516.837969789639828, 209.8792719553279937 ) ) ;
#5874 = CARTESIAN_POINT ( 'NONE',  ( -20.38220705570000035, 1509.051558519629907, 229.2949352805979970 ) ) ;
#5875 = CARTESIAN_POINT ( 'NONE',  ( -32.57952228147021145, 1421.659236551914319, 269.5001856740272501 ) ) ;
#5876 = CARTESIAN_POINT ( 'NONE',  ( -0.8957367667660000032, 1409.883006492629875, 233.0638040154979933 ) ) ;
#5878 = ORIENTED_EDGE ( 'NONE', *, *, #107533, .F. ) ;
#5877 = CARTESIAN_POINT ( 'NONE',  ( -0.1496009369319929727, 1415.938742849230039, 227.0988434848029840 ) ) ;
#5879 = FACE_OUTER_BOUND ( 'NONE', #7172, .T. ) ;
#5880 = CARTESIAN_POINT ( 'NONE',  ( -27.91175324445159944, 1440.913060390089868, 230.7978836448200184 ) ) ;
#5881 = CARTESIAN_POINT ( 'NONE',  ( -62.08642864540000517, 1384.386629093810143, 284.7566818690589798 ) ) ;
#5882 = CARTESIAN_POINT ( 'NONE',  ( -0.3530909465895950006, 1467.116854953090069, 235.6078142961000026 ) ) ;
#5883 = CARTESIAN_POINT ( 'NONE',  ( 10.97762738470000166, 1408.611869070129842, 270.1116084948980074 ) ) ;
#5884 = CARTESIAN_POINT ( 'NONE',  ( -5.774609660074999873, 1516.777260590120022, 213.7418541773069762 ) ) ;
#5885 = CARTESIAN_POINT ( 'NONE',  ( 23.31696727199999941, 1409.831874797830096, 209.1795042131419962 ) ) ;
#5886 = CARTESIAN_POINT ( 'NONE',  ( 28.72841836131054194, 1526.333389947990099, 198.1146668274930107 ) ) ;
#5887 = CARTESIAN_POINT ( 'NONE',  ( 4.637787270109999582, 1462.124489585889933, 228.1829287868989979 ) ) ;
#5888 = CARTESIAN_POINT ( 'NONE',  ( -7.714725160980429486, 1516.751726750540229, 209.7571990288649886 ) ) ;
#5889 = CARTESIAN_POINT ( 'NONE',  ( 4.626591867355000609, 1517.096587378560116, 210.8266407735670214 ) ) ;
#5890 = CARTESIAN_POINT ( 'NONE',  ( -22.04555908422410582, 1524.082740465118377, 233.7638702259614263 ) ) ;
#5891 = CARTESIAN_POINT ( 'NONE',  ( 15.10371975099999986, 1409.440493903229935, 192.9533947891980006 ) ) ;
#5892 = CARTESIAN_POINT ( 'NONE',  ( -15.36992167882205429, 1486.076716614789348, 186.5633141537735753 ) ) ;
#5894 = EDGE_LOOP ( 'NONE', ( #57752, #110494, #17510, #35887 ) ) ;
#5893 = CARTESIAN_POINT ( 'NONE',  ( -49.90786910739999627, 1388.283118323920007, 226.7687942016589773 ) ) ;
#5895 = CARTESIAN_POINT ( 'NONE',  ( -52.00221346620590168, 1385.110007062809927, 265.8307340536850347 ) ) ;
#5896 = EDGE_CURVE ( 'NONE', #9209, #75410, #40698, .T. ) ;
#5897 = CARTESIAN_POINT ( 'NONE',  ( 17.52111108772825432, 1410.887420319047806, 225.4767960855723743 ) ) ;
#5898 = EDGE_CURVE ( 'NONE', #25016, #9292, #4941, .T. ) ;
#5899 = CARTESIAN_POINT ( 'NONE',  ( -10.80134480061119895, 1446.564900598669965, 153.0805715986579969 ) ) ;
#5900 = CARTESIAN_POINT ( 'NONE',  ( 18.80339027203730140, 1425.953307585449693, 225.0197318394450008 ) ) ;
#5901 = CARTESIAN_POINT ( 'NONE',  ( -7.121584071090000023, 1409.161751583130126, 195.9581075130980139 ) ) ;
#5902 = CARTESIAN_POINT ( 'NONE',  ( 12.25880158789999896, 1421.301048178839892, 203.8561358684090123 ) ) ;
#5903 = CARTESIAN_POINT ( 'NONE',  ( 1.968601690575629615, 1498.935401749600032, 197.9561509338619771 ) ) ;
#5905 = DIRECTION ( 'NONE',  ( 0.8672669759446630655, 0.000000000000000000, -0.4978433412588735285 ) ) ;
#5904 = CARTESIAN_POINT ( 'NONE',  ( 6.555393117025000826, 1516.809497469189864, 216.4498952504870033 ) ) ;
#5906 = CARTESIAN_POINT ( 'NONE',  ( -3.665756888920000289, 1508.551704408389924, 204.1347675262390169 ) ) ;
#5907 = CARTESIAN_POINT ( 'NONE',  ( 10.16550028177676168, 1422.464185489443253, 137.0999999980980988 ) ) ;
#5908 = EDGE_LOOP ( 'NONE', ( #82449, #56903, #10950, #27179 ) ) ;
#5909 = CARTESIAN_POINT ( 'NONE',  ( 4.615644804385000022, 1517.009964551830080, 202.1744681489270192 ) ) ;
#5910 = CARTESIAN_POINT ( 'NONE',  ( -13.58256619105009477, 1416.843574567863016, 221.9093686888480192 ) ) ;
#5911 = ORIENTED_EDGE ( 'NONE', *, *, #92691, .F. ) ;
#5912 = CARTESIAN_POINT ( 'NONE',  ( 0.08876556219990000551, 1487.215267144130166, 230.3027642732979814 ) ) ;
#5913 = ADVANCED_FACE ( 'NONE', ( #1960 ), #93816, .T. ) ;
#5914 = B_SPLINE_CURVE_WITH_KNOTS ( 'NONE', 5,
 ( #57432, #99384, #84251, #41702, #109469, #14833, #91558, #74228, #110012, #49022, #108358, #101037, #92647, #22660, #58518, #56862, #14282, #82610 ),
 .UNSPECIFIED., .F., .F.,
 ( 6, 3, 3, 3, 3, 6 ),
 ( 14.02535798500000119, 16.90079360149999843, 18.14364336469999728, 21.12354018079999918, 24.53920724549999832, 25.26141249534510180 ),
 .UNSPECIFIED. ) ;
#5915 = CARTESIAN_POINT ( 'NONE',  ( 22.79799990230000262, 1450.565005821530121, 218.5548369444179855 ) ) ;
#5916 = CARTESIAN_POINT ( 'NONE',  ( 10.89432528737160055, 1461.587524139910101, 210.3982013538480089 ) ) ;
#5917 = CARTESIAN_POINT ( 'NONE',  ( 7.866724121416869941, 1511.219705715099963, 203.6977230978289981 ) ) ;
#5918 =( BOUNDED_CURVE ( )  B_SPLINE_CURVE ( 2, ( #99780, #55622, #89198 ),
 .UNSPECIFIED., .F., .T. ) 
 B_SPLINE_CURVE_WITH_KNOTS ( ( 3, 3 ),
 ( 0.1572692979053489926, 0.2337410564013850112 ),
 .UNSPECIFIED. ) 
 CURVE ( )  GEOMETRIC_REPRESENTATION_ITEM ( )  RATIONAL_B_SPLINE_CURVE ( ( 1.002044729868130091, 1.002448067003099963, 1.002760198777220113 ) ) 
 REPRESENTATION_ITEM ( '' )  );
#5919 = CARTESIAN_POINT ( 'NONE',  ( 4.514829284230000184, 1467.261183020589897, 217.9965697402589910 ) ) ;
#5920 = CARTESIAN_POINT ( 'NONE',  ( 15.57895570635746729, 1420.991873654417759, 227.6562969275110504 ) ) ;
#5921 = CARTESIAN_POINT ( 'NONE',  ( 5.250757762980000187, 1425.396628029330259, 185.7731830333980270 ) ) ;
#5922 = CARTESIAN_POINT ( 'NONE',  ( -19.53581944440000129, 1426.498310938329951, 223.6168261148980037 ) ) ;
#5923 = CARTESIAN_POINT ( 'NONE',  ( -24.39260298050000131, 1436.577174086429977, 139.3086241096980018 ) ) ;
#5924 = CARTESIAN_POINT ( 'NONE',  ( -107.3811602000000107, 1388.471954844699894, 298.6581246683589939 ) ) ;
#5925 = CARTESIAN_POINT ( 'NONE',  ( 18.05311534039999799, 1478.533517822129852, 189.4273905463979872 ) ) ;
#5926 = CARTESIAN_POINT ( 'NONE',  ( -106.3262284460000018, 1391.611664250580134, 301.2004810296590449 ) ) ;
#5927 = CARTESIAN_POINT ( 'NONE',  ( -29.81576564734521995, 1462.384100490245146, 269.4688546054820790 ) ) ;
#5928 = ORIENTED_EDGE ( 'NONE', *, *, #77821, .F. ) ;
#5929 = CARTESIAN_POINT ( 'NONE',  ( 15.69795926444620271, 1519.551704408389924, 222.7678737639049871 ) ) ;
#5930 = CARTESIAN_POINT ( 'NONE',  ( -40.87222264588623943, 1425.533548234441241, 269.1063209156467906 ) ) ;
#5931 = CARTESIAN_POINT ( 'NONE',  ( 32.85805783624304155, 1523.678648413191695, 201.0453875934054508 ) ) ;
#5932 = CARTESIAN_POINT ( 'NONE',  ( -11.16733641199999916, 1453.313060387329870, 225.4924597496980141 ) ) ;
#5933 = CARTESIAN_POINT ( 'NONE',  ( -0.1157347679000000074, 1416.431691060530056, 233.7196346762979999 ) ) ;
#5934 = CARTESIAN_POINT ( 'NONE',  ( -12.92866756046528742, 1442.907176575177346, 186.4521622979591768 ) ) ;
#5935 = ADVANCED_FACE ( 'NONE', ( #89792 ), #107701, .T. ) ;
#5936 = CARTESIAN_POINT ( 'NONE',  ( -8.992268003901459750, 1437.995299232369916, 210.5002298188580028 ) ) ;
#5937 = FACE_OUTER_BOUND ( 'NONE', #15127, .T. ) ;
#5938 = CARTESIAN_POINT ( 'NONE',  ( -0.8307656363412412315, 1415.466171952180275, 233.3157467582985305 ) ) ;
#5939 = CARTESIAN_POINT ( 'NONE',  ( -15.14662681555729939, 1415.677402202029953, 208.0848883706039771 ) ) ;
#5940 = CARTESIAN_POINT ( 'NONE',  ( 23.84671661830000033, 1435.330256084430175, 136.8235927701979904 ) ) ;
#5942 = EDGE_CURVE ( 'NONE', #67300, #78937, #106545, .T. ) ;
#5941 = CARTESIAN_POINT ( 'NONE',  ( -12.57626553825837057, 1442.780697748498824, 169.4711281103210183 ) ) ;
#5944 = ORIENTED_EDGE ( 'NONE', *, *, #12567, .F. ) ;
#5943 = CARTESIAN_POINT ( 'NONE',  ( -15.10371725490000117, 1409.440493816029857, 225.2902966875980155 ) ) ;
#5945 = CARTESIAN_POINT ( 'NONE',  ( -113.4000000000000057, 1380.809950924229952, 299.4484696716589838 ) ) ;
#5946 = CARTESIAN_POINT ( 'NONE',  ( 14.56186259785490122, 1513.645442088340133, 224.1908963721469945 ) ) ;
#5947 = VERTEX_POINT ( 'NONE', #64070 ) ;
#5948 = ORIENTED_EDGE ( 'NONE', *, *, #35114, .T. ) ;
#5949 = CARTESIAN_POINT ( 'NONE',  ( -12.24556316650000021, 1502.082825312490058, 210.5128827789189927 ) ) ;
#5950 = CARTESIAN_POINT ( 'NONE',  ( -20.49599333844828664, 1525.960063244516959, 233.8638087104926058 ) ) ;
#5952 = CARTESIAN_POINT ( 'NONE',  ( -7.835336891880000820, 1460.591301111030134, 220.7785084851980173 ) ) ;
#5951 = CARTESIAN_POINT ( 'NONE',  ( 5.215576331900000362, 1455.428525482890109, 217.8852023316690065 ) ) ;
#5953 = CARTESIAN_POINT ( 'NONE',  ( -9.828024485749999428, 1446.801136681789785, 212.2328357390990163 ) ) ;
#5954 = CARTESIAN_POINT ( 'NONE',  ( -11.10223665490000045, 1433.397901385839987, 151.6819397502979712 ) ) ;
#5955 = DIRECTION ( 'NONE',  ( 0.000000000000000000, 0.000000000000000000, 1.000000000000000000 ) ) ;
#5956 = CARTESIAN_POINT ( 'NONE',  ( 13.82860585633196848, 1517.051704408389924, 192.0119494921260639 ) ) ;
#5957 = CARTESIAN_POINT ( 'NONE',  ( 33.91369110979999846, 1435.681798629080049, 135.0664268281979901 ) ) ;
#5958 = CARTESIAN_POINT ( 'NONE',  ( -14.15746895765553148, 1429.524163386080772, 222.2892373711416667 ) ) ;
#5959 = CARTESIAN_POINT ( 'NONE',  ( -4.314880714020009833, 1453.742010946499931, 199.5809203820919890 ) ) ;
#5960 = CARTESIAN_POINT ( 'NONE',  ( 1.131674255589999900, 1451.349625404129938, 182.9318192675980299 ) ) ;
#5961 = CARTESIAN_POINT ( 'NONE',  ( -4.309579507020567135, 1362.750343653446180, 208.3718459617061285 ) ) ;
#5962 = CARTESIAN_POINT ( 'NONE',  ( -11.10591547028436210, 1509.425967423228713, 236.9904550492935869 ) ) ;
#5964 = EDGE_LOOP ( 'NONE', ( #32970, #90754, #617, #7248 ) ) ;
#5963 = CARTESIAN_POINT ( 'NONE',  ( 1.012732680628119953E-08, 1406.631737762240164, 265.7406131533139728 ) ) ;
#5965 = EDGE_LOOP ( 'NONE', ( #80360, #67781, #4261, #92596 ) ) ;
#5966 = CARTESIAN_POINT ( 'NONE',  ( -11.86416350221509930, 1432.200641232820089, 149.9806832619509862 ) ) ;
#5967 = CARTESIAN_POINT ( 'NONE',  ( -0.3156253571057110463, 1500.458247417000166, 233.1765627430370103 ) ) ;
#5968 = CARTESIAN_POINT ( 'NONE',  ( -7.320734367630000072, 1471.591706303030151, 270.0738322358980099 ) ) ;
#5969 = CARTESIAN_POINT ( 'NONE',  ( -0.7525844464480936358, 1473.757687442616771, 219.3350183411363048 ) ) ;
#5970 = CARTESIAN_POINT ( 'NONE',  ( -125.6580589596999431, 1375.179104070691892, 301.0918496320489339 ) ) ;
#5971 = CARTESIAN_POINT ( 'NONE',  ( 37.04734811236939862, 1450.866104830520044, 135.5959735071040200 ) ) ;
#5972 = CARTESIAN_POINT ( 'NONE',  ( 0.2217422282631729968, 1451.716230971589766, 182.8672561695299805 ) ) ;
#5973 = CARTESIAN_POINT ( 'NONE',  ( -8.846250282050000635, 1384.840587597319882, 199.9252785036290163 ) ) ;
#5974 = CARTESIAN_POINT ( 'NONE',  ( 18.13470581173330132, 1431.285403419799877, 206.8618331735010258 ) ) ;
#5975 = CARTESIAN_POINT ( 'NONE',  ( -3.286483335600000277, 1456.341186815189758, 218.0120298563990104 ) ) ;
#5976 = CARTESIAN_POINT ( 'NONE',  ( 11.85145339950207521, 1363.709651157501412, 209.6218459617033432 ) ) ;
#5977 = CARTESIAN_POINT ( 'NONE',  ( -43.82815393974300378, 1429.932399413429948, 268.2833890840869913 ) ) ;
#5978 = ORIENTED_EDGE ( 'NONE', *, *, #61644, .T. ) ;
#5979 = CARTESIAN_POINT ( 'NONE',  ( -3.533055825017940244, 1491.511335076580053, 181.6418872453359938 ) ) ;
#5980 = ORIENTED_EDGE ( 'NONE', *, *, #33687, .F. ) ;
#5981 = ORIENTED_EDGE ( 'NONE', *, *, #31167, .F. ) ;
#5982 = CARTESIAN_POINT ( 'NONE',  ( -4.995994825704999975, 1516.665179208830068, 211.6114635085770033 ) ) ;
#5983 = CARTESIAN_POINT ( 'NONE',  ( -8.561916019487169294, 1448.548092552390017, 212.3149918286959803 ) ) ;
#5984 = CARTESIAN_POINT ( 'NONE',  ( 3.118627138969999990, 1507.020746158230168, 237.9289388427980043 ) ) ;
#5986 = CARTESIAN_POINT ( 'NONE',  ( -14.38276615813130022, 1509.537722091349906, 182.7943691049900110 ) ) ;
#5985 = CARTESIAN_POINT ( 'NONE',  ( 6.949265646015000186, 1517.089216728169959, 212.5747629931370000 ) ) ;
#5987 = CARTESIAN_POINT ( 'NONE',  ( -2.722115699650000220, 1440.429139517749945, 185.2447042016979992 ) ) ;
#5988 = CARTESIAN_POINT ( 'NONE',  ( -2.147779505350395191, 1450.027952981308999, 182.8955025268928978 ) ) ;
#5989 = ORIENTED_EDGE ( 'NONE', *, *, #43929, .F. ) ;
#5990 = CARTESIAN_POINT ( 'NONE',  ( -26.59118184279999753, 1435.506208013240212, 135.8223177419979777 ) ) ;
#5991 = CARTESIAN_POINT ( 'NONE',  ( 6.552897366944999469, 1516.858146885269889, 202.5651945608169910 ) ) ;
#5992 = CARTESIAN_POINT ( 'NONE',  ( -39.13294649639051670, 1449.732215464259525, 134.8602047732755693 ) ) ;
#5993 = CARTESIAN_POINT ( 'NONE',  ( 1.261852030525026258, 1508.993026050927256, 238.7550003759345998 ) ) ;
#5994 = CARTESIAN_POINT ( 'NONE',  ( -27.23383974134830154, 1417.435118850199842, 269.7057695636269727 ) ) ;
#5995 = DIRECTION ( 'NONE',  ( -5.980589973904019347E-17, 1.000000000000000000, -1.736889445713099699E-16 ) ) ;
#5996 = CARTESIAN_POINT ( 'NONE',  ( -2.560623336209999934, 1397.364455864229967, 196.3367421450979862 ) ) ;
#5998 = EDGE_LOOP ( 'NONE', ( #90814, #20701, #47201, #91238, #70087 ) ) ;
#5997 = CARTESIAN_POINT ( 'NONE',  ( -8.103791294879806983, 1364.808472168752587, 208.3718459617061285 ) ) ;
#5999 = ORIENTED_EDGE ( 'NONE', *, *, #85173, .T. ) ;
#6000 = DIRECTION ( 'NONE',  ( 0.000000000000000000, 0.000000000000000000, 1.000000000000000000 ) ) ;
#6001 = AXIS2_PLACEMENT_3D ( 'NONE', #71815, #63404, #78520 ) ;
#6002 = CARTESIAN_POINT ( 'NONE',  ( 3.959152859930000101, 1428.396642669490120, 216.3690266601789745 ) ) ;
#6003 = CARTESIAN_POINT ( 'NONE',  ( -13.83438311809999810, 1379.888128081619925, 206.0089139935990090 ) ) ;
#6004 = CARTESIAN_POINT ( 'NONE',  ( -2.500000000000000000, 1419.383254857029897, 144.0944172368980105 ) ) ;
#6005 = CARTESIAN_POINT ( 'NONE',  ( -1.465793849540000027, 1484.360957265730121, 182.4810413031979976 ) ) ;
#6006 = CARTESIAN_POINT ( 'NONE',  ( 1.136814033864999907, 1516.854133554269993, 211.4058994415870245 ) ) ;
#6007 = LINE ( 'NONE', #32317, #98441 ) ;
#6008 = DIRECTION ( 'NONE',  ( 0.000000000000000000, 1.000000000000000000, 0.000000000000000000 ) ) ;
#6009 = CARTESIAN_POINT ( 'NONE',  ( 8.466507779077819151, 1437.781662910839941, 212.4976436764690106 ) ) ;
#6010 = FACE_OUTER_BOUND ( 'NONE', #25973, .T. ) ;
#6011 = CARTESIAN_POINT ( 'NONE',  ( 7.556074062054999985, 1510.693074690949970, 204.3088345461070219 ) ) ;
#6012 = CARTESIAN_POINT ( 'NONE',  ( 2.282622912365000367, 1516.861367446839949, 206.8218623544969716 ) ) ;
#6013 = VERTEX_POINT ( 'NONE', #98188 ) ;
#6014 = CARTESIAN_POINT ( 'NONE',  ( -33.91369117178599879, 1451.728768195329849, 134.4203408260499941 ) ) ;
#6015 = CARTESIAN_POINT ( 'NONE',  ( -10.28735288409999882, 1471.931396637590069, 208.3821031841859792 ) ) ;
#6016 = CARTESIAN_POINT ( 'NONE',  ( -23.49708866447455691, 1448.323603619134701, 215.7384060670668759 ) ) ;
#6017 = ORIENTED_EDGE ( 'NONE', *, *, #89082, .T. ) ;
#6018 = CARTESIAN_POINT ( 'NONE',  ( -17.84338787571901364, 1523.481610426287716, 237.8836641337663309 ) ) ;
#6019 = CARTESIAN_POINT ( 'NONE',  ( 11.99125049862840164, 1436.336701747860161, 149.2203835722019960 ) ) ;
#6020 = B_SPLINE_SURFACE_WITH_KNOTS ( 'NONE', 5, 5, ( 
 ( #65952, #7125, #83277, #33404, #74355, #32331, #75454, #6575, #50779, #40724, #74896, #48595 ),
 ( #109590, #14402, #32859, #58094, #7667, #101158, #108483, #25000, #31766, #84912, #24452, #58640 ),
 ( #92773, #67599, #16049, #50252, #75979, #8205, #42372, #76527, #110678, #33970, #22790, #56995 ),
 ( #82729, #8759, #51895, #408, #104491, #60867, #59744, #52455, #26105, #103364, #94993, #60295 ),
 ( #35077, #27784, #34525, #87141, #36192, #77100, #18260, #102273, #68706, #17133, #42940, #43496 ),
 ( #86034, #102811, #44044, #44601, #25553, #85459, #69257, #77639, #93865, #53007, #61416, #95539 ),
 ( #35625, #26667, #9334, #94413, #17690, #952, #18812, #2060, #51323, #10431, #86584, #9876 ),
 ( #78183, #1493, #78744, #70376, #69820, #103938, #27236, #84183, #33229, #102617, #59009, #91493 ),
 ( #75799, #101517, #76908, #14773, #41643, #42196, #7482, #16948, #59555, #83090, #6383, #25917 ),
 ( #51150, #66320, #33776, #25363, #50055, #48959, #40531, #66865, #6926, #76347, #74707, #23720 ),
 ( #15850, #109409, #24804, #32135, #93669, #85277, #110496, #108838, #109950, #100438, #93136, #8576 ),
 ( #41083, #67418, #57906, #92040, #42746, #15312, #92578, #67972, #49505, #16404, #32685, #83630 ),
 ( #75260, #215, #50598, #34340, #102080, #68518, #58451, #100974, #24270, #84730, #8027, #35445 ),
 ( #72774, #78558, #51706, #104306, #86395, #10240, #36008, #9684, #43308, #52817, #38595, #60675 ),
 ( #81152, #103177, #70200, #106902, #26479, #85846, #759, #103756, #27057, #77999, #94801, #61781 ),
 ( #60115, #9145, #95357, #1305, #94233, #79126, #87518, #10807, #44977, #27597, #61243, #43852 ),
 ( #17508, #77457, #2434, #97946, #34887, #18076, #18617, #21214, #36549, #29647, #86948, #52271 ),
 ( #95905, #19166, #69633, #70746, #44416, #53372, #1874, #106361, #63834, #55423, #12845, #89556 ) ),
 .UNSPECIFIED., .F., .F., .F.,
 ( 6, 3, 3, 3, 3, 6 ),
 ( 6, 3, 3, 6 ),
 ( 8.580843589984830544, 11.93617684059999995, 16.46680586349999942, 17.68033087479999921, 18.28709338049999999, 18.73288479507320048 ),
 ( -0.0007644201731544349393, 0.4984688824269999929, 1.495406647280000056, 2.064389376412830046 ),
 .UNSPECIFIED. ) ;
#6021 = CARTESIAN_POINT ( 'NONE',  ( 13.65307821729999915, 1415.140114704729967, 197.5268032949979897 ) ) ;
#6022 = DIRECTION ( 'NONE',  ( 1.836970198721029688E-16, 1.000000000000000000, -1.793662034335764721E-47 ) ) ;
#6023 = CARTESIAN_POINT ( 'NONE',  ( 1.704192342800000001E-13, 1475.048391919030109, 269.6500679772980220 ) ) ;
#6024 = CYLINDRICAL_SURFACE ( 'NONE', #32104, 2.000000000000003553 ) ;
#6025 = CARTESIAN_POINT ( 'NONE',  ( 7.898231641030000638, 1488.783166887790003, 199.9435678271790096 ) ) ;
#6026 = CARTESIAN_POINT ( 'NONE',  ( -0.3175620501786377559, 1506.436298853426024, 187.1391428864371846 ) ) ;
#6027 = CARTESIAN_POINT ( 'NONE',  ( 24.32234920051570626, 1445.577642606156360, 214.2383469815599142 ) ) ;
#6028 = CARTESIAN_POINT ( 'NONE',  ( -1.842963673760081633, 1515.499673572818438, 205.0355315610892717 ) ) ;
#6029 = CARTESIAN_POINT ( 'NONE',  ( 16.40119952638874068, 1409.652464920799048, 226.0181189573841891 ) ) ;
#6031 = B_SPLINE_CURVE_WITH_KNOTS ( 'NONE', 5,
 ( #7132, #42378, #42946, #85465, #52460, #8765 ),
 .UNSPECIFIED., .F., .F.,
 ( 6, 6 ),
 ( -1.999999948112589854, 0.000000000000000000 ),
 .UNSPECIFIED. ) ;
#6030 = CARTESIAN_POINT ( 'NONE',  ( -7.328676208015000526, 1516.833844030519913, 216.0648195994369871 ) ) ;
#6032 = ORIENTED_EDGE ( 'NONE', *, *, #62416, .F. ) ;
#6033 = CARTESIAN_POINT ( 'NONE',  ( -17.55052187609999592, 1417.724842222909956, 206.6897972996389967 ) ) ;
#6034 = CARTESIAN_POINT ( 'NONE',  ( -7.722580352398438208, 1517.051704408390378, 206.9393828551336583 ) ) ;
#6035 = CARTESIAN_POINT ( 'NONE',  ( 0.4933970490180000779, 1420.589273614029935, 183.4078724835979983 ) ) ;
#6036 = EDGE_CURVE ( 'NONE', #97770, #67358, #53252, .T. ) ;
#6037 = CARTESIAN_POINT ( 'NONE',  ( -14.62138543496649845, 1508.449146121320155, 215.8538878429280032 ) ) ;
#6038 = CARTESIAN_POINT ( 'NONE',  ( 1.270728227940000066, 1414.996442546130083, 191.7853923321980005 ) ) ;
#6039 = CARTESIAN_POINT ( 'NONE',  ( -0.04745950029138250315, 1508.924973538250015, 179.5474405769929831 ) ) ;
#6040 = CARTESIAN_POINT ( 'NONE',  ( -11.35660239823070050, 1471.035763858380051, 207.9971984677779915 ) ) ;
#6041 = CARTESIAN_POINT ( 'NONE',  ( 2.058017575162654822, 1417.326595624436550, 233.1728886830721876 ) ) ;
#6042 = CARTESIAN_POINT ( 'NONE',  ( 17.98726295721315793, 1424.120998220819729, 225.5226115392007955 ) ) ;
#6043 = CARTESIAN_POINT ( 'NONE',  ( -109.1656546792999904, 1384.956445601399992, 297.1328575267269798 ) ) ;
#6044 = EDGE_CURVE ( 'NONE', #52345, #89175, #4689, .T. ) ;
#6045 = CARTESIAN_POINT ( 'NONE',  ( -5.311472889528250303E-07, 1407.436814443840149, 222.1874709566379806 ) ) ;
#6046 = CARTESIAN_POINT ( 'NONE',  ( 33.71363641244969500, 1440.913060384090159, 248.2283521579210230 ) ) ;
#6048 = CARTESIAN_POINT ( 'NONE',  ( -18.10730182580141090, 1463.999204004485136, 217.9814146746393533 ) ) ;
#6047 = CARTESIAN_POINT ( 'NONE',  ( -11.08439360582739930, 1470.227138793769882, 211.7024792797219845 ) ) ;
#6049 = CARTESIAN_POINT ( 'NONE',  ( -0.3788333198289999815, 1408.926289538330138, 186.6322588406980003 ) ) ;
#6050 = ORIENTED_EDGE ( 'NONE', *, *, #71943, .T. ) ;
#6051 = ORIENTED_EDGE ( 'NONE', *, *, #14089, .F. ) ;
#6052 = CARTESIAN_POINT ( 'NONE',  ( 10.56872017243719952, 1481.355203388010068, 208.7623620626110039 ) ) ;
#6053 = CARTESIAN_POINT ( 'NONE',  ( -19.79281846730729200, 1484.923549257670402, 190.6224826566608783 ) ) ;
#6054 = CARTESIAN_POINT ( 'NONE',  ( -5.051845285050000633, 1442.712514107189918, 200.9272700336389903 ) ) ;
#6055 = DIRECTION ( 'NONE',  ( -1.000000000000000000, 0.000000000000000000, 0.000000000000000000 ) ) ;
#6056 = CARTESIAN_POINT ( 'NONE',  ( -2.500000000000000000, 1419.383100980419840, 144.1003751433630100 ) ) ;
#6057 = CARTESIAN_POINT ( 'NONE',  ( 11.00329356315880069, 1422.205372314400165, 210.7649067250879966 ) ) ;
#6058 = CARTESIAN_POINT ( 'NONE',  ( -10.63964957199999972, 1491.500814366789882, 212.0075699686489941 ) ) ;
#6059 = CARTESIAN_POINT ( 'NONE',  ( -30.31940284292399923, 1523.382868172864164, 222.4933038710547635 ) ) ;
#6060 = CARTESIAN_POINT ( 'NONE',  ( -48.06877316588859372, 1383.815103002690194, 257.3679311951680120 ) ) ;
#6061 = CARTESIAN_POINT ( 'NONE',  ( -3.991161821394999976, 1511.207707629420156, 201.3372867307170111 ) ) ;
#6062 = CARTESIAN_POINT ( 'NONE',  ( -14.87725549029999961, 1489.466917449729863, 192.6664679402979914 ) ) ;
#6063 = CARTESIAN_POINT ( 'NONE',  ( -5.556349349672759175, 1511.457792576462907, 200.4111309786675577 ) ) ;
#6064 = CARTESIAN_POINT ( 'NONE',  ( 10.77265657036890012, 1491.996909311660147, 212.1278075563569985 ) ) ;
#6066 = VERTEX_POINT ( 'NONE', #40489 ) ;
#6065 = CARTESIAN_POINT ( 'NONE',  ( -1.875564068250000105, 1457.387223672290020, 219.2073648825989949 ) ) ;
#6067 = CARTESIAN_POINT ( 'NONE',  ( -1.376413794940000157, 1450.856769977960084, 182.9787630389979824 ) ) ;
#6068 = CARTESIAN_POINT ( 'NONE',  ( -27.74315420650000164, 1383.844892876249787, 225.5041886164589755 ) ) ;
#6069 = CARTESIAN_POINT ( 'NONE',  ( 4.692464771457559358, 1508.551704408389924, 205.4575493268739876 ) ) ;
#6070 = ORIENTED_EDGE ( 'NONE', *, *, #83645, .T. ) ;
#6071 = EDGE_LOOP ( 'NONE', ( #100719, #67842, #79528, #86986 ) ) ;
#6072 = CARTESIAN_POINT ( 'NONE',  ( -7.726443128496979895, 1385.956550061749795, 218.9144042117120250 ) ) ;
#6073 = CARTESIAN_POINT ( 'NONE',  ( -3.272123973762000038, 1515.551704204689941, 205.4774943669999914 ) ) ;
#6075 = CARTESIAN_POINT ( 'NONE',  ( -4.958564224928870168, 1476.141795758730041, 200.0452580833139962 ) ) ;
#6074 = CARTESIAN_POINT ( 'NONE',  ( 5.864566082395450408, 1517.051704408389924, 226.1537825710409777 ) ) ;
#6076 = AXIS2_PLACEMENT_3D ( 'NONE', #20156, #36966, #71157 ) ;
#6077 = CARTESIAN_POINT ( 'NONE',  ( 7.000867164840526513, 1506.106661430532313, 218.4736308527704978 ) ) ;
#6078 = CARTESIAN_POINT ( 'NONE',  ( -104.5771061929999917, 1379.756820536730174, 302.9490267888589869 ) ) ;
#6079 = CARTESIAN_POINT ( 'NONE',  ( -15.40447533607079578, 1419.996928346919958, 211.7847516026819505 ) ) ;
#6080 = CARTESIAN_POINT ( 'NONE',  ( -15.88879189127879954, 1508.551704408389924, 213.9582233978679824 ) ) ;
#6081 = CARTESIAN_POINT ( 'NONE',  ( 4.258779903668019173, 1409.061780258630051, 194.7559829868740167 ) ) ;
#6082 = CARTESIAN_POINT ( 'NONE',  ( 18.28847123799999963, 1425.325025442230071, 225.4709929694980133 ) ) ;
#6083 = CARTESIAN_POINT ( 'NONE',  ( 15.69667967640000050, 1457.921467858090182, 221.7535892932990009 ) ) ;
#6084 = CARTESIAN_POINT ( 'NONE',  ( 6.867528398042960447, 1434.820408621019851, 203.9336372596199851 ) ) ;
#6085 = DIRECTION ( 'NONE',  ( 1.000000000000000000, 0.000000000000000000, 0.000000000000000000 ) ) ;
#6086 = CIRCLE ( 'NONE', #13177, 1.999999999999999556 ) ;
#6087 = CARTESIAN_POINT ( 'NONE',  ( -3.617662457638250117, 1448.976550491250009, 184.9371969260439812 ) ) ;
#6088 = ORIENTED_EDGE ( 'NONE', *, *, #32338, .T. ) ;
#6089 = CARTESIAN_POINT ( 'NONE',  ( -22.07680858347428909, 1523.847233649538339, 184.4451117503444664 ) ) ;
#6090 = CARTESIAN_POINT ( 'NONE',  ( -8.593470627377898907, 1428.030732904877141, 134.0999999980980135 ) ) ;
#6091 = CARTESIAN_POINT ( 'NONE',  ( 14.29468422029999886, 1410.759725256029924, 191.3977978341980020 ) ) ;
#6092 = CARTESIAN_POINT ( 'NONE',  ( 31.44837959398582328, 1511.187213306747708, 197.3353852117981262 ) ) ;
#6093 = CARTESIAN_POINT ( 'NONE',  ( -20.37362044233400127, 1500.532225497879836, 190.6021518776060191 ) ) ;
#6094 = CARTESIAN_POINT ( 'NONE',  ( -108.2808028870000072, 1386.465776205880047, 310.9170304772590043 ) ) ;
#6095 = CARTESIAN_POINT ( 'NONE',  ( -7.395102162025949610, 1511.068351247050032, 215.4971964518929894 ) ) ;
#6096 = CARTESIAN_POINT ( 'NONE',  ( -9.230109932484202417, 1361.837706146139681, 207.6218459616987673 ) ) ;
#6097 = LINE ( 'NONE', #49227, #50092 ) ;
#6098 = CARTESIAN_POINT ( 'NONE',  ( -19.28416521189999955, 1426.095206623730064, 225.9565170197979853 ) ) ;
#6099 = CARTESIAN_POINT ( 'NONE',  ( -20.76266710848580033, 1464.825012654529928, 208.5383817516119791 ) ) ;
#6100 = CARTESIAN_POINT ( 'NONE',  ( 3.447128460625000113, 1516.778853242349896, 207.9866608880570027 ) ) ;
#6101 = CARTESIAN_POINT ( 'NONE',  ( 2.930076095445649731, 1409.015380899219963, 223.9343627405490054 ) ) ;
#6102 = CARTESIAN_POINT ( 'NONE',  ( 30.37359097063795588, 1526.143142182265819, 201.3152257445537714 ) ) ;
#6103 = CARTESIAN_POINT ( 'NONE',  ( -14.20352129384949968, 1379.588683704130062, 207.8472577655950033 ) ) ;
#6104 = CARTESIAN_POINT ( 'NONE',  ( 7.499139530464689507, 1425.344745441989971, 212.2485671964089988 ) ) ;
#6105 = ORIENTED_EDGE ( 'NONE', *, *, #97262, .T. ) ;
#6106 = CARTESIAN_POINT ( 'NONE',  ( -4.212364877099999840E-09, 1416.130848190830193, 240.4142140047979694 ) ) ;
#6107 = CARTESIAN_POINT ( 'NONE',  ( -28.11157287190000176, 1508.133875831329760, 208.0042757565580018 ) ) ;
#6109 = FACE_OUTER_BOUND ( 'NONE', #105250, .T. ) ;
#6108 = CARTESIAN_POINT ( 'NONE',  ( 1.469976146670000094, 1486.449623437230002, 182.0144994357980011 ) ) ;
#6110 = CARTESIAN_POINT ( 'NONE',  ( -13.69364981090000022, 1418.910360879329801, 238.2645903702979808 ) ) ;
#6111 = CYLINDRICAL_SURFACE ( 'NONE', #8919, 1.999999999999915179 ) ;
#6112 = CARTESIAN_POINT ( 'NONE',  ( -21.42407812907550024, 1452.164915093389936, 141.3791819868360164 ) ) ;
#6113 = CARTESIAN_POINT ( 'NONE',  ( -18.96350866050000050, 1416.837080243330092, 208.0006276345779952 ) ) ;
#6114 = EDGE_LOOP ( 'NONE', ( #16513, #45958, #99431, #72538 ) ) ;
#6115 = CARTESIAN_POINT ( 'NONE',  ( -107.9362316764580072, 1378.913060387339783, 300.0379977988180258 ) ) ;
#6116 = CARTESIAN_POINT ( 'NONE',  ( 10.93419921699999975, 1501.146262457190005, 205.7756198371390042 ) ) ;
#6117 = CARTESIAN_POINT ( 'NONE',  ( 15.82007826961449837, 1421.163257332559851, 227.5271101461229932 ) ) ;
#6118 = CARTESIAN_POINT ( 'NONE',  ( 11.23465321549999985, 1501.870423235890030, 206.7487909662190191 ) ) ;
#6119 = ORIENTED_EDGE ( 'NONE', *, *, #25408, .T. ) ;
#6120 = EDGE_LOOP ( 'NONE', ( #66319, #26316, #34487, #78376 ) ) ;
#6121 = CARTESIAN_POINT ( 'NONE',  ( -62.45667138380000694, 1385.073369564110180, 249.3006260568589880 ) ) ;
#6122 = CARTESIAN_POINT ( 'NONE',  ( -22.80833251699839792, 1409.709435844829841, 209.2324790707910154 ) ) ;
#6123 = CARTESIAN_POINT ( 'NONE',  ( -3.961468203580000402, 1423.998250314630013, 184.1718454746980171 ) ) ;
#6124 = CARTESIAN_POINT ( 'NONE',  ( 4.364199090702369332, 1509.032029411810072, 205.0059829744700153 ) ) ;
#6125 = CARTESIAN_POINT ( 'NONE',  ( -31.23437356469455040, 1511.187213306747708, 195.3468678195118287 ) ) ;
#6126 = CARTESIAN_POINT ( 'NONE',  ( -6.895798589700000925, 1507.635187917330086, 235.7209506179980281 ) ) ;
#6127 = CARTESIAN_POINT ( 'NONE',  ( -22.76667043220000153, 1415.847673962129875, 211.9494722144779928 ) ) ;
#6128 = B_SPLINE_CURVE_WITH_KNOTS ( 'NONE', 3,
 ( #46673, #65663, #88665, #11943, #21954, #72419, #39343, #46124, #3571, #4645, #80253, #107652, #56147, #30936, #47204, #71898, #98694, #13018, #106014, #72959, #29290, #63486, #59470, #100349, #32041, #40438, #101983 ),
 .UNSPECIFIED., .F., .F.,
 ( 4, 2, 1, 1, 1, 1, 1, 1, 2, 2, 2, 2, 1, 1, 1, 2, 2, 4 ),
 ( 0.000000000000000000, 0.2499999999978366749, 0.3749999999967544850, 0.4374999999962133623, 0.4687499999959512942, 0.4843749999958125163, 0.4921874999957430719, 0.4960937499957076557, 0.4980468749956977748, 0.4999999999956878938, 0.6249999999967579267, 0.6874999999973000486, 0.7187499999975709430, 0.7343749999977112752, 0.7421874999977768894, 0.7460937499978097520, 0.7499999999978425036, 1.000000000000000000 ),
 .UNSPECIFIED. ) ;
#6129 = ORIENTED_EDGE ( 'NONE', *, *, #52429, .T. ) ;
#6130 = CARTESIAN_POINT ( 'NONE',  ( 46.04304765074009964, 1443.742661411660038, 266.9755472754490029 ) ) ;
#6131 = CARTESIAN_POINT ( 'NONE',  ( -1.126474399395450021, 1424.149452017869862, 228.3764236718020015 ) ) ;
#6132 = CARTESIAN_POINT ( 'NONE',  ( 0.01346536989209999938, 1420.212931417629989, 183.8948729780979932 ) ) ;
#6133 = CARTESIAN_POINT ( 'NONE',  ( -6.947377821305000367, 1517.009964551830080, 204.5062011277169916 ) ) ;
#6134 = ORIENTED_EDGE ( 'NONE', *, *, #58907, .T. ) ;
#6135 = CARTESIAN_POINT ( 'NONE',  ( 11.38572442648590055, 1480.473707728230011, 212.2056756853490072 ) ) ;
#6136 = CARTESIAN_POINT ( 'NONE',  ( 15.05672294932299948, 1512.222316757829958, 196.4963374934199862 ) ) ;
#6137 = CARTESIAN_POINT ( 'NONE',  ( 12.53380745427929988, 1442.773887455719887, 186.4115735415020083 ) ) ;
#6138 = ORIENTED_EDGE ( 'NONE', *, *, #91780, .F. ) ;
#6139 = VERTEX_POINT ( 'NONE', #90331 ) ;
#6140 = CARTESIAN_POINT ( 'NONE',  ( -11.66561531531410090, 1481.205695410650151, 211.1318747291790032 ) ) ;
#6141 = FACE_OUTER_BOUND ( 'NONE', #107255, .T. ) ;
#6142 = CARTESIAN_POINT ( 'NONE',  ( -12.89209534591269879, 1512.335564144490036, 193.9409293534239964 ) ) ;
#6143 = CARTESIAN_POINT ( 'NONE',  ( 1.364635942960239934, 1452.865406250129809, 152.5018568859900085 ) ) ;
#6144 = CARTESIAN_POINT ( 'NONE',  ( 11.30339187070000051, 1420.292009770159893, 198.6214305233989990 ) ) ;
#6146 = B_SPLINE_SURFACE_WITH_KNOTS ( 'NONE', 5, 5, ( 
 ( #94017, #8906, #50391, #66648, #41429, #92357, #59894, #85059, #23505 ),
 ( #8350, #24586, #42514, #76673, #40863, #110267, #85606, #31909, #110823 ),
 ( #58779, #66098, #83412, #25696, #34116, #68306, #76126, #84519, #49283 ),
 ( #100224, #93457, #24035, #102414, #33544, #17282, #25144, #57697, #41974 ),
 ( #6707, #67742, #100750, #51475, #15090, #16189, #74493, #109190, #108621 ),
 ( #91811, #32475, #75039, #109726, #59349, #7807, #33003, #58233, #16728 ),
 ( #75595, #92917, #15629, #101851, #49836, #7265, #83965, #67189, #101290 ),
 ( #95136, #544, #54261, #62113, #88388, #43083, #60446, #19514, #96798 ),
 ( #77785, #61009, #69964, #17838, #71070, #43635, #1095, #26823, #18397 ),
 ( #78333, #86730, #45306, #70518, #96237, #104633, #52595, #27930, #10021 ),
 ( #77244, #53719, #44752, #52041, #1645, #87856, #44191, #9470, #61554 ),
 ( #35223, #79444, #2755, #11144, #34668, #27372, #104078, #26258, #35781 ) ),
 .UNSPECIFIED., .F., .F., .F.,
 ( 6, 3, 3, 6 ),
 ( 6, 3, 6 ),
 ( 33.18405829000000296, 37.67969033829999859, 42.57359936619999985, 50.39824048690000069 ),
 ( 0.000000000000000000, 1.000000000000000000, 2.000000000000000000 ),
 .UNSPECIFIED. ) ;
#6145 = CARTESIAN_POINT ( 'NONE',  ( 16.93202667939999984, 1409.669517366430000, 192.7683719188979978 ) ) ;
#6147 = CARTESIAN_POINT ( 'NONE',  ( -3.670436697740000032, 1428.951561676790107, 201.2856072060390034 ) ) ;
#6148 = CARTESIAN_POINT ( 'NONE',  ( -4.744745735780000473, 1495.278903626390047, 198.1817743977989892 ) ) ;
#6149 = TOROIDAL_SURFACE ( 'NONE', #7909, 11.34254167809999991, 1.000000000000000000 ) ;
#6150 = PLANE ( 'NONE',  #12439 ) ;
#6152 = CARTESIAN_POINT ( 'NONE',  ( -105.7010335431549919, 1391.686106122180036, 304.9005242218860303 ) ) ;
#6151 = CARTESIAN_POINT ( 'NONE',  ( -13.55647141870050021, 1434.955288304769965, 148.7473005004320044 ) ) ;
#6153 = CARTESIAN_POINT ( 'NONE',  ( 11.86987523124740029, 1426.731981355150083, 206.5550359663369875 ) ) ;
#6154 = B_SPLINE_CURVE_WITH_KNOTS ( 'NONE', 3,
 ( #85637, #17871, #86758, #93487, #52621, #52069, #67222, #77811, #86202, #9493, #85088, #16757, #43660, #10047, #69436, #42003, #44220, #33032, #24611, #92945, #50420, #76151, #16217, #8379, #76700, #7834, #33575, #67767, #54292, #55379, #62711, #97360, #21172, #104109, #3885, #36352, #19544, #20629, #71665, #96830, #45881, #80018, #11176, #79475, #54833, #3339, #37463, #36904, #105785, #29068, #2784, #88957, #63251, #12249, #71099, #46438, #80570, #69994, #27397, #38016, #72196, #87885, #20099, #105223, #28510, #78363, #53175, #106316, #27958, #53752, #29598, #70544, #45336, #11708, #63783, #97900, #89511, #61580, #88418, #12802, #1671, #62141, #95712, #18978, #35812, #87317, #10612, #44781, #78931, #2238, #104661, #96267, #48073, #74942, #109089, #64335, #100653, #30143, #107962, #22834, #55929, #90049, #99550, #58134, #4949, #98458, #31259, #31810, #14989, #40213, #91166, #73835, #23939, #6611, #72727, #65439, #90608, #106851, #46982, #13887, #14441, #82205, #21727, #40763, #48638, #39667, #32370, #57040, #4423, #92267, #81106, #82767, #30705, #65999, #6060, #66551, #22275, #74393, #56476, #13332, #38548, #98998, #39091, #108519, #47523, #100118, #81645, #23403, #57591, #91715, #73269, #107409, #49186, #64891, #83315, #5511, #59790, #84423, #51367, #446, #109629, #110724, #34567, #69302, #41325, #51935, #7708, #67645, #68752, #8800, #34013, #93909, #68208, #60907, #84955, #35121, #32900, #102311, #59244, #8247, #42415, #101198, #76570, #16088, #102855, #110173, #50825, #101754, #58683, #93363, #25598, #86077, #15537, #9373, #43536, #49735, #41867, #94456, #83864, #26713, #33445, #7167, #17734, #25042, #75495, #77681, #993, #26151, #16628, #76020, #60339, #103409, #17177, #85503, #24494, #67095, #42982, #77141, #92817, #50295, #1538, #36231, #20506, #46320, #105659, #53613, #11037, #27832, #45204, #71538, #79345, #70977, #96701, #72078, #10476, #12127, #105092, #52495, #63133, #11586, #45762, #70416, #80449, #36784, #19972, #79899, #62584, #37896, #28382, #95583, #54715, #28944, #61457, #86624, #104536, #44647, #97234, #88842, #87186, #54166, #106192, #27273, #78227, #62013, #96133, #3762, #3212, #2657, #19411, #29474, #88291, #37341, #95033, #87755, #18302, #9917, #44089, #78789, #35672, #69859, #103978, #18851, #53048, #2103, #107289, #64773, #5384, #98883, #65310, #82078, #49060, #57468, #12682, #22150, #73715 ),
 .UNSPECIFIED., .F., .F.,
 ( 4, 3, 3, 3, 3, 3, 3, 3, 3, 3, 3, 3, 3, 3, 3, 3, 3, 3, 3, 3, 3, 3, 3, 3, 3, 3, 3, 3, 3, 3, 3, 3, 3, 3, 3, 3, 3, 3, 3, 3, 3, 3, 3, 3, 3, 3, 3, 3, 3, 3, 3, 3, 3, 3, 3, 3, 3, 3, 3, 3, 3, 3, 3, 3, 3, 3, 3, 3, 3, 3, 3, 3, 3, 3, 3, 3, 3, 3, 3, 3, 3, 3, 3, 3, 3, 3, 3, 3, 3, 3, 3, 3, 3, 3, 3, 3, 3, 3, 4 ),
 ( 9.791890430535840295, 11.09285369171509927, 12.23580266145529905, 13.32189124266249891, 14.35786517582680055, 15.39383910899119989, 16.43170384348270119, 17.51424454637329831, 18.65578198009049871, 19.94097596983310083, 21.40871796212839939, 23.18825047988780241, 24.57707236516490212, 25.82694388649679951, 26.96416132553860123, 27.58084801741189906, 28.69213975917609716, 29.83228324127160036, 31.00605439822959752, 32.21975478572630180, 33.50968302461040338, 34.86206544079449543, 36.29158701301099654, 37.84399942373840275, 39.41521477598699619, 40.90066773311090742, 41.39509552353548827, 43.78336362953579908, 46.21013510696290894, 48.47057239092100644, 50.60413741464040527, 52.51664332244290279, 54.35176539055790101, 56.12437305792799691, 57.84500552525899764, 59.52142888499740536, 61.14147335462639887, 62.73422932219951065, 64.28850022341509884, 65.53909258067669441, 67.16750662264719551, 68.87443876010290467, 70.68916954752430115, 72.66968054463819726, 75.04465672271381038, 77.84631887446640519, 79.90746703447679522, 81.76360575179620582, 83.49913842151880772, 85.15038425320570070, 86.70972796428270613, 88.22871214351719971, 89.69423399335190084, 90.91108773661989062, 92.83291460103269799, 94.80415031745300780, 96.80839894437879423, 98.81724224162638848, 100.7996825303579982, 102.7346356577239987, 104.5974014464039925, 106.3969924060370005, 108.1506441523539905, 109.8627096898800062, 111.5372853772309867, 113.1614624162640013, 114.7605425252640003, 116.3232191975509977, 117.6367619671650004, 119.0824689242389951, 120.5712865488890060, 122.0980518405219897, 123.6174000461700047, 125.1072950620849724, 126.5560501033809970, 128.0293868453329935, 129.3730365330290226, 130.6858248218609901, 131.9587287906659867, 132.4493970711910151, 133.5505940240470011, 134.6525636770870165, 135.7548240709300273, 136.8874810004660105, 137.9883391253270020, 139.0879140777240082, 140.1858124869349922, 141.2816593830939951, 142.3738793671560074, 143.4636526237109990, 144.5496010613929911, 144.8160795072120095, 146.5657509711560067, 148.3964307047820057, 150.2900657918840182, 152.1597978627970065, 153.9625895061970198, 155.6511879984489894, 157.1997893379999880 ),
 .UNSPECIFIED. ) ;
#6155 = CARTESIAN_POINT ( 'NONE',  ( -9.721984167771511309, 1440.173042851740092, 206.7023544724380031 ) ) ;
#6156 = CARTESIAN_POINT ( 'NONE',  ( 7.214502255410000231, 1427.316505021429975, 144.1938086916980239 ) ) ;
#6157 = EDGE_LOOP ( 'NONE', ( #35933, #103858, #3055, #67312 ) ) ;
#6158 = CARTESIAN_POINT ( 'NONE',  ( 21.37693747720000204, 1440.913060387330006, 224.8635562088979896 ) ) ;
#6159 = AXIS2_PLACEMENT_3D ( 'NONE', #30330, #55017, #46065 ) ;
#6160 = DIRECTION ( 'NONE',  ( 1.192122195693504081E-14, -4.372198439846870180E-16, -1.000000000000000000 ) ) ;
#6161 = CARTESIAN_POINT ( 'NONE',  ( -101.9070034985570032, 1384.941843689829966, 311.0171509276760275 ) ) ;
#6162 = B_SPLINE_SURFACE_WITH_KNOTS ( 'NONE', 5, 5, ( 
 ( #102167, #50677, #76426, #110580, #59641, #17029 ),
 ( #43392, #51792, #8654, #69153, #34426, #42832 ),
 ( #76993, #86477, #68599, #102703, #25997, #60195 ),
 ( #94314, #9773, #75349, #109489, #10323, #28236 ),
 ( #2515, #18707, #27139, #88707, #95989, #104391 ),
 ( #62993, #36095, #78642, #87034, #106052, #44497 ),
 ( #63531, #36639, #105502, #28794, #61325, #69721 ),
 ( #43938, #95443, #53460, #70835, #52904, #103839 ),
 ( #1957, #70281, #27687, #104945, #61871, #19255 ) ),
 .UNSPECIFIED., .F., .F., .F.,
 ( 6, 3, 6 ),
 ( 6, 6 ),
 ( 3.650975912550000313, 7.249943402570000472, 12.02648879740000076 ),
 ( 0.000000000000000000, 2.000000000000000000 ),
 .UNSPECIFIED. ) ;
#6163 = CARTESIAN_POINT ( 'NONE',  ( -9.923943078109999760, 1386.701148096399947, 200.5013422001489687 ) ) ;
#6164 = CARTESIAN_POINT ( 'NONE',  ( 9.368003223766120158, 1423.587887591870185, 210.1931883339019862 ) ) ;
#6166 = ORIENTED_EDGE ( 'NONE', *, *, #45039, .F. ) ;
#6165 = CARTESIAN_POINT ( 'NONE',  ( 11.02661629080069972, 1423.097658921510174, 203.2974929890660007 ) ) ;
#6167 = CARTESIAN_POINT ( 'NONE',  ( 5.009886284249999377, 1430.069699660889910, 217.1776678749689893 ) ) ;
#6168 = CARTESIAN_POINT ( 'NONE',  ( 4.122931283589999374E-15, 1438.194204504490017, 150.6035180695979818 ) ) ;
#6169 = CARTESIAN_POINT ( 'NONE',  ( -13.58245609809999976, 1416.835809823829777, 221.9090836517979994 ) ) ;
#6170 = CARTESIAN_POINT ( 'NONE',  ( 11.35166415849999844, 1433.891578315870220, 151.4717738640979974 ) ) ;
#6171 = ADVANCED_FACE ( 'NONE', ( #66281 ), #59886, .T. ) ;
#6172 = CARTESIAN_POINT ( 'NONE',  ( 31.32742178679999512, 1440.913060387330006, 255.3819207742980097 ) ) ;
#6173 = B_SPLINE_SURFACE_WITH_KNOTS ( 'NONE', 5, 1, ( 
 ( #60404, #94523 ),
 ( #68815, #85566 ),
 ( #78288, #102916 ),
 ( #17797, #1602 ),
 ( #77204, #51998 ),
 ( #86138, #35182 ),
 ( #103475, #26781 ),
 ( #60969, #18360 ),
 ( #52554, #9982 ) ),
 .UNSPECIFIED., .F., .F., .F.,
 ( 6, 3, 6 ),
 ( 2, 2 ),
 ( 0.000000000000000000, 3.619946782640000027, 7.224553348539999753 ),
 ( 0.000000000000000000, 14.00000000000000000 ),
 .UNSPECIFIED. ) ;
#6174 = CARTESIAN_POINT ( 'NONE',  ( 3.439747417924114536, 1370.269341356917948, 210.1266736013298555 ) ) ;
#6175 = DIRECTION ( 'NONE',  ( -0.000000000000000000, 1.000000000000000000, -0.000000000000000000 ) ) ;
#6176 = CARTESIAN_POINT ( 'NONE',  ( -7.362157615257188148, 1458.222784178867641, 215.2209630148805104 ) ) ;
#6177 = LINE ( 'NONE', #74511, #23361 ) ;
#6178 = CARTESIAN_POINT ( 'NONE',  ( -18.15222296039999961, 1485.954920948629933, 188.9255103041979851 ) ) ;
#6179 = CARTESIAN_POINT ( 'NONE',  ( 31.92108011125350231, 1511.187213306747708, 220.9591791661896139 ) ) ;
#6180 = CARTESIAN_POINT ( 'NONE',  ( 18.64588652299999794, 1416.828040475229955, 209.6843149956849857 ) ) ;
#6181 = AXIS2_PLACEMENT_3D ( 'NONE', #52948, #36138, #2560 ) ;
#6182 = CARTESIAN_POINT ( 'NONE',  ( -20.68581318029999849, 1486.599741798989953, 210.1122336357950076 ) ) ;
#6183 = CARTESIAN_POINT ( 'NONE',  ( -21.84020450222019250, 1501.977400791986611, 234.9798068779743403 ) ) ;
#6184 = CARTESIAN_POINT ( 'NONE',  ( -113.4000000000000057, 1306.483669372790018, 304.2218459572590064 ) ) ;
#6185 = CARTESIAN_POINT ( 'NONE',  ( 12.61594199600000188, 1416.825532269230052, 223.3236178109980017 ) ) ;
#6186 = CARTESIAN_POINT ( 'NONE',  ( 11.21621798026153449, 1434.249418731722926, 151.6036331528934795 ) ) ;
#6187 = CARTESIAN_POINT ( 'NONE',  ( -9.959882553640550640, 1432.347050749440086, 152.5237167886959924 ) ) ;
#6188 = CARTESIAN_POINT ( 'NONE',  ( 14.03757890547870169, 1511.404489521279856, 234.8174622444540205 ) ) ;
#6189 = CIRCLE ( 'NONE', #31215, 1.999999999914150450 ) ;
#6190 = CARTESIAN_POINT ( 'NONE',  ( 0.2102264332707180217, 1457.221076095949911, 183.0723111843419986 ) ) ;
#6192 = EDGE_LOOP ( 'NONE', ( #12769, #72333, #88301, #56256, #29573 ) ) ;
#6191 = CARTESIAN_POINT ( 'NONE',  ( 3.350944662710000355, 1464.628126271390101, 199.8699733667390035 ) ) ;
#6193 = CARTESIAN_POINT ( 'NONE',  ( -12.93811130839999812, 1444.994950788469851, 169.4238961894979809 ) ) ;
#6194 = CARTESIAN_POINT ( 'NONE',  ( -28.74510110280450093, 1509.809709161739875, 211.3508879095350039 ) ) ;
#6195 = CARTESIAN_POINT ( 'NONE',  ( 11.87523146630000070, 1433.007068934590052, 149.1894884818979676 ) ) ;
#6196 = CARTESIAN_POINT ( 'NONE',  ( -39.90438676673540641, 1438.693166632869861, 134.0999999980629980 ) ) ;
#6197 = CARTESIAN_POINT ( 'NONE',  ( 2.980241439829999894, 1451.608296861789995, 190.1062771521989987 ) ) ;
#6198 = ORIENTED_EDGE ( 'NONE', *, *, #24711, .F. ) ;
#6199 = CARTESIAN_POINT ( 'NONE',  ( -0.7146574492519990329, 1485.443249444889943, 197.9912040296989915 ) ) ;
#6200 = DIRECTION ( 'NONE',  ( 0.1403878024439506045, 0.9900965937346509760, 0.000000000000000000 ) ) ;
#6201 = CARTESIAN_POINT ( 'NONE',  ( -103.8994048364797038, 1380.124163244008969, 306.1807731449942480 ) ) ;
#6202 = CARTESIAN_POINT ( 'NONE',  ( -11.69964062410000061, 1491.144390090590150, 207.3445954516889742 ) ) ;
#6203 = EDGE_CURVE ( 'NONE', #22181, #59085, #97210, .T. ) ;
#6204 = CARTESIAN_POINT ( 'NONE',  ( -20.92767404034479028, 1511.187213306747708, 235.3888156262297571 ) ) ;
#6205 = CARTESIAN_POINT ( 'NONE',  ( 31.98568811499627529, 1416.535344689362319, 269.3160153020001530 ) ) ;
#6206 = CARTESIAN_POINT ( 'NONE',  ( -16.91629849159999921, 1419.609072056739933, 208.4236488388899886 ) ) ;
#6207 = CARTESIAN_POINT ( 'NONE',  ( 2.472529913803023227, 1523.678648413191695, 242.8674788698241400 ) ) ;
#6208 = CARTESIAN_POINT ( 'NONE',  ( 3.906311210379999732, 1428.753781860530125, 185.1730557025980204 ) ) ;
#6209 = CARTESIAN_POINT ( 'NONE',  ( -59.88312530457670135, 1385.060781597019968, 243.7364172681270134 ) ) ;
#6210 = CARTESIAN_POINT ( 'NONE',  ( -12.23540616512669921, 1490.610661065379873, 208.3569505650620215 ) ) ;
#6211 = CARTESIAN_POINT ( 'NONE',  ( -26.79977994216764259, 1436.581364966177944, 136.7606519021615554 ) ) ;
#6212 = ORIENTED_EDGE ( 'NONE', *, *, #22433, .T. ) ;
#6213 = CARTESIAN_POINT ( 'NONE',  ( -28.86205551545040038, 1509.507027965300040, 208.7152694674689997 ) ) ;
#6214 = CARTESIAN_POINT ( 'NONE',  ( -16.29200499093240140, 1410.123450363890015, 226.4300118576410057 ) ) ;
#6216 = ORIENTED_EDGE ( 'NONE', *, *, #60493, .T. ) ;
#6215 = CARTESIAN_POINT ( 'NONE',  ( 0.5077272017738569954, 1412.024639619329946, 184.9986638035829856 ) ) ;
#6217 = CARTESIAN_POINT ( 'NONE',  ( -27.68254001883949655, 1507.989615300039986, 210.5775529569929745 ) ) ;
#6218 = CARTESIAN_POINT ( 'NONE',  ( 10.47535534418940095, 1470.915150549339842, 210.4403342155679866 ) ) ;
#6219 =( BOUNDED_CURVE ( )  B_SPLINE_CURVE ( 3, ( #76193, #110340, #33612, #67809 ),
 .UNSPECIFIED., .F., .F. ) 
 B_SPLINE_CURVE_WITH_KNOTS ( ( 4, 4 ),
 ( 0.5395807523979880838, 1.539014399141934941 ),
 .UNSPECIFIED. ) 
 CURVE ( )  GEOMETRIC_REPRESENTATION_ITEM ( )  RATIONAL_B_SPLINE_CURVE ( ( 1.000000000000000000, 0.9184788592064899726, 0.9184788592064899726, 1.000000000000000000 ) ) 
 REPRESENTATION_ITEM ( '' )  );
#6220 = CARTESIAN_POINT ( 'NONE',  ( 21.03123271209999956, 1507.789097944330024, 226.0655642189979915 ) ) ;
#6221 = CARTESIAN_POINT ( 'NONE',  ( -109.6586398049999929, 1384.698294257620091, 311.3175481042590036 ) ) ;
#6222 = DIRECTION ( 'NONE',  ( -0.02359658529091402182, 0.000000000000000000, 0.9997215618173935781 ) ) ;
#6223 = CARTESIAN_POINT ( 'NONE',  ( 0.2597461834470000119, 1465.026886499829970, 237.7737181796979939 ) ) ;
#6224 = CARTESIAN_POINT ( 'NONE',  ( 18.72649884289999989, 1410.063202272829813, 221.6652856211979952 ) ) ;
#6225 = CARTESIAN_POINT ( 'NONE',  ( -17.98886881720000019, 1424.630730734530061, 227.7167155485979890 ) ) ;
#6226 = CARTESIAN_POINT ( 'NONE',  ( -2.994327866758245804, 1512.053565093312500, 201.2273685530865919 ) ) ;
#6227 = CARTESIAN_POINT ( 'NONE',  ( -13.54126559747050074, 1379.893680670693811, 213.5390542146629684 ) ) ;
#6228 = CARTESIAN_POINT ( 'NONE',  ( -122.7580815721776446, 1314.643966242389979, 299.1095026942255686 ) ) ;
#6229 = CARTESIAN_POINT ( 'NONE',  ( 23.60905104348515593, 1509.747275849248581, 191.3746876935084060 ) ) ;
#6230 = CARTESIAN_POINT ( 'NONE',  ( -0.4792592228059999737, 1416.456888389930100, 233.6761958929980096 ) ) ;
#6231 = TOROIDAL_SURFACE ( 'NONE', #34846, 6.646318662569999702, 0.5000000000000000000 ) ;
#6232 = CARTESIAN_POINT ( 'NONE',  ( 10.02176186330000185, 1364.879735892739745, 210.6218459616991936 ) ) ;
#6233 = CARTESIAN_POINT ( 'NONE',  ( 4.610938211375000151, 1516.815231249920089, 205.0813186281270077 ) ) ;
#6234 = CARTESIAN_POINT ( 'NONE',  ( -8.629181194863379645, 1486.004047916040008, 183.3125379289229784 ) ) ;
#6235 = ORIENTED_EDGE ( 'NONE', *, *, #80260, .F. ) ;
#6236 = VECTOR ( 'NONE', #42122, 999.9999999999998863 ) ;
#6237 = CARTESIAN_POINT ( 'NONE',  ( 14.23445134770000031, 1463.710773101130144, 224.1807475960980298 ) ) ;
#6238 = CARTESIAN_POINT ( 'NONE',  ( -4.224005846046000379, 1441.584137753169898, 166.8519868219619866 ) ) ;
#6239 = VECTOR ( 'NONE', #25609, 1000.000000000000000 ) ;
#6241 = EDGE_LOOP ( 'NONE', ( #67711, #37297, #18313, #71605, #62776 ) ) ;
#6240 = CARTESIAN_POINT ( 'NONE',  ( -68.56276905719998638, 1379.747764319660064, 280.1490247721590094 ) ) ;
#6242 = ORIENTED_EDGE ( 'NONE', *, *, #109065, .T. ) ;
#6243 = CARTESIAN_POINT ( 'NONE',  ( -7.769784805680000517, 1383.283764732429972, 218.8591787099389876 ) ) ;
#6244 = ORIENTED_EDGE ( 'NONE', *, *, #52966, .T. ) ;
#6245 = CARTESIAN_POINT ( 'NONE',  ( 2.851735618451650023, 1484.953707064400078, 220.6267593247900152 ) ) ;
#6246 = EDGE_CURVE ( 'NONE', #62909, #101516, #66511, .T. ) ;
#6247 = CARTESIAN_POINT ( 'NONE',  ( -20.32611051789999834, 1410.902622711730146, 198.7319329392979910 ) ) ;
#6249 = CARTESIAN_POINT ( 'NONE',  ( 16.18216864280910272, 1410.860672406080084, 191.5684563615119771 ) ) ;
#6248 = CARTESIAN_POINT ( 'NONE',  ( -11.64413779052331854, 1425.860397285439376, 144.6913732887203992 ) ) ;
#6250 = ADVANCED_FACE ( 'NONE', ( #28659 ), #45487, .F. ) ;
#6251 = CARTESIAN_POINT ( 'NONE',  ( 4.626591867355000609, 1517.096587378560116, 210.8266407735670214 ) ) ;
#6252 = CARTESIAN_POINT ( 'NONE',  ( 37.53898081716540247, 1436.541061908490065, 135.4800556696710032 ) ) ;
#6253 = EDGE_CURVE ( 'NONE', #4626, #43885, #108696, .T. ) ;
#6254 = CARTESIAN_POINT ( 'NONE',  ( -11.73648056819999930, 1426.280364960429779, 144.1673147898980005 ) ) ;
#6255 = CYLINDRICAL_SURFACE ( 'NONE', #91173, 2.000000000000009770 ) ;
#6256 = EDGE_CURVE ( 'NONE', #56179, #94930, #89025, .T. ) ;
#6257 = CARTESIAN_POINT ( 'NONE',  ( 15.10766868565390730, 1461.886987926997563, 229.9399717845676605 ) ) ;
#6258 = APPLICATION_PROTOCOL_DEFINITION ( 'draft international standard', 'automotive_design', 1998, #34140 ) ;
#6259 = ADVANCED_FACE ( 'NONE', ( #35399 ), #44934, .T. ) ;
#6260 = CARTESIAN_POINT ( 'NONE',  ( 34.74890047445369845, 1451.658442319180040, 134.0999999982409747 ) ) ;
#6261 = CARTESIAN_POINT ( 'NONE',  ( 5.343479918049999888, 1396.099658817830004, 218.7752541424879951 ) ) ;
#6262 = CARTESIAN_POINT ( 'NONE',  ( 13.52268460260000005, 1497.923627545689897, 227.8730058995990078 ) ) ;
#6263 = CARTESIAN_POINT ( 'NONE',  ( -18.76032074160000107, 1456.949267706729870, 228.3571107660980033 ) ) ;
#6264 = ORIENTED_EDGE ( 'NONE', *, *, #50747, .T. ) ;
#6265 = ORIENTED_EDGE ( 'NONE', *, *, #94794, .T. ) ;
#6266 = EDGE_CURVE ( 'NONE', #64960, #108026, #19234, .T. ) ;
#6267 = CARTESIAN_POINT ( 'NONE',  ( 3.637353868009999935, 1426.366397907009969, 191.4055625021989897 ) ) ;
#6268 = CARTESIAN_POINT ( 'NONE',  ( -18.02257621027615642, 1526.382868172863937, 182.8951942368373977 ) ) ;
#6269 = CARTESIAN_POINT ( 'NONE',  ( 0.1579620925989999869, 1450.907544229120049, 181.8932541306980113 ) ) ;
#6270 = CARTESIAN_POINT ( 'NONE',  ( -19.38312692761750000, 1508.551704424289937, 210.1488772976939856 ) ) ;
#6271 = CARTESIAN_POINT ( 'NONE',  ( 2.330134126090001701, 1515.551704408337173, 205.1635078156689929 ) ) ;
#6272 = CARTESIAN_POINT ( 'NONE',  ( -41.14066433057620031, 1444.183247621620012, 136.8991340826939904 ) ) ;
#6273 = CARTESIAN_POINT ( 'NONE',  ( 40.71747596589879947, 1448.637563225589929, 134.7402674100779905 ) ) ;
#6274 = CARTESIAN_POINT ( 'NONE',  ( 12.78690713350000152, 1416.828040475229955, 222.7042044314979989 ) ) ;
#6275 = CIRCLE ( 'NONE', #68887, 1.999999999999999556 ) ;
#6276 = DIRECTION ( 'NONE',  ( -0.8926073982886787439, 0.000000000000000000, 0.4508348173337058951 ) ) ;
#6277 = CARTESIAN_POINT ( 'NONE',  ( -10.94175501169999976, 1391.017587509790019, 214.8528411101989661 ) ) ;
#6278 = EDGE_CURVE ( 'NONE', #50772, #11318, #43668, .T. ) ;
#6279 = CARTESIAN_POINT ( 'NONE',  ( -69.86210931808770397, 1384.736379523699952, 265.6221797416770301 ) ) ;
#6280 = ORIENTED_EDGE ( 'NONE', *, *, #25623, .T. ) ;
#6281 = CARTESIAN_POINT ( 'NONE',  ( 3.259101798884999734, 1517.102359858469754, 202.1722709844570147 ) ) ;
#6282 = CARTESIAN_POINT ( 'NONE',  ( -0.01012492377659850000, 1516.989863902050047, 207.9939175986969815 ) ) ;
#6283 = ORIENTED_EDGE ( 'NONE', *, *, #8891, .F. ) ;
#6284 = CARTESIAN_POINT ( 'NONE',  ( 41.33116270185299612, 1440.913060387330006, 268.8666020839340263 ) ) ;
#6285 = CARTESIAN_POINT ( 'NONE',  ( -0.0006570779929211399998, 1451.938362507649117, 153.9926151582928071 ) ) ;
#6286 = EDGE_LOOP ( 'NONE', ( #78337, #645, #104751, #38738 ) ) ;
#6287 = CARTESIAN_POINT ( 'NONE',  ( -17.55387852034892049, 1524.816846803860926, 180.7603862146448250 ) ) ;
#6288 = CARTESIAN_POINT ( 'NONE',  ( 7.660102788296829779, 1428.868901441670005, 214.7109318833680049 ) ) ;
#6289 = CARTESIAN_POINT ( 'NONE',  ( -18.75627164819999848, 1442.404900751590048, 208.2000273071639924 ) ) ;
#6290 = EDGE_CURVE ( 'NONE', #16710, #105489, #106925, .T. ) ;
#6291 = VECTOR ( 'NONE', #61511, 1000.000000000000114 ) ;
#6292 = LINE ( 'NONE', #5754, #20381 ) ;
#6293 = CARTESIAN_POINT ( 'NONE',  ( -4.405926214540000885, 1420.984874813729903, 186.2222319335980103 ) ) ;
#6294 = CARTESIAN_POINT ( 'NONE',  ( -6.092700172539130321, 1510.714321716110135, 201.6274141883939990 ) ) ;
#6295 = CARTESIAN_POINT ( 'NONE',  ( 2.101979435200000079, 1406.024670839530017, 266.9594151837979439 ) ) ;
#6296 = EDGE_CURVE ( 'NONE', #101169, #75664, #86348, .T. ) ;
#6297 = CARTESIAN_POINT ( 'NONE',  ( -6.054581406427221424, 1510.727597940411670, 201.6275102438071372 ) ) ;
#6299 = CARTESIAN_POINT ( 'NONE',  ( -11.60004869885203682, 1424.920234268488002, 136.4497806812309193 ) ) ;
#6298 = CARTESIAN_POINT ( 'NONE',  ( 16.43421760069999848, 1460.517322140429997, 229.1132056239979704 ) ) ;
#6300 = CARTESIAN_POINT ( 'NONE',  ( -4.479448571171882776, 1422.019686008850385, 184.5739666799692600 ) ) ;
#6301 = B_SPLINE_SURFACE_WITH_KNOTS ( 'NONE', 5, 5, ( 
 ( #19936, #96665, #79314, #37308, #36750, #4260 ),
 ( #4788, #3728, #29987, #88808, #98300, #72569 ),
 ( #79866, #46829, #54682, #71503, #53576, #63637 ),
 ( #29438, #55784, #97198, #3176, #27795, #106696 ),
 ( #80958, #28906, #97751, #64179, #88260, #87723 ),
 ( #55226, #70942, #21576, #89900, #13171, #47360 ),
 ( #63101, #37858, #72044, #28349, #12091, #38934 ),
 ( #11001, #106161, #73114, #80414, #61982, #45173 ),
 ( #105059, #62544, #91564, #92653, #22115, #90998 ) ),
 .UNSPECIFIED., .F., .F., .F.,
 ( 6, 3, 6 ),
 ( 6, 6 ),
 ( 3.061701835029610130, 6.405260106299999201, 7.456840382068469886 ),
 ( -0.0004170354784579379903, 2.000000000000000000 ),
 .UNSPECIFIED. ) ;
#6302 = CARTESIAN_POINT ( 'NONE',  ( 1.128757561074999805, 1516.608208975040043, 216.8328129478670121 ) ) ;
#6303 = ORIENTED_EDGE ( 'NONE', *, *, #22691, .T. ) ;
#6304 = ADVANCED_FACE ( 'NONE', ( #9632 ), #105111, .T. ) ;
#6305 = CARTESIAN_POINT ( 'NONE',  ( -0.8197074128579011632, 1486.333374263157339, 181.7749019119357570 ) ) ;
#6306 = CARTESIAN_POINT ( 'NONE',  ( -0.1482922428603659915, 1507.522720463130099, 180.8421728092000080 ) ) ;
#6307 = CARTESIAN_POINT ( 'NONE',  ( -113.4000000000000057, 1378.913060387289988, 304.2218459572590064 ) ) ;
#6308 = CARTESIAN_POINT ( 'NONE',  ( -0.7360974767499980365, 1517.045004075700035, 213.1642344714070134 ) ) ;
#6309 = CARTESIAN_POINT ( 'NONE',  ( 3.542288683788520132, 1515.375307391110027, 213.1422521534840087 ) ) ;
#6310 = CARTESIAN_POINT ( 'NONE',  ( 1.632486301776860348E-07, 1509.047264794319972, 239.1218459617020073 ) ) ;
#6312 = ORIENTED_EDGE ( 'NONE', *, *, #80921, .T. ) ;
#6311 = CARTESIAN_POINT ( 'NONE',  ( -12.28882577965210032, 1501.802949440490011, 211.5612507580339923 ) ) ;
#6313 = CARTESIAN_POINT ( 'NONE',  ( -2.165176160184186571, 1526.186458717538699, 177.9542909903756538 ) ) ;
#6314 = CARTESIAN_POINT ( 'NONE',  ( 25.21572900089999791, 1445.966631079429817, 221.6528564213980133 ) ) ;
#6315 = CARTESIAN_POINT ( 'NONE',  ( -11.85988639909999875, 1431.881489348090099, 150.3806999221980050 ) ) ;
#6316 = CARTESIAN_POINT ( 'NONE',  ( -3.330134203884999700, 1515.051704408389924, 204.7920544413669859 ) ) ;
#6317 = CARTESIAN_POINT ( 'NONE',  ( -4.553191091878280083, 1442.065269977319986, 201.3752770252120001 ) ) ;
#6318 = CARTESIAN_POINT ( 'NONE',  ( 3.199225641321900238, 1428.849793147289802, 155.3746604249230074 ) ) ;
#6319 = CARTESIAN_POINT ( 'NONE',  ( 20.74641727850000095, 1496.330958597389781, 205.0865742704490060 ) ) ;
#6320 = CARTESIAN_POINT ( 'NONE',  ( 12.13323926729999869, 1445.693284459350025, 187.5259842820979941 ) ) ;
#6322 = CARTESIAN_POINT ( 'NONE',  ( -3.921313488591959384, 1421.968803082632803, 139.1411894385240942 ) ) ;
#6321 = CARTESIAN_POINT ( 'NONE',  ( -22.24587359499999906, 1495.367887861130157, 224.6596000937979909 ) ) ;
#6323 = CARTESIAN_POINT ( 'NONE',  ( 6.537728378210000635, 1462.897344095490098, 208.5037906403959767 ) ) ;
#6324 = ORIENTED_EDGE ( 'NONE', *, *, #69262, .F. ) ;
#6325 = CARTESIAN_POINT ( 'NONE',  ( -1.135460355084999762, 1516.790374942449944, 205.8685445508469911 ) ) ;
#6326 = CARTESIAN_POINT ( 'NONE',  ( 14.64774519859999913, 1407.477793284829886, 267.7626194198979874 ) ) ;
#6327 = CARTESIAN_POINT ( 'NONE',  ( -0.3074737364230000214, 1409.850186678229875, 185.0722532870979933 ) ) ;
#6328 = CARTESIAN_POINT ( 'NONE',  ( -3.703568344589999839, 1497.311626104689822, 220.9591690177990131 ) ) ;
#6329 = EDGE_CURVE ( 'NONE', #37474, #77339, #10306, .T. ) ;
#6330 = CARTESIAN_POINT ( 'NONE',  ( 24.55543445757494325, 1439.121178053543872, 212.5561943058436327 ) ) ;
#6331 = AXIS2_PLACEMENT_3D ( 'NONE', #103287, #27165, #330 ) ;
#6332 = EDGE_CURVE ( 'NONE', #29958, #5600, #105800, .T. ) ;
#6333 = CARTESIAN_POINT ( 'NONE',  ( -9.068330085084843617, 1389.039739579077832, 217.5674789938883293 ) ) ;
#6334 = CARTESIAN_POINT ( 'NONE',  ( -12.94448954231350513, 1511.163060387329779, 185.4271167906579478 ) ) ;
#6335 = CARTESIAN_POINT ( 'NONE',  ( -10.29908310198690025, 1447.573334503160140, 210.1662163023220273 ) ) ;
#6336 = DIRECTION ( 'NONE',  ( -1.836970198721029688E-16, -1.000000000000000000, 0.000000000000000000 ) ) ;
#6337 = CARTESIAN_POINT ( 'NONE',  ( -12.02000798989999986, 1447.120367794319918, 187.5076484450979990 ) ) ;
#6338 = CARTESIAN_POINT ( 'NONE',  ( 2.314829377092709972, 1449.816261417490068, 155.0640813294609757 ) ) ;
#6339 = CARTESIAN_POINT ( 'NONE',  ( -14.41907353321770024, 1416.449138231110055, 221.3520838159390109 ) ) ;
#6340 = CARTESIAN_POINT ( 'NONE',  ( -10.49383960940000016, 1500.045019812190276, 215.0277856566890193 ) ) ;
#6341 = B_SPLINE_CURVE_WITH_KNOTS ( 'NONE', 5,
 ( #33615, #75658, #33077, #67812, #66174, #91887 ),
 .UNSPECIFIED., .F., .F.,
 ( 6, 6 ),
 ( 123.8981302308609997, 143.2822930469999960 ),
 .UNSPECIFIED. ) ;
#6342 = CARTESIAN_POINT ( 'NONE',  ( -9.881922048573189343, 1409.258144709340058, 197.8933969988160015 ) ) ;
#6343 = EDGE_CURVE ( 'NONE', #110657, #68857, #33541, .T. ) ;
#6344 = CARTESIAN_POINT ( 'NONE',  ( 20.59269117493390056, 1507.766073655780019, 227.7908423917359926 ) ) ;
#6345 = CARTESIAN_POINT ( 'NONE',  ( 3.140603745509999989, 1440.712167354720123, 157.0498910118980120 ) ) ;
#6346 = CARTESIAN_POINT ( 'NONE',  ( -3.774131035769999976, 1475.960033162130003, 267.5310482922980100 ) ) ;
#6347 = CARTESIAN_POINT ( 'NONE',  ( -4.238698856969680406, 1446.369308287780086, 163.0896733719079919 ) ) ;
#6348 = CARTESIAN_POINT ( 'NONE',  ( -11.80664835635214516, 1512.979863700403257, 192.6170353444451564 ) ) ;
#6349 = LINE ( 'NONE', #90901, #52146 ) ;
#6350 = CARTESIAN_POINT ( 'NONE',  ( -44.91925906889510145, 1384.764579480920020, 251.3795836030480189 ) ) ;
#6351 = CARTESIAN_POINT ( 'NONE',  ( 13.58268853708210067, 1416.851343896850040, 196.3340833727469885 ) ) ;
#6352 = CARTESIAN_POINT ( 'NONE',  ( 15.10371975099999986, 1409.440493903229935, 192.9533947891980006 ) ) ;
#6353 = CARTESIAN_POINT ( 'NONE',  ( -113.4000000000000057, 1347.163060387289988, 304.2218459572590064 ) ) ;
#6354 = CARTESIAN_POINT ( 'NONE',  ( 32.70818033930520841, 1524.201670966336224, 217.1264371928152457 ) ) ;
#6355 = CARTESIAN_POINT ( 'NONE',  ( 7.512750207965000371, 1509.038615934239942, 203.6084103740869864 ) ) ;
#6356 = CIRCLE ( 'NONE', #52821, 0.9999999999999956701 ) ;
#6357 = CARTESIAN_POINT ( 'NONE',  ( -18.50671984590000108, 1409.559329285129934, 198.4601733219979849 ) ) ;
#6358 = CARTESIAN_POINT ( 'NONE',  ( 12.91118672957320079, 1421.030139935020088, 203.7088207097539794 ) ) ;
#6359 = EDGE_CURVE ( 'NONE', #45310, #61133, #86480, .T. ) ;
#6360 = CARTESIAN_POINT ( 'NONE',  ( -6.691255413100000382, 1406.996319227029971, 269.6355722701979403 ) ) ;
#6361 = ORIENTED_EDGE ( 'NONE', *, *, #60271, .F. ) ;
#6362 = CARTESIAN_POINT ( 'NONE',  ( 31.34137657934019927, 1523.382868172864164, 221.9025654077410081 ) ) ;
#6363 = CARTESIAN_POINT ( 'NONE',  ( -13.59378551342209818, 1507.992802046239831, 209.4432269169830079 ) ) ;
#6364 = VECTOR ( 'NONE', #90126, 1000.000000000000000 ) ;
#6365 = CARTESIAN_POINT ( 'NONE',  ( -17.51543818711899902, 1417.552356043139980, 206.7803260800679936 ) ) ;
#6366 =( BOUNDED_CURVE ( )  B_SPLINE_CURVE ( 3, ( #28347, #71501, #28904, #29436 ),
 .UNSPECIFIED., .F., .F. ) 
 B_SPLINE_CURVE_WITH_KNOTS ( ( 4, 4 ),
 ( 1.971460695176299183, 2.757092281751130525 ),
 .UNSPECIFIED. ) 
 CURVE ( )  GEOMETRIC_REPRESENTATION_ITEM ( )  RATIONAL_B_SPLINE_CURVE ( ( 1.000000000000000000, 0.9492232417517829646, 0.9492232417517829646, 1.000000000000000000 ) ) 
 REPRESENTATION_ITEM ( '' )  );
#6368 = CARTESIAN_POINT ( 'NONE',  ( -12.17177947439780006, 1377.637977345770196, 211.0179508916049826 ) ) ;
#6367 = CARTESIAN_POINT ( 'NONE',  ( 10.80393815379999900, 1424.927943689529911, 143.4644770969979959 ) ) ;
#6369 = CARTESIAN_POINT ( 'NONE',  ( -15.83291935337495815, 1409.465937342200732, 225.2763755258536662 ) ) ;
#6370 = CARTESIAN_POINT ( 'NONE',  ( -14.68773312159869882, 1420.564508854909946, 212.7973254087889927 ) ) ;
#6371 = ADVANCED_FACE ( 'NONE', ( #10195 ), #48224, .T. ) ;
#6372 = CARTESIAN_POINT ( 'NONE',  ( 26.99540884559359810, 1450.681726017589881, 136.4489477893459934 ) ) ;
#6373 = CARTESIAN_POINT ( 'NONE',  ( -0.01126495432349849946, 1516.939530130779985, 202.1773791897269916 ) ) ;
#6374 = CARTESIAN_POINT ( 'NONE',  ( -8.704319915738482294, 1511.459876705991064, 214.6724670380187945 ) ) ;
#6375 = DIRECTION ( 'NONE',  ( 1.000000000000000000, 0.000000000000000000, 0.000000000000000000 ) ) ;
#6376 = CARTESIAN_POINT ( 'NONE',  ( 15.16677552193500134, 1513.509764667529907, 194.6542904276670072 ) ) ;
#6377 = CARTESIAN_POINT ( 'NONE',  ( -18.98074344019839899, 1419.205094861039925, 205.9182421121359994 ) ) ;
#6378 = CARTESIAN_POINT ( 'NONE',  ( -18.28964772222979818, 1379.850932135969970, 212.2591649744949791 ) ) ;
#6379 = CARTESIAN_POINT ( 'NONE',  ( 21.21721392852580124, 1509.704275884970230, 230.0128098300520207 ) ) ;
#6381 = ORIENTED_EDGE ( 'NONE', *, *, #92600, .F. ) ;
#6380 = CARTESIAN_POINT ( 'NONE',  ( -54.31440902440569829, 1379.704595983870149, 254.1403834083770334 ) ) ;
#6382 = ORIENTED_EDGE ( 'NONE', *, *, #9110, .F. ) ;
#6383 = CARTESIAN_POINT ( 'NONE',  ( 11.40220705808729917, 1434.449209149890066, 151.4764968396059999 ) ) ;
#6384 = CARTESIAN_POINT ( 'NONE',  ( -7.907916001329999389, 1397.529048966930077, 219.9234842523979978 ) ) ;
#6385 = CARTESIAN_POINT ( 'NONE',  ( -18.85211735460000071, 1409.571390833930081, 221.0529096949979930 ) ) ;
#6386 = ORIENTED_EDGE ( 'NONE', *, *, #46636, .T. ) ;
#6387 = CARTESIAN_POINT ( 'NONE',  ( -13.51311000297323339, 1443.997929519461877, 169.3513768787690026 ) ) ;
#6388 = EDGE_CURVE ( 'NONE', #98779, #18748, #109124, .T. ) ;
#6389 = CARTESIAN_POINT ( 'NONE',  ( -2.541451598548929826E-15, 1375.913060387289988, 209.1218459572589836 ) ) ;
#6390 = CARTESIAN_POINT ( 'NONE',  ( 15.32773529925650102, 1420.119835273649869, 210.6256678854140034 ) ) ;
#6392 = CARTESIAN_POINT ( 'NONE',  ( -13.76157194526980021, 1508.323015833239879, 184.1190294504459928 ) ) ;
#6391 = CARTESIAN_POINT ( 'NONE',  ( 35.00335893190000291, 1443.851131231850104, 135.3147355765980251 ) ) ;
#6393 = B_SPLINE_CURVE_WITH_KNOTS ( 'NONE', 3,
 ( #84558, #7847, #110312, #33587, #101892, #68345 ),
 .UNSPECIFIED., .F., .F.,
 ( 4, 2, 4 ),
 ( 0.000000000000000000, 0.4987707156545279630, 0.9977421829108459317 ),
 .UNSPECIFIED. ) ;
#6394 = CARTESIAN_POINT ( 'NONE',  ( 0.1761655985929999890, 1468.710735116929982, 182.5349289889980184 ) ) ;
#6395 = ADVANCED_FACE ( 'NONE', ( #72870 ), #42899, .T. ) ;
#6396 = CARTESIAN_POINT ( 'NONE',  ( -3.509040552655700029, 1464.225060470080052, 199.5119554303080065 ) ) ;
#6397 = CARTESIAN_POINT ( 'NONE',  ( 42.85031101989900293, 1440.913053629049955, 270.2009481551980343 ) ) ;
#6398 = SHAPE_REPRESENTATION_RELATIONSHIP ( 'NONE' , 'NONE' ,  #10812, #13206 ) ;
#6399 = CARTESIAN_POINT ( 'NONE',  ( 10.62399481180199956, 1396.284058461849781, 206.0104454596539938 ) ) ;
#6400 = CARTESIAN_POINT ( 'NONE',  ( 2.500000000000000000, 1419.401689857129895, 143.2540567177979938 ) ) ;
#6401 = CARTESIAN_POINT ( 'NONE',  ( 11.50749625859999981, 1427.423291567529986, 149.3076215910979840 ) ) ;
#6402 = CARTESIAN_POINT ( 'NONE',  ( 8.297002879045001222, 1511.752511073100095, 203.0778258940270007 ) ) ;
#6403 = EDGE_LOOP ( 'NONE', ( #42198, #100667, #76778, #6422 ) ) ;
#6404 = CARTESIAN_POINT ( 'NONE',  ( 13.11477892927669942, 1435.900992455230153, 150.6555893957250021 ) ) ;
#6405 = ORIENTED_EDGE ( 'NONE', *, *, #9651, .T. ) ;
#6406 = VERTEX_POINT ( 'NONE', #38152 ) ;
#6407 = EDGE_CURVE ( 'NONE', #34770, #20056, #82557, .T. ) ;
#6408 = CARTESIAN_POINT ( 'NONE',  ( -18.42347945445600033, 1478.095089849470014, 228.7109761469720013 ) ) ;
#6409 = CARTESIAN_POINT ( 'NONE',  ( -12.96438286449999922, 1461.237399744029972, 232.5537136377980119 ) ) ;
#6410 = CARTESIAN_POINT ( 'NONE',  ( -109.5086524770909762, 1386.853415303551856, 311.1534610470823168 ) ) ;
#6411 = CARTESIAN_POINT ( 'NONE',  ( 2.292940169014999974, 1516.565291103010168, 215.6678853655270132 ) ) ;
#6412 = CARTESIAN_POINT ( 'NONE',  ( -14.53481814003150063, 1379.710746619959991, 208.2793821099419915 ) ) ;
#6413 = ADVANCED_FACE ( 'NONE', ( #46581 ), #72905, .T. ) ;
#6414 = ADVANCED_FACE ( 'NONE', ( #80715 ), #48780, .T. ) ;
#6415 = EDGE_LOOP ( 'NONE', ( #96, #24588, #23195, #31135 ) ) ;
#6416 = CARTESIAN_POINT ( 'NONE',  ( -11.62340356170000000, 1502.516964898590004, 208.1148589984090052 ) ) ;
#6417 = CARTESIAN_POINT ( 'NONE',  ( 6.445219222570445439, 1513.425324099854834, 201.4942069324724514 ) ) ;
#6418 = CARTESIAN_POINT ( 'NONE',  ( -51.56180980459999574, 1379.702544246149955, 241.8087128069590221 ) ) ;
#6419 = VECTOR ( 'NONE', #67422, 1000.000000000000000 ) ;
#6420 = ORIENTED_EDGE ( 'NONE', *, *, #107298, .T. ) ;
#6421 = CARTESIAN_POINT ( 'NONE',  ( 4.028630584655000568, 1516.812923327049930, 205.6617440802170051 ) ) ;
#6422 = ORIENTED_EDGE ( 'NONE', *, *, #25350, .F. ) ;
#6423 = CARTESIAN_POINT ( 'NONE',  ( 7.719640903004999721, 1516.939452820819952, 209.1117431028050078 ) ) ;
#6424 = CARTESIAN_POINT ( 'NONE',  ( -7.156442445803939734, 1453.513166831520039, 203.0923578546739918 ) ) ;
#6425 = CARTESIAN_POINT ( 'NONE',  ( -35.09211443864747793, 1424.151985311556473, 269.5327834166636194 ) ) ;
#6426 = CARTESIAN_POINT ( 'NONE',  ( 6.658917431355000360, 1512.371207877119787, 217.3544136925769976 ) ) ;
#6428 = ORIENTED_EDGE ( 'NONE', *, *, #31071, .T. ) ;
#6427 = CARTESIAN_POINT ( 'NONE',  ( -1.027470347570780040, 1414.913060387399810, 225.5111429998570145 ) ) ;
#6429 = CARTESIAN_POINT ( 'NONE',  ( -0.008271327469596450460, 1451.342692138500297, 182.5054642300370062 ) ) ;
#6430 = CARTESIAN_POINT ( 'NONE',  ( -28.38246044266520229, 1440.913060387269979, 232.6696485458210191 ) ) ;
#6431 = CARTESIAN_POINT ( 'NONE',  ( -36.11870846930000312, 1384.478883252080095, 235.4680142451589973 ) ) ;
#6432 = CARTESIAN_POINT ( 'NONE',  ( -0.2944423246913550063, 1465.427648891259878, 236.3065114702050096 ) ) ;
#6433 = CARTESIAN_POINT ( 'NONE',  ( 6.198203255362690456, 1410.719740469389990, 269.3394747697590219 ) ) ;
#6434 = EDGE_CURVE ( 'NONE', #19317, #36910, #47879, .T. ) ;
#6435 = CARTESIAN_POINT ( 'NONE',  ( 7.334328272665000092, 1517.005755693489846, 214.1256940922069987 ) ) ;
#6436 = CARTESIAN_POINT ( 'NONE',  ( 23.02287022260000171, 1409.743200923030145, 209.1790448026619913 ) ) ;
#6437 = CARTESIAN_POINT ( 'NONE',  ( 29.30029655192928928, 1525.907212628473644, 196.8717316207784620 ) ) ;
#6438 = CARTESIAN_POINT ( 'NONE',  ( -156.6846457583352503, 1524.382868172863937, 77.25240589482224607 ) ) ;
#6440 = CARTESIAN_POINT ( 'NONE',  ( -7.709297277558810890, 1516.544444245480008, 210.8523772776020166 ) ) ;
#6439 = CIRCLE ( 'NONE', #52895, 1.999998160074185627 ) ;
#6441 = CARTESIAN_POINT ( 'NONE',  ( -0.7352271553329990939, 1516.963431999339946, 210.8369554172870153 ) ) ;
#6442 = CARTESIAN_POINT ( 'NONE',  ( 9.788553136239070085, 1435.243871060430138, 208.4607419252359932 ) ) ;
#6443 = CARTESIAN_POINT ( 'NONE',  ( 0.1409679171009999843, 1419.780819256630139, 184.3745687884979816 ) ) ;
#6444 = DIRECTION ( 'NONE',  ( 0.000000000000000000, 0.8286769424886414326, -0.5597271880011518430 ) ) ;
#6446 = VERTEX_POINT ( 'NONE', #15668 ) ;
#6445 = CARTESIAN_POINT ( 'NONE',  ( -64.47258353809999676, 1386.692755172200123, 254.0625783103589868 ) ) ;
#6447 = CARTESIAN_POINT ( 'NONE',  ( -43.14998543848509627, 1385.163626048319884, 247.9000986097850046 ) ) ;
#6448 = CARTESIAN_POINT ( 'NONE',  ( 31.34137657934008558, 1523.382868172864164, 196.3411265156547358 ) ) ;
#6449 = CARTESIAN_POINT ( 'NONE',  ( -3.180365954794715400, 1370.226539215816501, 210.2066197577219100 ) ) ;
#6450 = CARTESIAN_POINT ( 'NONE',  ( 2.562340869413348265, 1517.051704408389924, 221.9545077427458182 ) ) ;
#6451 = CARTESIAN_POINT ( 'NONE',  ( 6.554685473989913191, 1473.611172115990030, 218.5142022801588553 ) ) ;
#6452 = CARTESIAN_POINT ( 'NONE',  ( 12.23498997169999924, 1421.239601672929894, 203.4474965640889934 ) ) ;
#6453 = CARTESIAN_POINT ( 'NONE',  ( -2.214263094331805348, 1497.815544588951980, 198.0520811483251293 ) ) ;
#6455 = CARTESIAN_POINT ( 'NONE',  ( -19.53786426059057746, 1511.187213306747708, 181.5239794925695946 ) ) ;
#6454 = CARTESIAN_POINT ( 'NONE',  ( 2.292307230374999616, 1516.548716157039962, 216.0554627912370051 ) ) ;
#6456 = CARTESIAN_POINT ( 'NONE',  ( -15.27152961130000008, 1506.433683729329914, 224.9338604266980326 ) ) ;
#6457 = CARTESIAN_POINT ( 'NONE',  ( 29.78220350812352990, 1526.382868172863709, 221.7347658002323953 ) ) ;
#6458 = EDGE_LOOP ( 'NONE', ( #60135, #15344, #107470, #40291, #89219, #32445 ) ) ;
#6459 = CARTESIAN_POINT ( 'NONE',  ( 7.715625202974999652, 1516.786099423779888, 202.5670817708370066 ) ) ;
#6460 = CARTESIAN_POINT ( 'NONE',  ( -16.76527324706500011, 1513.875858217480072, 222.9845539743670031 ) ) ;
#6461 = CARTESIAN_POINT ( 'NONE',  ( 5.513435558014999849, 1509.038615934239942, 216.6345961781970288 ) ) ;
#6462 = CARTESIAN_POINT ( 'NONE',  ( 21.97919311359999739, 1451.781877468529956, 220.8331905986980246 ) ) ;
#6463 = CARTESIAN_POINT ( 'NONE',  ( 10.90371891546730154, 1461.552474635850103, 210.3079516580219774 ) ) ;
#6464 = CARTESIAN_POINT ( 'NONE',  ( 8.297169622465377259, 1424.294093603346710, 195.8426830675071244 ) ) ;
#6465 = CARTESIAN_POINT ( 'NONE',  ( 4.639337580630000346, 1465.928856497889910, 219.1434977748990036 ) ) ;
#6466 = CARTESIAN_POINT ( 'NONE',  ( 9.442266983135132463, 1417.594392525823650, 230.3524224733923802 ) ) ;
#6467 = CARTESIAN_POINT ( 'NONE',  ( 39.47629592728779357, 1446.978162307669891, 136.6467521598829649 ) ) ;
#6468 = CARTESIAN_POINT ( 'NONE',  ( -19.53850950879999715, 1426.169861875230026, 223.3587345906979920 ) ) ;
#6469 = CARTESIAN_POINT ( 'NONE',  ( -23.03159172119999809, 1435.301732086840275, 138.5817198000980000 ) ) ;
#6470 = CARTESIAN_POINT ( 'NONE',  ( -104.5812090319999896, 1389.496436508050010, 300.7817575048589447 ) ) ;
#6471 = CARTESIAN_POINT ( 'NONE',  ( 13.70990347210000060, 1507.817794156229866, 185.7059265823980070 ) ) ;
#6472 = CARTESIAN_POINT ( 'NONE',  ( -105.6984031270000060, 1391.691901357969982, 303.4437319069589876 ) ) ;
#6473 = CARTESIAN_POINT ( 'NONE',  ( 8.410267065803780360E-17, 1471.436294031830130, 269.3346704751489824 ) ) ;
#6474 = EDGE_LOOP ( 'NONE', ( #65988, #17906, #105704, #13012, #63697 ) ) ;
#6475 = CARTESIAN_POINT ( 'NONE',  ( 2.446787376320000096, 1432.353341358199941, 150.2884730787980061 ) ) ;
#6476 = CARTESIAN_POINT ( 'NONE',  ( -42.13563646669874885, 1427.775737239709770, 269.0721146450511583 ) ) ;
#6477 = CARTESIAN_POINT ( 'NONE',  ( 9.799878764200000703, 1423.431745859970079, 209.4822081458350169 ) ) ;
#6478 = CARTESIAN_POINT ( 'NONE',  ( -10.03739716579999808, 1408.913060387329779, 223.8190696839980092 ) ) ;
#6479 = CARTESIAN_POINT ( 'NONE',  ( -15.52964687406499955, 1451.324136384999974, 222.4830579234560162 ) ) ;
#6480 = CARTESIAN_POINT ( 'NONE',  ( -12.78293219662820057, 1442.837713915257837, 186.2730944851466575 ) ) ;
#6481 = CARTESIAN_POINT ( 'NONE',  ( -9.905282292037359326, 1438.748818913890091, 210.0876870654180095 ) ) ;
#6482 = CARTESIAN_POINT ( 'NONE',  ( 11.86629848900230044, 1432.349867578880094, 149.9824231379060109 ) ) ;
#6483 = CARTESIAN_POINT ( 'NONE',  ( -0.4967073565345429542, 1415.438070636819930, 233.3911243540180180 ) ) ;
#6484 = CARTESIAN_POINT ( 'NONE',  ( -14.16774589291680009, 1415.677402201999939, 204.4588472394289624 ) ) ;
#6485 = CARTESIAN_POINT ( 'NONE',  ( 32.86802468386292730, 1523.382868172864164, 217.2040256693915410 ) ) ;
#6486 = CARTESIAN_POINT ( 'NONE',  ( -12.68854658940551339, 1442.806680916267851, 169.4609767598299470 ) ) ;
#6488 = ORIENTED_EDGE ( 'NONE', *, *, #15968, .T. ) ;
#6487 = CARTESIAN_POINT ( 'NONE',  ( 18.80462376713409967, 1425.802750969149884, 225.5973978925190124 ) ) ;
#6489 = ADVANCED_FACE ( 'NONE', ( #25185 ), #908, .F. ) ;
#6490 = CARTESIAN_POINT ( 'NONE',  ( 1.457047359303009992, 1414.913057819779851, 191.9717114511999796 ) ) ;
#6491 = CARTESIAN_POINT ( 'NONE',  ( -3.314356077729999406, 1409.028800251930079, 230.9273595247980211 ) ) ;
#6492 = VERTEX_POINT ( 'NONE', #15131 ) ;
#6493 = ORIENTED_EDGE ( 'NONE', *, *, #49415, .T. ) ;
#6494 = CARTESIAN_POINT ( 'NONE',  ( 18.09118544614330304, 1416.225364278609959, 209.2081609163089979 ) ) ;
#6495 = CARTESIAN_POINT ( 'NONE',  ( -19.30300490007669367, 1526.348417187222140, 233.1578084719505171 ) ) ;
#6497 = CARTESIAN_POINT ( 'NONE',  ( -25.01541332120000050, 1440.913060508280068, 216.4497915762179900 ) ) ;
#6496 = CARTESIAN_POINT ( 'NONE',  ( -11.65615920360559699, 1428.981702016564896, 138.1374390033664383 ) ) ;
#6498 = CARTESIAN_POINT ( 'NONE',  ( -2.391931473960000165, 1445.002411567389800, 217.8135387986989997 ) ) ;
#6499 = CARTESIAN_POINT ( 'NONE',  ( -11.19195527129999945, 1433.382885624610026, 151.6055787587979751 ) ) ;
#6500 = DIRECTION ( 'NONE',  ( 0.000000000000000000, 0.000000000000000000, 1.000000000000000000 ) ) ;
#6501 = CARTESIAN_POINT ( 'NONE',  ( 25.71166857904860237, 1449.089649366449976, 209.5200665649139751 ) ) ;
#6502 = CARTESIAN_POINT ( 'NONE',  ( -25.20182348799999872, 1437.586142492700219, 138.0414809568979990 ) ) ;
#6503 = CARTESIAN_POINT ( 'NONE',  ( -14.06820649347891283, 1429.461423307730911, 222.2989188825169151 ) ) ;
#6504 = CARTESIAN_POINT ( 'NONE',  ( -3.857685964098449993, 1453.986003452039995, 199.3820233995429874 ) ) ;
#6505 = CARTESIAN_POINT ( 'NONE',  ( 2.325461800109999810, 1451.292411637130044, 183.5656961689980164 ) ) ;
#6506 = CARTESIAN_POINT ( 'NONE',  ( 9.093835586159539019, 1363.023136421986010, 210.6218459616987957 ) ) ;
#6507 = CARTESIAN_POINT ( 'NONE',  ( -29.04773278458495156, 1510.038324495063989, 216.6204971033638458 ) ) ;
#6508 = AXIS2_PLACEMENT_3D ( 'NONE', #33420, #75996, #67617 ) ;
#6510 = VERTEX_POINT ( 'NONE', #25737 ) ;
#6509 = DIRECTION ( 'NONE',  ( -1.224646799147350002E-16, 1.836970198721029688E-16, 1.000000000000000000 ) ) ;
#6511 = EDGE_LOOP ( 'NONE', ( #88904, #102526, #2843, #100300, #31212, #65315, #24732, #81040, #110198, #45270, #29478, #100457, #15424, #79597 ) ) ;
#6512 = CONICAL_SURFACE ( 'NONE', #45861, 1.000000000000005773, 0.7853981633970000820 ) ;
#6513 = CARTESIAN_POINT ( 'NONE',  ( -11.79189761063040010, 1427.869643660999827, 147.7507972342360176 ) ) ;
#6514 = CARTESIAN_POINT ( 'NONE',  ( 19.17904245640259830, 1497.230174812279984, 221.9978027818679891 ) ) ;
#6515 = CARTESIAN_POINT ( 'NONE',  ( -7.260537799720000685, 1471.133396844229992, 269.6205813391980541 ) ) ;
#6516 = CARTESIAN_POINT ( 'NONE',  ( -110.0636332773229924, 1384.926148836659877, 296.9511394268049571 ) ) ;
#6517 = CARTESIAN_POINT ( 'NONE',  ( -130.6584559203111269, 1340.114449826969121, 299.8150386652596353 ) ) ;
#6518 = CARTESIAN_POINT ( 'NONE',  ( 36.71369698479820443, 1450.233298359589753, 136.1820598115060079 ) ) ;
#6519 = CARTESIAN_POINT ( 'NONE',  ( 10.70848634212536865, 1506.855035729306792, 228.7236287190453936 ) ) ;
#6520 = EDGE_CURVE ( 'NONE', #59778, #88595, #51471, .T. ) ;
#6521 = CARTESIAN_POINT ( 'NONE',  ( -20.59722728060000208, 1484.571346146590031, 210.1121776662889999 ) ) ;
#6522 = CARTESIAN_POINT ( 'NONE',  ( 18.27180342219620002, 1431.618699553079978, 208.4181533866990037 ) ) ;
#6523 = CARTESIAN_POINT ( 'NONE',  ( -3.597719018270000291, 1458.022133392390060, 218.7636985456790057 ) ) ;
#6524 = CARTESIAN_POINT ( 'NONE',  ( 11.17471672580117925, 1365.463530159558559, 210.6218459617030021 ) ) ;
#6525 = CARTESIAN_POINT ( 'NONE',  ( -27.32593768275089730, 1412.870037644089962, 266.6661490471050229 ) ) ;
#6526 = AXIS2_PLACEMENT_3D ( 'NONE', #23608, #32574, #24142 ) ;
#6527 = EDGE_CURVE ( 'NONE', #96120, #48466, #17462, .T. ) ;
#6528 = ORIENTED_EDGE ( 'NONE', *, *, #97271, .T. ) ;
#6529 = CARTESIAN_POINT ( 'NONE',  ( -4.328142686769930414, 1515.114670419599861, 210.0487672904759791 ) ) ;
#6530 = ORIENTED_EDGE ( 'NONE', *, *, #61639, .T. ) ;
#6531 = ORIENTED_EDGE ( 'NONE', *, *, #24347, .F. ) ;
#6532 = CARTESIAN_POINT ( 'NONE',  ( 7.725990161824999980, 1517.181921232829836, 211.6070516194370157 ) ) ;
#6533 = ADVANCED_FACE ( 'NONE', ( #41472, #101331 ), #24621, .F. ) ;
#6534 = CARTESIAN_POINT ( 'NONE',  ( 38.51619765980534993, 1444.740067931809790, 136.9081133514089288 ) ) ;
#6535 = CARTESIAN_POINT ( 'NONE',  ( 8.854488364011938728, 1425.207168016459946, 194.9722730769710211 ) ) ;
#6537 = DIRECTION ( 'NONE',  ( 5.980589973904019347E-17, -1.000000000000000000, 1.736889445713099699E-16 ) ) ;
#6536 = CARTESIAN_POINT ( 'NONE',  ( 1.135185044044999980, 1516.778853242349896, 212.5689744308569971 ) ) ;
#6538 = CARTESIAN_POINT ( 'NONE',  ( -18.34539076389999934, 1455.459263898130075, 190.6407490677979979 ) ) ;
#6539 = EDGE_CURVE ( 'NONE', #47514, #19483, #6393, .T. ) ;
#6540 = CARTESIAN_POINT ( 'NONE',  ( 2.175409717514719593E-31, 1397.551704408390151, 209.1218459616989946 ) ) ;
#6541 = ORIENTED_EDGE ( 'NONE', *, *, #93928, .F. ) ;
#6542 = CARTESIAN_POINT ( 'NONE',  ( -26.29952725040000061, 1435.947996908099867, 136.5136938088979832 ) ) ;
#6543 =( BOUNDED_SURFACE ( )  B_SPLINE_SURFACE ( 4, 2, ( 
 ( #68361, #15685, #60504, #24639, #102467, #58837, #42581 ),
 ( #596, #92972, #76733, #33604, #94627, #84023, #43688 ),
 ( #110332, #45, #25757, #17341, #69465, #16245, #49891 ),
 ( #84574, #51536, #68915, #7866, #67800, #101909, #59404 ),
 ( #93516, #35841, #96859, #12273, #80043, #104689, #95740 ) ),
 .UNSPECIFIED., .F., .F., .F. ) 
 B_SPLINE_SURFACE_WITH_KNOTS ( ( 5, 5 ),
 ( 3, 2, 2, 3 ),
 ( 1.967616199060000071, 3.613988937050000239 ),
 ( 11.46118682297159985, 11.46128530315550087, 12.56637061435916003, 12.57442343279920038 ),
 .UNSPECIFIED. ) 
 GEOMETRIC_REPRESENTATION_ITEM ( )  RATIONAL_B_SPLINE_SURFACE ( (
 ( 0.8778316440755170591, 0.8778241674203509648, 0.8778166930676719604, 0.7939440089458740246, 1.000000000000000000, 0.9984984584740950186, 0.9970123125040389889),
 ( 0.8778316440755170591, 0.8778241674203509648, 0.8778166930676719604, 0.7939440089458740246, 1.000000000000000000, 0.9984984584740950186, 0.9970123125040389889),
 ( 0.8778316440755170591, 0.8778241674203509648, 0.8778166930676719604, 0.7939440089458740246, 1.000000000000000000, 0.9984984584740950186, 0.9970123125040389889),
 ( 0.8778316440755170591, 0.8778241674203509648, 0.8778166930676719604, 0.7939440089458740246, 1.000000000000000000, 0.9984984584740950186, 0.9970123125040389889),
 ( 0.8778316440755170591, 0.8778241674203509648, 0.8778166930676719604, 0.7939440089458740246, 1.000000000000000000, 0.9984984584740950186, 0.9970123125040389889) ) ) 
 REPRESENTATION_ITEM ( '' )  SURFACE ( )  );
#6544 = B_SPLINE_CURVE_WITH_KNOTS ( 'NONE', 3,
 ( #52853, #18108, #78028, #1336, #61274, #44446, #45565, #78590, #79706, #36044, #27630, #19199, #61816, #53401, #87552, #10840 ),
 .UNSPECIFIED., .F., .F.,
 ( 4, 3, 3, 3, 3, 4 ),
 ( -14.84820554333979992, -14.42705417563930048, -13.45967978722200087, -12.49597291703340041, -11.53390232449759978, -10.57397516620000033 ),
 .UNSPECIFIED. ) ;
#6545 = CARTESIAN_POINT ( 'NONE',  ( -6.556022232634999725, 1516.833525648419936, 202.1813725979570222 ) ) ;
#6546 = CARTESIAN_POINT ( 'NONE',  ( 1.546869376546317509, 1416.835807149388984, 190.2224235154945404 ) ) ;
#6547 = CARTESIAN_POINT ( 'NONE',  ( -48.74781190723079760, 1384.614220091390052, 223.3886898673410144 ) ) ;
#6548 = CARTESIAN_POINT ( 'NONE',  ( -33.44468239324360326, 1421.725958844539946, 269.5026010579289846 ) ) ;
#6549 = DIRECTION ( 'NONE',  ( 0.000000000000000000, 0.000000000000000000, 1.000000000000000000 ) ) ;
#6550 = CARTESIAN_POINT ( 'NONE',  ( -5.086423039969999671, 1397.753029223729982, 197.0860517657980040 ) ) ;
#6552 = ORIENTED_EDGE ( 'NONE', *, *, #48270, .F. ) ;
#6551 = FACE_OUTER_BOUND ( 'NONE', #65063, .T. ) ;
#6553 = ORIENTED_EDGE ( 'NONE', *, *, #89960, .T. ) ;
#6554 = CARTESIAN_POINT ( 'NONE',  ( -11.86629850686009924, 1432.349867577580198, 149.9824227077560010 ) ) ;
#6555 = CARTESIAN_POINT ( 'NONE',  ( 3.246772394788723481, 1511.187213306747708, 241.0944358625217774 ) ) ;
#6556 = CARTESIAN_POINT ( 'NONE',  ( -14.17772861730700207, 1379.591530685439920, 207.8208986668599891 ) ) ;
#6557 = CARTESIAN_POINT ( 'NONE',  ( -23.69417716570000110, 1435.324924696049948, 137.3225688245979654 ) ) ;
#6558 = CARTESIAN_POINT ( 'NONE',  ( -24.37286542989999916, 1441.888782162479856, 211.3878437502879990 ) ) ;
#6559 = EDGE_CURVE ( 'NONE', #18694, #34842, #10344, .T. ) ;
#6560 = CARTESIAN_POINT ( 'NONE',  ( -6.546001388695000145, 1516.557392317769882, 210.8318505190270002 ) ) ;
#6561 = CARTESIAN_POINT ( 'NONE',  ( -68.78255321330000527, 1379.747970357369923, 280.2961343352589552 ) ) ;
#6562 = CARTESIAN_POINT ( 'NONE',  ( -2.825590008402790065, 1484.262936871399916, 183.3074027492610298 ) ) ;
#6563 = AXIS2_PLACEMENT_3D ( 'NONE', #30992, #38288, #90337 ) ;
#6564 = CARTESIAN_POINT ( 'NONE',  ( 9.377625631454941768, 1436.953526060589866, 212.2519149868810189 ) ) ;
#6565 = CARTESIAN_POINT ( 'NONE',  ( 3.034663161748390348, 1440.440203176670138, 157.2490260270419924 ) ) ;
#6566 = CARTESIAN_POINT ( 'NONE',  ( 7.321169230994999388, 1516.531533746980131, 207.4131249475269954 ) ) ;
#6567 = ADVANCED_FACE ( 'NONE', ( #79489 ), #77777, .F. ) ;
#6568 = ORIENTED_EDGE ( 'NONE', *, *, #83590, .T. ) ;
#6569 = CARTESIAN_POINT ( 'NONE',  ( -33.91369117178599879, 1435.681798755369982, 134.4203392960459951 ) ) ;
#6570 = CARTESIAN_POINT ( 'NONE',  ( -9.978326636743720002, 1439.380423524790103, 208.6695145202539834 ) ) ;
#6571 =( BOUNDED_CURVE ( )  B_SPLINE_CURVE ( 3, ( #57163, #58252, #16206, #92373 ),
 .UNSPECIFIED., .F., .T. ) 
 B_SPLINE_CURVE_WITH_KNOTS ( ( 4, 4 ),
 ( 5.307843187739740287, 5.956424869281669920 ),
 .UNSPECIFIED. ) 
 CURVE ( )  GEOMETRIC_REPRESENTATION_ITEM ( )  RATIONAL_B_SPLINE_CURVE ( ( 1.000000000000000000, 0.9652512859188302485, 0.9652512859188302485, 1.000000000000000000 ) ) 
 REPRESENTATION_ITEM ( '' )  );
#6572 = FACE_OUTER_BOUND ( 'NONE', #78820, .T. ) ;
#6573 = ORIENTED_EDGE ( 'NONE', *, *, #60296, .T. ) ;
#6574 = CARTESIAN_POINT ( 'NONE',  ( 21.83550407203921040, 1523.678648413191695, 234.9693198511251069 ) ) ;
#6575 = CARTESIAN_POINT ( 'NONE',  ( 13.01189198590000018, 1435.390145910219871, 150.4640032787939958 ) ) ;
#6576 = CARTESIAN_POINT ( 'NONE',  ( 14.15566883900000050, 1416.254459047329874, 196.5762094978979917 ) ) ;
#6577 = CARTESIAN_POINT ( 'NONE',  ( 17.55898010899999662, 1488.218443485430043, 189.1283882809980241 ) ) ;
#6578 = CARTESIAN_POINT ( 'NONE',  ( -11.44789780662239664, 1425.801310437136181, 139.0691777563419578 ) ) ;
#6579 = CARTESIAN_POINT ( 'NONE',  ( 3.933438035067677863, 1449.506699156169361, 184.2458349000845601 ) ) ;
#6580 = CARTESIAN_POINT ( 'NONE',  ( 5.281945572889999774, 1487.428016119789845, 199.2096035253390198 ) ) ;
#6581 = DIRECTION ( 'NONE',  ( -0.4794255386041976763, 8.806904269216897590E-17, 0.8775825618903756453 ) ) ;
#6582 = CARTESIAN_POINT ( 'NONE',  ( 24.58878164341058792, 1443.302558083091526, 213.0807573783872613 ) ) ;
#6583 = CARTESIAN_POINT ( 'NONE',  ( 41.66793168306197259, 1443.219043443782311, 135.6262769008947089 ) ) ;
#6584 = CARTESIAN_POINT ( 'NONE',  ( -1.835536242490369840, 1450.383119622699951, 182.7750508701979868 ) ) ;
#6585 = CARTESIAN_POINT ( 'NONE',  ( -2.483949978725000118, 1517.156142772249950, 216.0726795003369887 ) ) ;
#6586 = ORIENTED_EDGE ( 'NONE', *, *, #79455, .T. ) ;
#6587 = CARTESIAN_POINT ( 'NONE',  ( 7.718696897759629749, 1516.903402714960066, 209.0140334714870107 ) ) ;
#6588 = CARTESIAN_POINT ( 'NONE',  ( -16.87841318179999917, 1420.387307786450037, 203.7287732364889905 ) ) ;
#6589 = CARTESIAN_POINT ( 'NONE',  ( -16.36323254953610373, 1508.551704408389924, 213.3980841489470208 ) ) ;
#6590 = CARTESIAN_POINT ( 'NONE',  ( -2.119623532050000314, 1475.831458439090056, 219.9786267809990079 ) ) ;
#6591 = CARTESIAN_POINT ( 'NONE',  ( 21.84020450222037724, 1501.977400791986611, 183.2638850454218016 ) ) ;
#6592 = CARTESIAN_POINT ( 'NONE',  ( 9.803834995107230554, 1517.151704408390060, 221.6221720662910002 ) ) ;
#6593 = CARTESIAN_POINT ( 'NONE',  ( 1.810458008787178885, 1416.704060343818810, 232.7176022638104200 ) ) ;
#6594 = CARTESIAN_POINT ( 'NONE',  ( 17.47617717604931542, 1422.886529812959225, 226.4807061310582128 ) ) ;
#6595 = CARTESIAN_POINT ( 'NONE',  ( -1.615118886346869953, 1455.072079523880120, 198.7395845362720195 ) ) ;
#6596 = CARTESIAN_POINT ( 'NONE',  ( 0.000000000000000000, 1523.382868172864164, 209.1218459616979999 ) ) ;
#6597 = CARTESIAN_POINT ( 'NONE',  ( 35.65332322675680388, 1440.913060386850020, 252.2033051962219758 ) ) ;
#6599 = LINE ( 'NONE', #101185, #90869 ) ;
#6598 = CARTESIAN_POINT ( 'NONE',  ( -11.01233496866419870, 1470.178673701140042, 211.9709904787150094 ) ) ;
#6600 = CARTESIAN_POINT ( 'NONE',  ( 13.07088740030000018, 1426.021987528729824, 222.4234160755980270 ) ) ;
#6601 = ORIENTED_EDGE ( 'NONE', *, *, #42077, .F. ) ;
#6602 = VERTEX_POINT ( 'NONE', #79848 ) ;
#6603 = DIRECTION ( 'NONE',  ( 0.000000000000000000, 1.000000000000000000, 0.000000000000000000 ) ) ;
#6604 = CARTESIAN_POINT ( 'NONE',  ( -4.958564224928870168, 1476.141795758730041, 200.0452580833139962 ) ) ;
#6605 = CIRCLE ( 'NONE', #72803, 3.000000000000002665 ) ;
#6606 = CARTESIAN_POINT ( 'NONE',  ( 16.06428792994640276, 1414.913060387329779, 208.9262477894010033 ) ) ;
#6607 = CARTESIAN_POINT ( 'NONE',  ( 11.41298749625700104, 1502.480512559349791, 211.2134296033459862 ) ) ;
#6608 = CARTESIAN_POINT ( 'NONE',  ( -762.4595216451192528, -8387.357407334291565, -1619.875998970129785 ) ) ;
#6609 = DIRECTION ( 'NONE',  ( 0.000000000000000000, 0.000000000000000000, 1.000000000000000000 ) ) ;
#6610 = CARTESIAN_POINT ( 'NONE',  ( 1.289688745822530125, 1508.551704408389924, 219.8224770426249677 ) ) ;
#6611 = CARTESIAN_POINT ( 'NONE',  ( -42.25319127006149955, 1383.824624454990044, 245.8538586339880112 ) ) ;
#6612 = CARTESIAN_POINT ( 'NONE',  ( -3.853756162035000266, 1510.775363762149937, 201.5636160667770014 ) ) ;
#6613 = CARTESIAN_POINT ( 'NONE',  ( 24.63041548480000031, 1451.910759679029979, 137.3284484590980128 ) ) ;
#6614 = DIRECTION ( 'NONE',  ( -0.8907681516580507886, 0.000000000000000000, 0.4544580288560209347 ) ) ;
#6615 = CARTESIAN_POINT ( 'NONE',  ( 10.96547367623530000, 1490.901970238939839, 209.8192269860039971 ) ) ;
#6617 = EDGE_LOOP ( 'NONE', ( #84907, #22921 ) ) ;
#6616 = CARTESIAN_POINT ( 'NONE',  ( -14.11150871393421724, 1517.034034075904401, 226.0802419627609368 ) ) ;
#6618 = CARTESIAN_POINT ( 'NONE',  ( -20.60448988230000111, 1484.737042837089803, 209.1218459616989946 ) ) ;
#6619 = CARTESIAN_POINT ( 'NONE',  ( -50.83427392639999454, 1384.622306023270085, 226.1831986462590010 ) ) ;
#6620 = CARTESIAN_POINT ( 'NONE',  ( 19.84207428532359785, 1508.528044499219959, 229.4304224270640020 ) ) ;
#6621 = VERTEX_POINT ( 'NONE', #69811 ) ;
#6622 = ORIENTED_EDGE ( 'NONE', *, *, #97190, .T. ) ;
#6623 = AXIS2_PLACEMENT_3D ( 'NONE', #82180, #66521, #22801 ) ;
#6624 = DIRECTION ( 'NONE',  ( -1.755985294532469921E-16, 1.000000000000000000, -1.338183447452831989E-16 ) ) ;
#6625 = CARTESIAN_POINT ( 'NONE',  ( 35.12919938944479270, 1437.169777039490100, 136.5372291599819903 ) ) ;
#6627 = CARTESIAN_POINT ( 'NONE',  ( 3.666164899629999585, 1486.466096722590009, 219.2737630301990066 ) ) ;
#6626 = DIRECTION ( 'NONE',  ( 0.000000000000000000, 0.000000000000000000, 1.000000000000000000 ) ) ;
#6628 = CARTESIAN_POINT ( 'NONE',  ( -7.996087907170001507, 1462.263563461390049, 203.4213808977189899 ) ) ;
#6629 = CARTESIAN_POINT ( 'NONE',  ( -107.7291480230000076, 1380.506275884730030, 298.7287515308590287 ) ) ;
#6630 = CARTESIAN_POINT ( 'NONE',  ( 4.760896992130000172, 1449.971761959190189, 190.6385172635989704 ) ) ;
#6631 = CARTESIAN_POINT ( 'NONE',  ( -10.80382370743670073, 1508.551704408389924, 217.9004706025669975 ) ) ;
#6632 = CARTESIAN_POINT ( 'NONE',  ( 12.30091743380850033, 1409.342617889579969, 200.6317861282630020 ) ) ;
#6633 = CARTESIAN_POINT ( 'NONE',  ( 18.80464347163499994, 1425.799926482960018, 225.6082800063759919 ) ) ;
#6634 = DIRECTION ( 'NONE',  ( 0.000000000000000000, 0.000000000000000000, -1.000000000000000000 ) ) ;
#6635 = CARTESIAN_POINT ( 'NONE',  ( 3.967425320557659507, 1431.784486675220023, 200.3531835805560206 ) ) ;
#6636 = CARTESIAN_POINT ( 'NONE',  ( -2.499999999569840092, 1440.150708319569958, 165.1395380847510239 ) ) ;
#6637 = AXIS2_PLACEMENT_3D ( 'NONE', #26441, #68481, #35406 ) ;
#6638 = CARTESIAN_POINT ( 'NONE',  ( -2.933306627113769771, 1448.953742279190010, 184.4303279486910014 ) ) ;
#6639 = EDGE_LOOP ( 'NONE', ( #92995, #5708, #96221, #76584 ) ) ;
#6640 = LINE ( 'NONE', #91743, #85039 ) ;
#6641 = CARTESIAN_POINT ( 'NONE',  ( 18.62804149895199757, 1457.295705444719943, 227.7225047233159785 ) ) ;
#6642 = CARTESIAN_POINT ( 'NONE',  ( -12.65123529389999923, 1435.857297067140053, 150.8939753325980178 ) ) ;
#6643 = B_SPLINE_CURVE_WITH_KNOTS ( 'NONE', 3,
 ( #82689, #46909, #31169, #98380, #72649, #20552, #30630, #54756, #64818, #65358, #3810, #12728, #81032, #22744, #12170, #63175, #106236, #46360, #98926, #48552, #22196, #55303, #4341, #106774, #28987, #37941, #80495, #99466, #29522, #63713, #97823, #56948, #64256, #91077, #5979, #105705, #21101, #89437, #30065, #21651, #55859, #89978, #13252 ),
 .UNSPECIFIED., .F., .F.,
 ( 4, 3, 3, 3, 3, 3, 3, 3, 3, 3, 3, 3, 3, 3, 4 ),
 ( 31.69285774156780278, 33.86896628700200296, 36.91232095655669809, 39.42219942477719741, 41.51453054943480225, 43.42754320367789944, 45.18198672082530010, 46.87502985914650111, 48.51047212527600294, 50.14591439140560425, 51.70904730156200202, 53.35035321201050351, 55.10040584591209978, 57.14372345036669998, 60.99056492696890075 ),
 .UNSPECIFIED. ) ;
#6644 = CARTESIAN_POINT ( 'NONE',  ( -1.176169269157790113E-08, 1473.984312740150017, 263.3285085788550077 ) ) ;
#6645 = EDGE_CURVE ( 'NONE', #16155, #63851, #24999, .T. ) ;
#6646 = CARTESIAN_POINT ( 'NONE',  ( 20.51827461483625825, 1436.445738427861443, 144.8727729820485592 ) ) ;
#6647 = CARTESIAN_POINT ( 'NONE',  ( 3.500000000000000000, 1407.163060387330006, 146.1721969590979882 ) ) ;
#6648 = CARTESIAN_POINT ( 'NONE',  ( -109.9855944269999952, 1384.926148861439970, 311.4562326602589906 ) ) ;
#6649 = CARTESIAN_POINT ( 'NONE',  ( -8.298113379911610465, 1511.753545947210114, 215.1666516095260135 ) ) ;
#6650 = CARTESIAN_POINT ( 'NONE',  ( -9.837816714745258651, 1361.043255431922262, 209.6218459617033432 ) ) ;
#6651 = DIRECTION ( 'NONE',  ( -0.3090169943749582204, -0.000000000000000000, -0.9510565162951499785 ) ) ;
#6652 = CARTESIAN_POINT ( 'NONE',  ( 14.00200617152209936, 1509.378643023580025, 234.5785651225629636 ) ) ;
#6653 = CARTESIAN_POINT ( 'NONE',  ( 32.38845791999495560, 1523.382868172864164, 202.1182848005512085 ) ) ;
#6654 = CARTESIAN_POINT ( 'NONE',  ( -7.337297350114999617, 1517.135701590510052, 208.3821536943570152 ) ) ;
#6655 = CARTESIAN_POINT ( 'NONE',  ( 5.805057908697529356, 1409.115777476449921, 223.0048059185109821 ) ) ;
#6656 = CIRCLE ( 'NONE', #42383, 1.500000000000001332 ) ;
#6657 = CARTESIAN_POINT ( 'NONE',  ( 8.902411381149999414, 1424.022968669029979, 122.9077991975980098 ) ) ;
#6658 = CARTESIAN_POINT ( 'NONE',  ( 7.509953471767339295, 1425.386002328900076, 212.2272222051859956 ) ) ;
#6659 = ORIENTED_EDGE ( 'NONE', *, *, #18790, .T. ) ;
#6660 = EDGE_CURVE ( 'NONE', #6800, #32914, #70276, .T. ) ;
#6661 = CARTESIAN_POINT ( 'NONE',  ( 13.69365034059999964, 1418.910360381229793, 238.2645940840980074 ) ) ;
#6663 = CARTESIAN_POINT ( 'NONE',  ( -17.64684345579999913, 1410.891992815630147, 194.5765879308980004 ) ) ;
#6662 = CARTESIAN_POINT ( 'NONE',  ( -2.522360636850000226, 1478.162778754029887, 182.0787142752979832 ) ) ;
#6664 = CARTESIAN_POINT ( 'NONE',  ( -6.208076407620000126, 1461.436029833090060, 207.2638656286190155 ) ) ;
#6665 = CARTESIAN_POINT ( 'NONE',  ( -4.804950797150000064, 1416.130848188830214, 240.4142140068979927 ) ) ;
#6666 = CARTESIAN_POINT ( 'NONE',  ( -4.646147438016499542, 1378.399971910029990, 214.5514622210689879 ) ) ;
#6667 = EDGE_CURVE ( 'NONE', #51820, #65412, #80948, .T. ) ;
#6668 = CARTESIAN_POINT ( 'NONE',  ( -5.464307007782710279, 1452.722242581880209, 151.9884548250850003 ) ) ;
#6669 = CARTESIAN_POINT ( 'NONE',  ( -18.64672481350000055, 1416.851343894929869, 208.5597484335680178 ) ) ;
#6670 = ORIENTED_EDGE ( 'NONE', *, *, #80171, .T. ) ;
#6671 = DIRECTION ( 'NONE',  ( 0.9455185755993178454, 0.000000000000000000, -0.3255681544571539243 ) ) ;
#6672 = CARTESIAN_POINT ( 'NONE',  ( 5.561733859871847763, 1387.291117539184825, 209.1218459616989946 ) ) ;
#6673 = CARTESIAN_POINT ( 'NONE',  ( 14.65055688039350024, 1420.306699661070070, 228.1705606154760062 ) ) ;
#6674 = CARTESIAN_POINT ( 'NONE',  ( 10.08490127059999963, 1462.177701891290099, 210.4147059520890082 ) ) ;
#6675 = ORIENTED_EDGE ( 'NONE', *, *, #27442, .F. ) ;
#6676 = ORIENTED_EDGE ( 'NONE', *, *, #54836, .T. ) ;
#6677 = CARTESIAN_POINT ( 'NONE',  ( -68.70832551159999468, 1385.106080149109857, 263.4315270082590246 ) ) ;
#6678 = CARTESIAN_POINT ( 'NONE',  ( -24.14171740887259787, 1410.987097078699890, 209.1436450758499745 ) ) ;
#6679 = VERTEX_POINT ( 'NONE', #110000 ) ;
#6680 = CARTESIAN_POINT ( 'NONE',  ( -102.9430107027000076, 1368.558218059089995, 309.9345252466190459 ) ) ;
#6681 = AXIS2_PLACEMENT_3D ( 'NONE', #27841, #54173, #1548 ) ;
#6682 = CARTESIAN_POINT ( 'NONE',  ( 7.468436490899999392, 1491.313758626190065, 211.3467155923090104 ) ) ;
#6683 = B_SPLINE_CURVE_WITH_KNOTS ( 'NONE', 4,
 ( #106769, #89973, #104155, #4864, #18468, #52664, #30060, #98374, #86801 ),
 .UNSPECIFIED., .F., .F.,
 ( 5, 4, 5 ),
 ( 0.000000000000000000, 2.461317144287991862E-05, 1.000000000000000000 ),
 .UNSPECIFIED. ) ;
#6684 = CARTESIAN_POINT ( 'NONE',  ( -0.4783097240599999966, 1498.354913959829901, 236.9202977269980011 ) ) ;
#6685 = CARTESIAN_POINT ( 'NONE',  ( -19.36978574289999955, 1410.873293175530080, 222.2371973171979960 ) ) ;
#6686 = CARTESIAN_POINT ( 'NONE',  ( 45.13182480330119972, 1448.544769101459906, 267.0067098273050306 ) ) ;
#6687 = CARTESIAN_POINT ( 'NONE',  ( -3.802992233161490265, 1508.880967439349888, 204.6292016850710240 ) ) ;
#6688 = CARTESIAN_POINT ( 'NONE',  ( -0.06123813080619999044, 1419.142829484630056, 184.6462053571979993 ) ) ;
#6689 = CARTESIAN_POINT ( 'NONE',  ( 5.772727908745000747, 1516.691414181030041, 205.6645793267070133 ) ) ;
#6690 = EDGE_CURVE ( 'NONE', #22976, #76210, #77968, .T. ) ;
#6691 = ORIENTED_EDGE ( 'NONE', *, *, #74662, .F. ) ;
#6692 = CARTESIAN_POINT ( 'NONE',  ( 18.49876145869168553, 1458.769598805399028, 227.6223408758116307 ) ) ;
#6693 = CARTESIAN_POINT ( 'NONE',  ( 15.13723819610809862, 1513.497693042470019, 194.6975888916769861 ) ) ;
#6694 = CARTESIAN_POINT ( 'NONE',  ( 4.343364931220000003, 1426.780599525880007, 211.8480867413289843 ) ) ;
#6695 = ORIENTED_EDGE ( 'NONE', *, *, #7012, .T. ) ;
#6696 = CARTESIAN_POINT ( 'NONE',  ( 3.440243711449999964, 1448.632170455610094, 184.1390994748980177 ) ) ;
#6697 = CARTESIAN_POINT ( 'NONE',  ( 7.302416004457981558, 1435.594922686310838, 204.5677890833769652 ) ) ;
#6698 = CARTESIAN_POINT ( 'NONE',  ( -14.21962194668809865, 1513.293387711960122, 193.9060419221420091 ) ) ;
#6699 = CARTESIAN_POINT ( 'NONE',  ( 6.966807131377220408, 1504.412568754190033, 219.8081154884820023 ) ) ;
#6700 = CARTESIAN_POINT ( 'NONE',  ( 7.455473913919999696, 1422.775276769710217, 195.6452099806990077 ) ) ;
#6701 = CARTESIAN_POINT ( 'NONE',  ( 1.233474458951280051, 1431.395778057770031, 218.5319384325650276 ) ) ;
#6702 = CARTESIAN_POINT ( 'NONE',  ( -5.254485968520000050, 1494.936664904289955, 197.9757700040989903 ) ) ;
#6703 = CARTESIAN_POINT ( 'NONE',  ( 1.821213500400669982, 1408.976658564170066, 186.8790236249210182 ) ) ;
#6705 = CARTESIAN_POINT ( 'NONE',  ( -18.51078443728962597, 1424.286743862528056, 225.0123096373268936 ) ) ;
#6704 = CARTESIAN_POINT ( 'NONE',  ( -16.67282884602620285, 1411.231623680630037, 191.7273266183159990 ) ) ;
#6706 = CARTESIAN_POINT ( 'NONE',  ( 11.56989304032649812, 1426.466096579750001, 206.5199424030009823 ) ) ;
#6707 = CARTESIAN_POINT ( 'NONE',  ( -11.18595519959999862, 1378.367123367120030, 214.3754839606289977 ) ) ;
#6708 = CARTESIAN_POINT ( 'NONE',  ( 2.424063131930000115, 1427.257651041929876, 147.9020499575979954 ) ) ;
#6709 = ORIENTED_EDGE ( 'NONE', *, *, #32585, .T. ) ;
#6710 = CARTESIAN_POINT ( 'NONE',  ( 12.77825866169999891, 1416.543503932829935, 222.2791103846979865 ) ) ;
#6711 = DIRECTION ( 'NONE',  ( -1.000000000000000000, 0.000000000000000000, -0.000000000000000000 ) ) ;
#6712 = AXIS2_PLACEMENT_3D ( 'NONE', #63183, #10533, #71028 ) ;
#6713 = CARTESIAN_POINT ( 'NONE',  ( -107.6372536681080021, 1384.927886973209979, 311.2581927475170005 ) ) ;
#6714 = CARTESIAN_POINT ( 'NONE',  ( -9.778401456010000103, 1386.774025706429939, 200.5312082851889954 ) ) ;
#6715 = CARTESIAN_POINT ( 'NONE',  ( 9.362767939971719855, 1424.864447360270105, 209.3171238155310050 ) ) ;
#6716 = CARTESIAN_POINT ( 'NONE',  ( 11.53900508938759906, 1422.010879093899803, 203.4012210850169993 ) ) ;
#6717 = CARTESIAN_POINT ( 'NONE',  ( -11.01004492055549910, 1462.557516207839853, 208.2324619591759927 ) ) ;
#6718 = CARTESIAN_POINT ( 'NONE',  ( -39.48812356950000435, 1450.238330950499858, 268.3665355202980436 ) ) ;
#6719 = LINE ( 'NONE', #106436, #50337 ) ;
#6720 = CARTESIAN_POINT ( 'NONE',  ( 11.13410507230000057, 1433.980233170309930, 151.6623994222979945 ) ) ;
#6721 = CARTESIAN_POINT ( 'NONE',  ( 3.330669073880000049E-15, 1465.000168611230038, 255.3819207742980097 ) ) ;
#6722 = FACE_OUTER_BOUND ( 'NONE', #86787, .T. ) ;
#6723 = CARTESIAN_POINT ( 'NONE',  ( 4.487249773072029768, 1509.038615930399828, 211.6097810847319920 ) ) ;
#6724 = DIRECTION ( 'NONE',  ( 1.000000000000000000, 0.000000000000000000, 0.000000000000000000 ) ) ;
#6725 = CARTESIAN_POINT ( 'NONE',  ( 5.544572127002579620, 1465.561989329190055, 218.7012434299869881 ) ) ;
#6726 = CARTESIAN_POINT ( 'NONE',  ( -15.65156082859999920, 1486.025561616130062, 186.7146735895979930 ) ) ;
#6727 = DIRECTION ( 'NONE',  ( 0.000000000000000000, 0.000000000000000000, 1.000000000000000000 ) ) ;
#6728 = CARTESIAN_POINT ( 'NONE',  ( -17.12887326659999943, 1409.676338055229962, 225.1570305523979982 ) ) ;
#6729 = CARTESIAN_POINT ( 'NONE',  ( 5.205339508856989816, 1440.970228299569953, 155.0076768800470006 ) ) ;
#6730 = CARTESIAN_POINT ( 'NONE',  ( 5.550896940410000369, 1461.183176948789878, 205.2452863306889981 ) ) ;
#6731 = CARTESIAN_POINT ( 'NONE',  ( -17.50306819544480064, 1410.886025037689933, 192.6233946069430090 ) ) ;
#6732 = CARTESIAN_POINT ( 'NONE',  ( 3.393535723931189676E-07, 1408.913060375439727, 194.3872976811450144 ) ) ;
#6733 = CARTESIAN_POINT ( 'NONE',  ( 12.74509880840539999, 1426.619167131859967, 203.6612177353580080 ) ) ;
#6734 = CARTESIAN_POINT ( 'NONE',  ( -7.951679572020000641, 1415.087745006229852, 224.2313155807979683 ) ) ;
#6735 = CARTESIAN_POINT ( 'NONE',  ( 0.2051860993799010102, 1460.061070970760056, 182.9504558288110161 ) ) ;
#6737 = ORIENTED_EDGE ( 'NONE', *, *, #107025, .F. ) ;
#6736 = CARTESIAN_POINT ( 'NONE',  ( 9.762629409768241118, 1468.224221565797279, 206.7965198539660321 ) ) ;
#6738 = CARTESIAN_POINT ( 'NONE',  ( -17.22592482065197927, 1444.324653571828776, 162.9227486220069920 ) ) ;
#6739 = CARTESIAN_POINT ( 'NONE',  ( -29.01179239785159680, 1509.906542726809903, 211.5837526005719837 ) ) ;
#6740 = CARTESIAN_POINT ( 'NONE',  ( 13.19848402559999911, 1434.900413493669930, 149.4779621765979982 ) ) ;
#6741 = CARTESIAN_POINT ( 'NONE',  ( -41.56943536072299850, 1444.920853409440042, 134.0999999984259716 ) ) ;
#6742 = CARTESIAN_POINT ( 'NONE',  ( -109.5354675709999981, 1384.888714447859911, 297.1231980247589490 ) ) ;
#6743 = ORIENTED_EDGE ( 'NONE', *, *, #107681, .F. ) ;
#6744 = CARTESIAN_POINT ( 'NONE',  ( -5.444242866291430616, 1391.534755755089918, 203.3364090815709915 ) ) ;
#6745 = FACE_OUTER_BOUND ( 'NONE', #93919, .T. ) ;
#6746 = CARTESIAN_POINT ( 'NONE',  ( -104.0047667647111780, 1380.199657110949147, 306.4945035597083347 ) ) ;
#6747 = CARTESIAN_POINT ( 'NONE',  ( -21.83550407203883736, 1523.678648413191695, 234.9693198511253627 ) ) ;
#6748 = CARTESIAN_POINT ( 'NONE',  ( 1.894388308689999967, 1506.148290744889891, 221.7829938216989945 ) ) ;
#6749 = CIRCLE ( 'NONE', #22877, 1.000000000000000888 ) ;
#6750 = CARTESIAN_POINT ( 'NONE',  ( 31.99848188241270108, 1416.544741823263621, 269.3157487230474771 ) ) ;
#6751 = CARTESIAN_POINT ( 'NONE',  ( -16.22868724909999827, 1418.857858964219986, 209.4919173468780116 ) ) ;
#6752 = CARTESIAN_POINT ( 'NONE',  ( -13.62224074200000068, 1380.247549972129946, 210.4815130236790139 ) ) ;
#6753 = CARTESIAN_POINT ( 'NONE',  ( 2.500000000000000000, 1434.142768478290236, 183.0182394750980279 ) ) ;
#6754 = CARTESIAN_POINT ( 'NONE',  ( -56.94461646417340717, 1385.046987227980026, 237.6273277843820040 ) ) ;
#6755 = CARTESIAN_POINT ( 'NONE',  ( -19.67623451925489775, 1525.581535527370761, 237.1855307018975054 ) ) ;
#6756 = CARTESIAN_POINT ( 'NONE',  ( 10.31871872550729918, 1424.391353036610099, 207.1214719758330034 ) ) ;
#6757 = VERTEX_POINT ( 'NONE', #59062 ) ;
#6758 = CARTESIAN_POINT ( 'NONE',  ( -28.53738215540000311, 1450.628365292199987, 136.4035485695980014 ) ) ;
#6759 = CARTESIAN_POINT ( 'NONE',  ( -15.88324579074509835, 1409.493232073089985, 225.5703039524069879 ) ) ;
#6761 = ORIENTED_EDGE ( 'NONE', *, *, #54326, .T. ) ;
#6760 = CARTESIAN_POINT ( 'NONE',  ( 1.886382439867170024, 1437.487153458199828, 227.5670087340569978 ) ) ;
#6762 = CARTESIAN_POINT ( 'NONE',  ( 4.972072924729999954, 1472.535148281390093, 218.0116174414390002 ) ) ;
#6763 = CARTESIAN_POINT ( 'NONE',  ( 9.690921760896669568, 1469.947179451500006, 211.8829996226070023 ) ) ;
#6764 = CARTESIAN_POINT ( 'NONE',  ( -21.04604312829590995, 1411.007314980063711, 218.1938530540165857 ) ) ;
#6765 = CARTESIAN_POINT ( 'NONE',  ( -109.6535179219999918, 1384.622105623380094, 311.3127935212589819 ) ) ;
#6766 = DIRECTION ( 'NONE',  ( -7.436362843295819681E-17, 1.000000000000000000, -1.457576885956999882E-16 ) ) ;
#6767 = CARTESIAN_POINT ( 'NONE',  ( 18.50818375480000100, 1409.559380405929915, 219.7813082434980174 ) ) ;
#6768 = DIRECTION ( 'NONE',  ( -0.4090087482554184417, 0.000000000000000000, 0.9125304618754027652 ) ) ;
#6769 = CARTESIAN_POINT ( 'NONE',  ( -17.46811834570000244, 1424.002211962029833, 227.1199482243980015 ) ) ;
#6770 = CARTESIAN_POINT ( 'NONE',  ( -4.982688954091917921, 1511.399508273119864, 200.6046720606312306 ) ) ;
#6771 = CARTESIAN_POINT ( 'NONE',  ( 9.698381235350000296, 1450.963213650890111, 206.3010183936889916 ) ) ;
#6772 = CARTESIAN_POINT ( 'NONE',  ( -96.21470915085021147, 1331.448250124730293, 287.0365551081087574 ) ) ;
#6773 = CARTESIAN_POINT ( 'NONE',  ( 22.98705083096197654, 1509.732498449673130, 190.4850602025729813 ) ) ;
#6774 = VECTOR ( 'NONE', #20623, 1000.000000000000000 ) ;
#6775 = CARTESIAN_POINT ( 'NONE',  ( -1.100379444789999939, 1455.838357077089768, 199.3345172646990022 ) ) ;
#6776 = CARTESIAN_POINT ( 'NONE',  ( -2.879956963085000154, 1516.827328999679821, 205.8693153165069702 ) ) ;
#6777 = B_SPLINE_CURVE_WITH_KNOTS ( 'NONE', 5,
 ( #85214, #77388, #61174, #1804, #84664, #50539 ),
 .UNSPECIFIED., .F., .F.,
 ( 6, 6 ),
 ( 141.1642459979999842, 150.6560418210000023 ),
 .UNSPECIFIED. ) ;
#6778 = CIRCLE ( 'NONE', #12384, 1.000000000000000888 ) ;
#6779 = CARTESIAN_POINT ( 'NONE',  ( -11.46119733878520108, 1485.818205503899890, 184.7882622351909845 ) ) ;
#6780 = ORIENTED_EDGE ( 'NONE', *, *, #73025, .F. ) ;
#6781 = CARTESIAN_POINT ( 'NONE',  ( -4.222410926209430038, 1441.597235995280016, 167.7030612426750054 ) ) ;
#6784 = VERTEX_POINT ( 'NONE', #109457 ) ;
#6783 = CARTESIAN_POINT ( 'NONE',  ( -68.71522126961548338, 1379.747817121739899, 280.3072533349409809 ) ) ;
#6782 = AXIS2_PLACEMENT_3D ( 'NONE', #57334, #38834, #65166 ) ;
#6785 = CARTESIAN_POINT ( 'NONE',  ( -12.02612939183720009, 1377.659857216290220, 211.7505375168460091 ) ) ;
#6786 = ORIENTED_EDGE ( 'NONE', *, *, #89707, .T. ) ;
#6787 =( GEOMETRIC_REPRESENTATION_CONTEXT ( 3 ) GLOBAL_UNCERTAINTY_ASSIGNED_CONTEXT ( ( #62554 ) ) GLOBAL_UNIT_ASSIGNED_CONTEXT ( ( #41521, #76220, #93548 ) ) REPRESENTATION_CONTEXT ( 'NONE', 'WORKASPACE' ) );
#6788 = CARTESIAN_POINT ( 'NONE',  ( -16.01537990865516292, 1514.821748405528524, 224.2191644384507754 ) ) ;
#6789 = CARTESIAN_POINT ( 'NONE',  ( 11.36630642249999923, 1502.069393327289845, 207.5140256288290175 ) ) ;
#6791 = CARTESIAN_POINT ( 'NONE',  ( 16.18564167855010183, 1410.718174707190201, 191.5748361957220141 ) ) ;
#6790 = CARTESIAN_POINT ( 'NONE',  ( -11.43729212106539883, 1425.481250161560183, 144.1595925846119997 ) ) ;
#6792 = CARTESIAN_POINT ( 'NONE',  ( -1.117840124865000062, 1516.949031626070109, 210.8389850543470061 ) ) ;
#6793 = CARTESIAN_POINT ( 'NONE',  ( 37.45063484360860429, 1436.678284271650227, 135.9172768678939747 ) ) ;
#6794 = B_SPLINE_CURVE_WITH_KNOTS ( 'NONE', 3,
 ( #34593, #60364, #2130, #95060, #51961, #35697, #85530, #44117, #36254, #8824, #18327, #1565, #94486, #69886, #35145, #105118 ),
 .UNSPECIFIED., .F., .F.,
 ( 4, 3, 3, 3, 3, 4 ),
 ( -7.454956845832920287, -7.041679458493519839, -6.041855899781880090, -5.045615715417369529, -4.051023835724380184, -3.058675454860000364 ),
 .UNSPECIFIED. ) ;
#6795 = CARTESIAN_POINT ( 'NONE',  ( -11.15483420530000025, 1425.160608745730087, 144.1639996088979956 ) ) ;
#6796 = CARTESIAN_POINT ( 'NONE',  ( -1.870694922257569948, 1509.048000892659957, 179.3712176469529993 ) ) ;
#6797 = CARTESIAN_POINT ( 'NONE',  ( 12.64308048353610126, 1500.885237595450008, 210.4353653217530109 ) ) ;
#6798 = CARTESIAN_POINT ( 'NONE',  ( 0.000000000000000000, 0.000000000000000000, 0.000000000000000000 ) ) ;
#6799 = CARTESIAN_POINT ( 'NONE',  ( 39.48448845331249402, 1449.205409213759822, 134.0999999980729740 ) ) ;
#6800 = VERTEX_POINT ( 'NONE', #33277 ) ;
#6801 = CARTESIAN_POINT ( 'NONE',  ( -16.61337445550000069, 1463.629612651790012, 220.4655171657990138 ) ) ;
#6802 = CARTESIAN_POINT ( 'NONE',  ( 4.219439013950669448, 1441.595895969210005, 182.7715284958480026 ) ) ;
#6803 = ORIENTED_EDGE ( 'NONE', *, *, #2824, .T. ) ;
#6804 = ORIENTED_EDGE ( 'NONE', *, *, #56458, .F. ) ;
#6805 = B_SPLINE_CURVE_WITH_KNOTS ( 'NONE', 3,
 ( #71080, #44201, #20079, #11156, #1655, #18406, #18963, #78346, #86740, #10032, #105205, #96809, #52051, #54273, #35791, #68865, #11690, #102969, #103532, #95145, #27941, #26267, #62122, #2218, #45317, #96249, #69975, #19523, #1103, #60457, #88398 ),
 .UNSPECIFIED., .F., .F.,
 ( 4, 3, 3, 3, 3, 3, 3, 3, 3, 3, 4 ),
 ( 2.324858856890000158, 2.629659992475509966, 2.924842188867320392, 3.130565735668509930, 3.432172540442299802, 3.731439316943959916, 4.025646101810540500, 4.318556006757110488, 4.608870342396969910, 4.895817133586150227, 4.991117563610000474 ),
 .UNSPECIFIED. ) ;
#6806 = CARTESIAN_POINT ( 'NONE',  ( 11.60004869885203682, 1426.170871907920400, 138.0044153181233071 ) ) ;
#6807 = CARTESIAN_POINT ( 'NONE',  ( 15.13342375178309851, 1507.606285622089899, 226.3974328904010065 ) ) ;
#6808 = CARTESIAN_POINT ( 'NONE',  ( 0.2421685061019999974, 1451.163597886330081, 182.5480898430980119 ) ) ;
#6809 = AXIS2_PLACEMENT_3D ( 'NONE', #15796, #75752, #109898 ) ;
#6810 = CARTESIAN_POINT ( 'NONE',  ( -21.11329577064019958, 1508.551704414039932, 210.1840812171020048 ) ) ;
#6811 = DIRECTION ( 'NONE',  ( -6.123233995736769734E-17, -1.000000000000000000, 7.888609052210119587E-33 ) ) ;
#6812 = CARTESIAN_POINT ( 'NONE',  ( 3.401541474470889614, 1468.225229937070026, 218.5224292273400124 ) ) ;
#6813 = CARTESIAN_POINT ( 'NONE',  ( -3.487586626227472841, 1508.731359868795380, 204.5668839433602386 ) ) ;
#6814 = CARTESIAN_POINT ( 'NONE',  ( 36.37832874669670247, 1435.767865795960006, 134.4205480902799934 ) ) ;
#6815 = CARTESIAN_POINT ( 'NONE',  ( 2.268814847818510394, 1421.223351404420100, 183.2269488433420008 ) ) ;
#6816 = CARTESIAN_POINT ( 'NONE',  ( 26.72206613759999883, 1436.390045543859969, 136.7408624964980106 ) ) ;
#6817 = CARTESIAN_POINT ( 'NONE',  ( -10.07692313350000113, 1391.913060387289988, 214.3555494166390076 ) ) ;
#6818 = CARTESIAN_POINT ( 'NONE',  ( -82.75703543348309665, 1384.807624658469877, 286.4509065024590200 ) ) ;
#6819 = ORIENTED_EDGE ( 'NONE', *, *, #51369, .F. ) ;
#6820 = CARTESIAN_POINT ( 'NONE',  ( -0.01126495432349849946, 1516.939530130779985, 202.1773791897269916 ) ) ;
#6821 = CARTESIAN_POINT ( 'NONE',  ( 7.713648834184999359, 1516.710624944440042, 208.3691743819339877 ) ) ;
#6822 = EDGE_LOOP ( 'NONE', ( #50881, #56359, #102236, #102265 ) ) ;
#6823 = LINE ( 'NONE', #40982, #25800 ) ;
#6824 = CARTESIAN_POINT ( 'NONE',  ( -0.002327269815061227144, 1451.794865080891896, 154.0455392037681293 ) ) ;
#6825 = VERTEX_POINT ( 'NONE', #92636 ) ;
#6826 = CARTESIAN_POINT ( 'NONE',  ( -13.38213216230000135, 1415.140114695929924, 220.8789972148979928 ) ) ;
#6827 = CARTESIAN_POINT ( 'NONE',  ( -1.925297167936410148, 1517.051704408389924, 187.5582988455250018 ) ) ;
#6828 = B_SPLINE_CURVE_WITH_KNOTS ( 'NONE', 3,
 ( #97454, #3419, #26949, #53271, #27488, #80099, #89044, #1769, #105867, #62797, #19634, #77902, #29147, #52712, #87410, #61676, #63334, #95799, #86847, #19067, #87975, #11263, #10140, #35906, #70090, #104203, #79027, #20181, #2328, #45425, #79568, #2869, #36989, #105305, #96913, #88512, #13417, #108606, #57126, #3971, #5602, #99083, #38095, #22361, #91252, #39753, #56562, #90690, #108043, #82304, #97989, #21811, #106946, #56010, #65524, #38638, #90134, #13978, #48166, #73915, #66080, #64968, #47606, #81731, #64423, #89594, #63873, #21256, #48722, #31340, #40294, #55467, #14533, #5039, #30232, #72272, #99631, #22919, #74479, #12886, #100206, #82847, #39184, #47064, #6137 ),
 .UNSPECIFIED., .F., .F.,
 ( 4, 2, 1, 1, 2, 2, 2, 1, 1, 2, 2, 2, 2, 1, 1, 2, 2, 2, 2, 1, 2, 2, 2, 2, 2, 2, 2, 2, 2, 2, 2, 1, 2, 2, 2, 1, 1, 2, 2, 2, 1, 1, 1, 2, 2, 2, 2, 2, 4 ),
 ( 0.000000000000000000, 0.03124999999979321402, 0.04687499999968981756, 0.05468749999963812281, 0.05859374999961227543, 0.06249999999958642805, 0.09374999999943356421, 0.1093749999993740563, 0.1171874999993623018, 0.1210937499993691435, 0.1249999999993759714, 0.1874999999992264521, 0.2187499999991654176, 0.2343749999991026067, 0.2421874999990496768, 0.2460937499990234201, 0.2499999999989971911, 0.3124999999987780330, 0.3437499999986242671, 0.3593749999985473287, 0.3671874999985022536, 0.3749999999984571231, 0.4374999999983198995, 0.4687499999981770138, 0.4999999999980341281, 0.5624999999977483567, 0.5937499999976966203, 0.6093749999976747489, 0.6249999999976528775, 0.6874999999980238030, 0.7187499999982092103, 0.7343749999982962517, 0.7421874999983337773, 0.7499999999983713028, 0.7812499999987206900, 0.7968749999989165334, 0.8046874999989963584, 0.8085937499990306643, 0.8124999999990649702, 0.8437499999992383870, 0.8593749999993495203, 0.8671874999993995914, 0.8710937499994046984, 0.8730468749993932631, 0.8749999999993817168, 0.9062499999995329292, 0.9218749999996082023, 0.9374999999996835864, 1.000000000000000000 ),
 .UNSPECIFIED. ) ;
#6829 = CARTESIAN_POINT ( 'NONE',  ( -9.343473286536170264, 1461.635954483039995, 206.4705841331299894 ) ) ;
#6830 = CARTESIAN_POINT ( 'NONE',  ( 21.19109013666399832, 1409.653069700570086, 206.4065099927269955 ) ) ;
#6831 = CARTESIAN_POINT ( 'NONE',  ( 9.908749694887600157, 1468.699217298059921, 207.6203599669360074 ) ) ;
#6832 = CARTESIAN_POINT ( 'NONE',  ( -6.488994010384053546, 1468.824241490008717, 218.3969213443690762 ) ) ;
#6833 = CARTESIAN_POINT ( 'NONE',  ( -11.87558183880000051, 1433.006727494650022, 147.8551147428979959 ) ) ;
#6835 = EDGE_CURVE ( 'NONE', #17250, #7904, #33834, .T. ) ;
#6834 = CARTESIAN_POINT ( 'NONE',  ( 23.26829263668760106, 1427.370071165639956, 206.2054270095080142 ) ) ;
#6837 = CARTESIAN_POINT ( 'NONE',  ( 9.079024693347159669, 1468.625100210450000, 202.5093681977309927 ) ) ;
#6836 = CARTESIAN_POINT ( 'NONE',  ( 12.79059621819999926, 1461.442156363629920, 233.1425226920979696 ) ) ;
#6838 = CARTESIAN_POINT ( 'NONE',  ( -4.694043468504164096, 1422.166103873277052, 184.6933998799214578 ) ) ;
#6839 = CARTESIAN_POINT ( 'NONE',  ( 0.3402564618027850152, 1410.306538916012187, 185.0315799371184653 ) ) ;
#6840 = VERTEX_POINT ( 'NONE', #43364 ) ;
#6841 = CARTESIAN_POINT ( 'NONE',  ( 1.491506560153237793, 1511.187213306747708, 175.5704429466618421 ) ) ;
#6842 = CARTESIAN_POINT ( 'NONE',  ( -15.77149559868386675, 1420.276057766250915, 210.6539470928313165 ) ) ;
#6843 = CARTESIAN_POINT ( 'NONE',  ( 1.220352910582999995, 1516.613788747029275, 216.8329590593428975 ) ) ;
#6844 = CARTESIAN_POINT ( 'NONE',  ( 1.715361092244999996, 1516.743010792419909, 212.5670474586069929 ) ) ;
#6845 = CARTESIAN_POINT ( 'NONE',  ( 18.53418647859999879, 1507.620785850130005, 188.5293807644980006 ) ) ;
#6846 = CARTESIAN_POINT ( 'NONE',  ( -10.98821264772629469, 1424.974956303378349, 138.3384972958762660 ) ) ;
#6848 = ORIENTED_EDGE ( 'NONE', *, *, #33831, .F. ) ;
#6847 = CARTESIAN_POINT ( 'NONE',  ( -11.87651332576620078, 1501.535165843179811, 211.4045997421629863 ) ) ;
#6849 = CARTESIAN_POINT ( 'NONE',  ( 1.320018090259999832, 1507.624001450029937, 186.1627566462979928 ) ) ;
#6850 = CARTESIAN_POINT ( 'NONE',  ( -1.568956603680000006, 1508.180600514190019, 220.9064527986990072 ) ) ;
#6851 = CARTESIAN_POINT ( 'NONE',  ( -10.95162904410000060, 1431.051873458699902, 151.6569759818979719 ) ) ;
#6852 = CARTESIAN_POINT ( 'NONE',  ( 1.557255085340000011, 1435.511706276389987, 227.5437143207990118 ) ) ;
#6853 = CARTESIAN_POINT ( 'NONE',  ( -109.9672919399559987, 1384.428774922700086, 311.4339036070600173 ) ) ;
#6854 = DIRECTION ( 'NONE',  ( 1.755985294532464991E-16, -1.000000000000000000, 1.338183447452830017E-16 ) ) ;
#6855 = CARTESIAN_POINT ( 'NONE',  ( -6.544710712048379619, 1426.691555418079815, 202.4711062780949931 ) ) ;
#6856 = CIRCLE ( 'NONE', #36995, 2.000000000000003553 ) ;
#6857 = DIRECTION ( 'NONE',  ( -6.162707975952100561E-15, -1.000000000000000000, -1.094450614310000083E-14 ) ) ;
#6859 = CARTESIAN_POINT ( 'NONE',  ( -10.71539411164560107, 1482.205790377970288, 206.4284175877959910 ) ) ;
#6858 = CARTESIAN_POINT ( 'NONE',  ( -26.30997306620000131, 1508.005173063729899, 215.7207955781479995 ) ) ;
#6860 = CARTESIAN_POINT ( 'NONE',  ( 5.316196956075329716, 1517.151704408390060, 187.2259631713411636 ) ) ;
#6861 = ORIENTED_EDGE ( 'NONE', *, *, #39266, .T. ) ;
#6863 = AXIS2_PLACEMENT_3D ( 'NONE', #11598, #29485, #63681 ) ;
#6862 = CARTESIAN_POINT ( 'NONE',  ( 6.547556931335000385, 1516.633288330999903, 205.8595812817970057 ) ) ;
#6864 = CARTESIAN_POINT ( 'NONE',  ( 12.72968732700000061, 1407.074333243529964, 268.4159762977980108 ) ) ;
#6865 = CARTESIAN_POINT ( 'NONE',  ( -0.08525575416679999352, 1408.910083189030047, 186.0349129820979783 ) ) ;
#6866 = AXIS2_PLACEMENT_3D ( 'NONE', #12829, #100147, #83341 ) ;
#6867 = CARTESIAN_POINT ( 'NONE',  ( 10.94830312428359953, 1490.380690179980093, 209.7447272360980151 ) ) ;
#6868 = CIRCLE ( 'NONE', #5032, 1.000000000000000888 ) ;
#6869 = ADVANCED_FACE ( 'NONE', ( #93185 ), #60826, .F. ) ;
#6870 = CARTESIAN_POINT ( 'NONE',  ( 24.50944912269722664, 1438.648100259966668, 212.6421093072691235 ) ) ;
#6871 = EDGE_CURVE ( 'NONE', #6988, #100587, #84886, .T. ) ;
#6872 = CARTESIAN_POINT ( 'NONE',  ( -8.903760273451595708, 1388.803743861253452, 217.7495020015849434 ) ) ;
#6873 =( BOUNDED_CURVE ( )  B_SPLINE_CURVE ( 3, ( #3375, #28553, #45918, #20139 ),
 .UNSPECIFIED., .F., .F. ) 
 B_SPLINE_CURVE_WITH_KNOTS ( ( 4, 4 ),
 ( 5.644024340868369904, 5.936278781197910526 ),
 .UNSPECIFIED. ) 
 CURVE ( )  GEOMETRIC_REPRESENTATION_ITEM ( )  RATIONAL_B_SPLINE_CURVE ( ( 1.000000000000000000, 0.9928949349872718821, 0.9928949349872718821, 1.000000000000000000 ) ) 
 REPRESENTATION_ITEM ( '' )  );
#6874 = CARTESIAN_POINT ( 'NONE',  ( 27.78931436370000085, 1508.066562786630129, 211.8879754161380333 ) ) ;
#6875 = ADVANCED_FACE ( 'NONE', ( #6551 ), #47597, .F. ) ;
#6876 = DIRECTION ( 'NONE',  ( 9.261055619630009070E-47, -1.000000000000000000, 1.836970198721029688E-16 ) ) ;
#6877 = CARTESIAN_POINT ( 'NONE',  ( -15.56126507649999979, 1417.814061455979981, 204.2177041305290004 ) ) ;
#6878 = CARTESIAN_POINT ( 'NONE',  ( -13.96458816240000012, 1446.023138053109960, 188.4738050279979973 ) ) ;
#6879 = EDGE_CURVE ( 'NONE', #43545, #22154, #58072, .T. ) ;
#6880 = CARTESIAN_POINT ( 'NONE',  ( -19.88180708459617207, 1485.246950916194237, 190.7624080160636595 ) ) ;
#6881 = EDGE_CURVE ( 'NONE', #62929, #43414, #36882, .T. ) ;
#6882 = CARTESIAN_POINT ( 'NONE',  ( -16.15556852644305863, 1419.752504305882894, 210.0532078212941940 ) ) ;
#6883 = CARTESIAN_POINT ( 'NONE',  ( -4.212749018120000244, 1497.360448316590009, 220.3810617930989793 ) ) ;
#6884 = CARTESIAN_POINT ( 'NONE',  ( 1.998401444330000344E-15, 1425.981674191730008, 219.6133832206979832 ) ) ;
#6885 = CARTESIAN_POINT ( 'NONE',  ( -31.34137657934027388, 1501.977400791986611, 196.3411265156551906 ) ) ;
#6886 = CARTESIAN_POINT ( 'NONE',  ( -2.744509240469999778, 1475.260335887530118, 269.4960840521980572 ) ) ;
#6888 = CIRCLE ( 'NONE', #22938, 975.0211406871101190 ) ;
#6887 = CARTESIAN_POINT ( 'NONE',  ( -17.07488731192356823, 1517.051704408389924, 212.8400904445188075 ) ) ;
#6889 = CARTESIAN_POINT ( 'NONE',  ( -7.980162481601299262, 1424.786834349992887, 210.5240428619318322 ) ) ;
#6890 = CARTESIAN_POINT ( 'NONE',  ( 17.83371091504290007, 1414.294633887780037, 223.5299421325470064 ) ) ;
#6891 = CARTESIAN_POINT ( 'NONE',  ( -49.76313179303890166, 1384.741186450630039, 261.2525457107669808 ) ) ;
#6892 = CARTESIAN_POINT ( 'NONE',  ( -107.1386201206849904, 1391.913060387289988, 301.4226135078189941 ) ) ;
#6893 = B_SPLINE_CURVE_WITH_KNOTS ( 'NONE', 3,
 ( #74775, #5907, #57976, #14840, #90446, #49029, #50129, #15928, #30549, #92110 ),
 .UNSPECIFIED., .F., .F.,
 ( 4, 2, 2, 2, 4 ),
 ( 0.000000000000000000, 0.0007408354861221088392, 0.001481670972244217678, 0.002222506458366326626, 0.002963341944488435357 ),
 .UNSPECIFIED. ) ;
#6894 = CARTESIAN_POINT ( 'NONE',  ( -17.01308424645448980, 1414.913060581098534, 207.5694819292969271 ) ) ;
#6895 = CARTESIAN_POINT ( 'NONE',  ( -25.40163730124199759, 1470.069713657840111, 211.2641496062430235 ) ) ;
#6896 = CARTESIAN_POINT ( 'NONE',  ( 4.038582018749999669, 1515.598601288590089, 209.1218459616989946 ) ) ;
#6897 = CARTESIAN_POINT ( 'NONE',  ( 2.918143513847768445E-16, 1426.814114634534008, 137.0999999980979851 ) ) ;
#6898 = CARTESIAN_POINT ( 'NONE',  ( -22.18401561299999969, 1410.609167765330085, 202.6466877633079946 ) ) ;
#6899 = EDGE_CURVE ( 'NONE', #56418, #10960, #95872, .T. ) ;
#6900 = CARTESIAN_POINT ( 'NONE',  ( -9.709241970235968466, 1380.610007537143929, 201.4292193300254326 ) ) ;
#6901 = CARTESIAN_POINT ( 'NONE',  ( -15.97833203511600253, 1420.726030562786036, 227.0316138336059737 ) ) ;
#6902 = CARTESIAN_POINT ( 'NONE',  ( 10.53834095255740166, 1479.220444398180007, 206.2733528961080083 ) ) ;
#6903 = ORIENTED_EDGE ( 'NONE', *, *, #97405, .F. ) ;
#6904 = CARTESIAN_POINT ( 'NONE',  ( -4.107001541143308287, 1410.432827086315910, 232.1774397938114589 ) ) ;
#6905 = CARTESIAN_POINT ( 'NONE',  ( -9.488417199124221213, 1447.702184401620116, 190.7505744106450152 ) ) ;
#6907 = EDGE_CURVE ( 'NONE', #71433, #108182, #46276, .T. ) ;
#6906 = CARTESIAN_POINT ( 'NONE',  ( -7.550614507920475837, 1510.484595328588057, 214.6890571836817969 ) ) ;
#6908 = CARTESIAN_POINT ( 'NONE',  ( 4.602958218326069779E-16, 1426.918876943007945, 134.0999999980979851 ) ) ;
#6910 = CARTESIAN_POINT ( 'NONE',  ( -15.20279857216500119, 1514.921193539169963, 193.2119409213669883 ) ) ;
#6909 = CARTESIAN_POINT ( 'NONE',  ( 11.71693939160000042, 1426.292619179529993, 142.7697690241979842 ) ) ;
#6911 = CARTESIAN_POINT ( 'NONE',  ( -15.73574044604409927, 1409.462552572229924, 225.2910003602459881 ) ) ;
#6912 = CARTESIAN_POINT ( 'NONE',  ( -123.3741145675100057, 1345.325269380309919, 298.7729623350389829 ) ) ;
#6913 = EDGE_CURVE ( 'NONE', #72650, #43618, #16563, .T. ) ;
#6914 = CARTESIAN_POINT ( 'NONE',  ( 28.11203376910000173, 1444.250560465929993, 137.5208087134980133 ) ) ;
#6915 = CARTESIAN_POINT ( 'NONE',  ( -9.094910673856409389, 1384.931050598509955, 199.9427862989620053 ) ) ;
#6916 = CARTESIAN_POINT ( 'NONE',  ( -2.873329398885000163, 1516.572193931679976, 201.7997408644770019 ) ) ;
#6917 = DIRECTION ( 'NONE',  ( 0.000000000000000000, 1.000000000000000000, 0.000000000000000000 ) ) ;
#6918 = CARTESIAN_POINT ( 'NONE',  ( -7.615348975238497076, 1398.139300407672863, 198.4687090422606275 ) ) ;
#6919 = CARTESIAN_POINT ( 'NONE',  ( 16.88678280943500098, 1513.362623229679912, 196.1895945485670154 ) ) ;
#6920 = CARTESIAN_POINT ( 'NONE',  ( -22.90642118200990041, 1417.395382955499826, 209.8927238903939951 ) ) ;
#6921 = CARTESIAN_POINT ( 'NONE',  ( -41.40576702097160222, 1380.117442311619925, 227.6002273774099933 ) ) ;
#6922 = CARTESIAN_POINT ( 'NONE',  ( 20.82055072771269977, 1509.307918567249999, 229.0039304369510091 ) ) ;
#6924 = VERTEX_POINT ( 'NONE', #34506 ) ;
#6923 = CARTESIAN_POINT ( 'NONE',  ( -29.73889674292890106, 1379.618472333520003, 218.1103683386099874 ) ) ;
#6925 = ORIENTED_EDGE ( 'NONE', *, *, #9707, .T. ) ;
#6926 = CARTESIAN_POINT ( 'NONE',  ( 11.52705822141970060, 1434.294195329290005, 151.3489372875870060 ) ) ;
#6927 = CARTESIAN_POINT ( 'NONE',  ( -12.55568685759999958, 1398.285279232130051, 212.9384880290180320 ) ) ;
#6928 = CARTESIAN_POINT ( 'NONE',  ( -19.69385343140000444, 1409.600784903429940, 217.8674699180880054 ) ) ;
#6929 = ORIENTED_EDGE ( 'NONE', *, *, #3181, .T. ) ;
#6930 = CARTESIAN_POINT ( 'NONE',  ( -13.12297772262875029, 1444.782698483078320, 169.4025063443241095 ) ) ;
#6931 = CARTESIAN_POINT ( 'NONE',  ( 22.30235455686514712, 1509.698861494391622, 228.4320621754980607 ) ) ;
#6932 = DIRECTION ( 'NONE',  ( -6.123233995736769734E-17, -1.000000000000000000, -1.124819836996399911E-32 ) ) ;
#6934 = CARTESIAN_POINT ( 'NONE',  ( 17.71884614950000270, 1424.302129513130012, 226.3668682875980096 ) ) ;
#6933 = CARTESIAN_POINT ( 'NONE',  ( 1.581901184577762853, 1426.946688134061105, 137.0999999980979851 ) ) ;
#6935 = CARTESIAN_POINT ( 'NONE',  ( 0.5045109264089999712, 1429.776885342730111, 184.2481756784980291 ) ) ;
#6936 = CARTESIAN_POINT ( 'NONE',  ( -9.507368510479999202, 1414.971339025629959, 194.7268509206979843 ) ) ;
#6937 = CARTESIAN_POINT ( 'NONE',  ( -17.34523078839999854, 1417.790224563129868, 207.1689930853989949 ) ) ;
#6938 =( NAMED_UNIT ( * ) PLANE_ANGLE_UNIT ( ) SI_UNIT ( $, .RADIAN. ) );
#6939 = B_SPLINE_SURFACE_WITH_KNOTS ( 'NONE', 5, 5, ( 
 ( #24378, #6490, #84831, #109509, #74813, #40641, #108959, #100542, #41200 ),
 ( #15421, #23277, #101624, #23822, #58013, #75902, #31683, #84297, #92692 ),
 ( #49613, #42297, #15967, #8131, #50700, #99985, #57473, #91598, #42860 ),
 ( #32246, #24913, #49066, #32785, #68082, #83201, #76449, #17053, #92149 ),
 ( #51250, #66969, #101079, #75370, #66426, #83745, #7041, #14874, #58562 ),
 ( #50170, #7588, #102193, #65865, #41743, #110604, #59122, #110054, #33328 ) ),
 .UNSPECIFIED., .F., .F., .F.,
 ( 6, 6 ),
 ( 6, 3, 6 ),
 ( 0.4666582264849999939, 2.797885342226240191 ),
 ( -1.082960624482799909E-05, 1.000000000000000000, 2.000000000000000000 ),
 .UNSPECIFIED. ) ;
#6940 = CARTESIAN_POINT ( 'NONE',  ( 8.265387638122250635, 1396.201694164710034, 201.7848193804910011 ) ) ;
#6941 = CARTESIAN_POINT ( 'NONE',  ( 2.500000000000000000, 1419.503957648720871, 138.2096356918212905 ) ) ;
#6942 = CARTESIAN_POINT ( 'NONE',  ( 10.95984484989999963, 1431.648774854440035, 151.7380654299980165 ) ) ;
#6943 = CARTESIAN_POINT ( 'NONE',  ( 8.207084954655000431, 1512.038636172079805, 202.7922115676269925 ) ) ;
#6944 = ORIENTED_EDGE ( 'NONE', *, *, #64219, .T. ) ;
#6945 = CARTESIAN_POINT ( 'NONE',  ( 13.51212582107970128, 1435.883254532899855, 150.4097860975269896 ) ) ;
#6946 = ORIENTED_EDGE ( 'NONE', *, *, #78980, .F. ) ;
#6947 = VERTEX_POINT ( 'NONE', #42352 ) ;
#6948 = CARTESIAN_POINT ( 'NONE',  ( -19.64522922078770151, 1497.936653429400167, 228.8931875647859897 ) ) ;
#6949 = CARTESIAN_POINT ( 'NONE',  ( -10.87454802859999781, 1463.204792800929908, 232.0658476886979713 ) ) ;
#6950 = VECTOR ( 'NONE', #66871, 1000.000000000000000 ) ;
#6951 = CARTESIAN_POINT ( 'NONE',  ( -108.9749535673422116, 1387.771090604488109, 310.7965837917592467 ) ) ;
#6952 = CARTESIAN_POINT ( 'NONE',  ( 6.943602653455000606, 1516.858069504249897, 216.0629462479770098 ) ) ;
#6953 = CARTESIAN_POINT ( 'NONE',  ( -7.943222529415674416, 1511.827399570821171, 212.3015523490330452 ) ) ;
#6954 = B_SPLINE_SURFACE_WITH_KNOTS ( 'NONE', 3, 5, ( 
 ( #76204, #110349, #33625, #11221, #71712, #28558 ),
 ( #80617, #37508, #21774, #47030, #20142, #3380 ),
 ( #45384, #105830, #62756, #55428, #3933, #29108 ),
 ( #81155, #54337, #63294, #38060, #4470, #11753 ) ),
 .UNSPECIFIED., .F., .F., .F.,
 ( 4, 4 ),
 ( 6, 6 ),
 ( 5.479561955150000330, 5.505632801049999969 ),
 ( 0.000000000000000000, 1.000000000000000000 ),
 .UNSPECIFIED. ) ;
#6955 = AXIS2_PLACEMENT_3D ( 'NONE', #33066, #85671, #76183 ) ;
#6956 = ORIENTED_EDGE ( 'NONE', *, *, #106940, .F. ) ;
#6957 = CARTESIAN_POINT ( 'NONE',  ( -11.40807687090000044, 1502.267969405689882, 207.7237911178790171 ) ) ;
#6958 = FACE_OUTER_BOUND ( 'NONE', #84212, .T. ) ;
#6959 = CARTESIAN_POINT ( 'NONE',  ( -7.611657828400000270, 1376.295363933120143, 206.9293838565190242 ) ) ;
#6960 = TOROIDAL_SURFACE ( 'NONE', #96319, 32.13701971169416538, 1.000000000000000000 ) ;
#6961 = ORIENTED_EDGE ( 'NONE', *, *, #85737, .F. ) ;
#6962 = CARTESIAN_POINT ( 'NONE',  ( -3.461360131404999763, 1516.874084700499907, 205.8683838714370040 ) ) ;
#6963 = ORIENTED_EDGE ( 'NONE', *, *, #69228, .F. ) ;
#6964 = CARTESIAN_POINT ( 'NONE',  ( 4.618583391875000110, 1516.939762005280045, 209.1087859301640322 ) ) ;
#6965 = CARTESIAN_POINT ( 'NONE',  ( -7.977617884082539135, 1452.731462069070176, 204.2954127766810188 ) ) ;
#6966 = CARTESIAN_POINT ( 'NONE',  ( -12.21036482539999923, 1409.841853000129959, 189.5541482494979846 ) ) ;
#6967 = CARTESIAN_POINT ( 'NONE',  ( -2.261018246749999960, 1409.497062291729890, 232.5268568490979817 ) ) ;
#6969 = VERTEX_POINT ( 'NONE', #92205 ) ;
#6968 = CARTESIAN_POINT ( 'NONE',  ( -0.6362176846849959544, 1414.913060387399810, 225.3300418929160003 ) ) ;
#6970 = CARTESIAN_POINT ( 'NONE',  ( 19.06118660449999780, 1425.780408082830036, 222.6829976502980060 ) ) ;
#6971 = CARTESIAN_POINT ( 'NONE',  ( 19.63722818192610120, 1522.051704408389924, 218.2362632616380154 ) ) ;
#6972 = CARTESIAN_POINT ( 'NONE',  ( -86.94413116030000310, 1384.337889815429889, 307.7010151988590110 ) ) ;
#6974 = EDGE_CURVE ( 'NONE', #6784, #50075, #13600, .T. ) ;
#6973 = CARTESIAN_POINT ( 'NONE',  ( -0.1209835420493560049, 1465.026716009449956, 237.7730318938839957 ) ) ;
#6975 = CIRCLE ( 'NONE', #62409, 1.000000000000000888 ) ;
#6976 = EDGE_CURVE ( 'NONE', #11504, #106239, #107717, .T. ) ;
#6977 = CARTESIAN_POINT ( 'NONE',  ( 7.520399230329999796, 1408.700311873330065, 270.3839821972980531 ) ) ;
#6978 = CARTESIAN_POINT ( 'NONE',  ( -6.549762485114999144, 1516.729202374750002, 213.7405950387170037 ) ) ;
#6979 = CARTESIAN_POINT ( 'NONE',  ( 23.98652862120000151, 1410.713095165929872, 208.5703825711269985 ) ) ;
#6980 = CARTESIAN_POINT ( 'NONE',  ( -2.500574544111449971, 1448.942056179399970, 154.5733147259969940 ) ) ;
#6981 = CARTESIAN_POINT ( 'NONE',  ( 16.69693468393730029, 1428.155315606670001, 202.0365457747359699 ) ) ;
#6982 = CARTESIAN_POINT ( 'NONE',  ( 7.167019213315450443, 1508.551563895499839, 214.6350865034499691 ) ) ;
#6983 = CARTESIAN_POINT ( 'NONE',  ( 1.718203463455000080, 1516.898441858519845, 210.8221056461869978 ) ) ;
#6984 = CARTESIAN_POINT ( 'NONE',  ( -21.82415348264071753, 1524.756004293092019, 233.6168747274685700 ) ) ;
#6985 = CARTESIAN_POINT ( 'NONE',  ( 0.2691385670090000182, 1419.231489590830051, 184.6448893939979996 ) ) ;
#6986 = CARTESIAN_POINT ( 'NONE',  ( 2.456308003337250412, 1421.792674159936951, 137.0999999980978714 ) ) ;
#6988 = VERTEX_POINT ( 'NONE', #67579 ) ;
#6987 = CARTESIAN_POINT ( 'NONE',  ( -57.13410461910000038, 1390.772211217349877, 257.4385327720589771 ) ) ;
#6989 = CARTESIAN_POINT ( 'NONE',  ( -44.92722774579330292, 1385.152941095250071, 251.3752464619300042 ) ) ;
#6990 = EDGE_CURVE ( 'NONE', #87156, #95283, #30152, .T. ) ;
#6991 = CARTESIAN_POINT ( 'NONE',  ( 7.132065395029999699, 1475.995241008230096, 267.2559760689979953 ) ) ;
#6992 = DIRECTION ( 'NONE',  ( 0.000000000000000000, -1.000000000000000000, 0.000000000000000000 ) ) ;
#6993 = CARTESIAN_POINT ( 'NONE',  ( -2.361220391463635160, 1495.123712929674411, 220.0409822458833844 ) ) ;
#6994 = CARTESIAN_POINT ( 'NONE',  ( 6.104420695803289831, 1484.441873671279836, 218.1702592719159952 ) ) ;
#6995 = FACE_OUTER_BOUND ( 'NONE', #19469, .T. ) ;
#6996 = CARTESIAN_POINT ( 'NONE',  ( 0.8010214712846820406, 1452.931212010089894, 183.3398705925079923 ) ) ;
#6998 = CARTESIAN_POINT ( 'NONE',  ( -7.544733521170000401, 1384.899971913130003, 219.0877090843589770 ) ) ;
#6997 = DIRECTION ( 'NONE',  ( -0.9455185755993178454, 0.000000000000000000, 0.3255681544571539243 ) ) ;
#6999 = CARTESIAN_POINT ( 'NONE',  ( -10.35382106464290075, 1447.820467530350015, 209.5541548230679894 ) ) ;
#7000 = CARTESIAN_POINT ( 'NONE',  ( 31.40702543711093497, 1523.611961620354123, 221.9096305968278671 ) ) ;
#7001 = VERTEX_POINT ( 'NONE', #8186 ) ;
#7002 = CARTESIAN_POINT ( 'NONE',  ( -2.873958889724999910, 1516.588006113850042, 202.1873174023370154 ) ) ;
#7003 = CARTESIAN_POINT ( 'NONE',  ( 11.93818824289999903, 1433.480083226980014, 149.8972169559980046 ) ) ;
#7004 = CARTESIAN_POINT ( 'NONE',  ( 15.81201445386249915, 1506.433683730510211, 224.3933755863170063 ) ) ;
#7005 = AXIS2_PLACEMENT_3D ( 'NONE', #80933, #4231, #38365 ) ;
#7006 = EDGE_CURVE ( 'NONE', #21616, #44160, #62344, .T. ) ;
#7007 = CARTESIAN_POINT ( 'NONE',  ( 22.75126231049999959, 1450.312999748930224, 218.7949445992479980 ) ) ;
#7008 = CARTESIAN_POINT ( 'NONE',  ( 10.80995225166140017, 1461.830262730540198, 211.0065464265690025 ) ) ;
#7009 = LINE ( 'NONE', #41167, #18058 ) ;
#7010 = CARTESIAN_POINT ( 'NONE',  ( 26.81178797887219645, 1450.703257649033958, 136.4517338180884849 ) ) ;
#7011 = CARTESIAN_POINT ( 'NONE',  ( 3.918670472299999208, 1441.329835342249908, 183.9132893515979958 ) ) ;
#7012 = EDGE_CURVE ( 'NONE', #23487, #86024, #109392, .T. ) ;
#7013 = CARTESIAN_POINT ( 'NONE',  ( 29.16088018400000337, 1435.515811254470009, 135.2139231482979937 ) ) ;
#7014 = VECTOR ( 'NONE', #48384, 1000.000000000000000 ) ;
#7015 = CARTESIAN_POINT ( 'NONE',  ( 38.22332642270760061, 1448.618965483920192, 136.4075853064549904 ) ) ;
#7016 = CARTESIAN_POINT ( 'NONE',  ( -23.53722878629999826, 1435.319033575220146, 213.4336055579080380 ) ) ;
#7017 = CARTESIAN_POINT ( 'NONE',  ( -12.78776258895079998, 1416.851343896850040, 195.5391574246120001 ) ) ;
#7018 = CARTESIAN_POINT ( 'NONE',  ( -108.7811652620000018, 1387.776015447450163, 297.7301139582590395 ) ) ;
#7019 = CARTESIAN_POINT ( 'NONE',  ( 10.17004918770000010, 1507.385806824230031, 183.8335291379979992 ) ) ;
#7020 = CARTESIAN_POINT ( 'NONE',  ( 3.775314256393730084, 1507.374707593759922, 220.2027404254530154 ) ) ;
#7021 = CARTESIAN_POINT ( 'NONE',  ( -2.751978043620916026, 1471.436294014188888, 269.3346704505487992 ) ) ;
#7022 = ORIENTED_EDGE ( 'NONE', *, *, #26100, .F. ) ;
#7023 = CARTESIAN_POINT ( 'NONE',  ( -8.377772372675931223, 1439.624752306900064, 206.1459263295090238 ) ) ;
#7024 = CARTESIAN_POINT ( 'NONE',  ( -42.08860907271759544, 1427.691514611570938, 269.0733891839905141 ) ) ;
#7025 = ADVANCED_FACE ( 'NONE', ( #95518 ), #26815, .T. ) ;
#7026 = B_SPLINE_CURVE_WITH_KNOTS ( 'NONE', 5,
 ( #86304, #104763, #105314, #44321, #45433, #28048, #96364, #19643, #53846, #2881, #87983, #79577 ),
 .UNSPECIFIED., .F., .F.,
 ( 6, 3, 3, 6 ),
 ( 0.000000000000000000, 0.5093891872483979899, 0.7698042424308239040, 1.000000000000000000 ),
 .UNSPECIFIED. ) ;
#7027 = CARTESIAN_POINT ( 'NONE',  ( -4.159863671365049420, 1508.728286123109910, 213.5483371690740171 ) ) ;
#7028 = CARTESIAN_POINT ( 'NONE',  ( -5.192567649020000786, 1483.459673190490093, 199.8090161968289635 ) ) ;
#7029 = CARTESIAN_POINT ( 'NONE',  ( -15.02666660005860244, 1451.829519320988311, 222.9333663745973411 ) ) ;
#7030 = CARTESIAN_POINT ( 'NONE',  ( -13.10582615840648479, 1444.796545787240802, 186.4375160407790588 ) ) ;
#7031 = CARTESIAN_POINT ( 'NONE',  ( -8.589403565197139656, 1436.797923814430078, 209.9038308123180059 ) ) ;
#7032 = CARTESIAN_POINT ( 'NONE',  ( 16.48231804958387059, 1525.661276915132476, 181.5746648898756348 ) ) ;
#7033 = VECTOR ( 'NONE', #94551, 1000.000000000000000 ) ;
#7034 = EDGE_CURVE ( 'NONE', #92642, #40565, #91648, .T. ) ;
#7035 = CARTESIAN_POINT ( 'NONE',  ( -4.037103925677953953, 1415.961567342583521, 232.4510850075154451 ) ) ;
#7036 = CARTESIAN_POINT ( 'NONE',  ( -16.26938466631711933, 1451.108877157205370, 148.8960758721039781 ) ) ;
#7037 = CARTESIAN_POINT ( 'NONE',  ( 25.69726023690000005, 1436.490352274229963, 137.0663831747980055 ) ) ;
#7038 = CARTESIAN_POINT ( 'NONE',  ( -12.80739992162959240, 1442.848094250957729, 169.4485940490470739 ) ) ;
#7040 = ORIENTED_EDGE ( 'NONE', *, *, #102955, .T. ) ;
#7039 = CARTESIAN_POINT ( 'NONE',  ( 18.01711958838799887, 1424.180322377740140, 225.4683465207770041 ) ) ;
#7041 = CARTESIAN_POINT ( 'NONE',  ( -0.2033579075130829972, 1416.218865267220053, 191.1379978179999739 ) ) ;
#7042 = CARTESIAN_POINT ( 'NONE',  ( -11.90005270625540135, 1409.328619384790045, 226.7881248095609976 ) ) ;
#7043 = EDGE_LOOP ( 'NONE', ( #96909, #88078, #105508, #32308 ) ) ;
#7044 = ORIENTED_EDGE ( 'NONE', *, *, #97353, .T. ) ;
#7045 = CARTESIAN_POINT ( 'NONE',  ( 17.19251027932519804, 1415.089118586289942, 209.7053761061400223 ) ) ;
#7046 = B_SPLINE_CURVE_WITH_KNOTS ( 'NONE', 3,
 ( #68412, #102515, #67306, #25252, #7916, #109841, #58890, #93023, #16295, #84621, #51041, #50499, #42087, #110383, #76236, #59455, #16840, #101966, #57943, #6424, #23205, #48444, #14808, #31611, #109442, #6965, #73082, #82583, #57404, #15348, #38899, #39473, #90966, #101009, #92075, #40016, #107222, #107774, #30511, #64700, #74196, #98818, #49543 ),
 .UNSPECIFIED., .F., .F.,
 ( 4, 3, 3, 3, 3, 3, 3, 3, 3, 3, 3, 3, 3, 3, 4 ),
 ( -31.90163827269670094, -31.43425787619030132, -29.98858318685319801, -28.53496177318270099, -27.07797101134740103, -26.89876598673080110, -25.44723142269879901, -23.99928790089909825, -22.55496867767820035, -21.04730123312180012, -19.61770596032359748, -18.19541948610630300, -16.78105471453919861, -15.31006667213799943, -13.91937871329999865 ),
 .UNSPECIFIED. ) ;
#7047 = CARTESIAN_POINT ( 'NONE',  ( -8.861482052969998691, 1384.950957082100103, 218.6848127019790127 ) ) ;
#7049 = CARTESIAN_POINT ( 'NONE',  ( -20.54560411990000190, 1453.269583021529797, 220.8539909785980058 ) ) ;
#7048 = CARTESIAN_POINT ( 'NONE',  ( 2.216729547819999979, 1455.498911564990067, 218.4410051553589938 ) ) ;
#7050 = CARTESIAN_POINT ( 'NONE',  ( -2.090539597859999876, 1443.965784278489764, 218.2184972947390236 ) ) ;
#7051 = ADVANCED_FACE ( 'NONE', ( #12619 ), #8245, .T. ) ;
#7052 = CARTESIAN_POINT ( 'NONE',  ( -11.86372866770000023, 1433.130351995409910, 150.2717319648980094 ) ) ;
#7053 = CARTESIAN_POINT ( 'NONE',  ( -44.32302097390000029, 1380.083786706710043, 232.1686497034590104 ) ) ;
#7054 = CIRCLE ( 'NONE', #23108, 39.03564169359999170 ) ;
#7055 = CARTESIAN_POINT ( 'NONE',  ( 14.35058941227343077, 1519.551704408389924, 224.2459111387558437 ) ) ;
#7056 = CARTESIAN_POINT ( 'NONE',  ( 7.535764321409999411, 1423.202263985780064, 213.6586556354689890 ) ) ;
#7058 = EDGE_CURVE ( 'NONE', #109848, #72154, #27937, .T. ) ;
#7057 = CARTESIAN_POINT ( 'NONE',  ( -12.77587743780000018, 1416.568813547830132, 195.5427461491979955 ) ) ;
#7059 = FACE_BOUND ( 'NONE', #66429, .T. ) ;
#7060 = CARTESIAN_POINT ( 'NONE',  ( 3.057433871810000259, 1450.174788091120035, 183.8252404729979901 ) ) ;
#7061 = CARTESIAN_POINT ( 'NONE',  ( 7.787085240219187909, 1364.374563602181297, 208.3718459617061285 ) ) ;
#7062 = CARTESIAN_POINT ( 'NONE',  ( -21.39654334329791396, 1509.777343320284899, 230.1584121880257783 ) ) ;
#7064 = ORIENTED_EDGE ( 'NONE', *, *, #83873, .F. ) ;
#7063 = CARTESIAN_POINT ( 'NONE',  ( -2.296399283793280044E-09, 1415.822370859000102, 241.4911618200540033 ) ) ;
#7065 = VERTEX_POINT ( 'NONE', #72011 ) ;
#7066 = CARTESIAN_POINT ( 'NONE',  ( -11.82359547739990013, 1429.509793761799983, 149.2101411770329946 ) ) ;
#7067 = CARTESIAN_POINT ( 'NONE',  ( 14.00740487959999925, 1500.888346221290021, 227.6900866534990087 ) ) ;
#7068 = CARTESIAN_POINT ( 'NONE',  ( -5.402393449050000740, 1473.936434490630063, 270.1311850751980046 ) ) ;
#7069 = CARTESIAN_POINT ( 'NONE',  ( -10.76610293753739889, 1461.751116445120033, 211.3389343603909936 ) ) ;
#7070 = CARTESIAN_POINT ( 'NONE',  ( -126.6653580272000283, 1320.102705746890024, 317.4872039844593132 ) ) ;
#7071 = CARTESIAN_POINT ( 'NONE',  ( 38.63621758546330653, 1450.019455539890032, 134.8311675663850053 ) ) ;
#7072 = CIRCLE ( 'NONE', #21347, 19.90662746966999919 ) ;
#7073 = CARTESIAN_POINT ( 'NONE',  ( -13.71477132504269925, 1421.034959706790005, 222.0387691072829739 ) ) ;
#7074 = CARTESIAN_POINT ( 'NONE',  ( -8.156254627529998302, 1384.896657259020003, 199.6468325161289954 ) ) ;
#7075 = CARTESIAN_POINT ( 'NONE',  ( 9.919384991629041082, 1468.593841060750037, 207.7518384896150110 ) ) ;
#7076 = DIRECTION ( 'NONE',  ( -0.000000000000000000, -1.000000000000000000, -0.000000000000000000 ) ) ;
#7077 = CARTESIAN_POINT ( 'NONE',  ( 11.16357413047867730, 1367.453876867194367, 209.6218459617033432 ) ) ;
#7078 = CARTESIAN_POINT ( 'NONE',  ( -8.361732071192520266, 1406.610899605839904, 269.0188235946120585 ) ) ;
#7079 = ORIENTED_EDGE ( 'NONE', *, *, #40772, .F. ) ;
#7080 = CARTESIAN_POINT ( 'NONE',  ( 2.485517042439642221, 1524.599984580802357, 242.5124281696222965 ) ) ;
#7081 = B_SPLINE_SURFACE_WITH_KNOTS ( 'NONE', 5, 1, ( 
 ( #86287, #79020 ),
 ( #19626, #1202 ),
 ( #96349, #35335 ),
 ( #10133, #62790 ),
 ( #11257, #44305 ),
 ( #19059, #78448 ) ),
 .UNSPECIFIED., .F., .F., .F.,
 ( 6, 6 ),
 ( 2, 2 ),
 ( 0.000000000000000000, 3.595663933400000012 ),
 ( 0.000000000000000000, 14.00000000000000000 ),
 .UNSPECIFIED. ) ;
#7082 = VERTEX_POINT ( 'NONE', #73647 ) ;
#7083 = ORIENTED_EDGE ( 'NONE', *, *, #54592, .T. ) ;
#7084 = CARTESIAN_POINT ( 'NONE',  ( -1.701729858475000023, 1516.969638403840008, 212.0041719496170174 ) ) ;
#7085 = CARTESIAN_POINT ( 'NONE',  ( 4.974056298193653802, 1423.234490133592544, 184.3173436926480520 ) ) ;
#7086 = CARTESIAN_POINT ( 'NONE',  ( 7.705921152320070355, 1424.884187513139977, 194.3337803165900084 ) ) ;
#7088 = CARTESIAN_POINT ( 'NONE',  ( -2.571340789771010549, 1440.211241685782170, 170.5281974536487439 ) ) ;
#7087 = CARTESIAN_POINT ( 'NONE',  ( -7.710285875814999912, 1516.582197289609894, 212.3822242253069987 ) ) ;
#7089 = CARTESIAN_POINT ( 'NONE',  ( -18.39440931229999876, 1485.488557115530057, 189.1449212182980091 ) ) ;
#7090 = CARTESIAN_POINT ( 'NONE',  ( -17.34910718890199988, 1498.334872555480160, 229.4722646656200027 ) ) ;
#7091 = B_SPLINE_SURFACE_WITH_KNOTS ( 'NONE', 4, 5, ( 
 ( #80441, #97227, #64203, #72594, #19401, #37334 ),
 ( #4291, #53604, #105085, #45755, #55809, #89385 ),
 ( #71530, #46856, #89926, #28374, #87748, #105650 ),
 ( #106722, #96693, #3206, #11578, #45197, #28935 ),
 ( #30013, #13201, #21604, #78783, #36225, #63125 ) ),
 .UNSPECIFIED., .F., .F., .F.,
 ( 5, 5 ),
 ( 6, 6 ),
 ( 0.8555274230859999385, 1.128731558089999920 ),
 ( 0.000000000000000000, 2.000000000000000000 ),
 .UNSPECIFIED. ) ;
#7092 = ORIENTED_EDGE ( 'NONE', *, *, #89715, .F. ) ;
#7093 = CARTESIAN_POINT ( 'NONE',  ( -109.5441724459999904, 1379.129497135580095, 302.6503169382589817 ) ) ;
#7094 = CARTESIAN_POINT ( 'NONE',  ( 2.290256263724999908, 1517.170721208160103, 202.1706708033170230 ) ) ;
#7095 = TOROIDAL_SURFACE ( 'NONE', #69718, 3.000000000000000000, 0.5000000000000000000 ) ;
#7096 = B_SPLINE_SURFACE_WITH_KNOTS ( 'NONE', 4, 5, ( 
 ( #2735, #3286, #105735, #96778, #72681, #20049 ),
 ( #4372, #72149, #11659, #71615, #45834, #79968 ),
 ( #29019, #63205, #97312, #106268, #29554, #63739 ),
 ( #106805, #30095, #64290, #109036, #23351, #48022 ),
 ( #91115, #40162, #22228, #108471, #31207, #24443 ) ),
 .UNSPECIFIED., .F., .F., .F.,
 ( 5, 5 ),
 ( 6, 6 ),
 ( 29.43575841650000058, 48.27399281030000111 ),
 ( -1.387778780779999841E-17, 1.000000000000000000 ),
 .UNSPECIFIED. ) ;
#7097 = CARTESIAN_POINT ( 'NONE',  ( 10.27486387009999902, 1471.877390917489947, 213.0768048428889756 ) ) ;
#7098 = CARTESIAN_POINT ( 'NONE',  ( -40.95419143721069588, 1384.585776280029904, 213.8410145222069900 ) ) ;
#7099 = CARTESIAN_POINT ( 'NONE',  ( -41.51852662024420226, 1431.123461163979982, 270.1901905831499562 ) ) ;
#7100 = B_SPLINE_CURVE_WITH_KNOTS ( 'NONE', 3,
 ( #67459, #93175, #16445, #8069 ),
 .UNSPECIFIED., .F., .F.,
 ( 4, 4 ),
 ( 0.000000000000000000, 1.000000000000000000 ),
 .UNSPECIFIED. ) ;
#7101 = CARTESIAN_POINT ( 'NONE',  ( -24.18363701780000241, 1464.258769156330118, 212.1671259816380086 ) ) ;
#7102 = AXIS2_PLACEMENT_3D ( 'NONE', #12045, #30492, #45680 ) ;
#7104 = ORIENTED_EDGE ( 'NONE', *, *, #62690, .F. ) ;
#7103 = DIRECTION ( 'NONE',  ( 0.000000000000000000, 1.000000000000000000, 0.000000000000000000 ) ) ;
#7105 = ORIENTED_EDGE ( 'NONE', *, *, #75513, .F. ) ;
#7106 = CARTESIAN_POINT ( 'NONE',  ( 5.826685344680000433, 1451.766759332889933, 210.9235202141190086 ) ) ;
#7107 = CARTESIAN_POINT ( 'NONE',  ( 3.771101265954107884, 1425.575893895815852, 185.2173869927980832 ) ) ;
#7108 = CARTESIAN_POINT ( 'NONE',  ( 1.353590696506990154, 1425.853514710840045, 191.1378424660090047 ) ) ;
#7109 = ADVANCED_FACE ( 'NONE', ( #54651 ), #9835, .T. ) ;
#7110 = CARTESIAN_POINT ( 'NONE',  ( -24.40603932400000176, 1441.493461285830108, 212.0691197944780129 ) ) ;
#7112 = CARTESIAN_POINT ( 'NONE',  ( -2.282622950494999969, 1516.861367446839949, 211.4218295478370067 ) ) ;
#7111 = CIRCLE ( 'NONE', #109032, 0.9999999999999880096 ) ;
#7113 = CARTESIAN_POINT ( 'NONE',  ( 5.398404081564367019, 1459.746910339853230, 201.1147253787919169 ) ) ;
#7114 = CARTESIAN_POINT ( 'NONE',  ( -0.07726447814961530380, 1452.995338318107770, 183.2382765434469434 ) ) ;
#7115 = FACE_OUTER_BOUND ( 'NONE', #38780, .T. ) ;
#7116 = CARTESIAN_POINT ( 'NONE',  ( 18.80463396749128435, 1425.801069675071858, 225.6039139557115902 ) ) ;
#7117 = CARTESIAN_POINT ( 'NONE',  ( 1.700706776364999895, 1516.923170579120097, 206.8211163054370161 ) ) ;
#7118 = ORIENTED_EDGE ( 'NONE', *, *, #44010, .T. ) ;
#7119 = DIRECTION ( 'NONE',  ( 0.000000000000000000, -1.000000000000000000, 6.123233995736769734E-17 ) ) ;
#7120 = CARTESIAN_POINT ( 'NONE',  ( -11.27244568259999902, 1471.218590734589952, 207.2933119717289969 ) ) ;
#7121 = CARTESIAN_POINT ( 'NONE',  ( -19.87427776918198674, 1456.662545660512478, 225.4134381264325668 ) ) ;
#7122 = ORIENTED_EDGE ( 'NONE', *, *, #33674, .F. ) ;
#7123 = CARTESIAN_POINT ( 'NONE',  ( 7.331631502509999621, 1481.335631838190011, 208.7201577476780017 ) ) ;
#7124 = EDGE_CURVE ( 'NONE', #52007, #105623, #98821, .T. ) ;
#7125 = CARTESIAN_POINT ( 'NONE',  ( 12.92481085168819988, 1434.740917461700064, 149.3164734981210131 ) ) ;
#7126 = CARTESIAN_POINT ( 'NONE',  ( 6.152613576320070443, 1468.998513094850068, 233.7412649376300067 ) ) ;
#7127 = CARTESIAN_POINT ( 'NONE',  ( -17.64296983559999887, 1417.255069634780057, 208.0149687280789976 ) ) ;
#7128 = CARTESIAN_POINT ( 'NONE',  ( 12.78690713350000152, 1416.828040475229955, 222.7042044314979989 ) ) ;
#7129 = EDGE_CURVE ( 'NONE', #77376, #31615, #18258, .T. ) ;
#7130 = CARTESIAN_POINT ( 'NONE',  ( 7.000551371890000318, 1488.139301625489907, 200.2663657335290281 ) ) ;
#7131 = CARTESIAN_POINT ( 'NONE',  ( 4.026786250540000722, 1422.913060387330006, 179.4243885131980107 ) ) ;
#7132 = CARTESIAN_POINT ( 'NONE',  ( 10.92857032808210072, 1460.888924644350027, 208.5047758900509791 ) ) ;
#7133 = CIRCLE ( 'NONE', #69751, 1.999999999999995559 ) ;
#7135 = CARTESIAN_POINT ( 'NONE',  ( -11.86590139589999815, 1432.348266868109931, 151.0567667964980103 ) ) ;
#7134 = CARTESIAN_POINT ( 'NONE',  ( -6.937338783705000012, 1516.706638732659940, 213.7399656364970042 ) ) ;
#7136 = CARTESIAN_POINT ( 'NONE',  ( 18.25280056480000113, 1432.153207019990077, 210.9297336666290050 ) ) ;
#7137 = CARTESIAN_POINT ( 'NONE',  ( 6.555393117025000826, 1516.809497469189864, 216.4498952504870033 ) ) ;
#7138 = VERTEX_POINT ( 'NONE', #15353 ) ;
#7139 = DIRECTION ( 'NONE',  ( -9.462326934583649054E-47, 1.000000000000000000, -1.836970198721029688E-16 ) ) ;
#7140 = CARTESIAN_POINT ( 'NONE',  ( 15.87406479873239995, 1409.467378496833362, 192.9778776010643071 ) ) ;
#7141 = CARTESIAN_POINT ( 'NONE',  ( 0.8259447189419999447, 1418.827400219930041, 184.7842358559980198 ) ) ;
#7142 = DIRECTION ( 'NONE',  ( 0.000000000000000000, 1.000000000000000000, 0.000000000000000000 ) ) ;
#7143 = CARTESIAN_POINT ( 'NONE',  ( 2.691662542991876794, 1524.776010967675802, 176.4305926583369342 ) ) ;
#7144 = CARTESIAN_POINT ( 'NONE',  ( -2.023054527036900030, 1423.041924723330112, 191.3215604683840070 ) ) ;
#7145 = CARTESIAN_POINT ( 'NONE',  ( -11.36893632117620001, 1470.999913913189857, 208.1399306574149932 ) ) ;
#7146 = CARTESIAN_POINT ( 'NONE',  ( -6.565194752462199190, 1508.347353571651638, 219.9240066229079105 ) ) ;
#7147 = CIRCLE ( 'NONE', #28654, 0.9999999999999987788 ) ;
#7148 = FACE_OUTER_BOUND ( 'NONE', #67438, .T. ) ;
#7149 = ADVANCED_FACE ( 'NONE', ( #16987 ), #35774, .F. ) ;
#7150 = CARTESIAN_POINT ( 'NONE',  ( -3.958338178574812627, 1515.551704408389696, 210.9648098108357033 ) ) ;
#7151 = CARTESIAN_POINT ( 'NONE',  ( 37.28204567502979927, 1440.913060386509869, 255.1050374929049838 ) ) ;
#7153 = CARTESIAN_POINT ( 'NONE',  ( 4.328426199472190206, 1515.103843506339899, 208.0564445731249918 ) ) ;
#7152 = CARTESIAN_POINT ( 'NONE',  ( -10.13174304484510024, 1472.026935049100075, 209.9584671908849884 ) ) ;
#7154 = CARTESIAN_POINT ( 'NONE',  ( 13.31375889959999803, 1429.098084184829986, 222.1181957922979961 ) ) ;
#7155 = ORIENTED_EDGE ( 'NONE', *, *, #24852, .F. ) ;
#7156 = ADVANCED_FACE ( 'NONE', ( #40572 ), #63763, .T. ) ;
#7157 = ORIENTED_EDGE ( 'NONE', *, *, #63723, .T. ) ;
#7158 = EDGE_CURVE ( 'NONE', #36610, #41661, #55585, .T. ) ;
#7159 = CARTESIAN_POINT ( 'NONE',  ( -19.64841113585741539, 1485.306958117290833, 190.2729878873239215 ) ) ;
#7160 = DIRECTION ( 'NONE',  ( 1.755985294532469921E-16, -1.000000000000000000, 1.338183447452831989E-16 ) ) ;
#7161 = FACE_OUTER_BOUND ( 'NONE', #10061, .T. ) ;
#7162 = CARTESIAN_POINT ( 'NONE',  ( 2.483039259372770591, 1508.999772102527686, 238.0619777347729666 ) ) ;
#7163 = CARTESIAN_POINT ( 'NONE',  ( -3.321447364419999548, 1484.261043626330093, 183.3707343507980170 ) ) ;
#7164 = ADVANCED_FACE ( 'NONE', ( #19210 ), #103709, .F. ) ;
#7165 = CARTESIAN_POINT ( 'NONE',  ( -30.31052258194577576, 1523.604703353109699, 222.4930856806593908 ) ) ;
#7166 = CARTESIAN_POINT ( 'NONE',  ( 17.61183580542134663, 1523.982201850120191, 180.5695639321423300 ) ) ;
#7167 = CARTESIAN_POINT ( 'NONE',  ( -68.31774780045299167, 1383.786899405800114, 292.8199513039460271 ) ) ;
#7168 = CARTESIAN_POINT ( 'NONE',  ( -13.90870118630000007, 1453.159462792929844, 194.1873857778979868 ) ) ;
#7169 = DIRECTION ( 'NONE',  ( 0.000000000000000000, -1.000000000000000000, -0.000000000000000000 ) ) ;
#7170 = CARTESIAN_POINT ( 'NONE',  ( 12.27488635486660051, 1492.418620469620009, 210.4946640001330138 ) ) ;
#7172 = EDGE_LOOP ( 'NONE', ( #88279, #42626, #45662, #531 ) ) ;
#7171 = CARTESIAN_POINT ( 'NONE',  ( 0.3560709500229989888, 1455.537836849089899, 218.5814834089789827 ) ) ;
#7173 = FACE_OUTER_BOUND ( 'NONE', #86809, .T. ) ;
#7174 = AXIS2_PLACEMENT_3D ( 'NONE', #100986, #56804, #108849 ) ;
#7175 = B_SPLINE_CURVE_WITH_KNOTS ( 'NONE', 5,
 ( #103520, #18953, #2208, #105192, #28484, #62676 ),
 .UNSPECIFIED., .F., .F.,
 ( 6, 6 ),
 ( 0.000000000000000000, 1.000000000000000000 ),
 .UNSPECIFIED. ) ;
#7176 = B_SPLINE_SURFACE_WITH_KNOTS ( 'NONE', 5, 5, ( 
 ( #47746, #82994, #72955, #40984, #29834, #38779 ),
 ( #32036, #13014, #47200, #5184, #81326, #4641 ),
 ( #30381, #98690, #30932, #21950, #90279, #39339 ),
 ( #51055, #66773, #85186, #43208, #102525, #8472 ),
 ( #60015, #34238, #49950, #84632, #58904, #7930 ),
 ( #101416, #42099, #42646, #76800, #68423, #17968 ) ),
 .UNSPECIFIED., .F., .F., .F.,
 ( 6, 6 ),
 ( 6, 6 ),
 ( 17.24302740239999920, 89.20802345619999585 ),
 ( -2.775557561569999727E-17, 2.000000000410000034 ),
 .UNSPECIFIED. ) ;
#7177 = CARTESIAN_POINT ( 'NONE',  ( -53.33610125319999895, 1383.102638364699942, 230.8253073736590011 ) ) ;
#7178 = CARTESIAN_POINT ( 'NONE',  ( 8.319417205733840248, 1436.545527341170100, 206.8831545614739866 ) ) ;
#7179 = EDGE_LOOP ( 'NONE', ( #73607, #78031, #95120, #54723, #17130, #89487 ) ) ;
#7180 = EDGE_LOOP ( 'NONE', ( #84068, #48104, #2557, #66954 ) ) ;
#7181 = CARTESIAN_POINT ( 'NONE',  ( -21.43625278670000256, 1505.201739750890056, 211.1850546088390104 ) ) ;
#7182 = CARTESIAN_POINT ( 'NONE',  ( -2.801044513574019845, 1515.551704203360032, 205.2926231456509925 ) ) ;
#7184 = FACE_OUTER_BOUND ( 'NONE', #60503, .T. ) ;
#7183 = DIRECTION ( 'NONE',  ( -0.004026485253183625761, 0.9999913661844073154, 0.001027118858031680253 ) ) ;
#7185 = AXIS2_PLACEMENT_3D ( 'NONE', #90101, #5002, #22328 ) ;
#7186 = ADVANCED_FACE ( 'NONE', ( #86990 ), #86722, .T. ) ;
#7187 = CARTESIAN_POINT ( 'NONE',  ( -9.025098172850000822, 1462.934938264289940, 204.1976517399190243 ) ) ;
#7188 = CARTESIAN_POINT ( 'NONE',  ( -106.8622583199999951, 1380.214950530570150, 299.5452633442590127 ) ) ;
#7189 = CARTESIAN_POINT ( 'NONE',  ( 1.378013107889999977, 1443.686999423290217, 202.9879073201189783 ) ) ;
#7190 = CARTESIAN_POINT ( 'NONE',  ( -2.620401159595194596, 1523.462669333492386, 176.0805060895363852 ) ) ;
#7191 = DIRECTION ( 'NONE',  ( 2.042903098301770100E-14, 1.000000000000000000, -6.143886524153290706E-15 ) ) ;
#7192 = DIRECTION ( 'NONE',  ( -1.755985294532469921E-16, 1.000000000000000000, -1.338183447452831989E-16 ) ) ;
#7193 = CARTESIAN_POINT ( 'NONE',  ( 0.7988375143999999484, 1409.446852857530075, 185.3482159754979932 ) ) ;
#7194 = CARTESIAN_POINT ( 'NONE',  ( 2.166404729989209965, 1486.720363920270074, 197.3876830102489919 ) ) ;
#7195 = EDGE_CURVE ( 'NONE', #74194, #51048, #27605, .T. ) ;
#7196 = CARTESIAN_POINT ( 'NONE',  ( -12.02612939183720009, 1377.659857216290220, 211.7505375168460091 ) ) ;
#7197 = CARTESIAN_POINT ( 'NONE',  ( -4.243814737821510086, 1441.427819818469970, 162.1743596817549928 ) ) ;
#7198 = AXIS2_PLACEMENT_3D ( 'NONE', #30074, #22755, #73199 ) ;
#7199 = CARTESIAN_POINT ( 'NONE',  ( -2.104349271192939685, 1450.141963089990213, 182.8680826352290012 ) ) ;
#7200 = VERTEX_POINT ( 'NONE', #107654 ) ;
#7201 =( BOUNDED_CURVE ( )  B_SPLINE_CURVE ( 3, ( #51098, #78501, #85223, #104248 ),
 .UNSPECIFIED., .F., .F. ) 
 B_SPLINE_CURVE_WITH_KNOTS ( ( 4, 4 ),
 ( 4.712388980384689674, 6.283185307179586232 ),
 .UNSPECIFIED. ) 
 CURVE ( )  GEOMETRIC_REPRESENTATION_ITEM ( )  RATIONAL_B_SPLINE_CURVE ( ( 1.000000000000000000, 0.8047378541243649375, 0.8047378541243649375, 1.000000000000000000 ) ) 
 REPRESENTATION_ITEM ( '' )  );
#7202 = EDGE_CURVE ( 'NONE', #16155, #12333, #78372, .T. ) ;
#7203 = CARTESIAN_POINT ( 'NONE',  ( -13.77266209894789917, 1522.051704408389924, 217.0393652727940150 ) ) ;
#7204 = CARTESIAN_POINT ( 'NONE',  ( 33.36586802512172767, 1512.187213306747481, 201.9069332299488622 ) ) ;
#7205 = CARTESIAN_POINT ( 'NONE',  ( 14.79572149000000003, 1410.747178327829943, 191.5201547110980016 ) ) ;
#7206 = CARTESIAN_POINT ( 'NONE',  ( -6.443502200292150068E-09, 1472.319935551380013, 259.7298202287869913 ) ) ;
#7207 = CARTESIAN_POINT ( 'NONE',  ( 20.44283505528667888, 1436.443178919755610, 144.9572787325427328 ) ) ;
#7208 = CARTESIAN_POINT ( 'NONE',  ( 1.698736666709999898, 1476.148439429189921, 197.7469619067989868 ) ) ;
#7209 = CARTESIAN_POINT ( 'NONE',  ( -108.5111915540000069, 1387.700385856930097, 310.5423399582590491 ) ) ;
#7210 = CARTESIAN_POINT ( 'NONE',  ( 0.1246760915043968326, 1486.459310424578462, 181.8129998335755317 ) ) ;
#7211 = CARTESIAN_POINT ( 'NONE',  ( -8.082564370841041068, 1362.241991287404062, 210.6218459616991936 ) ) ;
#7212 = CARTESIAN_POINT ( 'NONE',  ( -46.27659351362679985, 1440.462201645729920, 267.5895223780760261 ) ) ;
#7213 = CARTESIAN_POINT ( 'NONE',  ( 13.52332530298609825, 1508.669884114960041, 233.4688069057430084 ) ) ;
#7214 = CARTESIAN_POINT ( 'NONE',  ( -8.053805599429999518, 1425.213684849519950, 208.0209531150689770 ) ) ;
#7215 = CARTESIAN_POINT ( 'NONE',  ( -7.726684725664999753, 1517.208444099459939, 207.9957078235169945 ) ) ;
#7216 = VECTOR ( 'NONE', #71677, 999.9999999999998863 ) ;
#7217 = FACE_OUTER_BOUND ( 'NONE', #98343, .T. ) ;
#7218 = B_SPLINE_SURFACE_WITH_KNOTS ( 'NONE', 5, 5, ( 
 ( #80788, #21394, #55605, #53968, #88101, #71328 ),
 ( #89728, #105441, #11388, #28730, #48853, #72940 ),
 ( #40968, #82437, #107632, #13003, #100330, #56130 ),
 ( #99207, #90265, #5167, #56686, #90823, #14104 ),
 ( #107079, #22486, #15197, #91924, #74594, #40417 ),
 ( #30367, #48294, #64557, #57801, #81866, #109296 ) ),
 .UNSPECIFIED., .F., .F., .F.,
 ( 6, 6 ),
 ( 6, 6 ),
 ( 13.29217618510000065, 14.75807319179999944 ),
 ( 0.000000000000000000, 2.000000000000000000 ),
 .UNSPECIFIED. ) ;
#7219 = CYLINDRICAL_SURFACE ( 'NONE', #105204, 2.000000000000003109 ) ;
#7220 = CARTESIAN_POINT ( 'NONE',  ( 7.519426757291130414, 1425.430319809400089, 212.2093128352389897 ) ) ;
#7221 = CARTESIAN_POINT ( 'NONE',  ( -26.57297411396899989, 1451.985062530020059, 135.0132826329440263 ) ) ;
#7222 = VERTEX_POINT ( 'NONE', #91409 ) ;
#7223 = CARTESIAN_POINT ( 'NONE',  ( 25.18659394999999890, 1435.864776774990105, 221.5022687698979951 ) ) ;
#7224 = CARTESIAN_POINT ( 'NONE',  ( 1.461742694410000043, 1494.215630625830045, 181.6758722823980179 ) ) ;
#7225 = CARTESIAN_POINT ( 'NONE',  ( -19.58933252839999994, 1465.550215966989981, 206.2255664879889991 ) ) ;
#7226 = CARTESIAN_POINT ( 'NONE',  ( -24.17505645849999851, 1437.686240857209896, 211.9528072102179976 ) ) ;
#7227 = CARTESIAN_POINT ( 'NONE',  ( 7.526515472008799890, 1517.051704408389924, 209.5611024095850041 ) ) ;
#7228 = CARTESIAN_POINT ( 'NONE',  ( -18.87589743271229992, 1452.253899524100007, 144.5155550433779865 ) ) ;
#7229 = DIRECTION ( 'NONE',  ( -1.964544591288419982E-14, -1.000000000000000000, 8.043425993822650894E-15 ) ) ;
#7230 = EDGE_LOOP ( 'NONE', ( #76055, #38360, #105301, #16877, #105249, #74565 ) ) ;
#7231 = CARTESIAN_POINT ( 'NONE',  ( 11.07826983750000061, 1500.667907230989840, 205.8218841770989798 ) ) ;
#7232 = CARTESIAN_POINT ( 'NONE',  ( 13.12206485389999955, 1420.327681803430096, 229.1659002618980026 ) ) ;
#7233 = CARTESIAN_POINT ( 'NONE',  ( 11.52816659857622383, 1414.661898229710005, 211.3132496073693005 ) ) ;
#7234 = EDGE_LOOP ( 'NONE', ( #30614, #37440, #98816, #77017, #103197 ) ) ;
#7235 = EDGE_LOOP ( 'NONE', ( #2156, #21366, #70373, #71162, #9440, #30933, #91937, #29011, #55062 ) ) ;
#7236 = CARTESIAN_POINT ( 'NONE',  ( -50.84508920509999541, 1384.755135372010045, 226.1764230024589892 ) ) ;
#7237 = CARTESIAN_POINT ( 'NONE',  ( -23.92522223069349963, 1410.731318646559885, 209.8608519489140178 ) ) ;
#7238 = ORIENTED_EDGE ( 'NONE', *, *, #57100, .T. ) ;
#7239 = CARTESIAN_POINT ( 'NONE',  ( -107.4576978852700080, 1306.483669372790018, 307.4681403979390097 ) ) ;
#7240 = CARTESIAN_POINT ( 'NONE',  ( -45.35511022099471035, 1436.791113516306268, 266.1975110343311712 ) ) ;
#7241 = CARTESIAN_POINT ( 'NONE',  ( -25.00976051679999657, 1436.598010167069788, 137.9330532114979917 ) ) ;
#7242 = CARTESIAN_POINT ( 'NONE',  ( 3.176066407067710262, 1508.610720099250102, 213.8016370287309655 ) ) ;
#7243 = ORIENTED_EDGE ( 'NONE', *, *, #41858, .F. ) ;
#7244 = CARTESIAN_POINT ( 'NONE',  ( 45.61112093737630602, 1446.140457532640085, 266.6912352721849970 ) ) ;
#7245 = CARTESIAN_POINT ( 'NONE',  ( -10.80488858036439836, 1391.913060387170162, 205.5034207131209882 ) ) ;
#7246 = CARTESIAN_POINT ( 'NONE',  ( -16.91308933013565508, 1421.902804263020471, 226.8507505944365619 ) ) ;
#7247 = CARTESIAN_POINT ( 'NONE',  ( 7.710610402995000001, 1516.594591938570147, 205.6677260153969939 ) ) ;
#7248 = ORIENTED_EDGE ( 'NONE', *, *, #86288, .F. ) ;
#7249 = CARTESIAN_POINT ( 'NONE',  ( 18.56582872426456632, 1458.623439932988958, 227.5449210459607059 ) ) ;
#7250 = CARTESIAN_POINT ( 'NONE',  ( -0.7827245234523669826, 1444.561379792319940, 199.0971546026119938 ) ) ;
#7251 = AXIS2_PLACEMENT_3D ( 'NONE', #29628, #63812, #65468 ) ;
#7252 = CARTESIAN_POINT ( 'NONE',  ( 13.03846733632719790, 1432.812993616249969, 222.4048857007069842 ) ) ;
#7253 = VERTEX_POINT ( 'NONE', #83537 ) ;
#7254 = CARTESIAN_POINT ( 'NONE',  ( -10.37371817630540072, 1479.852997517780068, 210.7819975190230082 ) ) ;
#7255 = CARTESIAN_POINT ( 'NONE',  ( 26.92459677059870060, 1451.501184678159916, 136.0683855680960050 ) ) ;
#7256 = CARTESIAN_POINT ( 'NONE',  ( -2.564245648394030130, 1508.551704408389924, 214.1089243555790063 ) ) ;
#7257 = CARTESIAN_POINT ( 'NONE',  ( 11.80702251126379920, 1501.961501625749861, 213.8659162354030059 ) ) ;
#7258 = CARTESIAN_POINT ( 'NONE',  ( 7.340164244669999505, 1422.546863311710013, 195.5659725453989779 ) ) ;
#7259 = CARTESIAN_POINT ( 'NONE',  ( -1.860813652961599951, 1432.605433200009884, 218.4608168085190130 ) ) ;
#7260 = CARTESIAN_POINT ( 'NONE',  ( 10.07826753830500088, 1480.104525031030107, 205.9543300576330012 ) ) ;
#7261 = CARTESIAN_POINT ( 'NONE',  ( 3.377914574041609885, 1409.031019763529912, 187.3393513309910077 ) ) ;
#7263 = DIRECTION ( 'NONE',  ( 0.9995237679829612754, -0.03085834145158970754, -2.563637404923585686E-08 ) ) ;
#7262 = CARTESIAN_POINT ( 'NONE',  ( 1.803096684420000040, 1417.508280449130098, 234.1739293872979886 ) ) ;
#7264 = CARTESIAN_POINT ( 'NONE',  ( 4.051730709047915546, 1441.572134815625986, 170.5366858379989310 ) ) ;
#7265 = CARTESIAN_POINT ( 'NONE',  ( -11.52159655330000021, 1380.583467895319927, 215.6172400537489864 ) ) ;
#7266 = CARTESIAN_POINT ( 'NONE',  ( 9.609284535499998725, 1429.602790706330097, 148.1400166355980161 ) ) ;
#7267 = EDGE_LOOP ( 'NONE', ( #39811, #86125, #42482, #44787 ) ) ;
#7268 = CARTESIAN_POINT ( 'NONE',  ( 11.22551998620189906, 1414.913060387399810, 220.6642913648300066 ) ) ;
#7269 = AXIS2_PLACEMENT_3D ( 'NONE', #110647, #7632, #51293 ) ;
#7270 = CARTESIAN_POINT ( 'NONE',  ( 5.161034791280000533, 1485.814572579490005, 218.5690567784690188 ) ) ;
#7271 = CARTESIAN_POINT ( 'NONE',  ( 17.40764059099999628, 1414.996444526030018, 210.6782161193179945 ) ) ;
#7272 = CARTESIAN_POINT ( 'NONE',  ( -12.84952252529999939, 1390.894616655729806, 209.7716342346369913 ) ) ;
#7273 = CARTESIAN_POINT ( 'NONE',  ( -15.92986207429999901, 1416.139014782290133, 209.7537124246929920 ) ) ;
#7274 = CARTESIAN_POINT ( 'NONE',  ( 11.47825147261290013, 1422.092222879909968, 203.3953002428119987 ) ) ;
#7275 = CARTESIAN_POINT ( 'NONE',  ( -10.86989658753349985, 1462.792704963670076, 207.1137526030339870 ) ) ;
#7276 = CARTESIAN_POINT ( 'NONE',  ( -23.03655027839999647, 1458.194572356429944, 255.3819207742980097 ) ) ;
#7277 = CARTESIAN_POINT ( 'NONE',  ( -8.861333410889999485, 1384.870662623839962, 218.6848950059789729 ) ) ;
#7279 = EDGE_CURVE ( 'NONE', #79544, #79854, #42245, .T. ) ;
#7278 = CARTESIAN_POINT ( 'NONE',  ( 9.833393186232889605, 1517.151704408390060, 205.7359371553449989 ) ) ;
#7280 = CARTESIAN_POINT ( 'NONE',  ( 6.648507829046476303, 1432.796636465103802, 201.9740417089893185 ) ) ;
#7281 = CARTESIAN_POINT ( 'NONE',  ( -9.651319794912328831, 1460.367258809480063, 209.5401502381419903 ) ) ;
#7282 = AXIS2_PLACEMENT_3D ( 'NONE', #4594, #29240, #30329 ) ;
#7283 = CARTESIAN_POINT ( 'NONE',  ( -16.92750792760880074, 1420.371514553650059, 203.6344363212050155 ) ) ;
#7284 = CARTESIAN_POINT ( 'NONE',  ( 11.60899603973430061, 1420.226618356180097, 197.9003279743849930 ) ) ;
#7285 = CARTESIAN_POINT ( 'NONE',  ( 7.901747246281610515, 1464.504505592670057, 216.3084624029710028 ) ) ;
#7286 = CARTESIAN_POINT ( 'NONE',  ( -18.98347673960000037, 1486.208000860629909, 189.2831150523980170 ) ) ;
#7287 = AXIS2_PLACEMENT_3D ( 'NONE', #9205, #94857, #34942 ) ;
#7288 = CARTESIAN_POINT ( 'NONE',  ( 3.533737149336580341, 1474.412271694010087, 219.9835368386560219 ) ) ;
#7289 = CARTESIAN_POINT ( 'NONE',  ( -17.58360215189999920, 1410.891091606730015, 225.4625532605979856 ) ) ;
#7290 = CARTESIAN_POINT ( 'NONE',  ( -8.080362626630025247, 1425.655864844915413, 208.1442273905381910 ) ) ;
#7291 = FACE_OUTER_BOUND ( 'NONE', #30719, .T. ) ;
#7292 = DIRECTION ( 'NONE',  ( -0.9786619618251657382, 0.000000000000000000, 0.2054769195713179730 ) ) ;
#7293 = EDGE_CURVE ( 'NONE', #73940, #72816, #93041, .T. ) ;
#7294 = CARTESIAN_POINT ( 'NONE',  ( 12.72996564059999969, 1416.826388557929931, 223.1307082869980150 ) ) ;
#7295 = CARTESIAN_POINT ( 'NONE',  ( 12.74442039725110121, 1426.727524945199775, 204.3806995420410146 ) ) ;
#7296 = CARTESIAN_POINT ( 'NONE',  ( -8.229021131380180876, 1439.448077257160094, 228.6152060057279982 ) ) ;
#7297 = DIRECTION ( 'NONE',  ( 0.1976594630508882178, -0.9325252259461312976, 0.3022043011615674901 ) ) ;
#7298 = CARTESIAN_POINT ( 'NONE',  ( -16.75443776603389878, 1420.334096955099994, 204.7363179042169747 ) ) ;
#7299 = CARTESIAN_POINT ( 'NONE',  ( 0.2060721707870890040, 1459.560850903249730, 182.9719205269209965 ) ) ;
#7301 = ORIENTED_EDGE ( 'NONE', *, *, #23300, .T. ) ;
#7300 = CARTESIAN_POINT ( 'NONE',  ( 7.151487810977736892, 1466.240892066645756, 202.2032590110584067 ) ) ;
#7302 = CARTESIAN_POINT ( 'NONE',  ( -27.23063139319997816, 1443.913060387329097, 161.8596747266978753 ) ) ;
#7303 = CARTESIAN_POINT ( 'NONE',  ( -37.73093663436678469, 1445.052233488290085, 136.8111089660027062 ) ) ;
#7304 = DIRECTION ( 'NONE',  ( 0.9112835967509683721, 0.3049192395332191996, -0.2767425945804181109 ) ) ;
#7305 = CARTESIAN_POINT ( 'NONE',  ( -41.54171725205129917, 1442.308966536679918, 134.0999999980950008 ) ) ;
#7306 = CARTESIAN_POINT ( 'NONE',  ( -109.8952781789999875, 1384.897890919899965, 297.0284440182589947 ) ) ;
#7307 = ORIENTED_EDGE ( 'NONE', *, *, #14442, .F. ) ;
#7308 = CARTESIAN_POINT ( 'NONE',  ( -1.726831718310000152, 1484.334257313489843, 198.5613320218990054 ) ) ;
#7309 = B_SPLINE_CURVE_WITH_KNOTS ( 'NONE', 3,
 ( #58479, #17535, #243, #67998, #76373, #34371, #75826, #68545, #109977, #16431, #24833, #85872, #6953, #110522, #41110, #75287, #92606, #85303, #25389, #109433, #9173, #102644, #50623, #33254, #51736, #84756, #25944, #60140, #43338, #33804, #77486, #93695, #32159, #66346, #102110, #100462, #59582, #23745, #32710, #50082, #16975, #101000, #51174, #24296, #84211, #7507, #8053, #59038, #67445 ),
 .UNSPECIFIED., .F., .F.,
 ( 4, 2, 1, 2, 2, 2, 1, 1, 2, 2, 2, 2, 1, 1, 1, 2, 2, 2, 2, 1, 1, 1, 2, 2, 2, 1, 1, 2, 2, 4 ),
 ( 0.000000000000000000, 0.06249999999961332320, 0.09374999999955876961, 0.1093749999996599526, 0.1249999999997611078, 0.1875000000001662837, 0.2187500000003581302, 0.2343750000004542200, 0.2421875000005638823, 0.2500000000006735723, 0.3750000000012407853, 0.4375000000015574209, 0.4687500000017156832, 0.4843750000018106627, 0.4921875000018929858, 0.4960937500019232393, 0.5000000000019535484, 0.6250000000019894086, 0.6875000000019952928, 0.7187500000020067281, 0.7343750000020016211, 0.7421875000020143887, 0.7460937500020170532, 0.7500000000020197177, 0.8125000000015978330, 0.8437500000013867796, 0.8593750000012922996, 0.8671875000012422285, 0.8750000000011921575, 1.000000000000000000 ),
 .UNSPECIFIED. ) ;
#7310 = CARTESIAN_POINT ( 'NONE',  ( 10.17891481550000066, 1479.588126538789766, 206.0283001565290135 ) ) ;
#7311 = CARTESIAN_POINT ( 'NONE',  ( -103.6636288076488341, 1379.952131678016485, 305.1582356039069737 ) ) ;
#7312 = DIRECTION ( 'NONE',  ( 0.06728379684272124683, -0.9969860201949396483, 0.03862338952348206428 ) ) ;
#7313 = CARTESIAN_POINT ( 'NONE',  ( -4.834465893738980391, 1433.076913074690083, 216.1502409442880150 ) ) ;
#7314 = CYLINDRICAL_SURFACE ( 'NONE', #107244, 1.463110112869996149 ) ;
#7315 = CARTESIAN_POINT ( 'NONE',  ( 22.78790659570000088, 1507.631725798030175, 209.8615682015409902 ) ) ;
#7316 = DIRECTION ( 'NONE',  ( -0.000000000000000000, -1.000000000000000000, -0.000000000000000000 ) ) ;
#7317 = CARTESIAN_POINT ( 'NONE',  ( 2.500000000000000000, 1436.879499792069964, 182.8948590173980051 ) ) ;
#7318 = CARTESIAN_POINT ( 'NONE',  ( -53.14982994521080428, 1385.030877996189929, 230.4728250025019918 ) ) ;
#7319 = ADVANCED_FACE ( 'NONE', ( #32043 ), #1830, .F. ) ;
#7320 = CARTESIAN_POINT ( 'NONE',  ( -11.66275644280949919, 1391.913060387289988, 209.7846402079380255 ) ) ;
#7321 = CARTESIAN_POINT ( 'NONE',  ( 10.46737987522440072, 1424.278786533029916, 206.5800728862719779 ) ) ;
#7322 = ORIENTED_EDGE ( 'NONE', *, *, #96614, .F. ) ;
#7323 = CARTESIAN_POINT ( 'NONE',  ( -32.07934838669999777, 1451.337335293929982, 136.0002333985979988 ) ) ;
#7324 = CARTESIAN_POINT ( 'NONE',  ( -15.80146386689030003, 1410.855256520919966, 226.7268951530490142 ) ) ;
#7326 = ORIENTED_EDGE ( 'NONE', *, *, #37919, .T. ) ;
#7325 = DIRECTION ( 'NONE',  ( 3.085874980950000024E-15, -2.120525977030000242E-14, -1.000000000000000000 ) ) ;
#7327 = CARTESIAN_POINT ( 'NONE',  ( 3.883237672519999517, 1472.390963103490094, 218.5418498176989885 ) ) ;
#7328 = ADVANCED_FACE ( 'NONE', ( #108196 ), #78705, .F. ) ;
#7329 = CARTESIAN_POINT ( 'NONE',  ( -19.19237350200172187, 1410.944925138707504, 222.5985789656905638 ) ) ;
#7330 = CARTESIAN_POINT ( 'NONE',  ( -109.9814243290000064, 1384.586435984209857, 311.4451819562590345 ) ) ;
#7331 = CARTESIAN_POINT ( 'NONE',  ( -0.3290055904713540258, 1418.886737140139985, 184.6767946731409893 ) ) ;
#7332 = CARTESIAN_POINT ( 'NONE',  ( 41.48540613818578038, 1445.929842224576305, 269.6377302435102479 ) ) ;
#7333 = CARTESIAN_POINT ( 'NONE',  ( 16.90258613670328813, 1433.073112335133601, 217.3043047566771122 ) ) ;
#7334 = CARTESIAN_POINT ( 'NONE',  ( 1.956921220169999698, 1417.602764174529966, 233.5179091431980112 ) ) ;
#7335 = CARTESIAN_POINT ( 'NONE',  ( 5.972707271129999107, 1446.365007016290065, 202.2403774837590049 ) ) ;
#7336 = CARTESIAN_POINT ( 'NONE',  ( -113.4000000000000057, 1348.229899472569969, 298.0159978832119805 ) ) ;
#7337 = CARTESIAN_POINT ( 'NONE',  ( 4.063550476549999679, 1497.713060387329961, 230.5763704537980061 ) ) ;
#7338 = CARTESIAN_POINT ( 'NONE',  ( -3.205905787939999918, 1454.493866239789895, 199.5427767106090187 ) ) ;
#7339 = CARTESIAN_POINT ( 'NONE',  ( -0.01327257453019850021, 1516.940252185109784, 206.2479269295770052 ) ) ;
#7340 = CARTESIAN_POINT ( 'NONE',  ( 2.500000000000000000, 1448.989771342329959, 154.5778231068980233 ) ) ;
#7341 = ORIENTED_EDGE ( 'NONE', *, *, #91494, .F. ) ;
#7342 = VECTOR ( 'NONE', #75145, 1000.000000000000000 ) ;
#7343 = CARTESIAN_POINT ( 'NONE',  ( -109.1321617031399995, 1384.741658746849907, 311.2608059278249470 ) ) ;
#7344 = CARTESIAN_POINT ( 'NONE',  ( -4.232926184839439721, 1441.503792767389996, 164.1558557344339988 ) ) ;
#7346 = ORIENTED_EDGE ( 'NONE', *, *, #59735, .T. ) ;
#7345 = CARTESIAN_POINT ( 'NONE',  ( -68.61213284361410558, 1379.747544145440088, 280.2245858376650176 ) ) ;
#7347 = CARTESIAN_POINT ( 'NONE',  ( -17.45404115237240106, 1417.661807274269904, 206.3269853752529741 ) ) ;
#7348 = ORIENTED_EDGE ( 'NONE', *, *, #59133, .T. ) ;
#7349 = CARTESIAN_POINT ( 'NONE',  ( -16.09179319795009633, 1514.742486295231856, 224.1276633295240117 ) ) ;
#7350 = CYLINDRICAL_SURFACE ( 'NONE', #102933, 2.000000000000000000 ) ;
#7352 = CARTESIAN_POINT ( 'NONE',  ( 15.97954657421199798, 1409.471061115830025, 193.0248343784320184 ) ) ;
#7351 = CARTESIAN_POINT ( 'NONE',  ( -11.43885624517646526, 1425.480338822508202, 144.2656653268024343 ) ) ;
#7353 = CARTESIAN_POINT ( 'NONE',  ( 4.044321679994999919, 1517.001127920769704, 211.4073335515969916 ) ) ;
#7354 = CIRCLE ( 'NONE', #69974, 2.000000000000001776 ) ;
#7355 = CARTESIAN_POINT ( 'NONE',  ( 39.86835271869999531, 1441.199396608850066, 136.8459542608980257 ) ) ;
#7356 = B_SPLINE_CURVE_WITH_KNOTS ( 'NONE', 3,
 ( #63107, #97204, #98307, #46293, #55791, #37866, #21583, #89906, #88266, #54688, #97758, #96105, #106167, #44621, #78762, #29444, #2077, #19380, #21029, #89364, #53584, #12657, #80965, #105066, #27804, #36207, #61989, #40062, #47916, #75340, #32758, #4796, #56322, #107263, #38941, #31106, #101049, #74242, #73121, #82624, #99398, #65285, #22676, #57983, #83714, #30558, #15393, #57445, #108372, #64746, #109481, #13731, #39516, #14846 ),
 .UNSPECIFIED., .F., .F.,
 ( 4, 2, 2, 1, 1, 2, 2, 2, 2, 1, 1, 1, 1, 2, 2, 2, 2, 2, 2, 2, 2, 2, 1, 1, 2, 2, 1, 1, 1, 1, 2, 2, 4 ),
 ( 0.000000000000000000, 0.06249999999991798227, 0.09374999999990608901, 0.1093749999998750166, 0.1171874999998856054, 0.1210937499998925304, 0.1249999999998994693, 0.1875000000009550416, 0.2187500000015098200, 0.2343750000017873758, 0.2421875000019497182, 0.2460937500020323188, 0.2480468750020981550, 0.2490234375021571356, 0.2500000000022161162, 0.3750000000027837177, 0.4375000000030658254, 0.4687500000032305825, 0.5000000000033952841, 0.5625000000037223558, 0.5937500000039129811, 0.6093750000040102366, 0.6171875000040586423, 0.6210937500040828452, 0.6230468750040973891, 0.6250000000041118220, 0.6875000000031932235, 0.7187500000027338132, 0.7343750000024805713, 0.7421875000023285818, 0.7460937500022526425, 0.7500000000021767033, 1.000000000000000000 ),
 .UNSPECIFIED. ) ;
#7357 = SURFACE_STYLE_FILL_AREA ( #76768 ) ;
#7358 = CARTESIAN_POINT ( 'NONE',  ( 14.87107281846884455, 1462.053534961335572, 230.0773967180462876 ) ) ;
#7359 = CONTEXT_DEPENDENT_SHAPE_REPRESENTATION ( #58522, #29430 ) ;
#7360 = DIRECTION ( 'NONE',  ( 0.9455185755993178454, 0.000000000000000000, -0.3255681544571539243 ) ) ;
#7361 = CARTESIAN_POINT ( 'NONE',  ( -37.82787436099530254, 1438.484237118849933, 136.5974028198669998 ) ) ;
#7362 = EDGE_LOOP ( 'NONE', ( #11005, #13102, #31358, #73118, #38631 ) ) ;
#7363 = CARTESIAN_POINT ( 'NONE',  ( 13.84583968663999798, 1499.900157016389812, 227.7510566287420204 ) ) ;
#7364 = CARTESIAN_POINT ( 'NONE',  ( -120.2678896395927666, 1379.913060387289988, 304.3291340586740716 ) ) ;
#7365 = B_SPLINE_CURVE_WITH_KNOTS ( 'NONE', 5,
 ( #70727, #55010, #52795, #2413, #105956, #20265, #62892, #19722, #20812, #86927, #36530, #10218 ),
 .UNSPECIFIED., .F., .F.,
 ( 6, 3, 3, 6 ),
 ( 0.000000000000000000, 0.3925153839664296540, 0.7975051279878269117, 1.000000000000000000 ),
 .UNSPECIFIED. ) ;
#7366 = ORIENTED_EDGE ( 'NONE', *, *, #47219, .F. ) ;
#7367 = VERTEX_POINT ( 'NONE', #88519 ) ;
#7368 = DIRECTION ( 'NONE',  ( -0.7067700363774163108, -0.03085824620771824081, 0.7067700363767903671 ) ) ;
#7369 = DIRECTION ( 'NONE',  ( 0.6906235816661250304, -0.2466512791670444904, -0.6798545542481230219 ) ) ;
#7370 = AXIS2_PLACEMENT_3D ( 'NONE', #75224, #56206, #82513 ) ;
#7371 = DIRECTION ( 'NONE',  ( 0.000000000000000000, 0.000000000000000000, -1.000000000000000000 ) ) ;
#7372 = CARTESIAN_POINT ( 'NONE',  ( -14.15554687228640063, 1508.551704408389924, 210.3501763792300210 ) ) ;
#7373 = CARTESIAN_POINT ( 'NONE',  ( 4.045211208830000515, 1515.528099018290050, 210.6101754513790070 ) ) ;
#7374 = CARTESIAN_POINT ( 'NONE',  ( 11.78238356083980065, 1440.882651838439870, 188.1224447589279976 ) ) ;
#7375 = CARTESIAN_POINT ( 'NONE',  ( 40.71747597329999735, 1438.773003763650195, 134.0999987698980078 ) ) ;
#7376 = FACE_OUTER_BOUND ( 'NONE', #75524, .T. ) ;
#7377 = CARTESIAN_POINT ( 'NONE',  ( 27.11300533590000228, 1438.407748754029853, 136.9651466902979848 ) ) ;
#7378 = CARTESIAN_POINT ( 'NONE',  ( -12.18027861210000040, 1391.555521559479985, 211.6651143923290306 ) ) ;
#7379 = CARTESIAN_POINT ( 'NONE',  ( -85.67554441382009145, 1384.820767901929912, 289.3504411783320052 ) ) ;
#7380 = EDGE_LOOP ( 'NONE', ( #81488, #45826 ) ) ;
#7381 = CARTESIAN_POINT ( 'NONE',  ( -5.004442077115000664, 1516.690345681169902, 201.4087281291169802 ) ) ;
#7382 = CARTESIAN_POINT ( 'NONE',  ( -2.297629659184999618, 1516.970035769810011, 208.3868227339359862 ) ) ;
#7383 = VERTEX_POINT ( 'NONE', #96362 ) ;
#7384 = CARTESIAN_POINT ( 'NONE',  ( 11.77725414648410052, 1427.326574604300049, 146.8862230489449985 ) ) ;
#7385 = CIRCLE ( 'NONE', #16307, 15.41143114519999990 ) ;
#7386 = CARTESIAN_POINT ( 'NONE',  ( 4.076676381798102433, 1511.455724275399234, 217.3418713267658973 ) ) ;
#7387 = ORIENTED_EDGE ( 'NONE', *, *, #20315, .T. ) ;
#7388 = DIRECTION ( 'NONE',  ( -0.8907681516580484571, 1.273087901431153894E-31, 0.4544580288560254311 ) ) ;
#7389 = CARTESIAN_POINT ( 'NONE',  ( -16.68463233076019492, 1442.773887286370609, 162.0935120523188857 ) ) ;
#7390 = CARTESIAN_POINT ( 'NONE',  ( 21.59396340175304019, 1525.159196711359755, 233.4989680424126561 ) ) ;
#7391 = VECTOR ( 'NONE', #16740, 1000.000000000000227 ) ;
#7392 = CARTESIAN_POINT ( 'NONE',  ( 24.15268678416311587, 1411.115268795248767, 208.9542267914210925 ) ) ;
#7393 = CARTESIAN_POINT ( 'NONE',  ( -12.70045074689999964, 1422.978954057429974, 222.3368426438979952 ) ) ;
#7394 = CARTESIAN_POINT ( 'NONE',  ( 11.04934308535739973, 1470.239499499950171, 206.9398480105810165 ) ) ;
#7395 = CARTESIAN_POINT ( 'NONE',  ( -10.93363683719999813, 1471.692480041690033, 205.6467075678189929 ) ) ;
#7396 = CARTESIAN_POINT ( 'NONE',  ( 7.630292994640000437, 1493.382908296590131, 217.4308410871590240 ) ) ;
#7397 = CARTESIAN_POINT ( 'NONE',  ( -65.11626332599999500, 1379.739664436940075, 272.5544191705590151 ) ) ;
#7398 = CARTESIAN_POINT ( 'NONE',  ( -16.12193243460000147, 1473.842759945530133, 223.3670126793980160 ) ) ;
#7400 = CYLINDRICAL_SURFACE ( 'NONE', #95804, 2.000000000000003109 ) ;
#7399 = CARTESIAN_POINT ( 'NONE',  ( 15.59938138249999895, 1461.167668198130059, 229.6381429124979832 ) ) ;
#7401 = CARTESIAN_POINT ( 'NONE',  ( 13.37887034578663048, 1473.256410945989728, 270.1124231610745596 ) ) ;
#7402 = CARTESIAN_POINT ( 'NONE',  ( 0.7533001353030019942, 1516.714320817460020, 216.4479181143769893 ) ) ;
#7403 = ORIENTED_EDGE ( 'NONE', *, *, #110402, .T. ) ;
#7404 = CIRCLE ( 'NONE', #73604, 1.997270720800846444 ) ;
#7405 = DIRECTION ( 'NONE',  ( -1.000000000000000000, 0.000000000000000000, 0.000000000000000000 ) ) ;
#7406 = CARTESIAN_POINT ( 'NONE',  ( -21.60819468828554335, 1524.659802833172535, 234.6460983332875685 ) ) ;
#7407 = CARTESIAN_POINT ( 'NONE',  ( -1.704794841465000044, 1517.096587378560116, 213.7484378375869767 ) ) ;
#7408 = CARTESIAN_POINT ( 'NONE',  ( 5.416019587700000137, 1505.806237347190063, 219.5704354396989970 ) ) ;
#7409 = CARTESIAN_POINT ( 'NONE',  ( -11.60004869885203860, 1425.963618636351384, 138.7040202299609462 ) ) ;
#7411 = ORIENTED_EDGE ( 'NONE', *, *, #85629, .F. ) ;
#7410 = CARTESIAN_POINT ( 'NONE',  ( 4.119379022663339995, 1508.879004046169939, 213.4915743296109838 ) ) ;
#7412 = CARTESIAN_POINT ( 'NONE',  ( -15.60757908461217269, 1415.701611827778834, 209.6322609307934499 ) ) ;
#7413 = CARTESIAN_POINT ( 'NONE',  ( -1.561170263100000177, 1508.551704408389924, 220.0946958077990132 ) ) ;
#7414 = CARTESIAN_POINT ( 'NONE',  ( -11.66015940019999952, 1426.002483172329903, 146.0081277900980012 ) ) ;
#7415 = CARTESIAN_POINT ( 'NONE',  ( -15.64577121609999821, 1415.699210022930174, 209.5376526706779998 ) ) ;
#7416 = CARTESIAN_POINT ( 'NONE',  ( -7.332216129953320838, 1441.976895380970063, 202.1891949145530134 ) ) ;
#7417 = CARTESIAN_POINT ( 'NONE',  ( 17.71193101166619854, 1517.151704408390060, 196.6727161458730109 ) ) ;
#7418 = FACE_OUTER_BOUND ( 'NONE', #13238, .T. ) ;
#7419 = DIRECTION ( 'NONE',  ( 0.000000000000000000, 0.000000000000000000, -1.000000000000000000 ) ) ;
#7421 = CARTESIAN_POINT ( 'NONE',  ( -15.05898902610000079, 1503.430790790689798, 209.1800621844290049 ) ) ;
#7420 = CARTESIAN_POINT ( 'NONE',  ( -21.43773211839999959, 1495.369928931229879, 226.0474949278979864 ) ) ;
#7422 = CARTESIAN_POINT ( 'NONE',  ( -16.16762553486000087, 1459.157033785442081, 229.6200968447579953 ) ) ;
#7423 = ORIENTED_EDGE ( 'NONE', *, *, #25343, .T. ) ;
#7424 = CARTESIAN_POINT ( 'NONE',  ( 0.7356989345870019736, 1517.020847257979995, 205.6609797614169963 ) ) ;
#7425 = CARTESIAN_POINT ( 'NONE',  ( 14.60988619030000102, 1407.613819657329941, 267.1471522769979856 ) ) ;
#7426 = CARTESIAN_POINT ( 'NONE',  ( 1.665334536940000074E-16, 1408.913060387329779, 186.4687945730979948 ) ) ;
#7427 = CARTESIAN_POINT ( 'NONE',  ( 17.47809751519999821, 1410.883709062829894, 192.6106407635979849 ) ) ;
#7428 = EDGE_CURVE ( 'NONE', #46291, #99393, #101196, .T. ) ;
#7429 = LINE ( 'NONE', #85226, #80320 ) ;
#7430 = CARTESIAN_POINT ( 'NONE',  ( 2.713367651848939577, 1454.423712428280169, 218.1168998963650267 ) ) ;
#7431 = CARTESIAN_POINT ( 'NONE',  ( -0.5077264128435760027, 1412.020084291579906, 233.2448261540379804 ) ) ;
#7432 = VECTOR ( 'NONE', #9572, 1000.000000000000114 ) ;
#7433 = CARTESIAN_POINT ( 'NONE',  ( 12.94229023090000119, 1461.456462053329915, 233.4393938603979848 ) ) ;
#7434 = CARTESIAN_POINT ( 'NONE',  ( -14.83256633360000087, 1416.408364792800057, 204.9070730081490126 ) ) ;
#7435 = CARTESIAN_POINT ( 'NONE',  ( -13.52564516290000007, 1444.429216800270069, 187.6720164552979782 ) ) ;
#7436 = EDGE_CURVE ( 'NONE', #31574, #106669, #67280, .T. ) ;
#7437 = CARTESIAN_POINT ( 'NONE',  ( -3.556250521940888198, 1497.014257045862678, 220.2466743886169240 ) ) ;
#7438 = CARTESIAN_POINT ( 'NONE',  ( -16.55781857232240384, 1419.635042661685247, 209.2150186604269209 ) ) ;
#7439 = CARTESIAN_POINT ( 'NONE',  ( -4.351525890989999645, 1495.862468678689993, 219.4621222446990316 ) ) ;
#7440 = CARTESIAN_POINT ( 'NONE',  ( 1.448679645196929933, 1507.129709964000085, 181.1126013477120011 ) ) ;
#7441 = CARTESIAN_POINT ( 'NONE',  ( 3.968827104744170331, 1521.951704408389787, 188.7040005449509863 ) ) ;
#7442 = CARTESIAN_POINT ( 'NONE',  ( 11.64966881943793808, 1425.711239460408251, 138.1863722522803641 ) ) ;
#7443 = CARTESIAN_POINT ( 'NONE',  ( -14.20981385350011017, 1419.004818489330546, 200.1611769720297502 ) ) ;
#7444 = CIRCLE ( 'NONE', #14632, 4.004820216691862278 ) ;
#7445 = CARTESIAN_POINT ( 'NONE',  ( -23.58453086489999961, 1470.876928620230046, 266.7402721287979830 ) ) ;
#7446 = FACE_OUTER_BOUND ( 'NONE', #29816, .T. ) ;
#7447 = CARTESIAN_POINT ( 'NONE',  ( -13.59245260875518113, 1513.749539319655923, 192.3712733982298744 ) ) ;
#7448 = CARTESIAN_POINT ( 'NONE',  ( -17.36863403203877709, 1486.486724665740667, 187.7553479223266777 ) ) ;
#7449 = CARTESIAN_POINT ( 'NONE',  ( -44.38402502188429821, 1384.767141598809758, 250.3222099174190021 ) ) ;
#7450 = CARTESIAN_POINT ( 'NONE',  ( -106.6236903171660089, 1391.913060387289988, 302.6845673397129985 ) ) ;
#7451 = CARTESIAN_POINT ( 'NONE',  ( 11.94473499015900053, 1415.666200591219877, 223.2621103331699999 ) ) ;
#7452 = CARTESIAN_POINT ( 'NONE',  ( -107.1425330629999877, 1379.500016098490050, 299.4908666160590087 ) ) ;
#7453 = CARTESIAN_POINT ( 'NONE',  ( 7.480280153066277471, 1471.188496245784791, 215.9764434431355085 ) ) ;
#7454 = CARTESIAN_POINT ( 'NONE',  ( -20.70484064406366187, 1525.907212628473644, 233.2025904124108706 ) ) ;
#7455 = CARTESIAN_POINT ( 'NONE',  ( -0.7469581576472559270, 1395.939144740979827, 220.1009958539310105 ) ) ;
#7456 = CARTESIAN_POINT ( 'NONE',  ( -9.730454605791324596, 1380.582231750482379, 201.4572460339118436 ) ) ;
#7457 = VECTOR ( 'NONE', #34267, 1000.000000000000114 ) ;
#7458 = CARTESIAN_POINT ( 'NONE',  ( -15.03991797343599934, 1422.464147859393734, 228.7611401550659878 ) ) ;
#7459 = CARTESIAN_POINT ( 'NONE',  ( 11.42820171992390144, 1478.773761690850051, 206.4058094161790109 ) ) ;
#7460 = CARTESIAN_POINT ( 'NONE',  ( -1.600048698852036821, 1402.754281879943164, 137.0999999980979851 ) ) ;
#7461 = CARTESIAN_POINT ( 'NONE',  ( -8.548024229050710687, 1437.883693539470187, 228.3934038729859708 ) ) ;
#7462 = CARTESIAN_POINT ( 'NONE',  ( 16.55387768533850945, 1524.739563915906047, 180.7878331405790675 ) ) ;
#7463 = CARTESIAN_POINT ( 'NONE',  ( -17.65533443933999891, 1419.497285706960156, 207.2321711664930035 ) ) ;
#7465 = CARTESIAN_POINT ( 'NONE',  ( -12.32144544124709995, 1378.870868370589960, 211.6518144768560035 ) ) ;
#7464 = CARTESIAN_POINT ( 'NONE',  ( -16.12185590881189867, 1416.489668067350067, 209.3435334434090009 ) ) ;
#7466 = CARTESIAN_POINT ( 'NONE',  ( -4.992349863779999453, 1391.620913471789891, 203.8075142969990168 ) ) ;
#7467 = CARTESIAN_POINT ( 'NONE',  ( 17.53704155054290936, 1524.872178180562514, 237.4421490224650313 ) ) ;
#7468 = CARTESIAN_POINT ( 'NONE',  ( -125.0414468819000007, 1320.102705746890251, 297.8620945402790312 ) ) ;
#7469 = CARTESIAN_POINT ( 'NONE',  ( 9.922759194041839592, 1450.941995602500128, 205.8041822776330037 ) ) ;
#7470 = DIRECTION ( 'NONE',  ( 0.9977304882603014180, -0.06733403890946067227, 0.000000000000000000 ) ) ;
#7471 = CARTESIAN_POINT ( 'NONE',  ( 6.551643386774999023, 1516.807958722750072, 203.3403553877570005 ) ) ;
#7472 = CARTESIAN_POINT ( 'NONE',  ( -116.0368005749632943, 1305.714868215269917, 309.0484770343335867 ) ) ;
#7473 = CARTESIAN_POINT ( 'NONE',  ( -12.92123606608499564, 1398.295999377893168, 210.5944397367629506 ) ) ;
#7474 = CARTESIAN_POINT ( 'NONE',  ( 16.85261132413500107, 1513.023086264660151, 195.9232021551670186 ) ) ;
#7475 = FACE_BOUND ( 'NONE', #87948, .T. ) ;
#7476 = CARTESIAN_POINT ( 'NONE',  ( -3.771520276259990201, 1377.996768148150068, 211.7927965281820093 ) ) ;
#7477 = AXIS2_PLACEMENT_3D ( 'NONE', #11984, #55663, #29326 ) ;
#7478 = CARTESIAN_POINT ( 'NONE',  ( 3.005276066433927973, 1369.205039411293910, 210.6218459616987957 ) ) ;
#7480 = VERTEX_POINT ( 'NONE', #21818 ) ;
#7479 = CARTESIAN_POINT ( 'NONE',  ( -40.65834370721180591, 1379.654954877820046, 229.2787104343509839 ) ) ;
#7481 = ORIENTED_EDGE ( 'NONE', *, *, #21895, .F. ) ;
#7482 = CARTESIAN_POINT ( 'NONE',  ( 11.87854472459999933, 1434.090690883939942, 150.8572398186979626 ) ) ;
#7483 = CARTESIAN_POINT ( 'NONE',  ( -12.90425718179999848, 1398.295578896729921, 211.5077388498779953 ) ) ;
#7484 = ORIENTED_EDGE ( 'NONE', *, *, #54478, .T. ) ;
#7485 = CARTESIAN_POINT ( 'NONE',  ( 1.475648591298595717E-05, 1397.578653621796548, 222.1218461011892771 ) ) ;
#7486 = CARTESIAN_POINT ( 'NONE',  ( 0.2223009155142280091, 1416.826860677879949, 227.1890218400880030 ) ) ;
#7487 = CARTESIAN_POINT ( 'NONE',  ( -18.69816095120789612, 1526.382868172863937, 183.3860352823957953 ) ) ;
#7489 = CARTESIAN_POINT ( 'NONE',  ( 17.94031933599999817, 1421.715617410530058, 225.1230053650979812 ) ) ;
#7488 = CARTESIAN_POINT ( 'NONE',  ( -0.3986462593559989553, 1443.308886971090260, 200.2051758347389807 ) ) ;
#7490 = CARTESIAN_POINT ( 'NONE',  ( 17.30154577271699878, 1488.410570188420024, 229.9719745730320142 ) ) ;
#7491 = CARTESIAN_POINT ( 'NONE',  ( 1.840176472590000056, 1468.706575379429978, 182.8606869624980220 ) ) ;
#7492 = CARTESIAN_POINT ( 'NONE',  ( -9.986922776509999267, 1415.932617989529945, 193.6517757706980092 ) ) ;
#7493 = CARTESIAN_POINT ( 'NONE',  ( 0.9889191132270008788, 1418.023982291090078, 204.0456544364789977 ) ) ;
#7494 =( NAMED_UNIT ( * ) SI_UNIT ( $, .STERADIAN. ) SOLID_ANGLE_UNIT ( ) );
#7495 = CARTESIAN_POINT ( 'NONE',  ( 4.329448776274299249, 1515.064792882709980, 211.4519800890089982 ) ) ;
#7496 = CARTESIAN_POINT ( 'NONE',  ( 1.184716195880000100, 1415.245980409429876, 191.1061508846980246 ) ) ;
#7497 = CARTESIAN_POINT ( 'NONE',  ( 11.86609764940000034, 1432.335824637460064, 149.9825529227980212 ) ) ;
#7498 = CARTESIAN_POINT ( 'NONE',  ( 4.146234843596174002, 1509.069516669909945, 179.8708435902544238 ) ) ;
#7499 = ORIENTED_EDGE ( 'NONE', *, *, #98330, .F. ) ;
#7500 = CARTESIAN_POINT ( 'NONE',  ( 13.20527699253010034, 1434.869030501559791, 149.0170173390359878 ) ) ;
#7501 = ORIENTED_EDGE ( 'NONE', *, *, #45307, .T. ) ;
#7502 = VERTEX_POINT ( 'NONE', #106412 ) ;
#7503 = CARTESIAN_POINT ( 'NONE',  ( 13.14776788045321609, 1444.759486401034792, 169.3987463143653258 ) ) ;
#7504 = CARTESIAN_POINT ( 'NONE',  ( -9.617209207600001974, 1463.011625836029907, 234.9738963373979743 ) ) ;
#7505 = DIRECTION ( 'NONE',  ( 1.755985294532464991E-16, -1.000000000000000000, 1.338183447452830017E-16 ) ) ;
#7506 = CARTESIAN_POINT ( 'NONE',  ( 4.036119644515000715, 1516.647924054489977, 216.4458205765370167 ) ) ;
#7507 = CARTESIAN_POINT ( 'NONE',  ( -8.520858377768730563, 1511.400001115551277, 214.1155622411217507 ) ) ;
#7508 = VERTEX_POINT ( 'NONE', #29697 ) ;
#7509 = CARTESIAN_POINT ( 'NONE',  ( -12.08541892319999889, 1503.227962273290132, 208.3926044072909747 ) ) ;
#7510 = LINE ( 'NONE', #75830, #85819 ) ;
#7511 = CARTESIAN_POINT ( 'NONE',  ( -11.40322695539999920, 1375.342188321910044, 209.3118815522890088 ) ) ;
#7512 = B_SPLINE_CURVE_WITH_KNOTS ( 'NONE', 3,
 ( #99073, #13970, #3409, #56553, #37539, #63325 ),
 .UNSPECIFIED., .F., .F.,
 ( 4, 2, 4 ),
 ( 0.000000000000000000, 0.02504328917203360247, 0.04927314457962859995 ),
 .UNSPECIFIED. ) ;
#7513 = EDGE_CURVE ( 'NONE', #11042, #20112, #71758, .T. ) ;
#7514 = ORIENTED_EDGE ( 'NONE', *, *, #98951, .F. ) ;
#7515 = CARTESIAN_POINT ( 'NONE',  ( 2.477986732234999767, 1516.922519270759949, 205.8529865360470126 ) ) ;
#7516 = ORIENTED_EDGE ( 'NONE', *, *, #22039, .T. ) ;
#7517 = CARTESIAN_POINT ( 'NONE',  ( 19.52188586753710098, 1440.913060387330006, 213.1792421281620022 ) ) ;
#7518 = DIRECTION ( 'NONE',  ( -1.836970198721029688E-16, -1.000000000000000000, 0.000000000000000000 ) ) ;
#7519 = EDGE_CURVE ( 'NONE', #92476, #68340, #95620, .T. ) ;
#7521 = EDGE_CURVE ( 'NONE', #82285, #43603, #44875, .T. ) ;
#7520 = CARTESIAN_POINT ( 'NONE',  ( -12.59263084910000075, 1409.352804746330094, 190.6087445503980007 ) ) ;
#7522 = CARTESIAN_POINT ( 'NONE',  ( 7.645478567275000081, 1514.134513140269974, 215.1770428866170164 ) ) ;
#7524 = EDGE_LOOP ( 'NONE', ( #45606, #56564, #83485, #89018, #89075 ) ) ;
#7523 = CARTESIAN_POINT ( 'NONE',  ( 0.3443494227334849556, 1415.932840154009909, 226.9638899044090010 ) ) ;
#7525 = CARTESIAN_POINT ( 'NONE',  ( 21.53595778569999908, 1429.715726643929884, 219.1980677462979941 ) ) ;
#7526 = DIRECTION ( 'NONE',  ( -0.3090169943749382919, 2.144236138472229863E-15, 0.9510565162951565288 ) ) ;
#7527 = CARTESIAN_POINT ( 'NONE',  ( -113.4000000000000057, 1384.574445395800012, 311.2057750932590352 ) ) ;
#7528 = DIRECTION ( 'NONE',  ( -0.4978433412588614271, 0.000000000000000000, 0.8672669759446700599 ) ) ;
#7529 = AXIS2_PLACEMENT_3D ( 'NONE', #92724, #28288, #54623 ) ;
#7530 = CARTESIAN_POINT ( 'NONE',  ( 12.94490868551340057, 1411.836793529460010, 269.3560162488220158 ) ) ;
#7531 = CARTESIAN_POINT ( 'NONE',  ( 0.7564342142240020328, 1516.783665406140017, 213.7345173100169973 ) ) ;
#7532 = B_SPLINE_CURVE_WITH_KNOTS ( 'NONE', 5,
 ( #104108, #76698, #44219, #8936, #102985, #17309, #101879, #69993, #18977, #84544, #33574, #60473 ),
 .UNSPECIFIED., .F., .F.,
 ( 6, 3, 3, 6 ),
 ( 0.000000000000000000, 0.2618501547404907814, 0.6384622943148291485, 1.000000000000000000 ),
 .UNSPECIFIED. ) ;
#7533 = CARTESIAN_POINT ( 'NONE',  ( 23.56365677970000050, 1409.992931709729874, 209.3923694546319894 ) ) ;
#7534 = FACE_OUTER_BOUND ( 'NONE', #24165, .T. ) ;
#7535 = CARTESIAN_POINT ( 'NONE',  ( 7.321627509198920691, 1508.611138448520023, 214.6350682835270050 ) ) ;
#7536 = CARTESIAN_POINT ( 'NONE',  ( -2.476733514145000203, 1516.858326417339867, 211.6155457388669845 ) ) ;
#7537 = DIRECTION ( 'NONE',  ( 7.524247891465669597E-10, -7.387944558779740342E-11, 1.000000000000000000 ) ) ;
#7538 = DIRECTION ( 'NONE',  ( -1.000000000000000000, 0.000000000000000000, 0.000000000000000000 ) ) ;
#7539 =( BOUNDED_SURFACE ( )  B_SPLINE_SURFACE ( 3, 2, ( 
 ( #49576, #58526, #5349 ),
 ( #39509, #56313, #41159 ),
 ( #13723, #40053, #40605 ),
 ( #48478, #74234, #41708 ),
 ( #22668, #7554, #7000 ),
 ( #32208, #14288, #108365 ),
 ( #73682, #82616, #66935 ),
 ( #101043, #64738, #66389 ),
 ( #31646, #65278, #47908 ),
 ( #108916, #6457, #100508 ) ),
 .UNSPECIFIED., .F., .F., .F. ) 
 B_SPLINE_SURFACE_WITH_KNOTS ( ( 4, 2, 2, 2, 4 ),
 ( 3, 3 ),
 ( 0.000000000000000000, 0.3926990816987241395, 0.7853981633974482790, 1.178097245096172418, 1.570796326794896558 ),
 ( 0.000000000000000000, 1.000000000000000000 ),
 .UNSPECIFIED. ) 
 GEOMETRIC_REPRESENTATION_ITEM ( )  RATIONAL_B_SPLINE_SURFACE ( (
 ( 1.000000000000000000, 0.7763623250684322796, 1.000000000000000000),
 ( 1.000000000000000000, 0.7763684247038049602, 1.000000000000000000),
 ( 1.000000000000000000, 0.7746454561793517657, 1.000000000000000000),
 ( 1.000000000000000000, 0.7679730451976943817, 1.000000000000000000),
 ( 1.000000000000000000, 0.7630177051949541545, 1.000000000000000000),
 ( 1.000000000000000000, 0.7504512394525465480, 1.000000000000000000),
 ( 1.000000000000000000, 0.7428408967918798123, 1.000000000000000000),
 ( 1.000000000000000000, 0.7259222650918639719, 1.000000000000000000),
 ( 1.000000000000000000, 0.7166207884813426965, 1.000000000000000000),
 ( 1.000000000000000000, 0.7071067811865868746, 1.000000000000000000) ) ) 
 REPRESENTATION_ITEM ( '' )  SURFACE ( )  );
#7540 = CARTESIAN_POINT ( 'NONE',  ( 1.330041181847649856, 1409.969615095589916, 232.6005830404007213 ) ) ;
#7542 = ORIENTED_EDGE ( 'NONE', *, *, #86442, .T. ) ;
#7541 = CARTESIAN_POINT ( 'NONE',  ( -56.97380248630000210, 1389.509217074559956, 269.0144898038590213 ) ) ;
#7544 = AXIS2_PLACEMENT_3D ( 'NONE', #45884, #2787, #35815 ) ;
#7543 = CARTESIAN_POINT ( 'NONE',  ( -51.29381094165059807, 1385.114229371170040, 264.3850473588399836 ) ) ;
#7545 = CARTESIAN_POINT ( 'NONE',  ( 38.77643282620000065, 1448.325309301239713, 259.1405302821979717 ) ) ;
#7546 = CARTESIAN_POINT ( 'NONE',  ( -16.81223434880759982, 1414.913060387349788, 207.5743820648510223 ) ) ;
#7547 = CARTESIAN_POINT ( 'NONE',  ( -8.733798672629999871, 1419.056601762730224, 233.0476203166980156 ) ) ;
#7548 = CARTESIAN_POINT ( 'NONE',  ( 13.16517659032117038, 1517.151704408390060, 194.0489770726361485 ) ) ;
#7549 = CARTESIAN_POINT ( 'NONE',  ( -24.05825847430000053, 1444.359855996980059, 212.4695695426480029 ) ) ;
#7550 = CARTESIAN_POINT ( 'NONE',  ( 11.74136607283499956, 1511.863761374039996, 224.9732485802669828 ) ) ;
#7552 = CARTESIAN_POINT ( 'NONE',  ( -35.00335893040000457, 1443.851131231850104, 135.3147355765980251 ) ) ;
#7551 = CARTESIAN_POINT ( 'NONE',  ( -2.485205687335000135, 1517.181921232829836, 216.8478361320569832 ) ) ;
#7553 = CARTESIAN_POINT ( 'NONE',  ( -9.156505819859109607, 1449.262359179090026, 209.6968860301970210 ) ) ;
#7554 = CARTESIAN_POINT ( 'NONE',  ( 32.74318896774105525, 1524.667648926078300, 222.0534297170919160 ) ) ;
#7555 = VERTEX_POINT ( 'NONE', #50920 ) ;
#7556 = CARTESIAN_POINT ( 'NONE',  ( 5.001338628314999646, 1516.911981270829983, 203.3378372969070256 ) ) ;
#7557 = AXIS2_PLACEMENT_3D ( 'NONE', #55350, #104632, #71068 ) ;
#7558 = CARTESIAN_POINT ( 'NONE',  ( -27.01380866140000236, 1450.681584507220123, 136.4483241423979791 ) ) ;
#7559 = CARTESIAN_POINT ( 'NONE',  ( 12.45806603379999977, 1422.765585813930102, 223.7640243073979889 ) ) ;
#7560 = CARTESIAN_POINT ( 'NONE',  ( 38.22966134442160069, 1444.824641043079964, 137.0630644299180005 ) ) ;
#7561 = CARTESIAN_POINT ( 'NONE',  ( 30.31940284292409515, 1512.187213306747481, 195.7503880523414352 ) ) ;
#7562 = CARTESIAN_POINT ( 'NONE',  ( 26.08557971843411138, 1450.768665719140927, 136.6909322435282377 ) ) ;
#7563 = CARTESIAN_POINT ( 'NONE',  ( 0.000000000000000000, 1443.913060387330006, 126.8032249175980155 ) ) ;
#7564 = CARTESIAN_POINT ( 'NONE',  ( 29.17443018255550058, 1436.411321637160199, 136.6577757746120199 ) ) ;
#7565 = CARTESIAN_POINT ( 'NONE',  ( -38.64468767635309376, 1444.005792560380087, 137.1818110982019903 ) ) ;
#7566 = CARTESIAN_POINT ( 'NONE',  ( -21.73794315169999791, 1429.924065208830143, 218.8049817396780270 ) ) ;
#7567 = DIRECTION ( 'NONE',  ( -0.7063774289747313251, 0.04540766091858282338, 0.7063774289747313251 ) ) ;
#7568 = CARTESIAN_POINT ( 'NONE',  ( -108.7478840269999978, 1386.424881223649891, 297.4056966952589960 ) ) ;
#7569 = EDGE_CURVE ( 'NONE', #46920, #9209, #87710, .T. ) ;
#7570 = CARTESIAN_POINT ( 'NONE',  ( 13.97274253350000173, 1508.900194118629997, 185.2208288689979838 ) ) ;
#7571 = CARTESIAN_POINT ( 'NONE',  ( -21.37468300741611316, 1525.408337840050081, 184.8352431113903265 ) ) ;
#7572 = CARTESIAN_POINT ( 'NONE',  ( -16.15327634166941095, 1469.074778267816782, 269.3697231530343288 ) ) ;
#7573 = ORIENTED_EDGE ( 'NONE', *, *, #93872, .F. ) ;
#7574 = CARTESIAN_POINT ( 'NONE',  ( -26.31257376103580370, 1482.825501787880057, 210.8488302918380271 ) ) ;
#7575 = CARTESIAN_POINT ( 'NONE',  ( 5.234983244518070400, 1455.659623156430143, 218.3679346420140064 ) ) ;
#7576 = CARTESIAN_POINT ( 'NONE',  ( 642.7360634221799955, 11220.04953453920098, 2085.137448048184979 ) ) ;
#7577 = CARTESIAN_POINT ( 'NONE',  ( 13.86092937120069912, 1410.765486813650114, 191.1266627561969926 ) ) ;
#7578 = CARTESIAN_POINT ( 'NONE',  ( -1.802301101800737992, 1409.910657974563946, 186.0681198055114862 ) ) ;
#7579 = CARTESIAN_POINT ( 'NONE',  ( -12.86383581051971525, 1444.953095748689520, 186.0976155970778052 ) ) ;
#7580 = CARTESIAN_POINT ( 'NONE',  ( -9.030488842750038714, 1438.110210707299984, 210.2927785181310014 ) ) ;
#7581 = CARTESIAN_POINT ( 'NONE',  ( -2.329898843064519998, 1515.219291385629958, 213.4472495155459910 ) ) ;
#7582 = CARTESIAN_POINT ( 'NONE',  ( -12.68222283512827353, 1419.450370853951199, 228.4188145333208411 ) ) ;
#7583 = CARTESIAN_POINT ( 'NONE',  ( -3.387022137372330821, 1451.546079549640808, 153.9286616154712419 ) ) ;
#7584 = CARTESIAN_POINT ( 'NONE',  ( -18.04214276402350237, 1416.520646088689773, 209.4829372689819706 ) ) ;
#7585 = CARTESIAN_POINT ( 'NONE',  ( 25.62964228539999922, 1435.682999602769996, 136.4541818545979766 ) ) ;
#7586 = CARTESIAN_POINT ( 'NONE',  ( 17.66551557898246827, 1519.551704408389924, 217.9010776244259660 ) ) ;
#7587 = VERTEX_POINT ( 'NONE', #101843 ) ;
#7588 = CARTESIAN_POINT ( 'NONE',  ( -0.2210724871084639997, 1414.913057862230062, 192.7532066038650100 ) ) ;
#7589 = CARTESIAN_POINT ( 'NONE',  ( 21.22517422831483458, 1508.705765652955961, 226.2458636531372633 ) ) ;
#7590 = EDGE_LOOP ( 'NONE', ( #2326, #71859, #88162, #11047 ) ) ;
#7591 = VERTEX_POINT ( 'NONE', #51464 ) ;
#7592 = CARTESIAN_POINT ( 'NONE',  ( -3.300826323869999968, 1500.561897259590069, 230.1976133252990167 ) ) ;
#7593 = CARTESIAN_POINT ( 'NONE',  ( 3.669386717837979983, 1517.051704638620095, 202.5807756278150009 ) ) ;
#7595 = CARTESIAN_POINT ( 'NONE',  ( -12.77219964900000093, 1461.479478047029943, 231.7859092782980213 ) ) ;
#7594 = CARTESIAN_POINT ( 'NONE',  ( 1.878980900259999975, 1455.587583919590088, 218.5151519414690142 ) ) ;
#7596 = CARTESIAN_POINT ( 'NONE',  ( -7.374483111930000057, 1447.147829244589957, 214.6826825380690025 ) ) ;
#7597 = CARTESIAN_POINT ( 'NONE',  ( -11.87549035710000034, 1433.045081316169899, 150.0791374503980080 ) ) ;
#7598 = ADVANCED_FACE ( 'NONE', ( #85596 ), #95679, .F. ) ;
#7599 = CARTESIAN_POINT ( 'NONE',  ( -12.29413384569110157, 1378.302811799279880, 210.0202395160829951 ) ) ;
#7600 = CARTESIAN_POINT ( 'NONE',  ( -2.681752544285345596, 1420.275109781218589, 185.9665801933430487 ) ) ;
#7601 = CARTESIAN_POINT ( 'NONE',  ( 7.224319591869999613, 1424.601783486629984, 212.7752974582190291 ) ) ;
#7602 = CARTESIAN_POINT ( 'NONE',  ( -14.52664492645137351, 1429.813426209209183, 222.1557458822846627 ) ) ;
#7603 = FACE_BOUND ( 'NONE', #103983, .T. ) ;
#7604 = CARTESIAN_POINT ( 'NONE',  ( 1.530053592280000041, 1452.704408633029971, 183.4894966516980048 ) ) ;
#7605 = CARTESIAN_POINT ( 'NONE',  ( 7.875197786978843872, 1364.470992309426492, 208.3718459617061285 ) ) ;
#7606 = CARTESIAN_POINT ( 'NONE',  ( -27.54257285163602020, 1509.986926926110982, 197.2303957788377318 ) ) ;
#7608 = VERTEX_POINT ( 'NONE', #97624 ) ;
#7607 = CARTESIAN_POINT ( 'NONE',  ( -2.797860769668700114E-09, 1414.981275559920050, 244.4714746855989915 ) ) ;
#7609 = VERTEX_POINT ( 'NONE', #3590 ) ;
#7610 = CARTESIAN_POINT ( 'NONE',  ( -11.74434471530499913, 1426.711920943479981, 144.6829737354520091 ) ) ;
#7611 = DIRECTION ( 'NONE',  ( -0.01734307837366609595, 0.9988445490243716973, 0.04481946582484658964 ) ) ;
#7612 = CARTESIAN_POINT ( 'NONE',  ( -4.146669009850000975, 1471.900945888130082, 270.0721599525979855 ) ) ;
#7613 = CARTESIAN_POINT ( 'NONE',  ( 12.21136012500357637, 1434.092705541917667, 147.4644113196944204 ) ) ;
#7614 = CARTESIAN_POINT ( 'NONE',  ( -119.4939992282754417, 1358.631207110788182, 300.8926790057471408 ) ) ;
#7615 = CARTESIAN_POINT ( 'NONE',  ( 18.65529551030000022, 1453.313060387329870, 201.7949864999779948 ) ) ;
#7616 = CARTESIAN_POINT ( 'NONE',  ( -9.104938183539999841, 1384.618211218890110, 199.9573581933690036 ) ) ;
#7617 = DIRECTION ( 'NONE',  ( 0.000000000000000000, -1.000000000000000000, 6.123233995736769734E-17 ) ) ;
#7618 = DIRECTION ( 'NONE',  ( 0.3090169943749383474, -0.000000000000000000, -0.9510565162951566398 ) ) ;
#7619 = CARTESIAN_POINT ( 'NONE',  ( 8.653423937789300524, 1367.169888897622059, 210.6218459616991936 ) ) ;
#7620 = CARTESIAN_POINT ( 'NONE',  ( -9.409898537430208876, 1446.992683627339829, 212.1329179144990178 ) ) ;
#7621 = CARTESIAN_POINT ( 'NONE',  ( -6.126475865403940624, 1406.019691185119882, 267.8379111553729786 ) ) ;
#7622 = CARTESIAN_POINT ( 'NONE',  ( -13.07119275721439955, 1435.903469544349946, 150.6799624932950223 ) ) ;
#7623 = VERTEX_POINT ( 'NONE', #72437 ) ;
#7624 = CARTESIAN_POINT ( 'NONE',  ( -4.327230971739010279, 1515.149487411890050, 209.5135165373189921 ) ) ;
#7625 = ORIENTED_EDGE ( 'NONE', *, *, #95512, .F. ) ;
#7626 = ORIENTED_EDGE ( 'NONE', *, *, #78141, .F. ) ;
#7627 = CARTESIAN_POINT ( 'NONE',  ( 8.002723364794999128, 1516.551704408390151, 206.0688700356170102 ) ) ;
#7628 = CARTESIAN_POINT ( 'NONE',  ( 9.651063919191019025, 1425.440657924460083, 195.4941620015079877 ) ) ;
#7630 = CARTESIAN_POINT ( 'NONE',  ( 0.1315954949189999945, 1432.375264448149892, 200.6910518521459892 ) ) ;
#7629 = CARTESIAN_POINT ( 'NONE',  ( -2.477986770365000257, 1516.922519270759949, 212.3907053662870226 ) ) ;
#7631 = CARTESIAN_POINT ( 'NONE',  ( 5.441672368615000366, 1511.126521646420088, 216.8250749888169935 ) ) ;
#7632 = DIRECTION ( 'NONE',  ( 0.000000000000000000, 0.000000000000000000, -1.000000000000000000 ) ) ;
#7633 = VERTEX_POINT ( 'NONE', #4663 ) ;
#7634 = CARTESIAN_POINT ( 'NONE',  ( -109.5441724399999970, 1379.437034645699896, 304.2218460466590386 ) ) ;
#7635 = ADVANCED_FACE ( 'NONE', ( #107115 ), #7859, .T. ) ;
#7636 = EDGE_CURVE ( 'NONE', #74254, #40999, #11875, .T. ) ;
#7637 = EDGE_CURVE ( 'NONE', #104222, #32267, #106325, .T. ) ;
#7638 = CARTESIAN_POINT ( 'NONE',  ( -5.781490582474999584, 1516.807958722750072, 202.5702025453269925 ) ) ;
#7639 = ADVANCED_FACE ( 'NONE', ( #65132 ), #57934, .T. ) ;
#7640 = CARTESIAN_POINT ( 'NONE',  ( -1.117292507960000014, 1467.878890391829827, 230.3293191710980068 ) ) ;
#7641 = EDGE_CURVE ( 'NONE', #69447, #63442, #51603, .T. ) ;
#7642 = CARTESIAN_POINT ( 'NONE',  ( -31.76456352044490572, 1384.560446604800063, 206.5901853932080030 ) ) ;
#7643 = CARTESIAN_POINT ( 'NONE',  ( -2.590851938810000199, 1407.641758401829975, 196.2196012994980094 ) ) ;
#7644 = CARTESIAN_POINT ( 'NONE',  ( -24.08426305480000451, 1411.115211393229856, 208.6111285346999864 ) ) ;
#7646 = ORIENTED_EDGE ( 'NONE', *, *, #107638, .T. ) ;
#7645 = CARTESIAN_POINT ( 'NONE',  ( 20.70484064406359437, 1525.907212628473872, 185.0411015109854134 ) ) ;
#7647 = CARTESIAN_POINT ( 'NONE',  ( -26.29896967323349699, 1469.338024908179932, 210.2737814497969850 ) ) ;
#7648 = CARTESIAN_POINT ( 'NONE',  ( 26.64485081109999953, 1469.250187268130048, 209.0988510226020196 ) ) ;
#7649 = CARTESIAN_POINT ( 'NONE',  ( -18.22628348410981047, 1379.600014138350616, 212.7175748282816414 ) ) ;
#7650 = EDGE_CURVE ( 'NONE', #35149, #2466, #36912, .T. ) ;
#7651 = CARTESIAN_POINT ( 'NONE',  ( -10.73113664029999903, 1382.357287394640252, 201.1356155892590039 ) ) ;
#7652 = CARTESIAN_POINT ( 'NONE',  ( -13.08109920040210028, 1436.034850317789960, 150.7074356796669861 ) ) ;
#7653 = CARTESIAN_POINT ( 'NONE',  ( 0.1595995995380000143, 1486.508831850330125, 181.8147405652979671 ) ) ;
#7654 = CARTESIAN_POINT ( 'NONE',  ( -1.118104767724999782, 1516.965971551240045, 211.4215139361070044 ) ) ;
#7655 = CARTESIAN_POINT ( 'NONE',  ( -68.30075113750000071, 1379.746851987089940, 279.1016318162590437 ) ) ;
#7656 = CARTESIAN_POINT ( 'NONE',  ( -2.065269763300760175, 1484.249225516169872, 183.0195811470669867 ) ) ;
#7657 = FACE_OUTER_BOUND ( 'NONE', #70071, .T. ) ;
#7658 = CARTESIAN_POINT ( 'NONE',  ( 18.80463394749709138, 1425.801072080043696, 225.6039047707025134 ) ) ;
#7659 = CARTESIAN_POINT ( 'NONE',  ( -7.339107240745000205, 1517.203017563489766, 207.9963360818169917 ) ) ;
#7660 = EDGE_LOOP ( 'NONE', ( #88905, #14828 ) ) ;
#7661 = CARTESIAN_POINT ( 'NONE',  ( -38.81202645930000017, 1450.612734574169963, 134.0999998922980012 ) ) ;
#7663 = EDGE_CURVE ( 'NONE', #10365, #32988, #103765, .T. ) ;
#7662 = CARTESIAN_POINT ( 'NONE',  ( -8.825147375033820296, 1438.586940765240115, 208.4641837083139819 ) ) ;
#7664 = CARTESIAN_POINT ( 'NONE',  ( 10.78872034293299897, 1416.913057013769958, 222.2791104510660034 ) ) ;
#7665 = EDGE_LOOP ( 'NONE', ( #61933, #6659, #56431, #22841 ) ) ;
#7666 = FACE_OUTER_BOUND ( 'NONE', #38525, .T. ) ;
#7667 = CARTESIAN_POINT ( 'NONE',  ( 12.92083169069850079, 1434.847021224489936, 149.8557914971470097 ) ) ;
#7668 = CARTESIAN_POINT ( 'NONE',  ( 7.829103442970730242, 1468.998337108560008, 233.3189757471670021 ) ) ;
#7669 = EDGE_CURVE ( 'NONE', #68439, #8198, #47635, .T. ) ;
#7670 = CARTESIAN_POINT ( 'NONE',  ( -14.96473955119999921, 1416.430699836160102, 207.9564624935089796 ) ) ;
#7671 = CARTESIAN_POINT ( 'NONE',  ( -11.11039799191612509, 1425.147017898752893, 138.4692043722531594 ) ) ;
#7672 = CARTESIAN_POINT ( 'NONE',  ( 3.965821128770000481, 1486.919029566390009, 198.6437641315989993 ) ) ;
#7673 = EDGE_CURVE ( 'NONE', #109170, #48273, #85146, .T. ) ;
#7674 = CARTESIAN_POINT ( 'NONE',  ( 1.468816372564279993, 1431.317999364719981, 218.4991881548640151 ) ) ;
#7675 = CARTESIAN_POINT ( 'NONE',  ( 4.232343036945110271, 1441.513652504289894, 164.4116054800499853 ) ) ;
#7677 = CARTESIAN_POINT ( 'NONE',  ( -7.000000000000000000, 1432.413060387330006, 146.1721969590979882 ) ) ;
#7676 = CARTESIAN_POINT ( 'NONE',  ( 0.01289778877310149806, 1516.939723362869927, 214.1281058189269970 ) ) ;
#7678 = CARTESIAN_POINT ( 'NONE',  ( 21.01954381400000216, 1509.698214756829884, 188.0278171981979938 ) ) ;
#7679 = CARTESIAN_POINT ( 'NONE',  ( -7.716252091104999877, 1516.810037859429940, 216.0641906620670056 ) ) ;
#7680 = ORIENTED_EDGE ( 'NONE', *, *, #8925, .F. ) ;
#7681 = CARTESIAN_POINT ( 'NONE',  ( -12.45685420760000106, 1416.832348283729971, 194.7671534681980177 ) ) ;
#7682 = CARTESIAN_POINT ( 'NONE',  ( -16.99051315430000386, 1420.323703249610162, 203.8408267910690199 ) ) ;
#7683 = EDGE_CURVE ( 'NONE', #61362, #88484, #60942, .T. ) ;
#7684 = CARTESIAN_POINT ( 'NONE',  ( 1.192913453829999915, 1420.839100914329947, 183.5603160090979884 ) ) ;
#7685 = CARTESIAN_POINT ( 'NONE',  ( 0.6307243961899989815, 1474.949842634390052, 220.1414127045989915 ) ) ;
#7686 = CARTESIAN_POINT ( 'NONE',  ( 3.261863598262784603, 1524.739915903631982, 176.4692008623654829 ) ) ;
#7687 = CARTESIAN_POINT ( 'NONE',  ( -11040.89558200930696, 2833.596074015641989, -8386.665009981023104 ) ) ;
#7688 = FACE_OUTER_BOUND ( 'NONE', #89830, .T. ) ;
#7689 = CARTESIAN_POINT ( 'NONE',  ( -16.17568633703940151, 1459.146939663510011, 230.7169128052520080 ) ) ;
#7690 = CARTESIAN_POINT ( 'NONE',  ( 17.31687731428424115, 1422.595274621808130, 226.6249846890611650 ) ) ;
#7691 = DIRECTION ( 'NONE',  ( 1.000000000000000000, 0.000000000000000000, 0.000000000000000000 ) ) ;
#7692 = CARTESIAN_POINT ( 'NONE',  ( -7.390160694869999602, 1438.194204504490017, 149.6789596403979772 ) ) ;
#7693 = CARTESIAN_POINT ( 'NONE',  ( 42.25133546600230261, 1440.913060352949969, 262.2708174827409948 ) ) ;
#7695 = CARTESIAN_POINT ( 'NONE',  ( -14.77048072796499945, 1514.151220560310094, 224.0952811371670066 ) ) ;
#7694 = CARTESIAN_POINT ( 'NONE',  ( -7.015951070247499644, 1421.061870212209897, 194.1995972353730053 ) ) ;
#7696 = DIRECTION ( 'NONE',  ( 0.000000000000000000, 0.000000000000000000, -1.000000000000000000 ) ) ;
#7697 = ORIENTED_EDGE ( 'NONE', *, *, #60037, .T. ) ;
#7698 = ORIENTED_EDGE ( 'NONE', *, *, #33959, .F. ) ;
#7699 = CARTESIAN_POINT ( 'NONE',  ( 14.43915977099999992, 1435.431951939009878, 149.5788185351979962 ) ) ;
#7700 = CARTESIAN_POINT ( 'NONE',  ( -19.42676974918696331, 1485.587889656283323, 189.9363221898242671 ) ) ;
#7701 = DIRECTION ( 'NONE',  ( 1.158258077154680071E-09, -1.836970198721029688E-16, -1.000000000000000000 ) ) ;
#7702 = CARTESIAN_POINT ( 'NONE',  ( 2.294753475282899302, 1410.371478230091043, 185.5182217525652675 ) ) ;
#7703 = LINE ( 'NONE', #41863, #55387 ) ;
#7704 = CARTESIAN_POINT ( 'NONE',  ( 16.06472692613853681, 1509.595107636989042, 234.5263603880145524 ) ) ;
#7705 = EDGE_CURVE ( 'NONE', #21410, #10141, #52835, .T. ) ;
#7706 = CARTESIAN_POINT ( 'NONE',  ( 33.91369120210129751, 1435.681798817170147, 134.0999999980979851 ) ) ;
#7707 = CARTESIAN_POINT ( 'NONE',  ( 20.71343476517511917, 1522.382868172863937, 179.9059455038194812 ) ) ;
#7708 = CARTESIAN_POINT ( 'NONE',  ( -56.45588150975670061, 1383.801723053599972, 274.2314575997830275 ) ) ;
#7709 = CARTESIAN_POINT ( 'NONE',  ( -0.01367056625530000021, 1452.767332469330086, 153.3854620859980002 ) ) ;
#7710 = ADVANCED_FACE ( 'NONE', ( #4531 ), #40008, .F. ) ;
#7711 = CARTESIAN_POINT ( 'NONE',  ( 10.01013843233299916, 1469.369181467840008, 209.9819040969830155 ) ) ;
#7712 = CARTESIAN_POINT ( 'NONE',  ( 11.86092065826349895, 1492.895007130480053, 212.5849778500719935 ) ) ;
#7714 = ORIENTED_EDGE ( 'NONE', *, *, #33706, .T. ) ;
#7713 = CARTESIAN_POINT ( 'NONE',  ( 1.776582264570000014, 1456.341121776589716, 219.1753798333990062 ) ) ;
#7715 = FACE_OUTER_BOUND ( 'NONE', #30958, .T. ) ;
#7716 = CARTESIAN_POINT ( 'NONE',  ( -51.11582849079999846, 1379.961985591460007, 254.5469988028590365 ) ) ;
#7717 = CARTESIAN_POINT ( 'NONE',  ( 8.062587302181759341, 1436.235894220949831, 206.1282943059349861 ) ) ;
#7718 = ORIENTED_EDGE ( 'NONE', *, *, #56962, .F. ) ;
#7719 = ORIENTED_EDGE ( 'NONE', *, *, #74104, .T. ) ;
#7720 = CARTESIAN_POINT ( 'NONE',  ( -13.50563910776669907, 1440.103950034289710, 194.8057323916819996 ) ) ;
#7721 = CARTESIAN_POINT ( 'NONE',  ( -8.747709872648618656, 1385.329978680540080, 218.6507686934189962 ) ) ;
#7722 = CARTESIAN_POINT ( 'NONE',  ( 36.58809064867419636, 1437.689614402119787, 136.5472558022989915 ) ) ;
#7724 = DIRECTION ( 'NONE',  ( 0.03489949670250495212, 0.9993908270190956511, 0.000000000000000000 ) ) ;
#7723 = DIRECTION ( 'NONE',  ( 5.497413460834789123E-05, 0.09152419561177496665, -0.9958028512689959255 ) ) ;
#7725 = CARTESIAN_POINT ( 'NONE',  ( 11.55221588404359956, 1480.217597516799970, 211.4789165460060190 ) ) ;
#7726 = CARTESIAN_POINT ( 'NONE',  ( -107.4285199579999954, 1381.409267714380121, 298.6311223556590448 ) ) ;
#7727 = EDGE_CURVE ( 'NONE', #18777, #102315, #26187, .T. ) ;
#7728 = CARTESIAN_POINT ( 'NONE',  ( -21.54116136312493879, 1523.382868172864164, 234.3126182787005689 ) ) ;
#7729 = CARTESIAN_POINT ( 'NONE',  ( -3.827327205999999649, 1422.542708386029972, 168.6405287067979941 ) ) ;
#7730 = CARTESIAN_POINT ( 'NONE',  ( -15.66330071820020287, 1508.551704408389924, 214.2112499943270052 ) ) ;
#7731 = CARTESIAN_POINT ( 'NONE',  ( -1.240189040380000218, 1457.347231108689812, 202.3619262432189885 ) ) ;
#7732 = CARTESIAN_POINT ( 'NONE',  ( 2.322154075020000263, 1410.372404442829975, 185.5255194826980016 ) ) ;
#7733 = CARTESIAN_POINT ( 'NONE',  ( 1.031331416711620097, 1508.991934534589973, 179.4420581554169871 ) ) ;
#7734 = CARTESIAN_POINT ( 'NONE',  ( 6.343729916319600370, 1432.997535027899858, 202.2534603803919993 ) ) ;
#7735 = CARTESIAN_POINT ( 'NONE',  ( -3.116664625471300187, 1441.244075315679993, 166.9150288857020143 ) ) ;
#7736 = B_SPLINE_CURVE_WITH_KNOTS ( 'NONE', 3,
 ( #63392, #97507, #38689, #5089, #20776, #39242, #54977, #12390, #38145, #59384 ),
 .UNSPECIFIED., .F., .F.,
 ( 4, 3, 3, 4 ),
 ( -12.93235455439439896, -12.28324979274049866, -11.03322287909449884, -9.791994790430690543 ),
 .UNSPECIFIED. ) ;
#7737 = CARTESIAN_POINT ( 'NONE',  ( -24.24033364359999965, 1452.066569283630088, 137.1576854437979875 ) ) ;
#7738 = ORIENTED_EDGE ( 'NONE', *, *, #11122, .T. ) ;
#7739 = CARTESIAN_POINT ( 'NONE',  ( -20.40768745807410056, 1466.146701207289880, 211.1092863667410029 ) ) ;
#7740 = FACE_OUTER_BOUND ( 'NONE', #30378, .T. ) ;
#7741 = CARTESIAN_POINT ( 'NONE',  ( 19.58792912137019826, 1456.031451223419936, 227.9529518234539864 ) ) ;
#7742 = DIRECTION ( 'NONE',  ( -0.9822959463214659959, 0.1391731009602450164, 0.1254014426134129889 ) ) ;
#7743 = CARTESIAN_POINT ( 'NONE',  ( 17.91320533999999753, 1507.617064948130064, 188.5294956351980318 ) ) ;
#7744 = EDGE_CURVE ( 'NONE', #45421, #75670, #4778, .T. ) ;
#7745 = CARTESIAN_POINT ( 'NONE',  ( -9.767263980911179754E-11, 1470.490992744460073, 255.3083357207799793 ) ) ;
#7746 = LINE ( 'NONE', #92298, #103559 ) ;
#7747 = CARTESIAN_POINT ( 'NONE',  ( -13.13536861894177576, 1507.686078928800043, 209.3105439034022197 ) ) ;
#7748 = CARTESIAN_POINT ( 'NONE',  ( -2.851018948600000158, 1476.884648983389980, 199.1362811694189929 ) ) ;
#7749 = CARTESIAN_POINT ( 'NONE',  ( -106.1392238060000039, 1388.866019527689787, 308.9234258288589672 ) ) ;
#7750 = CARTESIAN_POINT ( 'NONE',  ( -0.2620786904165167130, 1485.927256572733086, 181.8391900102611203 ) ) ;
#7751 = CARTESIAN_POINT ( 'NONE',  ( -8.144230935551448169, 1360.896704102203103, 210.6218459617030021 ) ) ;
#7752 = CARTESIAN_POINT ( 'NONE',  ( -46.12691182732100259, 1439.415857468709874, 266.9728105068039667 ) ) ;
#7753 = CARTESIAN_POINT ( 'NONE',  ( 13.88631813555559980, 1509.307012642660084, 234.3182586601199944 ) ) ;
#7754 = ADVANCED_FACE ( 'NONE', ( #53157 ), #103531, .T. ) ;
#7755 = CARTESIAN_POINT ( 'NONE',  ( -8.082242560709998358, 1425.089483080600075, 208.3127043135090162 ) ) ;
#7756 = CARTESIAN_POINT ( 'NONE',  ( -4.037051035714999792, 1516.939819969850078, 209.1350663277499962 ) ) ;
#7757 = DIRECTION ( 'NONE',  ( -0.02616798426433289068, 0.9993150019884036173, 0.02616798426433289068 ) ) ;
#7758 = CARTESIAN_POINT ( 'NONE',  ( 12.63038619288439968, 1428.207532477410041, 223.9332333053530135 ) ) ;
#7759 = CARTESIAN_POINT ( 'NONE',  ( 7.513965249524710011, 1425.915627064070122, 212.2777243754379981 ) ) ;
#7760 = CARTESIAN_POINT ( 'NONE',  ( -25.92826244057819807, 1451.942608940840046, 135.5698208547320007 ) ) ;
#7761 = ORIENTED_EDGE ( 'NONE', *, *, #26199, .T. ) ;
#7762 = CARTESIAN_POINT ( 'NONE',  ( 11.60711259459999845, 1422.283843339130044, 221.4360218614980340 ) ) ;
#7764 = CARTESIAN_POINT ( 'NONE',  ( -15.22870591643729909, 1512.406412987999829, 222.1534140603669698 ) ) ;
#7763 = CARTESIAN_POINT ( 'NONE',  ( -2.744860781518600579, 1525.790286462510494, 177.2996071530072300 ) ) ;
#7765 = EDGE_CURVE ( 'NONE', #109440, #5037, #65514, .T. ) ;
#7766 = FACE_OUTER_BOUND ( 'NONE', #19937, .T. ) ;
#7767 = CARTESIAN_POINT ( 'NONE',  ( -20.40418802293068623, 1454.957320664023200, 226.6330256283032725 ) ) ;
#7768 = CARTESIAN_POINT ( 'NONE',  ( 8.454790733525280544, 1428.363638633589972, 213.4109935021670026 ) ) ;
#7769 = EDGE_CURVE ( 'NONE', #20179, #73741, #107496, .T. ) ;
#7770 = CARTESIAN_POINT ( 'NONE',  ( -13.95553461971410414, 1416.818673879764901, 221.9083874777307130 ) ) ;
#7771 = ORIENTED_EDGE ( 'NONE', *, *, #8363, .F. ) ;
#7772 = CARTESIAN_POINT ( 'NONE',  ( -4.820018915960121220, 1409.974924445299848, 270.0724225275779418 ) ) ;
#7773 = CARTESIAN_POINT ( 'NONE',  ( 15.99884507355850083, 1421.963095027500003, 227.5209166517219899 ) ) ;
#7774 = CARTESIAN_POINT ( 'NONE',  ( -0.2746046721839675020, 1507.636717399409008, 237.3923158053290763 ) ) ;
#7775 = ORIENTED_EDGE ( 'NONE', *, *, #2245, .F. ) ;
#7776 = ORIENTED_EDGE ( 'NONE', *, *, #10600, .F. ) ;
#7777 = B_SPLINE_CURVE_WITH_KNOTS ( 'NONE', 5,
 ( #88083, #89162, #52825, #87525, #11371, #2987 ),
 .UNSPECIFIED., .F., .F.,
 ( 6, 6 ),
 ( 0.000000000000000000, 1.000000000000000000 ),
 .UNSPECIFIED. ) ;
#7778 = CARTESIAN_POINT ( 'NONE',  ( -23.94120819599999805, 1410.421789068329872, 209.3772794782499886 ) ) ;
#7779 = ADVANCED_FACE ( 'NONE', ( #73250 ), #27939, .T. ) ;
#7780 = VERTEX_POINT ( 'NONE', #32348 ) ;
#7781 = CARTESIAN_POINT ( 'NONE',  ( -5.062155874537689115, 1439.003721114779864, 206.7420737057830138 ) ) ;
#7782 = DIRECTION ( 'NONE',  ( -1.000000000000000000, 0.000000000000000000, 0.000000000000000000 ) ) ;
#7783 = EDGE_CURVE ( 'NONE', #90951, #54360, #98182, .T. ) ;
#7784 = CARTESIAN_POINT ( 'NONE',  ( -2.833554060450000023, 1507.639777131729943, 236.8757964686979847 ) ) ;
#7785 = CARTESIAN_POINT ( 'NONE',  ( -17.85390903009999874, 1410.880990427929873, 225.0173061825979914 ) ) ;
#7786 = CARTESIAN_POINT ( 'NONE',  ( 45.81235299787979898, 1442.782150107359939, 268.7577288735689649 ) ) ;
#7787 = CARTESIAN_POINT ( 'NONE',  ( -0.8768788928080630818, 1424.155975923929873, 228.3063952870599849 ) ) ;
#7788 = CARTESIAN_POINT ( 'NONE',  ( -16.94513000609982356, 1421.950298552636241, 226.8362257794649111 ) ) ;
#7789 = CARTESIAN_POINT ( 'NONE',  ( -0.7568987378019988999, 1516.805675336850072, 205.0906771642370074 ) ) ;
#7790 = ORIENTED_EDGE ( 'NONE', *, *, #68617, .T. ) ;
#7791 = CARTESIAN_POINT ( 'NONE',  ( 19.00830952430770893, 1457.291692359948456, 226.5122007821947818 ) ) ;
#7792 = CARTESIAN_POINT ( 'NONE',  ( 14.77306016951930090, 1514.147575501539905, 194.1509863539160108 ) ) ;
#7793 = LINE ( 'NONE', #68838, #62312 ) ;
#7794 = EDGE_LOOP ( 'NONE', ( #49867, #22893, #74763, #96499 ) ) ;
#7795 = FACE_OUTER_BOUND ( 'NONE', #48962, .T. ) ;
#7796 = CARTESIAN_POINT ( 'NONE',  ( 27.02941372530000308, 1451.801869924330049, 135.6489090826979975 ) ) ;
#7797 = CARTESIAN_POINT ( 'NONE',  ( -3.780333225011479836, 1508.551704408389924, 213.7482560551979986 ) ) ;
#7798 = CARTESIAN_POINT ( 'NONE',  ( 12.33991424210799970, 1501.419616770270068, 212.2020435037020150 ) ) ;
#7799 = CARTESIAN_POINT ( 'NONE',  ( 8.135441375949998388, 1421.256651981180084, 196.0379973919989709 ) ) ;
#7800 = ADVANCED_FACE ( 'NONE', ( #22254 ), #83843, .T. ) ;
#7801 = DIRECTION ( 'NONE',  ( 0.6038592750913972518, -0.7071067811868637643, -0.3679048462383240903 ) ) ;
#7802 = CARTESIAN_POINT ( 'NONE',  ( -4.867399450039999742, 1495.075882605090101, 197.7983437550990118 ) ) ;
#7803 = CARTESIAN_POINT ( 'NONE',  ( 1.762714104866460074, 1408.974615720260090, 186.8633000340620072 ) ) ;
#7805 = DIRECTION ( 'NONE',  ( -1.000000000000000000, 0.000000000000000000, 0.000000000000000000 ) ) ;
#7804 = CARTESIAN_POINT ( 'NONE',  ( 1.265494006419999984, 1415.708214660429803, 232.9654935851980042 ) ) ;
#7806 = CARTESIAN_POINT ( 'NONE',  ( 15.26168084529999902, 1409.446010026229715, 225.6870430949980175 ) ) ;
#7807 = CARTESIAN_POINT ( 'NONE',  ( -11.79942310750000090, 1380.362273894700138, 215.1811282860990104 ) ) ;
#7808 = ADVANCED_FACE ( 'NONE', ( #109605 ), #23912, .T. ) ;
#7809 = CARTESIAN_POINT ( 'NONE',  ( 17.22592475670000312, 1444.324653571829913, 162.9227486557980171 ) ) ;
#7810 = ORIENTED_EDGE ( 'NONE', *, *, #25761, .T. ) ;
#7811 = CARTESIAN_POINT ( 'NONE',  ( 12.60587301698949858, 1415.938742849230039, 221.9392866525910222 ) ) ;
#7812 = CARTESIAN_POINT ( 'NONE',  ( 11.50213335426050065, 1432.340329806790123, 151.2059253680629922 ) ) ;
#7813 = CARTESIAN_POINT ( 'NONE',  ( -10.45913315801519872, 1483.337912596790147, 203.4298690767190010 ) ) ;
#7814 = CARTESIAN_POINT ( 'NONE',  ( -12.49220149360000143, 1391.410447351959874, 209.7524444900410003 ) ) ;
#7815 = CARTESIAN_POINT ( 'NONE',  ( 15.20279842864010078, 1514.921193439799936, 225.0317510863630162 ) ) ;
#7816 = CARTESIAN_POINT ( 'NONE',  ( 11.85965305928869995, 1425.934783538740021, 202.8481194454130048 ) ) ;
#7817 = CARTESIAN_POINT ( 'NONE',  ( -11.03352341481849841, 1462.446812322350070, 208.7213867630900097 ) ) ;
#7818 = CARTESIAN_POINT ( 'NONE',  ( -37.18025134340000193, 1449.733372748519969, 265.6112251771979800 ) ) ;
#7819 = CARTESIAN_POINT ( 'NONE',  ( -10.37617513879240150, 1479.403831811299824, 210.6295454707710064 ) ) ;
#7820 = CARTESIAN_POINT ( 'NONE',  ( 11.88085280169999969, 1433.210362566009962, 150.1928659671980029 ) ) ;
#7821 = CARTESIAN_POINT ( 'NONE',  ( 31.32742178079999462, 1444.517716078169997, 255.3819207742980097 ) ) ;
#7822 = CARTESIAN_POINT ( 'NONE',  ( 12.50239138351419932, 1416.520646088689773, 196.1087943541830043 ) ) ;
#7823 = CARTESIAN_POINT ( 'NONE',  ( -17.54341085149529889, 1417.941250412889985, 206.8706738254780078 ) ) ;
#7824 = CARTESIAN_POINT ( 'NONE',  ( 12.90319585266200164, 1420.986560144630175, 203.4264861624149887 ) ) ;
#7825 = AXIS2_PLACEMENT_3D ( 'NONE', #110230, #68272, #85023 ) ;
#7826 = CARTESIAN_POINT ( 'NONE',  ( 8.179457570200950656, 1464.307649058119978, 216.6184750703820043 ) ) ;
#7827 = CARTESIAN_POINT ( 'NONE',  ( 2.370970874524633398, 1427.002265528473799, 137.0999999980980135 ) ) ;
#7828 = CARTESIAN_POINT ( 'NONE',  ( -6.790918657024139549, 1517.051704408389924, 184.0243675267330161 ) ) ;
#7829 = CARTESIAN_POINT ( 'NONE',  ( -17.03047024470000181, 1409.672928417430057, 225.3166904351979838 ) ) ;
#7830 = CARTESIAN_POINT ( 'NONE',  ( 23.92333147209999922, 1430.353917304629931, 213.3463240754979893 ) ) ;
#7831 = AXIS2_PLACEMENT_3D ( 'NONE', #92683, #9249, #69734 ) ;
#7832 = CARTESIAN_POINT ( 'NONE',  ( 0.5996034049719994874, 1477.819945573845416, 198.7231221488051744 ) ) ;
#7833 = CARTESIAN_POINT ( 'NONE',  ( -1.085894894499999928E-15, 1432.353341358199941, 150.3995506339979897 ) ) ;
#7834 = CARTESIAN_POINT ( 'NONE',  ( -16.59345386669420108, 1383.857040005859972, 219.6283172069809666 ) ) ;
#7835 = CARTESIAN_POINT ( 'NONE',  ( -2.425477467415915189, 1523.390106123591067, 175.1521078860136527 ) ) ;
#7836 =( BOUNDED_SURFACE ( )  B_SPLINE_SURFACE ( 3, 2, ( 
 ( #86491, #52915, #1398 ),
 ( #88168, #61883, #87047 ),
 ( #52371, #80310, #69732 ),
 ( #27697, #87616, #45077 ),
 ( #3626, #10335, #103851 ),
 ( #37206, #61335, #105515 ),
 ( #79220, #18719, #54582 ),
 ( #44507, #28806, #78654 ),
 ( #36106, #70292, #63003 ),
 ( #36649, #97111, #95999 ) ),
 .UNSPECIFIED., .F., .F., .F. ) 
 B_SPLINE_SURFACE_WITH_KNOTS ( ( 4, 2, 2, 2, 4 ),
 ( 3, 3 ),
 ( 0.000000000000000000, 0.3926990816987241395, 0.7853981633974482790, 1.178097245096172418, 1.570796326794896558 ),
 ( 0.000000000000000000, 1.000000000000000000 ),
 .UNSPECIFIED. ) 
 GEOMETRIC_REPRESENTATION_ITEM ( )  RATIONAL_B_SPLINE_SURFACE ( (
 ( 1.000000000000000000, 0.7763623250684343891, 1.000000000000000000),
 ( 1.000000000000000000, 0.7763684247033950658, 1.000000000000000000),
 ( 1.000000000000000000, 0.7746454561798882255, 1.000000000000000000),
 ( 1.000000000000000000, 0.7679730451971521488, 1.000000000000000000),
 ( 1.000000000000000000, 0.7630177051937461208, 1.000000000000000000),
 ( 1.000000000000000000, 0.7504512394537481423, 1.000000000000000000),
 ( 1.000000000000000000, 0.7428408967937900620, 1.000000000000000000),
 ( 1.000000000000000000, 0.7259222650899548324, 1.000000000000000000),
 ( 1.000000000000000000, 0.7166207884827766605, 1.000000000000000000),
 ( 1.000000000000000000, 0.7071067811865866526, 1.000000000000000000) ) ) 
 REPRESENTATION_ITEM ( '' )  SURFACE ( )  );
#7837 = CARTESIAN_POINT ( 'NONE',  ( -17.55008883411199960, 1487.029577352629758, 194.9701233786059902 ) ) ;
#7838 = CARTESIAN_POINT ( 'NONE',  ( -7.710610441124999603, 1516.594591938570147, 212.5759658869370128 ) ) ;
#7839 = CARTESIAN_POINT ( 'NONE',  ( -22.46469623289999618, 1417.574324945069975, 209.9387869133350080 ) ) ;
#7840 = CARTESIAN_POINT ( 'NONE',  ( 0.1690262106856909863, 1480.902069235160070, 182.0556410569679997 ) ) ;
#7842 = ORIENTED_EDGE ( 'NONE', *, *, #22655, .T. ) ;
#7841 = DIRECTION ( 'NONE',  ( 0.000000000000000000, 1.000000000000000000, 0.000000000000000000 ) ) ;
#7843 = CARTESIAN_POINT ( 'NONE',  ( -13.26516604059999693, 1444.994950788470987, 176.9857848810979704 ) ) ;
#7844 = DIRECTION ( 'NONE',  ( -1.156023075842281927E-31, 1.000000000000000000, -1.698192320643030073E-16 ) ) ;
#7845 = CARTESIAN_POINT ( 'NONE',  ( 3.968827103902559550, 1519.551704408389924, 188.7040005461919918 ) ) ;
#7846 = CARTESIAN_POINT ( 'NONE',  ( -40.66293689394410649, 1439.821779689789992, 134.0999999980979851 ) ) ;
#7847 = CARTESIAN_POINT ( 'NONE',  ( -29.38941616001999790, 1446.173485192630096, 137.1432708197739885 ) ) ;
#7848 = ORIENTED_EDGE ( 'NONE', *, *, #51201, .T. ) ;
#7849 = B_SPLINE_SURFACE_WITH_KNOTS ( 'NONE', 5, 5, ( 
 ( #110363, #33640, #25233, #86262, #52133, #9550 ),
 ( #52682, #86818, #26919, #34760, #78996, #35312 ),
 ( #87381, #43176, #95771, #19037, #105275, #9003 ),
 ( #104171, #19603, #62198, #629, #68947, #103047 ),
 ( #10110, #43720, #36410, #60543, #44282, #78426 ),
 ( #26345, #95223, #69498, #104720, #20151, #77873 ) ),
 .UNSPECIFIED., .F., .F., .F.,
 ( 6, 6 ),
 ( 6, 6 ),
 ( 29.52656374780000093, 158.0439293190000001 ),
 ( 0.000000000000000000, 1.000000000000000000 ),
 .UNSPECIFIED. ) ;
#7850 = CARTESIAN_POINT ( 'NONE',  ( -5.485381178602870555, 1391.646552095490051, 203.3186572502850140 ) ) ;
#7851 = DIRECTION ( 'NONE',  ( 0.000000000000000000, 0.000000000000000000, 1.000000000000000000 ) ) ;
#7852 = CARTESIAN_POINT ( 'NONE',  ( 7.835755939781712698, 1447.918173471444334, 204.3989379467183198 ) ) ;
#7853 = CARTESIAN_POINT ( 'NONE',  ( -28.84709929359999947, 1507.919204203629988, 212.2396942135479776 ) ) ;
#7854 = AXIS2_PLACEMENT_3D ( 'NONE', #65378, #101136, #6549 ) ;
#7855 = CARTESIAN_POINT ( 'NONE',  ( -8.284402606713660688, 1436.555342802109863, 212.1856797791610063 ) ) ;
#7856 = CARTESIAN_POINT ( 'NONE',  ( -15.70179666829999832, 1415.698136594249945, 210.0629521891549985 ) ) ;
#7857 = CARTESIAN_POINT ( 'NONE',  ( 7.650637082874630401, 1409.180226521390068, 221.9865298110669869 ) ) ;
#7858 = CARTESIAN_POINT ( 'NONE',  ( 2.500000002320000192, 1428.690610018730013, 183.7723879534980256 ) ) ;
#7859 = B_SPLINE_SURFACE_WITH_KNOTS ( 'NONE', 5, 1, ( 
 ( #89218, #38254 ),
 ( #98713, #21430 ),
 ( #4129, #56165 ),
 ( #64041, #55642 ),
 ( #89763, #13034 ),
 ( #106031, #97079 ) ),
 .UNSPECIFIED., .F., .F., .F.,
 ( 6, 6 ),
 ( 2, 2 ),
 ( 3.552713678800000397E-15, 14.76708736389999999 ),
 ( 0.000000000000000000, 14.00000000000000000 ),
 .UNSPECIFIED. ) ;
#7860 = CARTESIAN_POINT ( 'NONE',  ( -80.90147208277250002, 1385.161082712429788, 284.2695106278820276 ) ) ;
#7861 = CIRCLE ( 'NONE', #36488, 1.999999999999998668 ) ;
#7862 = CARTESIAN_POINT ( 'NONE',  ( -11.46257124287919993, 1391.913060387289988, 211.1273318420540193 ) ) ;
#7863 = CARTESIAN_POINT ( 'NONE',  ( 10.54782078997249961, 1426.750615647500126, 208.6717185375519819 ) ) ;
#7864 = ORIENTED_EDGE ( 'NONE', *, *, #109531, .T. ) ;
#7865 = CARTESIAN_POINT ( 'NONE',  ( -30.94580556280000039, 1451.832637120030085, 135.2368415506980170 ) ) ;
#7866 = CARTESIAN_POINT ( 'NONE',  ( 13.35741048202589809, 1443.501467202830099, 164.9741927960640453 ) ) ;
#7868 = ORIENTED_EDGE ( 'NONE', *, *, #30820, .T. ) ;
#7867 = CARTESIAN_POINT ( 'NONE',  ( 3.346707516019999940, 1443.005054410889898, 217.3642451189890323 ) ) ;
#7869 = CARTESIAN_POINT ( 'NONE',  ( 2.252978874640000129, 1474.529339387290065, 219.9022295252989920 ) ) ;
#7870 = CARTESIAN_POINT ( 'NONE',  ( -18.70871766619247722, 1410.928537324267609, 223.5363647290388940 ) ) ;
#7871 = CARTESIAN_POINT ( 'NONE',  ( -8.538839991170080523, 1362.569232148532137, 210.6218459616987957 ) ) ;
#7872 = CARTESIAN_POINT ( 'NONE',  ( -0.1681676274470000065, 1420.473121337229941, 182.7663689088979879 ) ) ;
#7873 = CARTESIAN_POINT ( 'NONE',  ( 38.93029842025811860, 1452.410457501353221, 269.5917637810125598 ) ) ;
#7874 = CARTESIAN_POINT ( 'NONE',  ( 17.95066969181503325, 1434.914995825377446, 215.4365105091481496 ) ) ;
#7875 = CARTESIAN_POINT ( 'NONE',  ( 1.797565579689999860, 1415.903556134529936, 232.4419632246980143 ) ) ;
#7876 = CARTESIAN_POINT ( 'NONE',  ( 9.709932644140000235, 1450.584296204089924, 205.0446109545989941 ) ) ;
#7877 = CARTESIAN_POINT ( 'NONE',  ( -23.79097509939970934, 1507.893976353429935, 222.8398596609989966 ) ) ;
#7878 = CARTESIAN_POINT ( 'NONE',  ( 3.679272716979999913, 1453.313060387329870, 228.5941172881979924 ) ) ;
#7879 = CARTESIAN_POINT ( 'NONE',  ( -10.22078022364619976, 1448.827725899079724, 207.2905427559460065 ) ) ;
#7880 = CARTESIAN_POINT ( 'NONE',  ( -2.492443689034999910, 1516.793978928989873, 205.8699571027569846 ) ) ;
#7881 = CARTESIAN_POINT ( 'NONE',  ( 2.704615531860000033, 1447.046937274380070, 168.9986710020979785 ) ) ;
#7882 = VERTEX_POINT ( 'NONE', #102829 ) ;
#7883 = FACE_OUTER_BOUND ( 'NONE', #6114, .T. ) ;
#7884 = CARTESIAN_POINT ( 'NONE',  ( 13.44384801999999901, 1473.247726564130062, 270.1124235791980368 ) ) ;
#7886 = ORIENTED_EDGE ( 'NONE', *, *, #89086, .T. ) ;
#7885 = CARTESIAN_POINT ( 'NONE',  ( -68.65513241966479541, 1379.747663328290173, 280.2694831111389817 ) ) ;
#7887 = CARTESIAN_POINT ( 'NONE',  ( -10.87959984532081315, 1378.671789283537464, 214.9412694382895950 ) ) ;
#7888 = ORIENTED_EDGE ( 'NONE', *, *, #110593, .T. ) ;
#7889 = CARTESIAN_POINT ( 'NONE',  ( -16.68633777358233061, 1513.912053498707792, 222.9853921125541376 ) ) ;
#7890 = CARTESIAN_POINT ( 'NONE',  ( -25.29760786810000184, 1449.800867303260020, 206.6892432500980306 ) ) ;
#7892 = CARTESIAN_POINT ( 'NONE',  ( 16.15008297119439717, 1409.578690898410059, 192.4543258895550082 ) ) ;
#7891 = CARTESIAN_POINT ( 'NONE',  ( -11.18153660112279901, 1426.464409952729966, 103.8952900393150003 ) ) ;
#7893 = CARTESIAN_POINT ( 'NONE',  ( 2.299983577604999940, 1516.861367446839949, 211.4044688825970013 ) ) ;
#7894 = CARTESIAN_POINT ( 'NONE',  ( 40.62990447646500058, 1439.681968513619950, 135.2802037849949954 ) ) ;
#7895 = EDGE_CURVE ( 'NONE', #13762, #35724, #67873, .T. ) ;
#7896 = CARTESIAN_POINT ( 'NONE',  ( 21.60845823726257464, 1524.659148609483054, 234.6463771270923360 ) ) ;
#7897 = CARTESIAN_POINT ( 'NONE',  ( -11.15477664960000048, 1425.160652183429875, 144.1598853320980140 ) ) ;
#7898 = CARTESIAN_POINT ( 'NONE',  ( -12.33979512284740032, 1378.416654683770048, 209.3708442725699967 ) ) ;
#7900 = ADVANCED_FACE ( 'NONE', ( #17152 ), #95557, .F. ) ;
#7899 = CARTESIAN_POINT ( 'NONE',  ( 17.11202944081011168, 1460.312853445443579, 228.6673605825106392 ) ) ;
#7901 = ITEM_DEFINED_TRANSFORMATION ( 'NONE', 'NONE', #62700,  #21632 ) ;
#7902 = CARTESIAN_POINT ( 'NONE',  ( 2.674013553562669898, 1508.551704408389924, 214.1019878693419969 ) ) ;
#7903 = CARTESIAN_POINT ( 'NONE',  ( -3.000000000000000000, 1374.913060387289988, 209.1218459616989946 ) ) ;
#7904 = VERTEX_POINT ( 'NONE', #9350 ) ;
#7905 = CARTESIAN_POINT ( 'NONE',  ( -21.26810766760000249, 1485.919195121089842, 201.7808564926190229 ) ) ;
#7906 = CARTESIAN_POINT ( 'NONE',  ( -1.925297170580940076, 1522.051704408389924, 187.5582988486569889 ) ) ;
#7907 = VERTEX_POINT ( 'NONE', #86600 ) ;
#7908 = ORIENTED_EDGE ( 'NONE', *, *, #77071, .F. ) ;
#7909 = AXIS2_PLACEMENT_3D ( 'NONE', #48143, #74457, #48700 ) ;
#7910 = CARTESIAN_POINT ( 'NONE',  ( -29.71787946601863339, 1509.988004069222825, 210.0607825035318115 ) ) ;
#7911 = CARTESIAN_POINT ( 'NONE',  ( 10.36757158123830003, 1453.224707006280141, 211.3662413356020124 ) ) ;
#7912 = CARTESIAN_POINT ( 'NONE',  ( -14.26759209886279933, 1380.297660956990057, 210.2716803301690334 ) ) ;
#7913 = CARTESIAN_POINT ( 'NONE',  ( -12.37112953626025735, 1417.358968133092048, 199.9426545053605651 ) ) ;
#7914 = CARTESIAN_POINT ( 'NONE',  ( 4.324092172210000307, 1515.269353063089966, 209.4835653193450185 ) ) ;
#7915 = AXIS2_PLACEMENT_3D ( 'NONE', #31833, #4973, #40788 ) ;
#7916 = CARTESIAN_POINT ( 'NONE',  ( -4.933290692019969725, 1455.123182729209930, 201.0873875226590144 ) ) ;
#7917 = ADVANCED_FACE ( 'NONE', ( #26124 ), #14964, .T. ) ;
#7918 = CARTESIAN_POINT ( 'NONE',  ( 40.71747596589879947, 1438.773003663980035, 134.7402664639769796 ) ) ;
#7919 = CARTESIAN_POINT ( 'NONE',  ( -0.08509234499448949107, 1516.966051576868949, 216.6298010462417665 ) ) ;
#7920 = B_SPLINE_SURFACE_WITH_KNOTS ( 'NONE', 5, 5, ( 
 ( #51803, #85371, #69164, #95453, #26009, #67511 ),
 ( #110590, #312, #102180, #101614, #103268, #26577 ),
 ( #60206, #50689, #93233, #18718, #33876, #87046 ),
 ( #52370, #69731, #34984, #77554, #10334, #68612 ),
 ( #52914, #110043, #77006, #9785, #16500, #17603 ),
 ( #86490, #8120, #85944, #24901, #94325, #18173 ),
 ( #44506, #9245, #76437, #60774, #42287, #857 ),
 ( #68068, #43951, #33316, #25460, #94899, #61334 ),
 ( #59655, #78094, #1396, #27149, #93763, #17041 ) ),
 .UNSPECIFIED., .F., .F., .F.,
 ( 6, 3, 6 ),
 ( 6, 6 ),
 ( 3.257013150990000216, 5.599849328569999507, 7.942685506149999242 ),
 ( 0.000000000000000000, 2.000000000000000000 ),
 .UNSPECIFIED. ) ;
#7921 = CARTESIAN_POINT ( 'NONE',  ( 25.40031078099999817, 1438.607438808799998, 138.1536180571980026 ) ) ;
#7922 = CARTESIAN_POINT ( 'NONE',  ( -10.33438234840000014, 1391.913060387289988, 213.9065263758590163 ) ) ;
#7923 = CARTESIAN_POINT ( 'NONE',  ( -95.92809462355350547, 1384.860634349370230, 295.2544286719970046 ) ) ;
#7924 = ORIENTED_EDGE ( 'NONE', *, *, #106730, .T. ) ;
#7925 = CARTESIAN_POINT ( 'NONE',  ( -3.454119954834999895, 1516.594591938570147, 201.4112355291069889 ) ) ;
#7926 = CARTESIAN_POINT ( 'NONE',  ( -4.623892098755000291, 1517.066898074209803, 208.3852847535989952 ) ) ;
#7927 = ORIENTED_EDGE ( 'NONE', *, *, #85881, .F. ) ;
#7928 = CARTESIAN_POINT ( 'NONE',  ( 19.32263322520000060, 1455.378559704889767, 209.1218459616989946 ) ) ;
#7929 = B_SPLINE_CURVE_WITH_KNOTS ( 'NONE', 5,
 ( #110661, #52989, #87122, #59187, #18243, #95523, #94975, #33954, #59728 ),
 .UNSPECIFIED., .F., .F.,
 ( 6, 3, 6 ),
 ( 0.000000000000000000, 0.3844850474641056115, 1.000000000000000000 ),
 .UNSPECIFIED. ) ;
#7930 = CARTESIAN_POINT ( 'NONE',  ( 20.28670476199999939, 1497.716955700230073, 227.3610620833980249 ) ) ;
#7931 = ORIENTED_EDGE ( 'NONE', *, *, #70625, .T. ) ;
#7932 = CARTESIAN_POINT ( 'NONE',  ( -13.79060599709999835, 1416.547221146729953, 221.8961093151980037 ) ) ;
#7933 = CARTESIAN_POINT ( 'NONE',  ( -11.83148324045470012, 1432.336210885780019, 150.3814747831369800 ) ) ;
#7934 = CARTESIAN_POINT ( 'NONE',  ( -17.24773937279860192, 1420.120834743239811, 204.7828160326650107 ) ) ;
#7935 = CARTESIAN_POINT ( 'NONE',  ( -9.851064782010787724, 1490.933270807075132, 214.0922473749026267 ) ) ;
#7936 = CARTESIAN_POINT ( 'NONE',  ( -13.30235076369999980, 1426.047137753730112, 222.1935098235980206 ) ) ;
#7937 = MANIFOLD_SOLID_BREP ( 'Stock-MAS-682-1', #35981 ) ;
#7938 = CARTESIAN_POINT ( 'NONE',  ( -8.568239406770191025, 1446.651419842080713, 153.8735861858707210 ) ) ;
#7939 = CARTESIAN_POINT ( 'NONE',  ( -0.03625434476629999653, 1508.564801718729768, 180.3428531422979972 ) ) ;
#7940 = CARTESIAN_POINT ( 'NONE',  ( -10.46250751532009993, 1491.356802638789986, 212.5409670664860187 ) ) ;
#7941 = CARTESIAN_POINT ( 'NONE',  ( -56.72784561730000519, 1379.717687562220135, 254.3030452203590244 ) ) ;
#7942 = CARTESIAN_POINT ( 'NONE',  ( -14.66954656289999903, 1451.336034133729981, 222.9742526267980054 ) ) ;
#7944 = CARTESIAN_POINT ( 'NONE',  ( 2.487935142314050108, 1509.038615934839981, 213.6090957367470082 ) ) ;
#7943 = CARTESIAN_POINT ( 'NONE',  ( -3.807470111109999777, 1497.262881795189742, 198.5198641202990189 ) ) ;
#7945 = CARTESIAN_POINT ( 'NONE',  ( -4.546321247799015808, 1423.767664050271151, 184.3780306669439426 ) ) ;
#7946 = ADVANCED_FACE ( 'NONE', ( #103954 ), #88770, .F. ) ;
#7947 = CARTESIAN_POINT ( 'NONE',  ( -5.365571251823850751, 1422.412084457530000, 136.7230467533039757 ) ) ;
#7948 = EDGE_LOOP ( 'NONE', ( #80381, #71777, #45644, #14878 ) ) ;
#7949 = CARTESIAN_POINT ( 'NONE',  ( -1.307006097452011906, 1486.249936161337018, 181.8003811105465104 ) ) ;
#7950 = DIRECTION ( 'NONE',  ( -0.6736849260863841948, 0.000000000000000000, 0.7390186874254148774 ) ) ;
#7951 = CARTESIAN_POINT ( 'NONE',  ( -1.121950782074999875, 1517.123342927159911, 214.1352753262870010 ) ) ;
#7952 = CARTESIAN_POINT ( 'NONE',  ( -2.902304511463737136, 1484.512052158883762, 183.2899361315264741 ) ) ;
#7953 = ADVANCED_FACE ( 'NONE', ( #68725 ), #54806, .T. ) ;
#7954 = CARTESIAN_POINT ( 'NONE',  ( -11.60004869885203860, 1426.112400841504041, 139.0398264042692063 ) ) ;
#7955 = TOROIDAL_SURFACE ( 'NONE', #68811, 3.250000000000000000, 0.5000000000000000000 ) ;
#7957 = ORIENTED_EDGE ( 'NONE', *, *, #100216, .F. ) ;
#7956 = CARTESIAN_POINT ( 'NONE',  ( 4.333361510917200121, 1508.551704406479985, 213.7899733016769801 ) ) ;
#7958 = CARTESIAN_POINT ( 'NONE',  ( -8.848550363540001129, 1384.918645891350025, 199.9247479929690030 ) ) ;
#7959 = CARTESIAN_POINT ( 'NONE',  ( -0.9720884905540009280, 1508.551704159290011, 220.3304486672990095 ) ) ;
#7960 = CARTESIAN_POINT ( 'NONE',  ( -11.44957079769999986, 1425.470528643129910, 145.1412166744979970 ) ) ;
#7961 = CARTESIAN_POINT ( 'NONE',  ( -10.84547348403736322, 1425.250141514038660, 146.5429171640950585 ) ) ;
#7962 = CARTESIAN_POINT ( 'NONE',  ( -4.055165558009999671, 1441.344553830540008, 184.7145706676980126 ) ) ;
#7963 = CARTESIAN_POINT ( 'NONE',  ( 14.38071331779389794, 1509.494653947579991, 235.3234850005289900 ) ) ;
#7964 = CARTESIAN_POINT ( 'NONE',  ( 21.06331657220000153, 1496.634916824290030, 207.0954909778190256 ) ) ;
#7965 = CARTESIAN_POINT ( 'NONE',  ( 18.54783228039999798, 1474.422996780290077, 200.1179429635390079 ) ) ;
#7967 = CARTESIAN_POINT ( 'NONE',  ( -10.78800201790000024, 1480.681111995489800, 211.1294777214090175 ) ) ;
#7966 = CARTESIAN_POINT ( 'NONE',  ( -20.02122337150000320, 1470.088377314129957, 226.2655331251979760 ) ) ;
#7968 = CARTESIAN_POINT ( 'NONE',  ( -17.15404056067600180, 1460.895016437030108, 228.2717488779379948 ) ) ;
#7969 = ORIENTED_EDGE ( 'NONE', *, *, #40056, .T. ) ;
#7970 = CARTESIAN_POINT ( 'NONE',  ( -2.492443689034999910, 1516.793978928989873, 205.8699571027569846 ) ) ;
#7971 = CARTESIAN_POINT ( 'NONE',  ( 21.63331298869999841, 1410.785270426130182, 269.4984061937980186 ) ) ;
#7972 = B_SPLINE_SURFACE_WITH_KNOTS ( 'NONE', 5, 1, ( 
 ( #38084, #106391 ),
 ( #29675, #30777 ),
 ( #21242, #55455 ),
 ( #89581, #12874 ),
 ( #47053, #60418 ),
 ( #7781, #93989 ) ),
 .UNSPECIFIED., .F., .F., .F.,
 ( 6, 6 ),
 ( 2, 2 ),
 ( -2.253879340347439943E-05, 15.90092593249339892 ),
 ( 0.000000000000000000, 14.00002253879340053 ),
 .UNSPECIFIED. ) ;
#7973 = CARTESIAN_POINT ( 'NONE',  ( 19.33005223189999811, 1449.732321041979958, 192.5069533228979992 ) ) ;
#7974 = CARTESIAN_POINT ( 'NONE',  ( -0.1513279769116150086, 1507.119540709420107, 237.3446492454640122 ) ) ;
#7975 = CARTESIAN_POINT ( 'NONE',  ( 19.53786426059019021, 1512.187213306747481, 181.5239794925693388 ) ) ;
#7976 = CARTESIAN_POINT ( 'NONE',  ( -1.555019539419999930, 1450.617762354220076, 182.9982681214980005 ) ) ;
#7977 = B_SPLINE_CURVE_WITH_KNOTS ( 'NONE', 3,
 ( #59570, #95371, #44991, #774, #1887, #94248, #34902, #76922, #85860, #53384, #36023, #18635, #52832, #69089, #103190, #1318, #86410, #9700, #25378, #78011, #70214, #35459, #87533, #104318, #10821, #79138, #20846, #88089, #64545, #5157, #79687, #12993, #98108, #104872, #97574, #96474, #11376, #30354, #3543, #37113, #105988, #88638, #12460, #62350, #63456, #55592, #71314, #4619, #81855, #55042, #63997, #62924, #89169, #45548, #46643, #38755, #47723, #105428, #89716, #47176, #107069, #37666, #21927, #19754, #80225, #72930, #2993, #56120, #98664, #53955, #28717, #71872, #97035, #90255, #13537, #54502, #20298, #11916, #28162, #46093, #29263, #72392, #70760, #80777, #81304, #4084, #38208, #106521, #29809, #21382, #15724, #40958, #6799, #48842, #82427, #49378, #74032, #82966, #50486, #90812, #58328, #14655, #33105, #5722, #84609, #108719, #100318, #56677, #67294, #39315, #48284, #92453, #66745, #73485, #66199, #65083, #14095, #109824, #6260, #39866, #74584, #57248, #91912, #30905 ),
 .UNSPECIFIED., .F., .F.,
 ( 4, 3, 3, 3, 3, 3, 3, 3, 3, 3, 3, 3, 3, 3, 3, 3, 3, 3, 3, 3, 3, 3, 3, 3, 3, 3, 3, 3, 3, 3, 3, 3, 3, 3, 3, 3, 3, 3, 3, 3, 3, 4 ),
 ( 1.525827422200500012E-12, 0.7233976230870560187, 1.453179569741549937, 2.189205328521389937, 2.931232241145099948, 3.681692766298920283, 4.436664690071680184, 5.195519429214390250, 5.957507372262750067, 6.722615320280829643, 7.488461881906269824, 8.253940118726170283, 8.872098167640000810, 9.627621990570389698, 10.37987637364419946, 11.12818954277669903, 11.87201083186580064, 12.60808579110319982, 13.25493343014260006, 13.90338779108970080, 14.62763215072740053, 14.71347577215040126, 15.43831616715549870, 16.16939286010799748, 16.92109434835699844, 17.66675291633200118, 18.41722697190180114, 19.17198454560039877, 19.93209662288229822, 20.69429497494040149, 21.45845626021019825, 22.18300476610000160, 22.94765126737859973, 23.71051286168500027, 24.46875718313560100, 25.22311654196029806, 25.97295706232930002, 26.71776956687309834, 27.45421738225800112, 28.18570414815399872, 28.90920564465159970, 29.42721172040000610 ),
 .UNSPECIFIED. ) ;
#7978 = CARTESIAN_POINT ( 'NONE',  ( 2.994688454485729956, 1464.609795419120246, 236.6065850994260131 ) ) ;
#7979 = CARTESIAN_POINT ( 'NONE',  ( -15.44336791849999990, 1417.906189380320029, 203.8647015642989970 ) ) ;
#7980 = B_SPLINE_CURVE_WITH_KNOTS ( 'NONE', 5,
 ( #70681, #88016, #3459, #28637, #6048, #104794 ),
 .UNSPECIFIED., .F., .F.,
 ( 6, 6 ),
 ( 0.000000000000000000, 1.000000000000000000 ),
 .UNSPECIFIED. ) ;
#7981 = CARTESIAN_POINT ( 'NONE',  ( -14.66018946070000162, 1444.034773379980152, 188.9384452558980172 ) ) ;
#7982 = CARTESIAN_POINT ( 'NONE',  ( -17.35500899530000041, 1519.913060387329779, 225.0914276473980067 ) ) ;
#7983 = CARTESIAN_POINT ( 'NONE',  ( -8.601854796231091171, 1436.861797634760023, 209.7917467578280082 ) ) ;
#7984 = CARTESIAN_POINT ( 'NONE',  ( -4.234183914609999988, 1496.289481068690066, 219.5317350564990022 ) ) ;
#7985 = CARTESIAN_POINT ( 'NONE',  ( 1.464604549361590013, 1491.527831886150125, 181.7930722882989869 ) ) ;
#7986 = CARTESIAN_POINT ( 'NONE',  ( -9.562842837499999860, 1427.428384263329917, 219.6133833293980047 ) ) ;
#7987 = B_SPLINE_CURVE_WITH_KNOTS ( 'NONE', 5,
 ( #63657, #39531, #30573, #21046, #37883, #38415, #97772, #29462, #55248, #22140, #47931, #37330 ),
 .UNSPECIFIED., .F., .F.,
 ( 6, 3, 3, 6 ),
 ( 0.000000000000000000, 3.329846645400000416, 4.930332151970000076, 12.58720418400000085 ),
 .UNSPECIFIED. ) ;
#7988 = CARTESIAN_POINT ( 'NONE',  ( -11.14967447845340054, 1508.551708988489963, 208.5621525772319842 ) ) ;
#7989 = CARTESIAN_POINT ( 'NONE',  ( 34.18677586421189574, 1522.382868172863937, 219.7932833225211766 ) ) ;
#7990 = CARTESIAN_POINT ( 'NONE',  ( -14.47363261859999994, 1473.619884778130199, 269.4256078961980165 ) ) ;
#7991 = CARTESIAN_POINT ( 'NONE',  ( 1.356522472024429993, 1410.335674015750101, 232.6399073486850000 ) ) ;
#7992 = CARTESIAN_POINT ( 'NONE',  ( -11.92422183665363633, 1391.277242661766650, 212.8274714238102945 ) ) ;
#7993 = CARTESIAN_POINT ( 'NONE',  ( -25.78156413019999960, 1509.813372445429877, 223.1298229008980059 ) ) ;
#7994 = CARTESIAN_POINT ( 'NONE',  ( -59.28208669626069849, 1384.698609697830079, 279.7264640965560147 ) ) ;
#7995 = CARTESIAN_POINT ( 'NONE',  ( -3.152270363119999974, 1474.954422145789977, 198.1306181043989909 ) ) ;
#7996 = AXIS2_PLACEMENT_3D ( 'NONE', #10466, #88833, #63659 ) ;
#7997 = CARTESIAN_POINT ( 'NONE',  ( -6.692947047070000544, 1442.760174925260117, 154.8612665581980252 ) ) ;
#7998 = B_SPLINE_SURFACE_WITH_KNOTS ( 'NONE', 5, 5, ( 
 ( #10244, #44420, #93140, #70204, #16408, #84734 ),
 ( #8031, #33780, #76351, #102084, #93673, #59559 ),
 ( #89159, #72382, #97565, #53945, #11368, #2983 ),
 ( #106511, #37104, #10811, #97025, #104310, #71303 ),
 ( #28709, #29800, #11907, #20837, #27601, #38743 ),
 ( #37656, #46632, #80766, #54492, #80214, #105978 ) ),
 .UNSPECIFIED., .F., .F., .F.,
 ( 6, 6 ),
 ( 6, 6 ),
 ( 29.60743822950000137, 29.67279265790000053 ),
 ( 0.000000000000000000, 2.000000000000000000 ),
 .UNSPECIFIED. ) ;
#7999 = CARTESIAN_POINT ( 'NONE',  ( -24.15811863269659909, 1444.790571029629973, 211.5220723686269935 ) ) ;
#8000 = CARTESIAN_POINT ( 'NONE',  ( -15.85591190879999779, 1415.880081504350073, 209.4912631162540038 ) ) ;
#8001 = DIRECTION ( 'NONE',  ( 0.1403900382919506529, 0.9900962767066567860, 0.000000000000000000 ) ) ;
#8002 = CARTESIAN_POINT ( 'NONE',  ( -22.45312464719999923, 1409.861582708429978, 204.8525374248079913 ) ) ;
#8003 = CARTESIAN_POINT ( 'NONE',  ( -11.09965908892124986, 1378.958238937004126, 203.7193492967838324 ) ) ;
#8004 = CARTESIAN_POINT ( 'NONE',  ( 4.702020435729999726, 1486.019901504789914, 218.8180113132190172 ) ) ;
#8005 = CARTESIAN_POINT ( 'NONE',  ( 10.35218644306529967, 1480.376106472589981, 207.1666581537910190 ) ) ;
#8006 = B_SPLINE_SURFACE_WITH_KNOTS ( 'NONE', 5, 5, ( 
 ( #30003, #107272, #23256, #40622, #57995, #64194 ),
 ( #91582, #23803, #5926, #38951, #92128, #64757 ),
 ( #48495, #14856, #80975, #13741, #73130, #46846 ),
 ( #4279, #82635, #100524, #38409, #98316, #40072 ),
 ( #74251, #83182, #6472, #47378, #108383, #31664 ),
 ( #89916, #56886, #98868, #47925, #21595, #55800 ) ),
 .UNSPECIFIED., .F., .F., .F.,
 ( 6, 6 ),
 ( 6, 6 ),
 ( 0.000000000000000000, 8.626417477929999578 ),
 ( 0.000000000000000000, 1.000000000000000000 ),
 .UNSPECIFIED. ) ;
#8007 = CARTESIAN_POINT ( 'NONE',  ( -4.714294778569999749E-15, 1435.943783413959864, 150.5249316333980119 ) ) ;
#8008 = CARTESIAN_POINT ( 'NONE',  ( -8.109401236050000961, 1440.034690421490041, 228.6983774484990022 ) ) ;
#8009 = CARTESIAN_POINT ( 'NONE',  ( 16.54283724222780450, 1524.843178112495707, 180.8452489027513934 ) ) ;
#8010 = CARTESIAN_POINT ( 'NONE',  ( -7.547972033258790958, 1385.319132597686121, 219.0723451529433987 ) ) ;
#8012 = CARTESIAN_POINT ( 'NONE',  ( -12.11165857595690021, 1378.231759176429932, 211.4183186711239841 ) ) ;
#8011 = CARTESIAN_POINT ( 'NONE',  ( -22.55885438500000006, 1410.621632387330010, 211.7835870406779861 ) ) ;
#8013 = CARTESIAN_POINT ( 'NONE',  ( 11.70658720183600110, 1426.715707391050046, 141.9907706309280115 ) ) ;
#8014 = DIRECTION ( 'NONE',  ( -0.000000000000000000, -1.000000000000000000, -0.000000000000000000 ) ) ;
#8015 = CARTESIAN_POINT ( 'NONE',  ( -122.8636594665699988, 1366.350733876289951, 299.0518252276390285 ) ) ;
#8016 = DIRECTION ( 'NONE',  ( -0.000000000000000000, -1.000000000000000000, -0.000000000000000000 ) ) ;
#8017 = DIRECTION ( 'NONE',  ( 0.5117323852940948159, -0.8591449038673372174, 0.000000000000000000 ) ) ;
#8018 = CARTESIAN_POINT ( 'NONE',  ( -6.556651409415000131, 1516.858146885269889, 202.5689485651570010 ) ) ;
#8019 = CARTESIAN_POINT ( 'NONE',  ( -12.60641157257676603, 1398.286779454209181, 212.2965709224484954 ) ) ;
#8020 = FACE_OUTER_BOUND ( 'NONE', #56108, .T. ) ;
#8021 = FACE_BOUND ( 'NONE', #109025, .T. ) ;
#8022 = CARTESIAN_POINT ( 'NONE',  ( 1.457628745759999900, 1507.679360684230005, 236.7889182215979815 ) ) ;
#8023 = CARTESIAN_POINT ( 'NONE',  ( 2.724500461543110319, 1367.224846223802842, 209.6218459617148824 ) ) ;
#8025 = VERTEX_POINT ( 'NONE', #18828 ) ;
#8024 = CARTESIAN_POINT ( 'NONE',  ( -25.86321635541839825, 1379.618046691589825, 215.5872060442630129 ) ) ;
#8026 = VERTEX_POINT ( 'NONE', #16602 ) ;
#8027 = CARTESIAN_POINT ( 'NONE',  ( 11.29013490629070127, 1434.173224897529963, 151.5467475927899841 ) ) ;
#8028 = CARTESIAN_POINT ( 'NONE',  ( 0.006135582747789999729, 1395.974572298430076, 220.7500239725980009 ) ) ;
#8029 = VERTEX_POINT ( 'NONE', #25570 ) ;
#8030 = CARTESIAN_POINT ( 'NONE',  ( -0.0002528412978207496297, 1396.454035521046762, 221.4895412923443985 ) ) ;
#8031 = CARTESIAN_POINT ( 'NONE',  ( -109.9850237230000118, 1384.918752160720032, 311.4561207072590037 ) ) ;
#8032 = CARTESIAN_POINT ( 'NONE',  ( -8.045796819630000485, 1385.423934774039935, 218.7531554344589892 ) ) ;
#8034 = CARTESIAN_POINT ( 'NONE',  ( 17.75627633020000218, 1419.037206885730029, 225.8504925643980243 ) ) ;
#8033 = CARTESIAN_POINT ( 'NONE',  ( 17.10397118209110090, 1459.366159650030113, 190.0191433627400102 ) ) ;
#8035 = CARTESIAN_POINT ( 'NONE',  ( 18.06964159120650137, 1488.412039253179955, 229.4705429282849991 ) ) ;
#8036 = B_SPLINE_CURVE_WITH_KNOTS ( 'NONE', 3,
 ( #26796, #61531, #33516, #60984, #26232, #17813, #95660, #53125, #87262, #67718, #10556, #11123, #36854, #88367, #11657, #106803, #104612, #54241, #46938, #80523, #4371, #71047, #27906, #45832, #62090, #89463, #30093, #28460, #79423, #96215, #54779, #55331, #97310, #64287, #29552, #45282, #63737, #78880, #29017, #98408, #70494, #3839, #88911 ),
 .UNSPECIFIED., .F., .F.,
 ( 4, 3, 3, 3, 3, 3, 3, 3, 3, 3, 3, 3, 3, 3, 4 ),
 ( 0.7655572723440000615, 0.9910019269298769862, 1.224379706003839940, 1.462078625881179983, 1.704827365636400138, 1.793853281190000093, 2.038466594486210148, 2.281256481516179768, 2.316155491860000026, 2.583989317150000353, 2.855920922269310047, 3.139267324261280301, 3.387490793020000002, 3.680707212640610404, 3.835724788559999876 ),
 .UNSPECIFIED. ) ;
#8037 = CARTESIAN_POINT ( 'NONE',  ( 4.249520622459999508, 1449.235034532409827, 184.3503851686980113 ) ) ;
#8038 = CARTESIAN_POINT ( 'NONE',  ( -2.763735881080000123, 1415.425644477329797, 191.8448309814980064 ) ) ;
#8039 = PLANE ( 'NONE',  #33939 ) ;
#8040 = CARTESIAN_POINT ( 'NONE',  ( 3.067664574526319576, 1396.020185594800068, 198.5347274153989758 ) ) ;
#8042 = CIRCLE ( 'NONE', #101134, 1.999999954277524639 ) ;
#8041 = CARTESIAN_POINT ( 'NONE',  ( 14.43002663333369995, 1416.512142030569976, 196.8803429896850048 ) ) ;
#8043 = CARTESIAN_POINT ( 'NONE',  ( 11.29278012259999997, 1431.667649477319856, 151.4912647795979979 ) ) ;
#8044 = CARTESIAN_POINT ( 'NONE',  ( 6.017564063794999640, 1514.771170611759999, 201.2298835190769921 ) ) ;
#8045 = VERTEX_POINT ( 'NONE', #59765 ) ;
#8046 = CARTESIAN_POINT ( 'NONE',  ( 13.22467655529630015, 1434.956598927620007, 149.6122180398979822 ) ) ;
#8047 = ORIENTED_EDGE ( 'NONE', *, *, #44567, .T. ) ;
#8048 = ORIENTED_EDGE ( 'NONE', *, *, #5552, .T. ) ;
#8049 = CARTESIAN_POINT ( 'NONE',  ( 13.46491591593493631, 1444.254331750074925, 169.3609691702259852 ) ) ;
#8050 = CARTESIAN_POINT ( 'NONE',  ( -8.808667445430000242, 1463.337573581429979, 235.3868220254979917 ) ) ;
#8051 = CARTESIAN_POINT ( 'NONE',  ( -8.343905337393612953, 1474.683381955320783, 203.1186823195534146 ) ) ;
#8052 = CARTESIAN_POINT ( 'NONE',  ( 2.291047489114999891, 1516.524310051880093, 216.8306159772470210 ) ) ;
#8053 = CARTESIAN_POINT ( 'NONE',  ( -8.566427451443020757, 1511.406470015435389, 214.2518601733771675 ) ) ;
#8054 = CARTESIAN_POINT ( 'NONE',  ( -19.03146662611517925, 1442.920952512881286, 211.1498405880065548 ) ) ;
#8055 = DIRECTION ( 'NONE',  ( -0.000000000000000000, -1.000000000000000000, -0.000000000000000000 ) ) ;
#8056 = CARTESIAN_POINT ( 'NONE',  ( -7.543040680839999901, 1375.366160259910203, 209.1218465795010104 ) ) ;
#8057 = EDGE_CURVE ( 'NONE', #13119, #42516, #63528, .T. ) ;
#8058 = EDGE_LOOP ( 'NONE', ( #12887, #52962, #53977, #47483, #10445, #27618, #62663, #66338, #34292, #49746 ) ) ;
#8059 = CARTESIAN_POINT ( 'NONE',  ( -2.299014068865000038, 1516.811292230880099, 206.2578025137869986 ) ) ;
#8060 = ORIENTED_EDGE ( 'NONE', *, *, #92004, .F. ) ;
#8061 = CARTESIAN_POINT ( 'NONE',  ( -2.330134126090000368, 1515.064792882589927, 204.7923971856590128 ) ) ;
#8062 = DIRECTION ( 'NONE',  ( -0.1070030146457459225, 0.000000000000000000, -0.9942586961433740322 ) ) ;
#8063 = EDGE_CURVE ( 'NONE', #80510, #92712, #69123, .T. ) ;
#8064 = CARTESIAN_POINT ( 'NONE',  ( -4.398465238590000048, 1410.004223061730045, 186.8505807875980054 ) ) ;
#8065 = CARTESIAN_POINT ( 'NONE',  ( 7.943523441464999557, 1514.557408760809949, 215.5609834051570033 ) ) ;
#8067 = EDGE_LOOP ( 'NONE', ( #90257, #48479, #13275, #15713, #25224 ) ) ;
#8066 = CARTESIAN_POINT ( 'NONE',  ( 0.2707663694632699847, 1415.088012641449950, 226.0844260569690221 ) ) ;
#8068 = CARTESIAN_POINT ( 'NONE',  ( 19.02456972039999883, 1426.130241254430075, 222.9765850832980050 ) ) ;
#8069 = CARTESIAN_POINT ( 'NONE',  ( 4.253777714910000007, 1442.471859903390168, 216.9083338397390150 ) ) ;
#8070 = DIRECTION ( 'NONE',  ( 0.03215278745245312569, -0.09160167974437756488, 0.9952765095826616726 ) ) ;
#8071 = CARTESIAN_POINT ( 'NONE',  ( 7.758583985612400369, 1432.346375769730230, 153.7649721816169972 ) ) ;
#8072 = CARTESIAN_POINT ( 'NONE',  ( -17.07488731192357179, 1517.151704408390060, 212.8400904445188075 ) ) ;
#8073 = CARTESIAN_POINT ( 'NONE',  ( 4.621897824414999967, 1516.858533673840157, 213.7337256555570093 ) ) ;
#8074 = CARTESIAN_POINT ( 'NONE',  ( -3.738592038228889969, 1428.502628658499816, 200.5405866258459753 ) ) ;
#8075 = CARTESIAN_POINT ( 'NONE',  ( -20.37457945109999713, 1508.379714647830042, 189.3932127643979868 ) ) ;
#8076 = CARTESIAN_POINT ( 'NONE',  ( 5.984345938447710012, 1508.551704613440052, 216.1343701986449730 ) ) ;
#8077 = CARTESIAN_POINT ( 'NONE',  ( -4.027051443935000030, 1516.733363207009916, 211.6130343286269806 ) ) ;
#8078 = AXIS2_PLACEMENT_3D ( 'NONE', #87900, #59943, #35267 ) ;
#8079 = FACE_OUTER_BOUND ( 'NONE', #32249, .T. ) ;
#8080 = CARTESIAN_POINT ( 'NONE',  ( 15.05358515569999867, 1410.831827814130065, 191.5175410460979890 ) ) ;
#8081 = EDGE_CURVE ( 'NONE', #43874, #49524, #20800, .T. ) ;
#8082 = CARTESIAN_POINT ( 'NONE',  ( -12.40790004000990443, 1486.029326377792813, 184.8800518666174355 ) ) ;
#8084 = VERTEX_POINT ( 'NONE', #12100 ) ;
#8083 = CARTESIAN_POINT ( 'NONE',  ( -73.03571372650000626, 1386.716914434789942, 272.3853015438590432 ) ) ;
#8085 = CARTESIAN_POINT ( 'NONE',  ( -59.96058067096299737, 1385.066329289970099, 280.8915114855749948 ) ) ;
#8086 = B_SPLINE_SURFACE_WITH_KNOTS ( 'NONE', 5, 5, ( 
 ( #73398, #30825, #65000, #99118, #82884, #109742, #17300, #102431, #50411 ),
 ( #69427, #101871, #33565, #76144, #33024, #24602, #59916, #68323, #17861 ),
 ( #16746, #41447, #67213, #34685, #8369, #68876, #560, #101309, #7284 ),
 ( #85627, #42538, #18413, #34137, #102977, #95154, #8928, #103541, #25714 ),
 ( #94036, #75612, #51495, #9485, #110289, #77261, #52611, #58796, #93476 ),
 ( #50953, #60464, #92936, #43650, #16207, #43101, #52060, #84536, #7824 ) ),
 .UNSPECIFIED., .F., .F., .F.,
 ( 6, 6 ),
 ( 6, 3, 6 ),
 ( 8.238698527393529147, 19.77813405259999868 ),
 ( -8.198479471770259521E-05, 1.500000000000000000, 3.003699267706470000 ),
 .UNSPECIFIED. ) ;
#8087 = CARTESIAN_POINT ( 'NONE',  ( 22.71362856800000074, 1462.471423918330174, 250.3594882937979946 ) ) ;
#8088 = CARTESIAN_POINT ( 'NONE',  ( -4.371985619807400525, 1370.450432915718920, 208.7651754562319582 ) ) ;
#8089 = CARTESIAN_POINT ( 'NONE',  ( -0.6331911303215019826, 1494.577966063601252, 220.2613815778443893 ) ) ;
#8090 = CARTESIAN_POINT ( 'NONE',  ( -23.68010693890000340, 1447.007135453729916, 214.9276627933680004 ) ) ;
#8091 = DIRECTION ( 'NONE',  ( 1.755985294532464991E-16, -1.000000000000000000, 1.338183447452830017E-16 ) ) ;
#8093 = CARTESIAN_POINT ( 'NONE',  ( -8.580669785819999618, 1384.878224714429962, 218.6695462856689858 ) ) ;
#8092 = CARTESIAN_POINT ( 'NONE',  ( 2.485217193935000068, 1516.534320418310244, 216.8308781079170160 ) ) ;
#8094 = CARTESIAN_POINT ( 'NONE',  ( -9.103435472426211206, 1449.500063809829953, 210.3012238382719943 ) ) ;
#8095 = CARTESIAN_POINT ( 'NONE',  ( 3.068292148129999717E-16, 1443.913060387330006, 150.8032249175980155 ) ) ;
#8096 = EDGE_LOOP ( 'NONE', ( #35184, #91254, #33714, #76928 ) ) ;
#8097 = CARTESIAN_POINT ( 'NONE',  ( -5.006329619514999330, 1516.755758396839838, 202.5714564999769891 ) ) ;
#8098 = CARTESIAN_POINT ( 'NONE',  ( 0.1080094079350000097, 1405.775964805630110, 268.4837719563980158 ) ) ;
#8099 = CARTESIAN_POINT ( 'NONE',  ( -19.53786426058999481, 1512.187213306747481, 236.7197124308268030 ) ) ;
#8100 = AXIS2_PLACEMENT_3D ( 'NONE', #32600, #85190, #109857 ) ;
#8101 = CARTESIAN_POINT ( 'NONE',  ( 12.97071388079999998, 1422.777285505929967, 222.8915848212980109 ) ) ;
#8102 = CARTESIAN_POINT ( 'NONE',  ( 37.79051012442420188, 1445.035584067519949, 137.0421779800970228 ) ) ;
#8103 = DIRECTION ( 'NONE',  ( 0.5877852522921419576, -1.082133391535728970E-16, -0.8090169943751880366 ) ) ;
#8104 = CARTESIAN_POINT ( 'NONE',  ( 25.64308588377748421, 1450.800358157930759, 136.9756054736515694 ) ) ;
#8105 = DIRECTION ( 'NONE',  ( -0.05752486295818479839, -0.9969860201949398704, -0.05205540968523020284 ) ) ;
#8106 = CARTESIAN_POINT ( 'NONE',  ( 32.00873375412530208, 1436.944025776200078, 136.6203492527909873 ) ) ;
#8107 = CARTESIAN_POINT ( 'NONE',  ( 39.81773801718750150, 1446.247923821029872, 136.7608449633160035 ) ) ;
#8108 = CARTESIAN_POINT ( 'NONE',  ( -4.162004322789402799, 1449.631395384008101, 185.0510854563681846 ) ) ;
#8109 = CARTESIAN_POINT ( 'NONE',  ( -109.3562791650000037, 1385.704763654729959, 297.1818586587590403 ) ) ;
#8110 = CARTESIAN_POINT ( 'NONE',  ( 8.313286323959999891, 1507.316772408030147, 183.0869040499979974 ) ) ;
#8111 = CARTESIAN_POINT ( 'NONE',  ( -21.14962954805721296, 1525.231909165033585, 184.4343201733738340 ) ) ;
#8112 = AXIS2_PLACEMENT_3D ( 'NONE', #109161, #92330, #518 ) ;
#8113 = FACE_OUTER_BOUND ( 'NONE', #80434, .T. ) ;
#8114 = ORIENTED_EDGE ( 'NONE', *, *, #43175, .F. ) ;
#8115 = CARTESIAN_POINT ( 'NONE',  ( -113.4000000000000057, 1391.413060387289988, 304.2218459572590064 ) ) ;
#8116 = CARTESIAN_POINT ( 'NONE',  ( -42.47163414147675553, 1428.396231719419120, 269.0629786396675058 ) ) ;
#8117 = FACE_OUTER_BOUND ( 'NONE', #53866, .T. ) ;
#8118 = CARTESIAN_POINT ( 'NONE',  ( 16.80488241574720121, 1503.399646969610103, 188.2277903123039948 ) ) ;
#8119 = CARTESIAN_POINT ( 'NONE',  ( 13.78830459049999924, 1507.504417904530101, 224.4506042099979766 ) ) ;
#8120 = CARTESIAN_POINT ( 'NONE',  ( 11.42883607589999961, 1502.384062944689958, 210.3441498915189811 ) ) ;
#8121 = CARTESIAN_POINT ( 'NONE',  ( -12.67125179517506695, 1445.026230862206148, 185.8434676868600945 ) ) ;
#8122 = B_SPLINE_SURFACE_WITH_KNOTS ( 'NONE', 5, 5, ( 
 ( #3378, #79521, #1722, #37505, #35298, #71710, #96872, #96312, #61093, #11220, #2826, #12289 ),
 ( #62186, #10661, #19590, #44829, #35862, #105828, #87931, #29106, #103605, #70046, #45383, #95758 ),
 ( #19023, #36944, #78982, #54335, #2286, #62755, #71142, #105262, #90653, #47027, #7622, #67006 ),
 ( #55973, #109546, #30751, #29648, #64932, #101661, #33365, #80615, #32819, #24950, #3929, #21216 ),
 ( #13937, #64383, #50207, #99045, #73878, #106903, #48125, #22323, #56525, #84332, #82263, #101116 ),
 ( #97947, #90097, #55424, #24413, #4999, #59159, #5563, #41780, #92729, #30190, #58597, #16004 ),
 ( #75935, #98504, #110090, #67558, #38058, #93279, #46483, #72236, #39144, #21772, #106362, #63835 ),
 ( #89557, #12846, #81153, #13380, #4467, #73319, #38596, #47568, #72775, #81692, #107456, #39714 ),
 ( #33922, #69776, #36150, #8716, #52412, #51852, #35030, #68661, #68118, #76485, #102230, #77053 ),
 ( #60252, #18216, #904, #69209, #9831, #104446, #70334, #27738, #17651, #43450, #35584, #93812 ),
 ( #103318, #59700, #110637, #61376, #25509, #17091, #42895, #103894, #61929, #16542, #34486, #51283 ),
 ( #360, #10379, #27193, #84866, #52961, #95495, #44552, #85989, #102761, #50733, #87094, #44000 ) ),
 .UNSPECIFIED., .F., .F., .F.,
 ( 6, 3, 3, 6 ),
 ( 6, 3, 3, 6 ),
 ( 5.901444351240000330, 6.549836289219999941, 7.702803945130000329, 8.339062479686310425 ),
 ( -4.054862768222389734E-05, 0.3888358943340000096, 1.166507657809999987, 1.690645290116310040 ),
 .UNSPECIFIED. ) ;
#8123 = CARTESIAN_POINT ( 'NONE',  ( 7.254058142540000809, 1424.158195616359990, 212.5403795493589882 ) ) ;
#8124 = CARTESIAN_POINT ( 'NONE',  ( -4.329448802513499395, 1515.064791340959800, 211.4517443289939820 ) ) ;
#8125 = CARTESIAN_POINT ( 'NONE',  ( -10.76135780955835131, 1418.364098519981781, 229.5605810891095473 ) ) ;
#8126 = CARTESIAN_POINT ( 'NONE',  ( -21.00754753991050450, 1450.948176978987703, 144.4512443326310347 ) ) ;
#8127 = CARTESIAN_POINT ( 'NONE',  ( -6.103113815119999508, 1482.731685980090106, 200.3426744219489990 ) ) ;
#8128 = CARTESIAN_POINT ( 'NONE',  ( 24.46423381230000160, 1435.351789881140121, 136.2073200738979892 ) ) ;
#8129 = CARTESIAN_POINT ( 'NONE',  ( -12.75960595697487676, 1442.830007631229819, 169.4538581461608828 ) ) ;
#8130 = ORIENTED_EDGE ( 'NONE', *, *, #42653, .T. ) ;
#8131 = CARTESIAN_POINT ( 'NONE',  ( 0.5835301444260361237, 1415.089118586289942, 191.9293356823729937 ) ) ;
#8132 = CARTESIAN_POINT ( 'NONE',  ( -18.31941652021488665, 1519.551704408389924, 214.4156261991469421 ) ) ;
#8133 = ORIENTED_EDGE ( 'NONE', *, *, #40616, .T. ) ;
#8134 = VERTEX_POINT ( 'NONE', #105629 ) ;
#8135 = CARTESIAN_POINT ( 'NONE',  ( -1.017068913289999932, 1494.761373610690043, 217.4896306674490063 ) ) ;
#8136 = CARTESIAN_POINT ( 'NONE',  ( -30.31940284292427634, 1518.913060387330006, 195.7503880523418616 ) ) ;
#8138 = CARTESIAN_POINT ( 'NONE',  ( -15.47578423070000042, 1455.753639292730213, 211.9081975729679925 ) ) ;
#8137 = CARTESIAN_POINT ( 'NONE',  ( 1.875671966999999940, 1456.514202392889956, 219.5762891471990201 ) ) ;
#8139 = CARTESIAN_POINT ( 'NONE',  ( -5.213813250899999474, 1445.091437330390136, 217.1001509711090023 ) ) ;
#8140 = CARTESIAN_POINT ( 'NONE',  ( 4.187230966989369918, 1424.086676286679904, 184.3159420495250060 ) ) ;
#8141 = CARTESIAN_POINT ( 'NONE',  ( -12.29651836606130111, 1378.320268164070058, 209.9934040429740207 ) ) ;
#8142 = CARTESIAN_POINT ( 'NONE',  ( -2.495937523808232861, 1421.225737875227424, 184.7764519901441531 ) ) ;
#8143 = CARTESIAN_POINT ( 'NONE',  ( 7.103763521679999471, 1424.020716665080045, 213.1883901192190081 ) ) ;
#8144 = CARTESIAN_POINT ( 'NONE',  ( -24.50758153960000030, 1438.442324728890071, 210.7299082220580146 ) ) ;
#8145 = CARTESIAN_POINT ( 'NONE',  ( -4.017758734575580526, 1453.901170738600058, 199.4485904977269684 ) ) ;
#8146 = CARTESIAN_POINT ( 'NONE',  ( 1.702416261868870073, 1493.957958506549858, 220.1113518634800243 ) ) ;
#8147 = CARTESIAN_POINT ( 'NONE',  ( 8.520620816894430405, 1363.877202865954587, 207.6218459616988241 ) ) ;
#8148 = CARTESIAN_POINT ( 'NONE',  ( -17.49344942435742567, 1509.643870198284048, 184.6887002396688899 ) ) ;
#8150 = EDGE_LOOP ( 'NONE', ( #18826, #78483, #60221, #9433 ) ) ;
#8149 = CARTESIAN_POINT ( 'NONE',  ( -2.798454660896469878E-09, 1414.971556725290156, 244.5047741046470264 ) ) ;
#8151 = VERTEX_POINT ( 'NONE', #45179 ) ;
#8152 = CARTESIAN_POINT ( 'NONE',  ( -11.80049257314770017, 1428.258320413980073, 148.2065752701799966 ) ) ;
#8153 = AXIS2_PLACEMENT_3D ( 'NONE', #37239, #72503, #71438 ) ;
#8154 = CARTESIAN_POINT ( 'NONE',  ( -19.87223104929999806, 1484.291808912129909, 191.2808552885979907 ) ) ;
#8155 = CARTESIAN_POINT ( 'NONE',  ( -1.412138242519999975, 1471.571752635429903, 269.6151167561980060 ) ) ;
#8156 = CARTESIAN_POINT ( 'NONE',  ( 11.95405219206525516, 1433.552936807464221, 147.6143242043138173 ) ) ;
#8157 = CARTESIAN_POINT ( 'NONE',  ( -125.0414468819037381, 1320.102705746890024, 297.8620945402922757 ) ) ;
#8158 = CARTESIAN_POINT ( 'NONE',  ( 17.73803434250000066, 1408.913060387329779, 209.1218459616979999 ) ) ;
#8159 = CARTESIAN_POINT ( 'NONE',  ( -8.395462808959999634, 1384.396046010230066, 199.8129347473389998 ) ) ;
#8160 = CARTESIAN_POINT ( 'NONE',  ( -15.28420222229999936, 1497.713060387329961, 193.8376437396979952 ) ) ;
#8161 = CARTESIAN_POINT ( 'NONE',  ( 5.215187551926136145, 1368.779556716638126, 210.6218459616991936 ) ) ;
#8162 = CARTESIAN_POINT ( 'NONE',  ( -9.105453163054910704, 1449.059532022529993, 210.1349288613230044 ) ) ;
#8163 = CARTESIAN_POINT ( 'NONE',  ( -20.58955907263800000, 1409.512823798320142, 267.0592759364189988 ) ) ;
#8164 = DIRECTION ( 'NONE',  ( 1.755985294532469921E-16, -1.000000000000000000, 1.338183447452831989E-16 ) ) ;
#8165 = ORIENTED_EDGE ( 'NONE', *, *, #15362, .F. ) ;
#8166 = CYLINDRICAL_SURFACE ( 'NONE', #53805, 1.638701816490922836 ) ;
#8167 = CARTESIAN_POINT ( 'NONE',  ( 14.26923756360000084, 1444.927653052269989, 189.5513799252980220 ) ) ;
#8168 = VERTEX_POINT ( 'NONE', #79321 ) ;
#8169 = ORIENTED_EDGE ( 'NONE', *, *, #76712, .F. ) ;
#8170 = CARTESIAN_POINT ( 'NONE',  ( 4.647253597870006026, 1422.128807924814055, 184.1025069751984802 ) ) ;
#8171 = CARTESIAN_POINT ( 'NONE',  ( 6.960583431767130236, 1424.680772738690166, 193.9777372977509913 ) ) ;
#8172 = CARTESIAN_POINT ( 'NONE',  ( 7.721907888235000073, 1517.026025493960105, 214.1263215447669950 ) ) ;
#8173 = CARTESIAN_POINT ( 'NONE',  ( -15.59759639429999822, 1470.467432881730019, 188.1491572198980009 ) ) ;
#8174 = CARTESIAN_POINT ( 'NONE',  ( 0.000000000000000000, 1420.119835273649869, 209.1218459616989946 ) ) ;
#8175 = VERTEX_POINT ( 'NONE', #80421 ) ;
#8176 = CARTESIAN_POINT ( 'NONE',  ( 32.78250617288038171, 1512.187213306747481, 199.9357095655690841 ) ) ;
#8177 = CIRCLE ( 'NONE', #74394, 30.10786454236638576 ) ;
#8178 =( BOUNDED_SURFACE ( )  B_SPLINE_SURFACE ( 3, 2, ( 
 ( #1651, #11682, #27378 ),
 ( #105760, #35786, #96244 ),
 ( #104083, #11149, #62118 ),
 ( #95692, #95141, #36326 ),
 ( #69970, #61559, #12223 ),
 ( #46417, #18958, #86736 ),
 ( #97335, #62681, #54267 ),
 ( #104638, #53724, #63231 ),
 ( #53154, #96803, #36880 ),
 ( #105198, #87292, #19519 ) ),
 .UNSPECIFIED., .F., .F., .F. ) 
 B_SPLINE_SURFACE_WITH_KNOTS ( ( 4, 2, 2, 2, 4 ),
 ( 3, 3 ),
 ( 1.570796326794896558, 1.963495408493620697, 2.356194490192344837, 2.748893571891068976, 3.141592653589793116 ),
 ( 0.000000000000000000, 1.000000000000000000 ),
 .UNSPECIFIED. ) 
 GEOMETRIC_REPRESENTATION_ITEM ( )  RATIONAL_B_SPLINE_SURFACE ( (
 ( 1.000000000000000000, 0.7071067811865878738, 1.000000000000000000),
 ( 1.000000000000000000, 0.7166207884821444996, 1.000000000000000000),
 ( 1.000000000000000000, 0.7259222650907969365, 1.000000000000000000),
 ( 1.000000000000000000, 0.7428408967929446272, 1.000000000000000000),
 ( 1.000000000000000000, 0.7504512394529284647, 1.000000000000000000),
 ( 1.000000000000000000, 0.7630177051945691291, 1.000000000000000000),
 ( 1.000000000000000000, 0.7679730451975484984, 1.000000000000000000),
 ( 1.000000000000000000, 0.7746454561794965388, 1.000000000000000000),
 ( 1.000000000000000000, 0.7763684247036931607, 1.000000000000000000),
 ( 1.000000000000000000, 0.7763623250684325017, 1.000000000000000000) ) ) 
 REPRESENTATION_ITEM ( '' )  SURFACE ( )  );
#8179 = CARTESIAN_POINT ( 'NONE',  ( -1.130002532395000037, 1516.621991115350056, 202.1860446705670142 ) ) ;
#8180 = CARTESIAN_POINT ( 'NONE',  ( -27.28719766109999867, 1508.596937417230038, 204.2391279096780181 ) ) ;
#8181 = FACE_OUTER_BOUND ( 'NONE', #105706, .T. ) ;
#8183 = CIRCLE ( 'NONE', #13538, 2.000000000000001776 ) ;
#8182 = CARTESIAN_POINT ( 'NONE',  ( -28.05711651015590036, 1384.551594447279967, 204.6011676599970031 ) ) ;
#8184 = CARTESIAN_POINT ( 'NONE',  ( -6.448255178740000204, 1408.606950374030021, 197.2260920491980016 ) ) ;
#8185 = CARTESIAN_POINT ( 'NONE',  ( -3.347801439296141268, 1512.187213306747481, 176.1543725841967500 ) ) ;
#8187 = ORIENTED_EDGE ( 'NONE', *, *, #49516, .T. ) ;
#8186 = CARTESIAN_POINT ( 'NONE',  ( -4.646147438016499542, 1378.399971910029990, 214.5514622210689879 ) ) ;
#8188 = CARTESIAN_POINT ( 'NONE',  ( 12.26470395605226571, 1426.140792135694483, 200.3478462435150504 ) ) ;
#8189 = CARTESIAN_POINT ( 'NONE',  ( 27.89257148229999927, 1508.131979115830063, 211.4058184921079828 ) ) ;
#8190 = CARTESIAN_POINT ( 'NONE',  ( -64.48963914116505691, 1379.738450935989476, 274.0683424708428788 ) ) ;
#8191 = CARTESIAN_POINT ( 'NONE',  ( -11.60387536552270049, 1481.105535834539978, 211.4044418330699955 ) ) ;
#8192 = CARTESIAN_POINT ( 'NONE',  ( -13.12992410348680039, 1436.052586817060046, 150.6851515388850089 ) ) ;
#8193 = CARTESIAN_POINT ( 'NONE',  ( -7.708745685915000756, 1516.523379810429788, 210.8299382363969983 ) ) ;
#8194 = CARTESIAN_POINT ( 'NONE',  ( -68.53407989799998745, 1379.748277114789971, 279.6522222015589705 ) ) ;
#8195 = CARTESIAN_POINT ( 'NONE',  ( -14.45007549780000033, 1415.597377782830108, 226.9959651844980044 ) ) ;
#8196 = CARTESIAN_POINT ( 'NONE',  ( 7.227136201815060446, 1482.982132909030042, 211.7482587894230051 ) ) ;
#8197 = CARTESIAN_POINT ( 'NONE',  ( -1.133653179125000188, 1516.978425811520083, 208.3843950493249793 ) ) ;
#8198 = VERTEX_POINT ( 'NONE', #96672 ) ;
#8199 = CARTESIAN_POINT ( 'NONE',  ( -7.965865502150356825, 1384.923562076983444, 199.4891873544885925 ) ) ;
#8200 = CARTESIAN_POINT ( 'NONE',  ( 5.429027314403359838, 1440.820888945739853, 154.8047238334139877 ) ) ;
#8201 = CARTESIAN_POINT ( 'NONE',  ( -20.52956604201131086, 1455.629392789516260, 224.1961909860604862 ) ) ;
#8202 = ORIENTED_EDGE ( 'NONE', *, *, #51511, .T. ) ;
#8203 = CARTESIAN_POINT ( 'NONE',  ( -2.596261494520238688, 1525.907212628473644, 240.7735774411713123 ) ) ;
#8204 = CARTESIAN_POINT ( 'NONE',  ( -12.02051106306990036, 1491.153688555679992, 206.6632162730240054 ) ) ;
#8205 = CARTESIAN_POINT ( 'NONE',  ( 12.82193894433369863, 1434.943467189540115, 150.1840956961830216 ) ) ;
#8206 = B_SPLINE_CURVE_WITH_KNOTS ( 'NONE', 5,
 ( #95820, #63895, #1791, #28620, #2894, #19088, #37012, #35928, #2349, #44898, #87431, #70112 ),
 .UNSPECIFIED., .F., .F.,
 ( 6, 3, 3, 6 ),
 ( 5.812629425579999953, 6.561021380799999747, 7.569428689259999565, 8.073601757938709156 ),
 .UNSPECIFIED. ) ;
#8207 = CARTESIAN_POINT ( 'NONE',  ( 2.706310507869800208, 1459.298787099630090, 233.8407132922810092 ) ) ;
#8208 = CARTESIAN_POINT ( 'NONE',  ( -17.06814468720000377, 1418.145817546499984, 204.3351068018390038 ) ) ;
#8209 = CARTESIAN_POINT ( 'NONE',  ( -11.43336139241818827, 1425.764428307910975, 138.9802830098579420 ) ) ;
#8210 = CARTESIAN_POINT ( 'NONE',  ( 10.20885384580000022, 1489.898602996290037, 203.1012352018590263 ) ) ;
#8211 = CARTESIAN_POINT ( 'NONE',  ( 0.000000000000000000, 1522.051704408389924, 209.1218459616979999 ) ) ;
#8212 = CARTESIAN_POINT ( 'NONE',  ( -15.09681984919999920, 1409.610690840030202, 226.1751760239980058 ) ) ;
#8213 = EDGE_CURVE ( 'NONE', #42280, #39961, #49451, .T. ) ;
#8215 = CARTESIAN_POINT ( 'NONE',  ( -1.842963333050206209, 1515.193466796482426, 204.7957666306796796 ) ) ;
#8214 = CARTESIAN_POINT ( 'NONE',  ( -6.937965698444999774, 1516.732530461250008, 214.1275461716370216 ) ) ;
#8216 = CARTESIAN_POINT ( 'NONE',  ( 20.99960916279999878, 1509.542875961329855, 188.7432993302979867 ) ) ;
#8217 = CARTESIAN_POINT ( 'NONE',  ( -4.034908597844999889, 1517.068717944079935, 216.4577469658269990 ) ) ;
#8218 = ORIENTED_EDGE ( 'NONE', *, *, #73439, .F. ) ;
#8219 = CARTESIAN_POINT ( 'NONE',  ( 7.720548113794640344, 1516.974097803170025, 209.2608539945439929 ) ) ;
#8220 = CARTESIAN_POINT ( 'NONE',  ( -16.83270678099999884, 1420.441345669400107, 203.3485545991589731 ) ) ;
#8221 = ORIENTED_EDGE ( 'NONE', *, *, #30760, .T. ) ;
#8222 = CARTESIAN_POINT ( 'NONE',  ( -18.39846574424100112, 1508.551704408389924, 210.4158962701780240 ) ) ;
#8223 = AXIS2_PLACEMENT_3D ( 'NONE', #105293, #10693, #17395 ) ;
#8224 = CARTESIAN_POINT ( 'NONE',  ( 2.214868538355918570, 1525.730671215507982, 176.6953666955783433 ) ) ;
#8225 = LINE ( 'NONE', #6591, #89729 ) ;
#8226 = CARTESIAN_POINT ( 'NONE',  ( -11.40193393769130026, 1470.847406381370092, 208.7670122399519812 ) ) ;
#8227 = CARTESIAN_POINT ( 'NONE',  ( -7.280829216295649609, 1508.396933602414720, 219.6675365539373388 ) ) ;
#8228 = CARTESIAN_POINT ( 'NONE',  ( 17.36968966387737723, 1422.689908039817965, 226.5801647642350076 ) ) ;
#8229 = DIRECTION ( 'NONE',  ( -6.123233995736769734E-17, -1.000000000000000000, -1.124819836996399911E-32 ) ) ;
#8230 = CARTESIAN_POINT ( 'NONE',  ( -8.340003444863377524, 1458.803746027120042, 213.9233038274046237 ) ) ;
#8231 = FACE_OUTER_BOUND ( 'NONE', #81918, .T. ) ;
#8232 = CARTESIAN_POINT ( 'NONE',  ( 41.06518263065470364, 1440.913060356710048, 260.7453200965900351 ) ) ;
#8234 = CARTESIAN_POINT ( 'NONE',  ( 8.313287170068500487, 1507.316777277299934, 183.0869016502879845 ) ) ;
#8233 = CARTESIAN_POINT ( 'NONE',  ( -11.38244087966499940, 1470.612899495130023, 209.7950405083470002 ) ) ;
#8235 = CARTESIAN_POINT ( 'NONE',  ( 10.95929498157123483, 1431.610953951363172, 151.7698544105677456 ) ) ;
#8236 = ORIENTED_EDGE ( 'NONE', *, *, #13923, .T. ) ;
#8237 = EDGE_LOOP ( 'NONE', ( #98778, #49873, #65399 ) ) ;
#8238 = CARTESIAN_POINT ( 'NONE',  ( -32.02808312589908013, 1512.187213306747481, 219.9649204700466782 ) ) ;
#8239 = CARTESIAN_POINT ( 'NONE',  ( -8.972797484658892486, 1506.569407359554816, 229.3146644943394676 ) ) ;
#8240 = CARTESIAN_POINT ( 'NONE',  ( -1.682117298743253553, 1526.345556099435726, 178.4797647222532930 ) ) ;
#8241 = CARTESIAN_POINT ( 'NONE',  ( 3.931910744533549718, 1448.296755838050103, 184.2998928686550073 ) ) ;
#8242 = CARTESIAN_POINT ( 'NONE',  ( -3.059934833509219576, 1425.992208071485948, 185.5324912608258785 ) ) ;
#8243 = LINE ( 'NONE', #74390, #53842 ) ;
#8245 = TOROIDAL_SURFACE ( 'NONE', #74469, 8.500000000000000000, 1.500000000000000000 ) ;
#8244 = CARTESIAN_POINT ( 'NONE',  ( -4.636368232763167008, 1378.015684711496988, 203.9444611951153377 ) ) ;
#8246 = CARTESIAN_POINT ( 'NONE',  ( 19.03958390842529980, 1453.804148033969796, 200.7927771423659919 ) ) ;
#8247 = CARTESIAN_POINT ( 'NONE',  ( -60.79172661048330184, 1383.795642611730045, 281.9543892178000419 ) ) ;
#8248 = ADVANCED_FACE ( 'NONE', ( #4269 ), #40913, .T. ) ;
#8249 = ADVANCED_FACE ( 'NONE', ( #54138 ), #28355, .F. ) ;
#8250 = CARTESIAN_POINT ( 'NONE',  ( 10.34308214130000003, 1452.551872000029789, 150.8401898677979887 ) ) ;
#8251 = CARTESIAN_POINT ( 'NONE',  ( 3.500000000000000000, 1424.163060387329779, 172.2701767054979882 ) ) ;
#8252 = CARTESIAN_POINT ( 'NONE',  ( 12.31939201916519977, 1492.268456928650039, 209.8911822630940094 ) ) ;
#8254 = ORIENTED_EDGE ( 'NONE', *, *, #46258, .T. ) ;
#8253 = CARTESIAN_POINT ( 'NONE',  ( 0.6519600591489990160, 1456.622952327490111, 219.3373220789989944 ) ) ;
#8255 = CARTESIAN_POINT ( 'NONE',  ( 32.39315898239710378, 1526.178928173328131, 216.9314351822641243 ) ) ;
#8256 = CARTESIAN_POINT ( 'NONE',  ( -44.05982002580000056, 1379.037918066350130, 230.4561377212590116 ) ) ;
#8257 = EDGE_CURVE ( 'NONE', #21200, #75280, #7356, .T. ) ;
#8258 = CARTESIAN_POINT ( 'NONE',  ( -21.13431252044160047, 1409.651086843229905, 211.8287216663260040 ) ) ;
#8259 = ORIENTED_EDGE ( 'NONE', *, *, #22699, .T. ) ;
#8260 = VERTEX_POINT ( 'NONE', #91572 ) ;
#8261 = EDGE_CURVE ( 'NONE', #105125, #43735, #18050, .T. ) ;
#8262 = CARTESIAN_POINT ( 'NONE',  ( 20.59988588776639773, 1509.677360688819817, 230.5839048903779940 ) ) ;
#8263 = DIRECTION ( 'NONE',  ( 0.000000000000000000, -1.000000000000000000, 6.123233995736769734E-17 ) ) ;
#8264 = CARTESIAN_POINT ( 'NONE',  ( 37.37547333107730196, 1438.147115316229929, 136.5735404978140082 ) ) ;
#8266 = CARTESIAN_POINT ( 'NONE',  ( -2.372478608332516892, 1522.862737210649811, 243.3440112565233449 ) ) ;
#8265 = DIRECTION ( 'NONE',  ( -0.000000000000000000, -1.000000000000000000, -0.000000000000000000 ) ) ;
#8267 = CARTESIAN_POINT ( 'NONE',  ( 11.55681713461770066, 1480.209600850990000, 211.4560790503059877 ) ) ;
#8268 = CARTESIAN_POINT ( 'NONE',  ( -108.0221525909999940, 1382.696190293120026, 297.7913543730589936 ) ) ;
#8269 = CARTESIAN_POINT ( 'NONE',  ( -21.84020450222019960, 1523.382868172864164, 234.9798068779743687 ) ) ;
#8270 = CARTESIAN_POINT ( 'NONE',  ( -32.28466283162165240, 1522.382868172863937, 199.0684425896249081 ) ) ;
#8271 = CARTESIAN_POINT ( 'NONE',  ( -10.52263122030180043, 1508.551704408389924, 218.0322449975469681 ) ) ;
#8272 = CARTESIAN_POINT ( 'NONE',  ( 4.526435456679999803, 1410.447042416829845, 186.2069608473979940 ) ) ;
#8273 = CARTESIAN_POINT ( 'NONE',  ( 4.853127557110000545, 1425.657129708029970, 185.6214293445979990 ) ) ;
#8274 = FACE_OUTER_BOUND ( 'NONE', #53660, .T. ) ;
#8275 = CARTESIAN_POINT ( 'NONE',  ( -2.499999942568179812, 1440.188496425770154, 170.5318011134379788 ) ) ;
#8276 = B_SPLINE_CURVE_WITH_KNOTS ( 'NONE', 5,
 ( #54352, #3946, #87947, #2304, #18492, #89017, #45937, #11768, #12309, #80075, #63308, #70607 ),
 .UNSPECIFIED., .F., .F.,
 ( 6, 3, 3, 6 ),
 ( 0.000000000000000000, 0.2928450906018923439, 0.7539279110859780086, 1.000000000000000000 ),
 .UNSPECIFIED. ) ;
#8277 = B_SPLINE_CURVE_WITH_KNOTS ( 'NONE', 3,
 ( #81039, #89445, #74321, #106245 ),
 .UNSPECIFIED., .F., .F.,
 ( 4, 4 ),
 ( 0.000000000000000000, 1.000000000000000000 ),
 .UNSPECIFIED. ) ;
#8278 = CARTESIAN_POINT ( 'NONE',  ( -22.03365245649999693, 1451.714665305230028, 143.0874833212980093 ) ) ;
#8279 = CARTESIAN_POINT ( 'NONE',  ( 1.790406358549999855, 1464.873382007230020, 236.3711796330979666 ) ) ;
#8280 = ORIENTED_EDGE ( 'NONE', *, *, #46216, .T. ) ;
#8281 = CARTESIAN_POINT ( 'NONE',  ( -3.130661101029999838, 1471.246791520290117, 187.3882170434989973 ) ) ;
#8283 = EDGE_CURVE ( 'NONE', #54897, #71672, #24320, .T. ) ;
#8282 = DIRECTION ( 'NONE',  ( 0.000000000000000000, -1.000000000000000000, 6.123233995736769734E-17 ) ) ;
#8284 = CARTESIAN_POINT ( 'NONE',  ( -12.26979726809049964, 1416.828039266780024, 194.6643405733680083 ) ) ;
#8285 = CARTESIAN_POINT ( 'NONE',  ( -2.499999999859999988, 1439.640830480200293, 184.0873493999980042 ) ) ;
#8286 = CARTESIAN_POINT ( 'NONE',  ( 17.02674992690000266, 1488.215563971529946, 189.0842524208980251 ) ) ;
#8287 = CARTESIAN_POINT ( 'NONE',  ( -3.721063415729999695E-09, 1475.837061091930082, 266.9611530633980010 ) ) ;
#8288 = CARTESIAN_POINT ( 'NONE',  ( 20.04791373445998204, 1436.429743172953977, 145.3885934355014342 ) ) ;
#8289 = CARTESIAN_POINT ( 'NONE',  ( -0.5624690339869999889, 1416.828040475229955, 227.7677324846980014 ) ) ;
#8290 = CARTESIAN_POINT ( 'NONE',  ( -8.733798672629999871, 1419.056601762730224, 233.0476203166980156 ) ) ;
#8291 = CARTESIAN_POINT ( 'NONE',  ( -0.9759527017809989102, 1477.437381222690192, 198.7358441459990104 ) ) ;
#8292 = CARTESIAN_POINT ( 'NONE',  ( -106.9262462220000032, 1389.757047639990105, 308.9264214093590226 ) ) ;
#8293 = EDGE_CURVE ( 'NONE', #94676, #44473, #27383, .T. ) ;
#8294 = CARTESIAN_POINT ( 'NONE',  ( -7.663889450468710507, 1510.954290761809943, 214.5915452069070000 ) ) ;
#8295 = CARTESIAN_POINT ( 'NONE',  ( 3.618222164275962882, 1359.470288639974342, 210.6218459617030021 ) ) ;
#8296 = CARTESIAN_POINT ( 'NONE',  ( -45.61713505807430380, 1439.852003152469933, 268.9753901037370269 ) ) ;
#8297 = CARTESIAN_POINT ( 'NONE',  ( 1.833097954248699812, 1429.276494549819972, 217.2158816865839981 ) ) ;
#8298 = CARTESIAN_POINT ( 'NONE',  ( -2.048534905309999932, 1444.110401950890036, 199.2775038477390126 ) ) ;
#8299 = EDGE_CURVE ( 'NONE', #100973, #100009, #29763, .T. ) ;
#8300 = ORIENTED_EDGE ( 'NONE', *, *, #20547, .T. ) ;
#8301 = CARTESIAN_POINT ( 'NONE',  ( 0.7402208603880020554, 1516.992029636990083, 208.3685455796920110 ) ) ;
#8302 = DIRECTION ( 'NONE',  ( 0.9858563016923833633, 0.000000000000000000, 0.1675928173085483863 ) ) ;
#8303 = CARTESIAN_POINT ( 'NONE',  ( -9.699660872752350116, 1472.030908259890111, 212.1562907213800031 ) ) ;
#8304 = CARTESIAN_POINT ( 'NONE',  ( 7.520380367349810413, 1425.880113479670172, 212.2583774670760022 ) ) ;
#8305 = ADVANCED_FACE ( 'NONE', ( #110023 ), #55777, .T. ) ;
#8306 = CARTESIAN_POINT ( 'NONE',  ( -26.01456120673969963, 1451.843691735240100, 135.7887858332240114 ) ) ;
#8307 = ORIENTED_EDGE ( 'NONE', *, *, #96093, .T. ) ;
#8308 = CARTESIAN_POINT ( 'NONE',  ( 26.01030838259999811, 1431.980453045119930, 231.9333039360980138 ) ) ;
#8310 = CARTESIAN_POINT ( 'NONE',  ( -15.29008555799489955, 1513.004579589639889, 223.0186118662149966 ) ) ;
#8309 = CARTESIAN_POINT ( 'NONE',  ( -2.599446155150084259, 1525.231909165033812, 176.7177777100700951 ) ) ;
#8311 = B_SPLINE_CURVE_WITH_KNOTS ( 'NONE', 5,
 ( #17192, #58151, #16645, #24508, #32919, #110187 ),
 .UNSPECIFIED., .F., .F.,
 ( 6, 6 ),
 ( 265.9669962020000185, 275.7680412249999904 ),
 .UNSPECIFIED. ) ;
#8312 = FACE_OUTER_BOUND ( 'NONE', #106646, .T. ) ;
#8313 = CARTESIAN_POINT ( 'NONE',  ( -19.36515920207871488, 1456.378690097197477, 228.5344338426573358 ) ) ;
#8314 = CARTESIAN_POINT ( 'NONE',  ( 3.892080479029999651, 1421.098424262469962, 205.7437050486190060 ) ) ;
#8315 = CARTESIAN_POINT ( 'NONE',  ( -17.99954540876850118, 1410.904693920620048, 195.2564682659330231 ) ) ;
#8316 = CARTESIAN_POINT ( 'NONE',  ( -25.37229503420000043, 1438.463288316339913, 138.1377907575980259 ) ) ;
#8317 = EDGE_LOOP ( 'NONE', ( #108206, #74502, #95926, #71184 ) ) ;
#8318 = CARTESIAN_POINT ( 'NONE',  ( -1.236138560472719972, 1408.568929830810248, 270.4289767352809690 ) ) ;
#8319 = CARTESIAN_POINT ( 'NONE',  ( 7.805697987095799206, 1418.513168923040212, 231.5901604170679775 ) ) ;
#8320 = CARTESIAN_POINT ( 'NONE',  ( 8.197348291215568850, 1436.381065636019912, 206.4883948098359951 ) ) ;
#8321 = VERTEX_POINT ( 'NONE', #10749 ) ;
#8322 = EDGE_LOOP ( 'NONE', ( #83112, #6235, #19977, #14053 ) ) ;
#8323 = CARTESIAN_POINT ( 'NONE',  ( -22.72614924474259723, 1409.716713977369864, 209.6046740144809917 ) ) ;
#8324 = CARTESIAN_POINT ( 'NONE',  ( -0.8389850993970380255, 1409.109437246339894, 185.8522822715279972 ) ) ;
#8325 = DIRECTION ( 'NONE',  ( 0.9942586961433741433, 0.000000000000000000, -0.1070030146457454784 ) ) ;
#8326 = CARTESIAN_POINT ( 'NONE',  ( -6.629188914260000232, 1428.588785140030041, 91.31218443469779800 ) ) ;
#8327 = CARTESIAN_POINT ( 'NONE',  ( -20.54885787271648567, 1436.446738464058399, 144.8383282339893299 ) ) ;
#8328 = CARTESIAN_POINT ( 'NONE',  ( 3.117403407738490007, 1508.880976867409800, 213.6144879028050241 ) ) ;
#8329 = CARTESIAN_POINT ( 'NONE',  ( 41.27561781798189600, 1456.929397665800025, 267.7644989067840129 ) ) ;
#8330 = CARTESIAN_POINT ( 'NONE',  ( -4.492644309999670682, 1508.880967335730247, 205.3188433609270191 ) ) ;
#8331 = CARTESIAN_POINT ( 'NONE',  ( -16.55054877997067209, 1421.400737720431835, 226.9740673232442134 ) ) ;
#8332 = CARTESIAN_POINT ( 'NONE',  ( 0.7355686427760019797, 1517.012231669750008, 205.8548062402470009 ) ) ;
#8333 = ORIENTED_EDGE ( 'NONE', *, *, #82212, .T. ) ;
#8334 = CARTESIAN_POINT ( 'NONE',  ( 18.33221555414402459, 1459.112549484824740, 227.7897102868277557 ) ) ;
#8335 = CARTESIAN_POINT ( 'NONE',  ( 0.6746223769683330485, 1445.135766336949928, 199.0746255971319840 ) ) ;
#8336 = CARTESIAN_POINT ( 'NONE',  ( 23.17738928069999815, 1409.983622293829967, 208.1777596987790275 ) ) ;
#8337 = ORIENTED_EDGE ( 'NONE', *, *, #99685, .T. ) ;
#8338 = CARTESIAN_POINT ( 'NONE',  ( -11.16939613673820020, 1480.956201967079778, 211.2843442006090129 ) ) ;
#8339 = CARTESIAN_POINT ( 'NONE',  ( 5.401943384969776218, 1434.552886126495196, 202.5243240070273032 ) ) ;
#8340 = CARTESIAN_POINT ( 'NONE',  ( 2.487935123032369855, 1509.038615930399828, 204.6345961886270004 ) ) ;
#8341 = CARTESIAN_POINT ( 'NONE',  ( -3.078458294640000315, 1387.009338736269910, 218.3238323482389944 ) ) ;
#8342 = CARTESIAN_POINT ( 'NONE',  ( 7.417144106380000323, 1422.547346766210012, 195.6244150781990072 ) ) ;
#8343 = CARTESIAN_POINT ( 'NONE',  ( 20.79403292647610257, 1409.639204018000100, 215.4572002851739967 ) ) ;
#8344 = CARTESIAN_POINT ( 'NONE',  ( -3.801318561300000010, 1497.265417599789998, 198.5158051468989981 ) ) ;
#8345 = CARTESIAN_POINT ( 'NONE',  ( 2.164129514809030042, 1408.988633455270246, 186.9734320209399812 ) ) ;
#8347 = DIRECTION ( 'NONE',  ( -0.9445946449598763284, 0.000000000000000000, 0.3282391760791590340 ) ) ;
#8346 = CARTESIAN_POINT ( 'NONE',  ( 2.223260522209999923, 1417.626103841329723, 234.7006573303980019 ) ) ;
#8348 = CARTESIAN_POINT ( 'NONE',  ( 1.039304647762639977, 1450.826060414650101, 181.7808938767670099 ) ) ;
#8349 = EDGE_CURVE ( 'NONE', #91497, #23258, #62011, .T. ) ;
#8350 = CARTESIAN_POINT ( 'NONE',  ( -11.90934194029999915, 1377.744960516140054, 212.2952750262290067 ) ) ;
#8351 = EDGE_CURVE ( 'NONE', #46444, #104691, #110244, .T. ) ;
#8352 = DIRECTION ( 'NONE',  ( 0.9455185755993178454, 0.000000000000000000, -0.3255681544571537578 ) ) ;
#8353 = ORIENTED_EDGE ( 'NONE', *, *, #101981, .T. ) ;
#8354 = CARTESIAN_POINT ( 'NONE',  ( -32.38845791999505508, 1523.382868172864164, 202.1182848005516348 ) ) ;
#8355 = DIRECTION ( 'NONE',  ( -1.755985294532469921E-16, 1.000000000000000000, -1.338183447452831989E-16 ) ) ;
#8356 = CARTESIAN_POINT ( 'NONE',  ( -10.94871860470700042, 1483.088542335439797, 204.4306030440669986 ) ) ;
#8357 = CARTESIAN_POINT ( 'NONE',  ( -12.24194870120000012, 1391.816349958050068, 206.8907653080489979 ) ) ;
#8358 = DIRECTION ( 'NONE',  ( -1.755985294532469921E-16, 1.000000000000000000, -1.338183447452831989E-16 ) ) ;
#8359 = CARTESIAN_POINT ( 'NONE',  ( -34.14991619301339654, 1450.428381852520033, 136.2391939585110094 ) ) ;
#8360 = CARTESIAN_POINT ( 'NONE',  ( -11.03223536238590086, 1462.458870289319975, 208.6692969917750133 ) ) ;
#8361 = B_SPLINE_CURVE_WITH_KNOTS ( 'NONE', 3,
 ( #54868, #19582, #54327, #104147, #80605, #3920, #61083, #95198, #53785, #95748, #19012, #87354, #78972, #2276, #36390, #87922, #79512, #2816, #36935, #39129 ),
 .UNSPECIFIED., .F., .F.,
 ( 4, 2, 1, 2, 2, 1, 1, 1, 1, 1, 2, 2, 4 ),
 ( 0.000000000000000000, 0.2500000000000632827, 0.3750000000000898170, 0.4375000000000980882, 0.5000000000001063594, 0.6250000000001328937, 0.6875000000001459943, 0.7187500000001525446, 0.7343750000001615375, 0.7421875000001608713, 0.7460937500001610934, 0.7500000000001613154, 1.000000000000000000 ),
 .UNSPECIFIED. ) ;
#8362 = CARTESIAN_POINT ( 'NONE',  ( -0.8182520991989999937, 1433.447543843880112, 150.4377610267980003 ) ) ;
#8363 = EDGE_CURVE ( 'NONE', #63441, #50666, #87000, .T. ) ;
#8364 = CARTESIAN_POINT ( 'NONE',  ( -21.22517433705326084, 1508.705765839073138, 191.9978281503293829 ) ) ;
#8365 = CARTESIAN_POINT ( 'NONE',  ( 11.89989176039999919, 1433.416276115000073, 150.2672394752979983 ) ) ;
#8366 = CARTESIAN_POINT ( 'NONE',  ( 27.19819524420000079, 1447.435760031770087, 248.0989693098979956 ) ) ;
#8367 = CARTESIAN_POINT ( 'NONE',  ( 11.91079909304919937, 1414.913060387399810, 198.1107945471090090 ) ) ;
#8368 = CARTESIAN_POINT ( 'NONE',  ( 0.5061640001184035675, 1467.094681707714244, 235.5773264646662710 ) ) ;
#8369 = CARTESIAN_POINT ( 'NONE',  ( 9.555970081965631024, 1422.926917982770192, 198.6394148135399860 ) ) ;
#8370 = CARTESIAN_POINT ( 'NONE',  ( 9.559796994581459373, 1464.142862108780264, 211.4021333761209860 ) ) ;
#8371 = CARTESIAN_POINT ( 'NONE',  ( 12.81185530964379815, 1416.835419214280137, 221.9980326694370092 ) ) ;
#8372 = CARTESIAN_POINT ( 'NONE',  ( 12.61713793920759663, 1398.287094680502605, 205.9900219852154351 ) ) ;
#8373 = CARTESIAN_POINT ( 'NONE',  ( -15.22206364535530021, 1509.523931070260005, 236.6035046314040073 ) ) ;
#8374 = B_SPLINE_CURVE_WITH_KNOTS ( 'NONE', 3,
 ( #14974, #7150, #40746, #57575, #100637, #13870 ),
 .UNSPECIFIED., .F., .F.,
 ( 4, 2, 4 ),
 ( 0.000000000000000000, 0.5000000000000000000, 1.000000000000000000 ),
 .UNSPECIFIED. ) ;
#8375 = CARTESIAN_POINT ( 'NONE',  ( -8.044681560367203943, 1424.920053392873342, 210.1656137535678397 ) ) ;
#8376 = AXIS2_PLACEMENT_3D ( 'NONE', #90181, #30835, #80706 ) ;
#8377 = CARTESIAN_POINT ( 'NONE',  ( 2.752776352959999784, 1478.720949088489988, 229.3133615295990069 ) ) ;
#8378 = DIRECTION ( 'NONE',  ( -0.6736849260863841948, 0.000000000000000000, 0.7390186874254148774 ) ) ;
#8379 = CARTESIAN_POINT ( 'NONE',  ( -15.99001483674529922, 1383.857625886600090, 219.4777900789640057 ) ) ;
#8380 = CARTESIAN_POINT ( 'NONE',  ( -2.397475438394535363, 1525.713797967456685, 175.0187375749330272 ) ) ;
#8381 = EDGE_CURVE ( 'NONE', #39065, #32037, #65646, .T. ) ;
#8382 = CARTESIAN_POINT ( 'NONE',  ( 10.59813984854799962, 1477.524079690600047, 229.9254213654089938 ) ) ;
#8383 = CARTESIAN_POINT ( 'NONE',  ( -4.609996619675000851, 1516.769879638719885, 212.5810025483170023 ) ) ;
#8384 = CARTESIAN_POINT ( 'NONE',  ( -21.93836957199999915, 1417.787473855720009, 209.9936763310599872 ) ) ;
#8385 = CARTESIAN_POINT ( 'NONE',  ( 0.1798334447694739935, 1474.584573357990166, 182.3269854996729862 ) ) ;
#8387 = VERTEX_POINT ( 'NONE', #32581 ) ;
#8386 = CARTESIAN_POINT ( 'NONE',  ( -6.033397232889999628, 1408.942087272730078, 222.3801906342980033 ) ) ;
#8388 = CARTESIAN_POINT ( 'NONE',  ( -25.25200574389469921, 1450.804213008409988, 137.6134964715130025 ) ) ;
#8389 = CARTESIAN_POINT ( 'NONE',  ( -16.65376764594610037, 1508.454796205149933, 213.7212175226700026 ) ) ;
#8390 = CARTESIAN_POINT ( 'NONE',  ( 12.40397477760000022, 1434.420140970890088, 149.9806263996979965 ) ) ;
#8391 = CARTESIAN_POINT ( 'NONE',  ( -41.66188030070010484, 1443.907795131759940, 134.0999999982419979 ) ) ;
#8392 = DIRECTION ( 'NONE',  ( 0.7071068048245321425, 1.133496607279266283E-10, 0.7071067575485621148 ) ) ;
#8393 = ORIENTED_EDGE ( 'NONE', *, *, #55867, .T. ) ;
#8394 = CARTESIAN_POINT ( 'NONE',  ( 15.84449002363500014, 1515.383078152259941, 223.0212718033670001 ) ) ;
#8395 = CARTESIAN_POINT ( 'NONE',  ( 9.664166848750001648, 1480.267612727490132, 204.8064600242389872 ) ) ;
#8396 = CARTESIAN_POINT ( 'NONE',  ( -17.29183738970000306, 1416.216252248629871, 214.4361153381880172 ) ) ;
#8397 = CARTESIAN_POINT ( 'NONE',  ( 9.520297885996999554, 1500.537487524489961, 228.7174115261980205 ) ) ;
#8398 = CARTESIAN_POINT ( 'NONE',  ( -8.242357959885127983, 1435.730723328530075, 211.7688826979850205 ) ) ;
#8399 = DIRECTION ( 'NONE',  ( -0.9995237709234272572, -0.03085824620765321644, -1.897025751615122517E-13 ) ) ;
#8400 = CARTESIAN_POINT ( 'NONE',  ( -15.16741077070000188, 1418.509014818010201, 212.0774864640089845 ) ) ;
#8401 = CARTESIAN_POINT ( 'NONE',  ( -5.360152366205530150, 1422.242722016050038, 144.1549655170190078 ) ) ;
#8402 = CARTESIAN_POINT ( 'NONE',  ( -12.10628020709999930, 1391.855112016120074, 208.7312492313569976 ) ) ;
#8403 = CARTESIAN_POINT ( 'NONE',  ( -85.40914635034850733, 1385.177617968390223, 289.1223791820979727 ) ) ;
#8404 = CARTESIAN_POINT ( 'NONE',  ( -11.52275967872940043, 1391.913060387289988, 210.8564297640039911 ) ) ;
#8405 = CARTESIAN_POINT ( 'NONE',  ( 10.54001418240659937, 1422.676165995590054, 209.0262571849499977 ) ) ;
#8406 = VERTEX_POINT ( 'NONE', #102384 ) ;
#8407 = CARTESIAN_POINT ( 'NONE',  ( -32.07183470040000373, 1450.932248063129919, 136.2258049830979871 ) ) ;
#8408 = EDGE_CURVE ( 'NONE', #105450, #40901, #103533, .T. ) ;
#8409 = FACE_OUTER_BOUND ( 'NONE', #75817, .T. ) ;
#8411 = ORIENTED_EDGE ( 'NONE', *, *, #42579, .T. ) ;
#8410 = CARTESIAN_POINT ( 'NONE',  ( -0.04641543425164609826, 1521.951704408389787, 230.3502074417858978 ) ) ;
#8412 = CARTESIAN_POINT ( 'NONE',  ( 2.356071275890000205, 1473.765556327289914, 219.2284513104989685 ) ) ;
#8413 = CARTESIAN_POINT ( 'NONE',  ( 33.23571934791672788, 1511.187213306747708, 219.4842663281462478 ) ) ;
#8414 = CARTESIAN_POINT ( 'NONE',  ( -7.132082164984229422, 1362.854272046530468, 207.6218459616988241 ) ) ;
#8415 = CARTESIAN_POINT ( 'NONE',  ( -9.086012908930001686, 1493.639819928789848, 201.8509011471290080 ) ) ;
#8416 = CARTESIAN_POINT ( 'NONE',  ( -4.283857371189049523, 1440.956241081810049, 155.9231041381889895 ) ) ;
#8417 = DIRECTION ( 'NONE',  ( 0.000000000000000000, 0.000000000000000000, 1.000000000000000000 ) ) ;
#8418 = CARTESIAN_POINT ( 'NONE',  ( 13.94796568798376946, 1429.572418609742044, 221.4045584918379745 ) ) ;
#8419 = CARTESIAN_POINT ( 'NONE',  ( 2.040662746359999780, 1417.628369438229811, 233.4326516709979842 ) ) ;
#8420 = CARTESIAN_POINT ( 'NONE',  ( 9.005061041439999414, 1450.163101882289993, 205.4957679819289922 ) ) ;
#8421 = CARTESIAN_POINT ( 'NONE',  ( -8.603573955260001682, 1512.656901503689824, 210.4681710982189884 ) ) ;
#8422 = CARTESIAN_POINT ( 'NONE',  ( -8.723604090509862630, 1369.380824275133136, 208.3718459617010978 ) ) ;
#8423 = ADVANCED_FACE ( 'NONE', ( #77210 ), #21383, .T. ) ;
#8424 = CARTESIAN_POINT ( 'NONE',  ( -30.61611611310621583, 1526.069472839374157, 216.5565799337567796 ) ) ;
#8425 = CARTESIAN_POINT ( 'NONE',  ( -7.337793750624999944, 1517.145312756229941, 206.2496372219370073 ) ) ;
#8426 = CIRCLE ( 'NONE', #94280, 95.87906523465393605 ) ;
#8427 = CARTESIAN_POINT ( 'NONE',  ( 4.271711532569999470, 1446.704874179759827, 157.7711585643980072 ) ) ;
#8428 = ADVANCED_FACE ( 'NONE', ( #41639 ), #93696, .F. ) ;
#8429 = CARTESIAN_POINT ( 'NONE',  ( -31.10384971727474479, 1525.795403621571268, 216.3488199036669926 ) ) ;
#8430 = CARTESIAN_POINT ( 'NONE',  ( -1.982554037259999902, 1496.032958330690008, 196.9258813337989977 ) ) ;
#8432 = VERTEX_POINT ( 'NONE', #23716 ) ;
#8431 = CARTESIAN_POINT ( 'NONE',  ( 1.157103504880000022, 1494.548177158689896, 220.2271105453990003 ) ) ;
#8433 = DIRECTION ( 'NONE',  ( -0.2054769195713187224, -0.000000000000000000, -0.9786619618251655162 ) ) ;
#8434 = VERTEX_POINT ( 'NONE', #59551 ) ;
#8435 = CARTESIAN_POINT ( 'NONE',  ( -16.43125158753896287, 1512.939392324912433, 220.7790245402972289 ) ) ;
#8436 = CARTESIAN_POINT ( 'NONE',  ( -24.07566136870000051, 1410.921070259630142, 208.6092334039690002 ) ) ;
#8438 = CARTESIAN_POINT ( 'NONE',  ( 16.05360826451080314, 1409.473653766179950, 193.0727167379100138 ) ) ;
#8437 = CARTESIAN_POINT ( 'NONE',  ( -11.04544962402649944, 1426.046997354040059, 102.3020123086109976 ) ) ;
#8439 = CARTESIAN_POINT ( 'NONE',  ( -4.608021707265000266, 1516.660388280709867, 210.8351633799069873 ) ) ;
#8440 = DIRECTION ( 'NONE',  ( -1.755985294532469921E-16, 1.000000000000000000, -1.338183447452831989E-16 ) ) ;
#8441 = CYLINDRICAL_SURFACE ( 'NONE', #83764, 1.000000000000000888 ) ;
#8442 = FILL_AREA_STYLE_COLOUR ( '', #96168 ) ;
#8443 = CARTESIAN_POINT ( 'NONE',  ( -12.70021235298639972, 1379.087509944640033, 208.7980280935229871 ) ) ;
#8444 = CARTESIAN_POINT ( 'NONE',  ( 15.05249117875021270, 1461.926097438958323, 229.9722081114364869 ) ) ;
#8445 = SHAPE_DEFINITION_REPRESENTATION ( #53566, #10812 ) ;
#8446 = CARTESIAN_POINT ( 'NONE',  ( 2.487935084889999704, 1508.551704408389924, 214.1089244042930204 ) ) ;
#8447 = CARTESIAN_POINT ( 'NONE',  ( -34.12598879534539975, 1437.021307524110171, 136.5549898716600126 ) ) ;
#8448 = ORIENTED_EDGE ( 'NONE', *, *, #11845, .T. ) ;
#8449 = CARTESIAN_POINT ( 'NONE',  ( 10.77727084197429974, 1397.924324489370292, 200.3403619048980033 ) ) ;
#8450 = CARTESIAN_POINT ( 'NONE',  ( -7.211935934568220574, 1517.151704408390060, 193.5679467272088345 ) ) ;
#8451 = CARTESIAN_POINT ( 'NONE',  ( -17.62109803770000127, 1460.304421794930022, 228.2025014059980208 ) ) ;
#8452 = ORIENTED_EDGE ( 'NONE', *, *, #2233, .T. ) ;
#8453 = EDGE_LOOP ( 'NONE', ( #28388, #56774, #780, #72782 ) ) ;
#8454 = AXIS2_PLACEMENT_3D ( 'NONE', #15785, #75743, #67357 ) ;
#8455 = FACE_OUTER_BOUND ( 'NONE', #84829, .T. ) ;
#8456 = CARTESIAN_POINT ( 'NONE',  ( 8.813958094369999330, 1425.194329715850017, 194.9377351523990001 ) ) ;
#8457 = CARTESIAN_POINT ( 'NONE',  ( -16.78480385485633519, 1526.748660780343471, 236.7163225783323526 ) ) ;
#8458 = CARTESIAN_POINT ( 'NONE',  ( -13.21112480721102500, 1416.964352618932935, 201.1890931735370032 ) ) ;
#8459 = CARTESIAN_POINT ( 'NONE',  ( 4.329448776040000446, 1515.064792882589927, 210.5737005773590056 ) ) ;
#8460 = TOROIDAL_SURFACE ( 'NONE', #90715, 2.000000000000000000, 1.000000000000000000 ) ;
#8461 = LINE ( 'NONE', #76786, #30052 ) ;
#8462 = DIRECTION ( 'NONE',  ( -0.7414773880254725835, -1.225281874271767957E-16, -0.6709778558543664229 ) ) ;
#8463 = DIRECTION ( 'NONE',  ( -0.9995237709234254808, 0.03085824620771311644, -1.986951185180850780E-13 ) ) ;
#8464 = CARTESIAN_POINT ( 'NONE',  ( 9.346483001066818730, 1451.068298621479926, 208.1598608262460175 ) ) ;
#8465 = CARTESIAN_POINT ( 'NONE',  ( -2.370970874524632510, 1427.002265528473799, 137.0999999980979851 ) ) ;
#8466 = CARTESIAN_POINT ( 'NONE',  ( -101.4814120043199921, 1384.878864375810053, 296.5146955053820079 ) ) ;
#8467 = ORIENTED_EDGE ( 'NONE', *, *, #53596, .F. ) ;
#8468 = CARTESIAN_POINT ( 'NONE',  ( -6.944231786295000042, 1516.882690742909972, 202.5683215544970039 ) ) ;
#8469 = CARTESIAN_POINT ( 'NONE',  ( 0.007128837152181529378, 1517.006509894990131, 209.8686634857439799 ) ) ;
#8470 = ORIENTED_EDGE ( 'NONE', *, *, #28567, .F. ) ;
#8471 = CARTESIAN_POINT ( 'NONE',  ( 11.74578019742499890, 1426.720260049070021, 144.7832389959820034 ) ) ;
#8472 = CARTESIAN_POINT ( 'NONE',  ( 19.97280420420000269, 1487.549460532730109, 227.0589497365980094 ) ) ;
#8473 = ORIENTED_EDGE ( 'NONE', *, *, #69990, .T. ) ;
#8474 = CARTESIAN_POINT ( 'NONE',  ( -13.68684928409999912, 1415.245980412430072, 220.9574426735980239 ) ) ;
#8475 = CARTESIAN_POINT ( 'NONE',  ( -11.62445858788020026, 1432.338721124250014, 150.9950008028209822 ) ) ;
#8476 = CARTESIAN_POINT ( 'NONE',  ( 22.04556278850125040, 1524.082582765195411, 233.7638865113347038 ) ) ;
#8477 = CARTESIAN_POINT ( 'NONE',  ( -10.13499527144800005, 1462.137798843650216, 208.1879751690069895 ) ) ;
#8478 = CARTESIAN_POINT ( 'NONE',  ( -4.599789036639999829, 1421.972502547630029, 185.2173717891980118 ) ) ;
#8479 = MANIFOLD_SOLID_BREP ( 'Stock-MAS-682-1', #41329 ) ;
#8480 = CARTESIAN_POINT ( 'NONE',  ( 10.01091973119789991, 1469.175247106300048, 207.4504093468829922 ) ) ;
#8481 = CARTESIAN_POINT ( 'NONE',  ( 0.06584449245319999588, 1508.965707083629923, 179.3766826265980114 ) ) ;
#8482 = CARTESIAN_POINT ( 'NONE',  ( -12.82501412541063601, 1410.734581749099561, 189.5959794609471487 ) ) ;
#8483 = CARTESIAN_POINT ( 'NONE',  ( -62.03809624990000060, 1379.749343316239901, 266.3689138319589915 ) ) ;
#8484 = CARTESIAN_POINT ( 'NONE',  ( 23.61616453110579883, 1435.156076846089945, 206.2084620324950208 ) ) ;
#8486 = CARTESIAN_POINT ( 'NONE',  ( 6.945936638575799904, 1467.632090493969827, 200.3893422253750032 ) ) ;
#8485 = CARTESIAN_POINT ( 'NONE',  ( -3.834487992390000155, 1497.252746959389924, 198.5300765076990217 ) ) ;
#8487 = CARTESIAN_POINT ( 'NONE',  ( -4.703918259281699044, 1423.649054296706709, 184.4972853060825173 ) ) ;
#8488 = ADVANCED_FACE ( 'NONE', ( #87512 ), #26474, .T. ) ;
#8489 = CARTESIAN_POINT ( 'NONE',  ( -5.360124858665960446, 1422.242564188120014, 144.1629134808320032 ) ) ;
#8490 = ORIENTED_EDGE ( 'NONE', *, *, #93521, .T. ) ;
#8491 = CARTESIAN_POINT ( 'NONE',  ( 16.82650268237432201, 1517.015067831505576, 223.4080418569560322 ) ) ;
#8492 = B_SPLINE_CURVE_WITH_KNOTS ( 'NONE', 3,
 ( #81251, #40355, #100272, #57192, #5670, #98608, #90759 ),
 .UNSPECIFIED., .F., .F.,
 ( 4, 3, 4 ),
 ( -157.7108139880000124, -101.4631914111549946, -30.86246212799579780 ),
 .UNSPECIFIED. ) ;
#8493 = CARTESIAN_POINT ( 'NONE',  ( -21.92026280708428132, 1524.524650307242837, 233.6742115692356094 ) ) ;
#8494 = CARTESIAN_POINT ( 'NONE',  ( -2.907988962752879658, 1484.679952288234063, 183.2543140236687407 ) ) ;
#8495 =( BOUNDED_CURVE ( )  B_SPLINE_CURVE ( 3, ( #62713, #96832, #97361, #106854 ),
 .UNSPECIFIED., .F., .F. ) 
 B_SPLINE_CURVE_WITH_KNOTS ( ( 4, 4 ),
 ( 1.268017777846622174, 1.928411132994934940 ),
 .UNSPECIFIED. ) 
 CURVE ( )  GEOMETRIC_REPRESENTATION_ITEM ( )  RATIONAL_B_SPLINE_CURVE ( ( 1.000000000000000000, 0.9639857288230757604, 0.9639857288230757604, 1.000000000000000000 ) ) 
 REPRESENTATION_ITEM ( '' )  );
#8496 = CARTESIAN_POINT ( 'NONE',  ( -14.93837056410000130, 1416.023439710309958, 212.9159407817990086 ) ) ;
#8498 = EDGE_LOOP ( 'NONE', ( #86653, #59052, #102105, #67868, #39334 ) ) ;
#8497 = CARTESIAN_POINT ( 'NONE',  ( 4.491288139582719552, 1508.884219106000046, 212.6094330128009915 ) ) ;
#8499 = CARTESIAN_POINT ( 'NONE',  ( 1.341949918430000110, 1416.837177098230086, 190.1629998231980210 ) ) ;
#8500 = CARTESIAN_POINT ( 'NONE',  ( 1.821641572679999932, 1508.445828156189918, 220.3212548158989819 ) ) ;
#8501 = ADVANCED_FACE ( 'NONE', ( #10234 ), #25749, .F. ) ;
#8502 = CARTESIAN_POINT ( 'NONE',  ( -10.93042732790000038, 1429.541181187929851, 151.2220225859979905 ) ) ;
#8503 = CARTESIAN_POINT ( 'NONE',  ( -14.78895068404719915, 1427.485687361509918, 221.7293924355389834 ) ) ;
#8504 = CARTESIAN_POINT ( 'NONE',  ( 2.793296738545309577, 1446.096199209579936, 199.4004782075479909 ) ) ;
#8505 = CARTESIAN_POINT ( 'NONE',  ( 11.22085813615770000, 1414.913060387329779, 197.6243702374680140 ) ) ;
#8506 = LINE ( 'NONE', #110429, #28813 ) ;
#8507 = FACE_BOUND ( 'NONE', #89066, .T. ) ;
#8509 = CARTESIAN_POINT ( 'NONE',  ( -11.41709147838199989, 1481.865887416040096, 208.5948008914320155 ) ) ;
#8508 = CARTESIAN_POINT ( 'NONE',  ( -21.39747632310000114, 1482.727152785329963, 225.0468285881979966 ) ) ;
#8511 = CARTESIAN_POINT ( 'NONE',  ( -5.260591405550000488, 1471.234187460190242, 214.2384833057390097 ) ) ;
#8510 = VECTOR ( 'NONE', #4287, 1000.000000000000000 ) ;
#8512 = ORIENTED_EDGE ( 'NONE', *, *, #82945, .T. ) ;
#8513 = CARTESIAN_POINT ( 'NONE',  ( 4.609064303374999838, 1516.723920667490120, 206.2441009858569885 ) ) ;
#8514 = CARTESIAN_POINT ( 'NONE',  ( 31.26225106439999735, 1415.948784915929991, 269.3319312554980343 ) ) ;
#8515 = CARTESIAN_POINT ( 'NONE',  ( 2.463295206089754608, 1464.794365557463379, 237.1801197134051336 ) ) ;
#8516 = CARTESIAN_POINT ( 'NONE',  ( 22.48977040930000015, 1469.151985490530251, 196.6582214529979922 ) ) ;
#8517 = CARTESIAN_POINT ( 'NONE',  ( -0.4212817365179999940, 1508.863410648129957, 238.3519434705980018 ) ) ;
#8518 = CARTESIAN_POINT ( 'NONE',  ( -10.67458942334280003, 1390.939239166159950, 215.3172498179779666 ) ) ;
#8519 = CARTESIAN_POINT ( 'NONE',  ( -41.35142502486309724, 1442.058002965339938, 136.3890446465489958 ) ) ;
#8520 = B_SPLINE_CURVE_WITH_KNOTS ( 'NONE', 3,
 ( #107887, #83243, #65915, #56957, #13259, #13809, #100033, #7088, #89986, #92193 ),
 .UNSPECIFIED., .F., .F.,
 ( 4, 2, 2, 2, 4 ),
 ( 0.000000000000000000, 0.2500000000000000000, 0.5000000000000000000, 0.7500000000000000000, 1.000000000000000000 ),
 .UNSPECIFIED. ) ;
#8521 = CARTESIAN_POINT ( 'NONE',  ( 13.57704973455800079, 1430.332977960800008, 195.9178655745220112 ) ) ;
#8522 = CARTESIAN_POINT ( 'NONE',  ( -15.77133688790000043, 1418.153097379740075, 203.3734809581490026 ) ) ;
#8523 = CARTESIAN_POINT ( 'NONE',  ( -14.34037905889999998, 1443.120642612440179, 188.8125533694979765 ) ) ;
#8524 = ADVANCED_FACE ( 'NONE', ( #81834 ), #36444, .F. ) ;
#8525 = CARTESIAN_POINT ( 'NONE',  ( -4.107751809467400150, 1485.192704402420077, 197.9515937704389898 ) ) ;
#8526 = CARTESIAN_POINT ( 'NONE',  ( -16.60289890951143121, 1419.621976417301084, 209.1245877213969777 ) ) ;
#8527 = CARTESIAN_POINT ( 'NONE',  ( 3.565775598909999733, 1407.753784349630223, 270.1349117941979898 ) ) ;
#8528 = ORIENTED_EDGE ( 'NONE', *, *, #27617, .T. ) ;
#8529 = EDGE_CURVE ( 'NONE', #97755, #71088, #78645, .T. ) ;
#8530 = CARTESIAN_POINT ( 'NONE',  ( 1.453919372226760043, 1501.892033211519902, 181.3410715267950195 ) ) ;
#8531 = CARTESIAN_POINT ( 'NONE',  ( -13.68648241757620099, 1409.391002885000034, 215.1022502297769847 ) ) ;
#8532 = B_SPLINE_CURVE_WITH_KNOTS ( 'NONE', 5,
 ( #49054, #7578, #98878, #31122, #99415, #41187 ),
 .UNSPECIFIED., .F., .F.,
 ( 6, 6 ),
 ( 0.000000000000000000, 1.000000000000000000 ),
 .UNSPECIFIED. ) ;
#8534 = EDGE_CURVE ( 'NONE', #50989, #100544, #107051, .T. ) ;
#8533 = CARTESIAN_POINT ( 'NONE',  ( 3.487592431261229642, 1509.038615938009798, 213.6090957240379851 ) ) ;
#8535 = CARTESIAN_POINT ( 'NONE',  ( -12.23039686304473506, 1377.875207865813309, 210.5705953414277189 ) ) ;
#8536 = CARTESIAN_POINT ( 'NONE',  ( -23.70279561169999738, 1471.127482098729843, 267.2984211408980286 ) ) ;
#8537 = CARTESIAN_POINT ( 'NONE',  ( -18.76586283470000183, 1443.851548150590133, 210.9125287142690013 ) ) ;
#8538 = CARTESIAN_POINT ( 'NONE',  ( -14.32480461217465262, 1514.214463197139139, 192.6030336675313777 ) ) ;
#8539 = LINE ( 'NONE', #78525, #109372 ) ;
#8540 = CARTESIAN_POINT ( 'NONE',  ( -66.03589273005509597, 1384.674347821650144, 290.1675141113110499 ) ) ;
#8541 = B_SPLINE_SURFACE_WITH_KNOTS ( 'NONE', 5, 5, ( 
 ( #44765, #78348, #96251, #103535, #53731, #29051 ),
 ( #9480, #1657, #87869, #11159, #35234, #62688 ),
 ( #3323, #37448, #71647, #82190, #21158, #100102 ),
 ( #12233, #22814, #73818, #4406, #64321, #55364 ),
 ( #63768, #81089, #38534, #107947, #22257, #65422 ),
 ( #37998, #89497, #80555, #30689, #46968, #72181 ) ),
 .UNSPECIFIED., .F., .F., .F.,
 ( 6, 6 ),
 ( 6, 6 ),
 ( 82.60151368457970023, 128.3333305958969959 ),
 ( -0.002296749680308819968, 2.002296750983780349 ),
 .UNSPECIFIED. ) ;
#8542 = CARTESIAN_POINT ( 'NONE',  ( 19.02839246307539511, 1456.959193721570273, 225.8332742494027912 ) ) ;
#8543 = AXIS2_PLACEMENT_3D ( 'NONE', #22574, #109393, #32669 ) ;
#8544 = CARTESIAN_POINT ( 'NONE',  ( -9.624350592200000776, 1441.605633920840091, 153.1179271311979733 ) ) ;
#8545 = EDGE_CURVE ( 'NONE', #65361, #21837, #90235, .T. ) ;
#8546 = CARTESIAN_POINT ( 'NONE',  ( -106.6639532879999877, 1379.150924026149823, 300.4020406703589856 ) ) ;
#8547 = FACE_OUTER_BOUND ( 'NONE', #65768, .T. ) ;
#8548 = DIRECTION ( 'NONE',  ( 1.442302170131585847E-09, -0.8818471531508758066, 0.4715353629153342663 ) ) ;
#8549 = AXIS2_PLACEMENT_3D ( 'NONE', #58188, #25104, #75550 ) ;
#8550 = CARTESIAN_POINT ( 'NONE',  ( -23.05373657170000001, 1411.078320233030126, 204.9169236815779982 ) ) ;
#8551 = CARTESIAN_POINT ( 'NONE',  ( -8.361580061790082397, 1382.865204230077325, 199.9025052525546471 ) ) ;
#8552 = CARTESIAN_POINT ( 'NONE',  ( 3.747879590680000206, 1486.431719912689914, 219.2436390487989968 ) ) ;
#8553 = CARTESIAN_POINT ( 'NONE',  ( 11.69055014891650046, 1479.114015910159878, 207.7900583562500003 ) ) ;
#8554 = CARTESIAN_POINT ( 'NONE',  ( 2.455820327400000114, 1434.541746329560056, 150.3615916412979914 ) ) ;
#8555 = CARTESIAN_POINT ( 'NONE',  ( -19.44024196839999874, 1446.691694840189939, 200.1268145916089907 ) ) ;
#8556 = CARTESIAN_POINT ( 'NONE',  ( -5.513222351421919853, 1508.611138448520023, 216.4434734794269843 ) ) ;
#8557 = CARTESIAN_POINT ( 'NONE',  ( -17.84104529106779680, 1489.004166502169937, 195.1797425130460226 ) ) ;
#8559 = CARTESIAN_POINT ( 'NONE',  ( -9.249153156179998447, 1382.907106044650163, 200.4653998181289865 ) ) ;
#8558 = CARTESIAN_POINT ( 'NONE',  ( -21.81077096749999811, 1409.674709292730086, 210.2046642649879971 ) ) ;
#8560 = CARTESIAN_POINT ( 'NONE',  ( 11.71130021051819980, 1426.712571118619962, 142.3277864718619696 ) ) ;
#8561 = CARTESIAN_POINT ( 'NONE',  ( 0.9603320758176961958, 1368.656171133117368, 210.4211784721450726 ) ) ;
#8562 = CARTESIAN_POINT ( 'NONE',  ( 2.372478608332516892, 1522.382868172863937, 243.3440112565233449 ) ) ;
#8563 = CARTESIAN_POINT ( 'NONE',  ( 6.984146249619830549, 1448.464884018210114, 201.5728536464569913 ) ) ;
#8564 = CARTESIAN_POINT ( 'NONE',  ( 11.16717556649999921, 1414.661898229710005, 205.5169791222290030 ) ) ;
#8565 = CARTESIAN_POINT ( 'NONE',  ( -3.456007423304999993, 1516.647534046129977, 202.5739645571870255 ) ) ;
#8567 = CARTESIAN_POINT ( 'NONE',  ( -8.010882276929157442, 1398.150985990356958, 219.3602984231706330 ) ) ;
#8566 = VECTOR ( 'NONE', #97905, 1000.000000000000114 ) ;
#8568 = DIRECTION ( 'NONE',  ( -0.9990022738941407576, 0.04465933583335028600, -2.184628763019654698E-05 ) ) ;
#8569 = DIRECTION ( 'NONE',  ( 1.755985294532469921E-16, -1.000000000000000000, 1.338183447452830017E-16 ) ) ;
#8570 = CARTESIAN_POINT ( 'NONE',  ( 1.969186904083861878, 1477.306100694335782, 198.9158131895061388 ) ) ;
#8571 = EDGE_CURVE ( 'NONE', #28705, #56028, #36712, .T. ) ;
#8572 = CARTESIAN_POINT ( 'NONE',  ( 7.440231166432099030, 1504.359119642949963, 219.0606402491349911 ) ) ;
#8574 = ORIENTED_EDGE ( 'NONE', *, *, #5027, .T. ) ;
#8573 = CARTESIAN_POINT ( 'NONE',  ( -31.33310914745869624, 1379.622867399459892, 219.3631401044190170 ) ) ;
#8575 = ORIENTED_EDGE ( 'NONE', *, *, #97509, .F. ) ;
#8576 = CARTESIAN_POINT ( 'NONE',  ( 11.25278939239490050, 1434.345226179090105, 151.5801780830220196 ) ) ;
#8577 = CARTESIAN_POINT ( 'NONE',  ( 21.55491250604723064, 1524.059663615499858, 184.0356616387038002 ) ) ;
#8578 = ORIENTED_EDGE ( 'NONE', *, *, #72151, .T. ) ;
#8579 = CARTESIAN_POINT ( 'NONE',  ( -0.0002530612592032526744, 1396.486685308509095, 221.5233369264674650 ) ) ;
#8580 = CARTESIAN_POINT ( 'NONE',  ( -22.37835337210000120, 1507.839481092230017, 193.8708192753979915 ) ) ;
#8581 = CARTESIAN_POINT ( 'NONE',  ( 30.25425994617009096, 1522.382868172863937, 218.9520509131588994 ) ) ;
#8584 = EDGE_CURVE ( 'NONE', #11042, #10258, #20278, .T. ) ;
#8583 = CARTESIAN_POINT ( 'NONE',  ( 6.861707994109999653, 1428.078401598830169, 112.4493539157979995 ) ) ;
#8582 = DIRECTION ( 'NONE',  ( 1.755985294532464991E-16, -1.000000000000000000, 1.338183447452830017E-16 ) ) ;
#8585 = CARTESIAN_POINT ( 'NONE',  ( 18.22709068499189655, 1488.412411835820194, 229.3642029072559865 ) ) ;
#8586 = CARTESIAN_POINT ( 'NONE',  ( 9.594803834039998591, 1488.165126248830120, 184.4998152664979898 ) ) ;
#8587 = CARTESIAN_POINT ( 'NONE',  ( 2.580208331920000209, 1468.552870077789976, 218.8097162688989670 ) ) ;
#8588 = DIRECTION ( 'NONE',  ( 1.755985294532469921E-16, -1.000000000000000000, 1.338183447452831989E-16 ) ) ;
#8589 = CARTESIAN_POINT ( 'NONE',  ( -12.78776258895079998, 1416.851343896850040, 195.5391574246120001 ) ) ;
#8590 = CARTESIAN_POINT ( 'NONE',  ( 13.69065454780360014, 1415.152886232609944, 197.6322036034630116 ) ) ;
#8591 = CARTESIAN_POINT ( 'NONE',  ( 11.56811281929999957, 1431.694744716809964, 151.1673513621979907 ) ) ;
#8592 = CARTESIAN_POINT ( 'NONE',  ( 7.211759810944999849, 1511.702066573629963, 202.3497083402869805 ) ) ;
#8593 = ORIENTED_EDGE ( 'NONE', *, *, #44723, .F. ) ;
#8594 = CARTESIAN_POINT ( 'NONE',  ( 13.64099228464760039, 1434.977781978229814, 148.9109081837199824 ) ) ;
#8595 = ORIENTED_EDGE ( 'NONE', *, *, #26521, .T. ) ;
#8596 = VERTEX_POINT ( 'NONE', #11899 ) ;
#8597 = CARTESIAN_POINT ( 'NONE',  ( 13.41809782280081897, 1444.381396344529094, 169.3665683494473910 ) ) ;
#8598 = CARTESIAN_POINT ( 'NONE',  ( -5.041740361659999614, 1464.446899236929994, 235.7978687534979940 ) ) ;
#8599 = AXIS2_PLACEMENT_3D ( 'NONE', #38062, #20144, #106367 ) ;
#8600 = CARTESIAN_POINT ( 'NONE',  ( -2.290886304614999869, 1517.184383877180153, 216.4605998004670084 ) ) ;
#8601 = CARTESIAN_POINT ( 'NONE',  ( -2.500000000000000000, 1448.210448412289907, 170.5244215879980061 ) ) ;
#8602 = CARTESIAN_POINT ( 'NONE',  ( -18.94224506989981904, 1443.728200593167458, 212.0298136739947665 ) ) ;
#8603 = CARTESIAN_POINT ( 'NONE',  ( 2.500000000000000000, 1448.251495160190188, 165.7055370936290046 ) ) ;
#8604 = CARTESIAN_POINT ( 'NONE',  ( -20.15452302159999931, 1507.845791376729949, 228.9024215066979764 ) ) ;
#8605 = CARTESIAN_POINT ( 'NONE',  ( 1.701027822874999984, 1516.937508036699910, 206.6270879340970055 ) ) ;
#8606 = ORIENTED_EDGE ( 'NONE', *, *, #65486, .T. ) ;
#8607 = CARTESIAN_POINT ( 'NONE',  ( 22.31762535187430174, 1440.913060387330006, 228.8232858593530068 ) ) ;
#8608 = CARTESIAN_POINT ( 'NONE',  ( -19.26331490529999968, 1508.281539162429908, 229.6732352803980177 ) ) ;
#8609 = CARTESIAN_POINT ( 'NONE',  ( -11.55154600989999913, 1410.249881412029936, 189.0607701063979960 ) ) ;
#8610 = CARTESIAN_POINT ( 'NONE',  ( 7.458171671575000161, 1513.513616978040091, 215.6792808263570009 ) ) ;
#8612 = ORIENTED_EDGE ( 'NONE', *, *, #75587, .F. ) ;
#8611 = CARTESIAN_POINT ( 'NONE',  ( 0.3878997263335109968, 1423.031706118989860, 192.4974707188740126 ) ) ;
#8613 = CARTESIAN_POINT ( 'NONE',  ( 18.42577565999999933, 1424.509266043230127, 223.4215470970979993 ) ) ;
#8614 = CARTESIAN_POINT ( 'NONE',  ( -14.16375222470900219, 1508.551704408389924, 210.3503176839390107 ) ) ;
#8616 = LINE ( 'NONE', #9733, #48463 ) ;
#8615 = VECTOR ( 'NONE', #86611, 1000.000000000000000 ) ;
#8617 = CARTESIAN_POINT ( 'NONE',  ( 0.001396730326707920156, 1465.018684410219976, 237.3906889929259876 ) ) ;
#8618 = CARTESIAN_POINT ( 'NONE',  ( 19.37374569213924858, 1526.382868172863937, 183.8768763279539655 ) ) ;
#8619 = AXIS2_PLACEMENT_3D ( 'NONE', #46454, #38031, #29617 ) ;
#8620 = CARTESIAN_POINT ( 'NONE',  ( -6.550389470255000290, 1516.755758396839838, 214.1281755516169767 ) ) ;
#8621 = CONICAL_SURFACE ( 'NONE', #76567, 6.911399307709998219, 0.04363323129990067523 ) ;
#8622 = CARTESIAN_POINT ( 'NONE',  ( -2.768293557658910053, 1429.049511582360083, 200.1700803755659877 ) ) ;
#8623 = CARTESIAN_POINT ( 'NONE',  ( 22.70509004431190192, 1409.705939603270053, 209.2982552845940063 ) ) ;
#8624 = VECTOR ( 'NONE', #15767, 1000.000000000000000 ) ;
#8625 = CARTESIAN_POINT ( 'NONE',  ( 6.769623004886519801, 1509.032014039220030, 216.3879256010220047 ) ) ;
#8626 = CARTESIAN_POINT ( 'NONE',  ( -5.770883602015000058, 1516.603620185149794, 211.4160555996369908 ) ) ;
#8627 = CARTESIAN_POINT ( 'NONE',  ( -11.74702494663919872, 1482.400884356720098, 207.2154382537309800 ) ) ;
#8628 = CARTESIAN_POINT ( 'NONE',  ( 29.95988583835885066, 1525.317349363550420, 221.5595150200594787 ) ) ;
#8630 = ORIENTED_EDGE ( 'NONE', *, *, #98027, .F. ) ;
#8629 = CARTESIAN_POINT ( 'NONE',  ( -64.53706522309998661, 1385.084217465399888, 254.0329369609589776 ) ) ;
#8631 = CARTESIAN_POINT ( 'NONE',  ( -61.29450154859880229, 1385.059859360860173, 283.1170003335910224 ) ) ;
#8632 = CARTESIAN_POINT ( 'NONE',  ( 5.442004255449999661, 1468.737548876029905, 250.5651368528980072 ) ) ;
#8633 = CARTESIAN_POINT ( 'NONE',  ( 3.347294972025637527, 1451.126043403471158, 184.0057138541948802 ) ) ;
#8634 = CARTESIAN_POINT ( 'NONE',  ( -28.85571497835669774, 1509.920724158590019, 214.5067048101039973 ) ) ;
#8635 = B_SPLINE_CURVE_WITH_KNOTS ( 'NONE', 5,
 ( #19447, #78827, #104570, #54200, #72635, #80480, #3798, #89424, #12714, #21641, #81022, #88326, #27865, #4331, #30055, #62045, #79930, #105129, #64246, #62618, #55846 ),
 .UNSPECIFIED., .F., .F.,
 ( 6, 3, 3, 3, 3, 3, 6 ),
 ( 0.000000000000000000, 0.05351524642481629568, 0.1243167101037662425, 0.1849540613865951477, 0.2691738040383257480, 0.5436324044764058172, 1.000000000000000000 ),
 .UNSPECIFIED. ) ;
#8636 = CARTESIAN_POINT ( 'NONE',  ( -2.709137183217330325, 1508.767349011980059, 237.8404265817369776 ) ) ;
#8637 = CARTESIAN_POINT ( 'NONE',  ( -12.71559489689999900, 1467.455103516190093, 192.9444858715990279 ) ) ;
#8638 = CARTESIAN_POINT ( 'NONE',  ( 10.96771871713499813, 1512.594959757389915, 225.0393121556670053 ) ) ;
#8640 = CARTESIAN_POINT ( 'NONE',  ( 17.73893480064900174, 1410.031254009529903, 222.7710511100789859 ) ) ;
#8639 = DIRECTION ( 'NONE',  ( -5.980589973904019347E-17, 1.000000000000000000, -1.736889445713099699E-16 ) ) ;
#8641 = CARTESIAN_POINT ( 'NONE',  ( -9.545666265298249797, 1448.964112459540047, 208.2525275868840140 ) ) ;
#8642 = CARTESIAN_POINT ( 'NONE',  ( -108.5927978296600003, 1383.291025085730098, 310.9196457646229987 ) ) ;
#8643 = CIRCLE ( 'NONE', #35515, 1.000000000000000888 ) ;
#8644 = ORIENTED_EDGE ( 'NONE', *, *, #84525, .T. ) ;
#8645 = CARTESIAN_POINT ( 'NONE',  ( 3.257220602695000355, 1517.040132827679827, 203.3350082531769942 ) ) ;
#8646 = CARTESIAN_POINT ( 'NONE',  ( 0.1078348715190000084, 1405.842710276629987, 267.2349610867980232 ) ) ;
#8647 = CARTESIAN_POINT ( 'NONE',  ( 29.06854786870000140, 1509.928156446929961, 206.2948012444579717 ) ) ;
#8648 = CARTESIAN_POINT ( 'NONE',  ( 12.78755496059999786, 1416.844618646730169, 222.9177554085979978 ) ) ;
#8649 = CARTESIAN_POINT ( 'NONE',  ( -6.220539724137306159, 1424.583771648741731, 186.6152494251206235 ) ) ;
#8650 = CARTESIAN_POINT ( 'NONE',  ( -19.48953932349999718, 1466.720370645889943, 212.7779717757290143 ) ) ;
#8651 = CARTESIAN_POINT ( 'NONE',  ( 2.765840192760000260, 1444.819550295790123, 203.5022050451889868 ) ) ;
#8652 = CARTESIAN_POINT ( 'NONE',  ( 33.29225716172200578, 1435.659897776519983, 135.5215965639700073 ) ) ;
#8653 = DIRECTION ( 'NONE',  ( 0.000000000000000000, 1.000000000000000000, 0.000000000000000000 ) ) ;
#8654 = CARTESIAN_POINT ( 'NONE',  ( -2.210109237099999735, 1430.259655991189902, 200.9461818968590023 ) ) ;
#8655 = EDGE_CURVE ( 'NONE', #26067, #25916, #97915, .T. ) ;
#8656 = CARTESIAN_POINT ( 'NONE',  ( 8.326538737159999926, 1507.918727144829973, 183.0016939534980338 ) ) ;
#8657 = CARTESIAN_POINT ( 'NONE',  ( 8.179408651070591674, 1464.307684099787593, 216.6184067479095745 ) ) ;
#8658 = CARTESIAN_POINT ( 'NONE',  ( -21.95768443299153461, 1524.412455883367329, 184.5445616807625981 ) ) ;
#8659 = CARTESIAN_POINT ( 'NONE',  ( -9.521904627593841042, 1448.210782710000103, 209.8760350557079732 ) ) ;
#8660 = ORIENTED_EDGE ( 'NONE', *, *, #61831, .F. ) ;
#8661 = CARTESIAN_POINT ( 'NONE',  ( 20.06031067115782918, 1526.189899547014420, 185.1817256993992942 ) ) ;
#8662 = CARTESIAN_POINT ( 'NONE',  ( 11.87980743189999977, 1433.311001100440080, 146.5967650327979754 ) ) ;
#8663 = CARTESIAN_POINT ( 'NONE',  ( 21.62164173326539895, 1522.051704408389924, 208.0273405521070060 ) ) ;
#8664 = CARTESIAN_POINT ( 'NONE',  ( 15.03006911687520031, 1447.439797465169931, 189.9780440897100107 ) ) ;
#8665 = LINE ( 'NONE', #8119, #44685 ) ;
#8667 = PLANE ( 'NONE',  #94587 ) ;
#8666 = DIRECTION ( 'NONE',  ( -0.3090169943749382919, -2.144236138472229863E-15, 0.9510565162951565288 ) ) ;
#8668 = CARTESIAN_POINT ( 'NONE',  ( -29.74048408400000199, 1509.991911973829929, 210.0353904563160086 ) ) ;
#8669 = CARTESIAN_POINT ( 'NONE',  ( 11.75869035672759999, 1517.151704408390060, 227.2994842695800060 ) ) ;
#8670 = CARTESIAN_POINT ( 'NONE',  ( -2.329906352152919968, 1515.372228416590133, 213.3835081558460161 ) ) ;
#8671 = CARTESIAN_POINT ( 'NONE',  ( -11.48552941940051220, 1418.748566887944889, 229.1496130817171775 ) ) ;
#8673 = ADVANCED_FACE ( 'NONE', ( #80758 ), #38710, .T. ) ;
#8672 = CARTESIAN_POINT ( 'NONE',  ( 17.99954443082109989, 1410.904693892220166, 222.9872220945560173 ) ) ;
#8674 = CARTESIAN_POINT ( 'NONE',  ( 3.208637323091700022, 1515.551704408389696, 212.9514660497620184 ) ) ;
#8675 = CARTESIAN_POINT ( 'NONE',  ( 24.07357629730000070, 1435.356839239090050, 136.9693785357980005 ) ) ;
#8676 = CARTESIAN_POINT ( 'NONE',  ( -10.83121030459200007, 1396.291294585879996, 206.8277440348720120 ) ) ;
#8677 = ORIENTED_EDGE ( 'NONE', *, *, #91091, .T. ) ;
#8678 = DIRECTION ( 'NONE',  ( -1.699538841806929935E-33, 1.000000000000000000, -1.698192320643030073E-16 ) ) ;
#8679 = CARTESIAN_POINT ( 'NONE',  ( 21.77056714271089177, 1509.419234230875190, 226.6994063304933036 ) ) ;
#8680 = EDGE_CURVE ( 'NONE', #17382, #54193, #56412, .T. ) ;
#8681 = VERTEX_POINT ( 'NONE', #108146 ) ;
#8682 = ORIENTED_EDGE ( 'NONE', *, *, #53997, .T. ) ;
#8683 = CARTESIAN_POINT ( 'NONE',  ( -12.60557393880000099, 1502.061266880889889, 211.1128455371190000 ) ) ;
#8684 = DIRECTION ( 'NONE',  ( 0.000000000000000000, 0.000000000000000000, -1.000000000000000000 ) ) ;
#8686 = CARTESIAN_POINT ( 'NONE',  ( 4.363122647530000009, 1432.413060387330006, 146.1721969590979882 ) ) ;
#8685 = CARTESIAN_POINT ( 'NONE',  ( 11.12372166200000123, 1426.894033309730048, 99.60654041669779701 ) ) ;
#8687 = CARTESIAN_POINT ( 'NONE',  ( 23.57985488250000117, 1410.231772307329948, 210.8506199998580257 ) ) ;
#8688 = CARTESIAN_POINT ( 'NONE',  ( -11.87499642090000052, 1433.007151748719934, 150.0792799791980201 ) ) ;
#8689 = CARTESIAN_POINT ( 'NONE',  ( -28.76039927569999932, 1380.228231664269970, 215.0392276715589901 ) ) ;
#8690 = CARTESIAN_POINT ( 'NONE',  ( -2.496155285332042784, 1421.191123497494345, 184.8720394902521207 ) ) ;
#8691 = CIRCLE ( 'NONE', #85580, 1.999999999999973577 ) ;
#8692 = CARTESIAN_POINT ( 'NONE',  ( 7.096850047520000260, 1424.506042705289929, 213.0086243585190005 ) ) ;
#8693 = CARTESIAN_POINT ( 'NONE',  ( -9.609628710759999137, 1464.248356776189894, 228.1965957863990013 ) ) ;
#8694 = CARTESIAN_POINT ( 'NONE',  ( 21.84020450222056553, 1512.187213306747481, 234.9798068779740277 ) ) ;
#8695 = CARTESIAN_POINT ( 'NONE',  ( 3.236908035719999965, 1449.131113800429830, 183.9272198847980064 ) ) ;
#8696 = AXIS2_PLACEMENT_3D ( 'NONE', #54348, #17936, #79534 ) ;
#8697 = CARTESIAN_POINT ( 'NONE',  ( 7.310316353548246049, 1364.149046361921137, 209.6218459617148824 ) ) ;
#8698 = B_SPLINE_CURVE_WITH_KNOTS ( 'NONE', 3,
 ( #100651, #107408, #31809, #65998, #49733, #21726, #14988, #82204, #13331, #66549, #55928, #5510, #39666, #109087, #81644, #107961, #49185, #23937, #31258, #74940, #32368, #83314, #40212, #30704, #74392, #91165, #14440, #6610, #108518, #58132, #47522, #64890, #98997, #22274, #93361, #86622, #16626, #85501, #25596, #84953 ),
 .UNSPECIFIED., .F., .F.,
 ( 4, 3, 3, 3, 3, 3, 3, 3, 3, 3, 3, 3, 3, 4 ),
 ( -10.41361588720000064, -10.13063035700000114, -9.847644826829998976, -9.281676235200000846, -8.963578704315109391, -8.116477003980460125, -7.172239364826979546, -6.079724662395450174, -4.751561961960000247, -3.666469461290509990, -2.567348413909280147, -1.622951925397099870, -0.7893940661170741890, 0.000000000000000000 ),
 .UNSPECIFIED. ) ;
#8700 = ORIENTED_EDGE ( 'NONE', *, *, #104366, .F. ) ;
#8699 = CYLINDRICAL_SURFACE ( 'NONE', #105167, 1.999999999999998668 ) ;
#8701 = VERTEX_POINT ( 'NONE', #100831 ) ;
#8702 = CARTESIAN_POINT ( 'NONE',  ( -19.83859993069999916, 1467.194195006989958, 209.1218459616989946 ) ) ;
#8703 = AXIS2_PLACEMENT_3D ( 'NONE', #5623, #31913, #90714 ) ;
#8704 = CARTESIAN_POINT ( 'NONE',  ( 7.540337753453409064, 1510.559702729411583, 203.3485307114503655 ) ) ;
#8705 = CARTESIAN_POINT ( 'NONE',  ( -0.4790278571090000326, 1472.619496933330083, 270.3713665238979615 ) ) ;
#8706 = DIRECTION ( 'NONE',  ( -1.836970198721029688E-16, -1.000000000000000000, -1.314768175368352060E-31 ) ) ;
#8708 = EDGE_CURVE ( 'NONE', #43597, #77376, #58399, .T. ) ;
#8707 = CARTESIAN_POINT ( 'NONE',  ( -120.3440751137400042, 1358.631207110790001, 304.2218459572590064 ) ) ;
#8709 = CARTESIAN_POINT ( 'NONE',  ( 15.55054316549999882, 1408.913060387329779, 199.4537366391079729 ) ) ;
#8710 = CARTESIAN_POINT ( 'NONE',  ( -2.758550930766380027, 1475.074343013350017, 198.0237746611490195 ) ) ;
#8711 = CARTESIAN_POINT ( 'NONE',  ( 22.65427326300000033, 1411.066072244829911, 206.6969470652379925 ) ) ;
#8712 = CARTESIAN_POINT ( 'NONE',  ( -22.81156273906369947, 1507.439214557219884, 208.2956905222379760 ) ) ;
#8713 = CARTESIAN_POINT ( 'NONE',  ( 9.798927948586740655, 1367.783618483544160, 210.6218459617030021 ) ) ;
#8714 = CARTESIAN_POINT ( 'NONE',  ( 6.465563136336550443, 1408.607608635380075, 196.5438154157149881 ) ) ;
#8715 = CARTESIAN_POINT ( 'NONE',  ( -18.72589922193079914, 1409.005224371739814, 266.8215888940370064 ) ) ;
#8716 = CARTESIAN_POINT ( 'NONE',  ( -13.80919631936640002, 1435.007083571719932, 148.9152799103790130 ) ) ;
#8717 = VERTEX_POINT ( 'NONE', #109268 ) ;
#8718 = DIRECTION ( 'NONE',  ( 0.000000000000000000, 0.000000000000000000, 1.000000000000000000 ) ) ;
#8719 = CARTESIAN_POINT ( 'NONE',  ( 13.41370794949999912, 1444.653901271769882, 188.3548391028979836 ) ) ;
#8720 = ORIENTED_EDGE ( 'NONE', *, *, #81624, .F. ) ;
#8721 = ORIENTED_EDGE ( 'NONE', *, *, #24671, .F. ) ;
#8722 = CARTESIAN_POINT ( 'NONE',  ( 4.695345900855497412, 1422.169280887841296, 184.1494170363840510 ) ) ;
#8723 = CARTESIAN_POINT ( 'NONE',  ( -21.83550407203936672, 1523.678648413191695, 183.2743720722710634 ) ) ;
#8724 = CIRCLE ( 'NONE', #26634, 1.999999999999997780 ) ;
#8725 = CARTESIAN_POINT ( 'NONE',  ( -3.449149233875000053, 1516.947419719950176, 213.7456339395970133 ) ) ;
#8726 = CARTESIAN_POINT ( 'NONE',  ( -17.41752696329999850, 1470.470948016929924, 189.2590027405980209 ) ) ;
#8727 = CARTESIAN_POINT ( 'NONE',  ( -16.26545371259889805, 1479.765189095689948, 229.1142011118929815 ) ) ;
#8728 = ORIENTED_EDGE ( 'NONE', *, *, #95396, .F. ) ;
#8729 = CARTESIAN_POINT ( 'NONE',  ( -113.4000000000000057, 1375.342264060499929, 302.0293834673589686 ) ) ;
#8730 = CARTESIAN_POINT ( 'NONE',  ( -3.899071993169999590E-16, 1420.943991414029824, 172.2701767054979882 ) ) ;
#8731 = CARTESIAN_POINT ( 'NONE',  ( -5.008848238024999233, 1516.858456333729919, 204.1217621043670079 ) ) ;
#8732 = CARTESIAN_POINT ( 'NONE',  ( -27.69670323179999727, 1508.056852025029912, 205.9292566894080210 ) ) ;
#8733 = CARTESIAN_POINT ( 'NONE',  ( -0.7321517276410000052, 1477.822672531229955, 230.6006906680979966 ) ) ;
#8734 = CARTESIAN_POINT ( 'NONE',  ( -47.74144289124880203, 1384.610046507420066, 221.9457723244100009 ) ) ;
#8735 = CARTESIAN_POINT ( 'NONE',  ( -2.867472949620000211, 1409.013194749230024, 194.6181666647979966 ) ) ;
#8736 = CARTESIAN_POINT ( 'NONE',  ( -28.25086642335310216, 1508.135711581739997, 208.8579954535609886 ) ) ;
#8738 = ORIENTED_EDGE ( 'NONE', *, *, #23524, .T. ) ;
#8737 = DIRECTION ( 'NONE',  ( 0.3363363969981701951, -0.9417419115948324482, 0.000000000000000000 ) ) ;
#8739 = CARTESIAN_POINT ( 'NONE',  ( -27.33099940864819999, 1488.742651603209879, 209.9611524475739941 ) ) ;
#8740 = CARTESIAN_POINT ( 'NONE',  ( 23.31685688550000179, 1508.124115173030077, 223.0011395122980105 ) ) ;
#8741 = LINE ( 'NONE', #76510, #58085 ) ;
#8742 = CARTESIAN_POINT ( 'NONE',  ( 19.02702702808590018, 1456.914964676220052, 225.6710515766719993 ) ) ;
#8743 = CARTESIAN_POINT ( 'NONE',  ( -4.802229637768189896, 1508.551704408389924, 204.6920723467030143 ) ) ;
#8744 = CARTESIAN_POINT ( 'NONE',  ( -5.771149113014999443, 1516.616791731099966, 211.6102065995370083 ) ) ;
#8745 = VECTOR ( 'NONE', #16992, 1000.000000000000114 ) ;
#8746 = CARTESIAN_POINT ( 'NONE',  ( -68.67770101600000032, 1379.747952267379787, 279.9599199388590023 ) ) ;
#8747 = CARTESIAN_POINT ( 'NONE',  ( -15.03087568459999979, 1418.003645312529898, 226.9475657730980060 ) ) ;
#8748 = CARTESIAN_POINT ( 'NONE',  ( 9.001872265064569945, 1479.644900270570133, 227.9349562530539970 ) ) ;
#8749 = CARTESIAN_POINT ( 'NONE',  ( 6.944466742375000834, 1516.939530130779985, 209.1105810159089913 ) ) ;
#8750 = VERTEX_POINT ( 'NONE', #32552 ) ;
#8751 = CARTESIAN_POINT ( 'NONE',  ( -36.37832876729999754, 1435.767865857450261, 134.0999984849980251 ) ) ;
#8752 = CARTESIAN_POINT ( 'NONE',  ( -11.50267440360000037, 1412.829103654730034, 228.8848828364980079 ) ) ;
#8753 = CARTESIAN_POINT ( 'NONE',  ( -25.94018854349999970, 1385.115782246259869, 224.2425052717590006 ) ) ;
#8754 = EDGE_LOOP ( 'NONE', ( #39377, #41102, #105605, #72609 ) ) ;
#8755 = CARTESIAN_POINT ( 'NONE',  ( -13.02200731483190133, 1385.301542061540204, 219.0627894650050109 ) ) ;
#8756 = AXIS2_PLACEMENT_3D ( 'NONE', #9855, #50756, #51874 ) ;
#8758 = ORIENTED_EDGE ( 'NONE', *, *, #67838, .F. ) ;
#8757 = CARTESIAN_POINT ( 'NONE',  ( -11.75527373628579930, 1491.528794388550068, 205.5782633857490111 ) ) ;
#8759 = CARTESIAN_POINT ( 'NONE',  ( 12.65519453621029911, 1434.571286974429995, 149.4915664245209825 ) ) ;
#8760 = B_SPLINE_SURFACE_WITH_KNOTS ( 'NONE', 5, 1, ( 
 ( #100559, #92710 ),
 ( #110071, #67542 ),
 ( #84847, #83029 ),
 ( #108223, #89771 ),
 ( #108778, #57310 ),
 ( #73547, #13042 ) ),
 .UNSPECIFIED., .F., .F., .F.,
 ( 6, 6 ),
 ( 2, 2 ),
 ( -9.032913087590760002E-05, 17.14253593653090135 ),
 ( 0.000000000000000000, 14.00009032913090046 ),
 .UNSPECIFIED. ) ;
#8761 = CARTESIAN_POINT ( 'NONE',  ( 6.041208603222500528, 1459.296510909109884, 233.3208609013059913 ) ) ;
#8762 = CARTESIAN_POINT ( 'NONE',  ( -23.63758762339999819, 1509.747673043829991, 226.8389689203980026 ) ) ;
#8763 = CARTESIAN_POINT ( 'NONE',  ( -21.62164173379369814, 1522.051704408389924, 210.2163513719069954 ) ) ;
#8764 = LINE ( 'NONE', #60300, #25103 ) ;
#8765 = CARTESIAN_POINT ( 'NONE',  ( 9.698064461892839105, 1462.705242386489999, 208.0596150282290182 ) ) ;
#8767 = CARTESIAN_POINT ( 'NONE',  ( 6.826200034800000260, 1424.874072630889941, 213.4902541782590220 ) ) ;
#8766 = CARTESIAN_POINT ( 'NONE',  ( 4.620008207075000151, 1516.777260590120022, 214.8964555921769772 ) ) ;
#8768 = CARTESIAN_POINT ( 'NONE',  ( 19.94909480960000181, 1508.591193236829895, 188.8781692952979938 ) ) ;
#8769 = CARTESIAN_POINT ( 'NONE',  ( -5.003848160104999998, 1517.005755693489846, 216.4561742428970206 ) ) ;
#8770 = VERTEX_POINT ( 'NONE', #5704 ) ;
#8771 = CARTESIAN_POINT ( 'NONE',  ( -16.65468421539999966, 1420.515480522079770, 203.5047434824589914 ) ) ;
#8772 = ORIENTED_EDGE ( 'NONE', *, *, #89921, .T. ) ;
#8773 = CIRCLE ( 'NONE', #71429, 14.91144628110000170 ) ;
#8774 = CARTESIAN_POINT ( 'NONE',  ( 19.30423710177419849, 1493.475036102569902, 199.7216101148530072 ) ) ;
#8775 = AXIS2_PLACEMENT_3D ( 'NONE', #91608, #23832, #48525 ) ;
#8776 = CARTESIAN_POINT ( 'NONE',  ( -8.493714061740000432, 1509.017688834789851, 209.4777728399689920 ) ) ;
#8777 = CARTESIAN_POINT ( 'NONE',  ( 2.622430729442982944, 1523.621879633028584, 176.0901726876731175 ) ) ;
#8778 = UNCERTAINTY_MEASURE_WITH_UNIT (LENGTH_MEASURE( 1.000000000000000082E-05 ), #93807, 'distance_accuracy_value', 'NONE');
#8779 = CARTESIAN_POINT ( 'NONE',  ( -7.544963895292410072, 1384.924630418719971, 219.0875845435980125 ) ) ;
#8780 = CARTESIAN_POINT ( 'NONE',  ( -34.68852446352314445, 1522.861859112239244, 199.9946320047847053 ) ) ;
#8781 = CARTESIAN_POINT ( 'NONE',  ( 22.96901158543816734, 1519.551704408389924, 206.5493031772561778 ) ) ;
#8782 = CARTESIAN_POINT ( 'NONE',  ( 17.34090440699278091, 1422.638053189401944, 226.6050307785843074 ) ) ;
#8783 = CARTESIAN_POINT ( 'NONE',  ( 6.225972109890000716, 1494.795958560490135, 219.7811165620990153 ) ) ;
#8784 = CARTESIAN_POINT ( 'NONE',  ( -7.254007743607123970, 1458.163048246020253, 215.3456065187994852 ) ) ;
#8785 = CARTESIAN_POINT ( 'NONE',  ( -7.450897614389999646, 1442.756953654919926, 149.7755488681980012 ) ) ;
#8786 = CARTESIAN_POINT ( 'NONE',  ( 42.65467180383260626, 1440.913060353519995, 262.7680395952199888 ) ) ;
#8788 = CARTESIAN_POINT ( 'NONE',  ( -19.70594995229999924, 1434.992946305789928, 207.5825935615879985 ) ) ;
#8787 = CARTESIAN_POINT ( 'NONE',  ( -11.39447792757199984, 1470.674147238439900, 209.5206840692040089 ) ) ;
#8789 = CARTESIAN_POINT ( 'NONE',  ( 11.94174092869224069, 1433.516789646251709, 150.0943515355301088 ) ) ;
#8790 = VERTEX_POINT ( 'NONE', #92432 ) ;
#8791 = DIRECTION ( 'NONE',  ( 0.9942586961433753645, 0.000000000000000000, -0.1070030146457356945 ) ) ;
#8792 = CARTESIAN_POINT ( 'NONE',  ( 32.37018134260395641, 1511.187213306747708, 200.1723992780595438 ) ) ;
#8793 = CARTESIAN_POINT ( 'NONE',  ( -4.326992699989999913, 1515.158586642889986, 209.4787185339210112 ) ) ;
#8794 = DIRECTION ( 'NONE',  ( -0.6736849260863837507, 0.000000000000000000, 0.7390186874254154326 ) ) ;
#8795 = CARTESIAN_POINT ( 'NONE',  ( 11.79002570591860000, 1447.121451514569799, 187.8029540059399949 ) ) ;
#8796 = TOROIDAL_SURFACE ( 'NONE', #3487, 1.000000000000000000, 1.000000000000000000 ) ;
#8797 = B_SPLINE_SURFACE_WITH_KNOTS ( 'NONE', 5, 5, ( 
 ( #9139, #69626, #95351, #85271, #42741, #76902 ),
 ( #68513, #102611, #43301, #1867, #52811, #86943 ),
 ( #94793, #60109, #36001, #77451, #26473, #60667 ),
 ( #77993, #35439, #70192, #98500, #22319, #3927 ),
 ( #73874, #100162, #74436, #4463, #108562, #99592 ),
 ( #99041, #91207, #21768, #14489, #55969, #73315 ) ),
 .UNSPECIFIED., .F., .F., .F.,
 ( 6, 6 ),
 ( 6, 6 ),
 ( 30.36509140000000073, 167.7881597310000075 ),
 ( 0.000000000000000000, 2.000000000000000000 ),
 .UNSPECIFIED. ) ;
#8798 = CARTESIAN_POINT ( 'NONE',  ( -4.636493443397069036, 1378.021649596855468, 203.9344422422949776 ) ) ;
#8799 = CARTESIAN_POINT ( 'NONE',  ( -4.226426730560000067, 1515.477082009289916, 209.1218459617439862 ) ) ;
#8801 = EDGE_CURVE ( 'NONE', #17951, #82950, #110035, .T. ) ;
#8800 = CARTESIAN_POINT ( 'NONE',  ( -57.43579072256620321, 1383.800285040919789, 276.0605554277290139 ) ) ;
#8802 = FACE_OUTER_BOUND ( 'NONE', #12727, .T. ) ;
#8803 = CARTESIAN_POINT ( 'NONE',  ( -27.40792122765466132, 1509.298960328587327, 212.0799651120152589 ) ) ;
#8804 = CARTESIAN_POINT ( 'NONE',  ( -19.66678637246580053, 1521.951704408389787, 215.8936635744080093 ) ) ;
#8806 = VERTEX_POINT ( 'NONE', #31993 ) ;
#8805 = CARTESIAN_POINT ( 'NONE',  ( 10.53451941872170039, 1452.171317966529841, 208.4890148705030128 ) ) ;
#8807 = CARTESIAN_POINT ( 'NONE',  ( -1.383993012750000196, 1414.983771848930019, 226.4898643371980143 ) ) ;
#8808 = CARTESIAN_POINT ( 'NONE',  ( -43.68437696189999997, 1382.328028760530287, 247.2103273439589941 ) ) ;
#8809 = CARTESIAN_POINT ( 'NONE',  ( -3.430374836980000008, 1431.708658569990121, 216.7924588047190184 ) ) ;
#8810 = EDGE_CURVE ( 'NONE', #106272, #105229, #63629, .T. ) ;
#8811 = ORIENTED_EDGE ( 'NONE', *, *, #22923, .T. ) ;
#8812 = ORIENTED_EDGE ( 'NONE', *, *, #35253, .T. ) ;
#8813 = DIRECTION ( 'NONE',  ( 0.000000000000000000, 0.000000000000000000, 1.000000000000000000 ) ) ;
#8814 = CARTESIAN_POINT ( 'NONE',  ( 38.29511879756229575, 1438.902673677490156, 136.6303356394320190 ) ) ;
#8816 = CARTESIAN_POINT ( 'NONE',  ( 2.472529913803022783, 1523.678648413191695, 175.3762130535718597 ) ) ;
#8815 = DIRECTION ( 'NONE',  ( -1.000000000000000000, 1.836970198721029688E-16, 0.000000000000000000 ) ) ;
#8817 = CARTESIAN_POINT ( 'NONE',  ( 11.76014171143800091, 1479.338753478690023, 208.6264959333659874 ) ) ;
#8818 = CARTESIAN_POINT ( 'NONE',  ( -109.6762195290000079, 1383.310342075810013, 297.1796156746589759 ) ) ;
#8819 = CARTESIAN_POINT ( 'NONE',  ( -12.59663421299888952, 1435.821309450346234, 150.9177216549062450 ) ) ;
#8820 = CARTESIAN_POINT ( 'NONE',  ( -19.08445480129999794, 1440.913060387330006, 209.8212738029720299 ) ) ;
#8821 = CARTESIAN_POINT ( 'NONE',  ( 3.513330320889999747, 1409.035748585529973, 186.9170200111979625 ) ) ;
#8822 = CARTESIAN_POINT ( 'NONE',  ( -0.2329096773732799996, 1486.060289406110087, 197.2204110355460216 ) ) ;
#8823 = CARTESIAN_POINT ( 'NONE',  ( 9.975222784249348607, 1470.060250684319954, 210.5865425885360196 ) ) ;
#8824 = CARTESIAN_POINT ( 'NONE',  ( -9.197582055050311567, 1449.962432854769986, 209.3192927283980111 ) ) ;
#8825 = CARTESIAN_POINT ( 'NONE',  ( -15.54139885464740090, 1421.077970550840064, 203.4236906915260192 ) ) ;
#8826 = VECTOR ( 'NONE', #70650, 1000.000000000000114 ) ;
#8827 = CARTESIAN_POINT ( 'NONE',  ( -1.816161586769259983, 1450.477603230480099, 183.3762537591580042 ) ) ;
#8828 = CARTESIAN_POINT ( 'NONE',  ( 1.769009636590000101, 1464.859476624029867, 237.2742850304979925 ) ) ;
#8829 = EDGE_LOOP ( 'NONE', ( #7924, #71453, #21652, #26337, #109582, #20371, #31744, #38232, #57977 ) ) ;
#8830 = CARTESIAN_POINT ( 'NONE',  ( 22.14279220764339939, 1473.984090239060151, 210.1089564727559775 ) ) ;
#8831 = CARTESIAN_POINT ( 'NONE',  ( -41.96992763659999781, 1449.933563106350221, 270.3374075954979503 ) ) ;
#8832 = CARTESIAN_POINT ( 'NONE',  ( -26.13694927001759893, 1446.561492601239934, 138.0017901643740004 ) ) ;
#8833 =( BOUNDED_SURFACE ( )  B_SPLINE_SURFACE ( 1, 2, ( 
 ( #25020, #25573, #16067, #7687, #34544, #16605, #33422, #42391, #50802 ),
 ( #77120, #83297, #426, #15516, #17154, #110151, #49713, #74917, #109067 ) ),
 .UNSPECIFIED., .F., .T., .F. ) 
 B_SPLINE_SURFACE_WITH_KNOTS ( ( 2, 2 ),
 ( 3, 2, 2, 2, 3 ),
 ( -10000.00000000000000, 10000.00000000000000 ),
 ( 0.000000000000000000, 1.570796326794899889, 3.141592653589790007, 4.712388980384689674, 6.283185307179590673 ),
 .UNSPECIFIED. ) 
 GEOMETRIC_REPRESENTATION_ITEM ( )  RATIONAL_B_SPLINE_SURFACE ( (
 ( 1.000000000000000000, 0.7071067811865480168, 1.000000000000000000, 0.7071067811865480168, 1.000000000000000000, 0.7071067811865480168, 1.000000000000000000, 0.7071067811865480168, 1.000000000000000000),
 ( 1.000000000000000000, 0.7071067811865480168, 1.000000000000000000, 0.7071067811865480168, 1.000000000000000000, 0.7071067811865480168, 1.000000000000000000, 0.7071067811865480168, 1.000000000000000000) ) ) 
 REPRESENTATION_ITEM ( '' )  SURFACE ( )  );
#8834 = DIRECTION ( 'NONE',  ( -0.9455185755993178454, 0.000000000000000000, 0.3255681544571537578 ) ) ;
#8835 = CARTESIAN_POINT ( 'NONE',  ( 16.93412905219999942, 1468.808412830429916, 189.7276331636979876 ) ) ;
#8836 = VECTOR ( 'NONE', #64356, 1000.000000000000227 ) ;
#8837 = CARTESIAN_POINT ( 'NONE',  ( -6.910112620815310491E-10, 1470.927955446970145, 256.4164964148890249 ) ) ;
#8838 = CARTESIAN_POINT ( 'NONE',  ( 20.51249426540298515, 1436.445542391833442, 144.8792686586828040 ) ) ;
#8839 = CARTESIAN_POINT ( 'NONE',  ( -1.362314668290000030, 1416.021639799829927, 227.8893587007979988 ) ) ;
#8840 = CARTESIAN_POINT ( 'NONE',  ( -8.457611602209999191, 1419.058770192229986, 232.4533566405980025 ) ) ;
#8841 = CARTESIAN_POINT ( 'NONE',  ( -0.8775662281799990749, 1477.001762535890066, 198.7462694420989919 ) ) ;
#8842 = CARTESIAN_POINT ( 'NONE',  ( -108.6169391080000111, 1387.815304053930049, 310.5755581212589505 ) ) ;
#8843 = CARTESIAN_POINT ( 'NONE',  ( -8.248023465271721477, 1511.495156305270029, 214.8261723429600067 ) ) ;
#8844 = CARTESIAN_POINT ( 'NONE',  ( 1.904758451061700386, 1358.442897800721767, 209.6218459617033432 ) ) ;
#8845 = CARTESIAN_POINT ( 'NONE',  ( -45.69545081991040547, 1437.710744842920121, 266.4180560666800375 ) ) ;
#8846 = CARTESIAN_POINT ( 'NONE',  ( 1.435735496894300134, 1429.431631213589981, 217.3000859563380232 ) ) ;
#8847 = AXIS2_PLACEMENT_3D ( 'NONE', #39162, #40824, #107471 ) ;
#8848 = CARTESIAN_POINT ( 'NONE',  ( -8.075931970399999216, 1424.985315206749874, 206.4140305923890253 ) ) ;
#8849 = ORIENTED_EDGE ( 'NONE', *, *, #2404, .F. ) ;
#8850 = CARTESIAN_POINT ( 'NONE',  ( -2.297629659184999618, 1516.970035769810011, 208.3868227339359862 ) ) ;
#8851 = CARTESIAN_POINT ( 'NONE',  ( -5.388310285459999349, 1432.653871653890064, 154.6144347680979934 ) ) ;
#8852 = CARTESIAN_POINT ( 'NONE',  ( -25.98561794621749854, 1441.261220175949802, 138.2899389286700114 ) ) ;
#8853 = CARTESIAN_POINT ( 'NONE',  ( 7.538390275667609330, 1425.596513388789845, 212.1820638689150087 ) ) ;
#8854 = AXIS2_PLACEMENT_3D ( 'NONE', #84412, #56601, #67086 ) ;
#8855 = CARTESIAN_POINT ( 'NONE',  ( -26.74532466102600026, 1451.223413308900035, 136.2813698317930005 ) ) ;
#8856 = EDGE_LOOP ( 'NONE', ( #15872, #105713, #5822, #106759 ) ) ;
#8857 = CARTESIAN_POINT ( 'NONE',  ( 29.14244744279999821, 1435.145987126659975, 238.0755329184979985 ) ) ;
#8859 = CARTESIAN_POINT ( 'NONE',  ( -14.90569725764700060, 1513.941944659479987, 223.9356467521019738 ) ) ;
#8858 = CARTESIAN_POINT ( 'NONE',  ( -3.261946504277382086, 1524.739563915922190, 176.4690228988872320 ) ) ;
#8860 = CARTESIAN_POINT ( 'NONE',  ( 4.616899834755000320, 1517.050041317280147, 201.3993091674070115 ) ) ;
#8861 = CARTESIAN_POINT ( 'NONE',  ( 27.78452742954910093, 1508.000976259739900, 207.7754991261529938 ) ) ;
#8862 = CARTESIAN_POINT ( 'NONE',  ( 2.589235753919999445E-16, 1524.551704408390151, 209.1218459616989946 ) ) ;
#8863 = CARTESIAN_POINT ( 'NONE',  ( -17.60627563539920004, 1410.895669414250051, 194.0661810348550205 ) ) ;
#8864 = CARTESIAN_POINT ( 'NONE',  ( -25.19103893129999960, 1437.530664664930100, 138.0353914523980166 ) ) ;
#8865 = ORIENTED_EDGE ( 'NONE', *, *, #8257, .T. ) ;
#8866 = CARTESIAN_POINT ( 'NONE',  ( -8.677567137620060933, 1408.534241456209884, 270.2786540372579793 ) ) ;
#8867 = CARTESIAN_POINT ( 'NONE',  ( 10.82050651005049957, 1419.935650953779941, 231.8985719784330115 ) ) ;
#8868 = DIRECTION ( 'NONE',  ( 0.3188159025760192167, 6.661338147751048295E-13, -0.9478166596260261256 ) ) ;
#8870 = ORIENTED_EDGE ( 'NONE', *, *, #11242, .F. ) ;
#8869 = CARTESIAN_POINT ( 'NONE',  ( -2.500000000000360156, 1439.188135388240198, 158.6514568555039943 ) ) ;
#8871 = VERTEX_POINT ( 'NONE', #66727 ) ;
#8872 = CARTESIAN_POINT ( 'NONE',  ( -23.19576873519860172, 1410.004524903090214, 210.0850936017089907 ) ) ;
#8873 = CARTESIAN_POINT ( 'NONE',  ( -10.68991641760000100, 1481.192726480790043, 208.4620359433729959 ) ) ;
#8874 = CARTESIAN_POINT ( 'NONE',  ( -2.923521517025829741, 1410.394928878200062, 186.6127595807840009 ) ) ;
#8875 = TOROIDAL_SURFACE ( 'NONE', #71529, 4.250000000000000000, 0.5000000000000000000 ) ;
#8876 = CARTESIAN_POINT ( 'NONE',  ( -44.28110705741969610, 1432.290621434800414, 266.2283975843345729 ) ) ;
#8877 = CARTESIAN_POINT ( 'NONE',  ( -18.28401409811200296, 1419.983726780179722, 194.9665186433740018 ) ) ;
#8878 = CARTESIAN_POINT ( 'NONE',  ( -19.57049444700000151, 1420.832488470329963, 222.7981928031980203 ) ) ;
#8879 = CARTESIAN_POINT ( 'NONE',  ( 40.86771873664179822, 1456.647620516569987, 268.9064048513220087 ) ) ;
#8880 = ADVANCED_FACE ( 'NONE', ( #7883 ), #99522, .F. ) ;
#8881 = CARTESIAN_POINT ( 'NONE',  ( -11.66261279208220181, 1391.913060387180167, 208.8812267457540202 ) ) ;
#8882 = CARTESIAN_POINT ( 'NONE',  ( -3.710825910270000083, 1429.315763641489866, 201.5588532669389963 ) ) ;
#8883 = CARTESIAN_POINT ( 'NONE',  ( 1.702754371344999962, 1517.014196759610059, 205.6580786742169948 ) ) ;
#8884 = ORIENTED_EDGE ( 'NONE', *, *, #69223, .F. ) ;
#8885 = CARTESIAN_POINT ( 'NONE',  ( -11.81944340819999972, 1433.674010844490113, 150.7526810563979893 ) ) ;
#8886 = CARTESIAN_POINT ( 'NONE',  ( 15.21196346850829961, 1512.378201925219855, 196.1437262287770125 ) ) ;
#8887 = CARTESIAN_POINT ( 'NONE',  ( -6.501609782144663896, 1522.051704408389924, 200.8207946853451631 ) ) ;
#8888 = ORIENTED_EDGE ( 'NONE', *, *, #30536, .T. ) ;
#8890 = VECTOR ( 'NONE', #109631, 1000.000000000000000 ) ;
#8889 = CARTESIAN_POINT ( 'NONE',  ( -1.205637028059169946, 1458.002444675669949, 229.8765855511719849 ) ) ;
#8891 = EDGE_CURVE ( 'NONE', #50916, #13762, #628, .T. ) ;
#8892 = CARTESIAN_POINT ( 'NONE',  ( 24.88318342085590018, 1452.039007177160101, 135.7900169370240064 ) ) ;
#8893 = EDGE_CURVE ( 'NONE', #86228, #53112, #16636, .T. ) ;
#8894 = CARTESIAN_POINT ( 'NONE',  ( -2.801140078490090168, 1508.551704408389924, 214.0906714726369842 ) ) ;
#8895 = CARTESIAN_POINT ( 'NONE',  ( -1.311629847093230189E-15, 1388.651670832440004, 217.0323832392490147 ) ) ;
#8896 = B_SPLINE_CURVE_WITH_KNOTS ( 'NONE', 5,
 ( #35803, #69984, #53742, #26276, #45328, #79467 ),
 .UNSPECIFIED., .F., .F.,
 ( 6, 6 ),
 ( -106.8619706870000101, -30.32814661860000172 ),
 .UNSPECIFIED. ) ;
#8897 = CARTESIAN_POINT ( 'NONE',  ( 7.367316997829999714, 1422.547007707180001, 195.5834347947990182 ) ) ;
#8899 = B_SPLINE_SURFACE_WITH_KNOTS ( 'NONE', 5, 5, ( 
 ( #25670, #77757, #69937, #59863, #25116, #51446 ),
 ( #93988, #61528, #60417, #104051, #1066, #17809 ),
 ( #95656, #60981, #102927, #9442, #18923, #86149 ),
 ( #43606, #68280, #517, #53121, #87258, #85577 ),
 ( #44724, #78876, #8324, #102388, #36297, #69379 ),
 ( #70490, #43057, #59320, #35194, #17254, #93432 ) ),
 .UNSPECIFIED., .F., .F., .F.,
 ( 6, 6 ),
 ( 6, 6 ),
 ( 4.807626846469999826, 6.388845116620970543 ),
 ( 0.000000000000000000, 1.432659768743509865 ),
 .UNSPECIFIED. ) ;
#8898 = CARTESIAN_POINT ( 'NONE',  ( 16.85557976710000005, 1409.501670203030017, 194.3276026113979924 ) ) ;
#8900 = CARTESIAN_POINT ( 'NONE',  ( -3.671863939699999690, 1495.492710535389961, 197.3513011073989958 ) ) ;
#8901 = CARTESIAN_POINT ( 'NONE',  ( 0.2331202188386839735, 1408.921201124740037, 186.4825399812679905 ) ) ;
#8903 = CARTESIAN_POINT ( 'NONE',  ( -19.53786426058999481, 1522.382868172863937, 236.7197124308268030 ) ) ;
#8902 = CARTESIAN_POINT ( 'NONE',  ( 30.77259778570388704, 1524.972383263453366, 196.5524048554408409 ) ) ;
#8904 = CARTESIAN_POINT ( 'NONE',  ( -16.48231778833706684, 1525.661275128775287, 181.5746610185808834 ) ) ;
#8905 = CARTESIAN_POINT ( 'NONE',  ( 9.833393186232889605, 1517.051704408389924, 205.7359371553449989 ) ) ;
#8906 = CARTESIAN_POINT ( 'NONE',  ( -12.04245058450000094, 1377.963961494360092, 211.7131635816590176 ) ) ;
#8907 = CARTESIAN_POINT ( 'NONE',  ( 3.036227701980231508, 1369.423328382213640, 207.6218459616989378 ) ) ;
#8908 = ORIENTED_EDGE ( 'NONE', *, *, #48641, .T. ) ;
#8909 = CARTESIAN_POINT ( 'NONE',  ( -32.22536377336284374, 1523.621879633028584, 201.4085774011532806 ) ) ;
#8910 = DIRECTION ( 'NONE',  ( -0.3090169943749383474, 0.000000000000000000, 0.9510565162951566398 ) ) ;
#8911 = CARTESIAN_POINT ( 'NONE',  ( -109.0150999517360049, 1384.924420285359929, 311.2646967347890268 ) ) ;
#8912 = B_SPLINE_CURVE_WITH_KNOTS ( 'NONE', 3,
 ( #69563, #44344, #25291, #103682, #59493, #42128, #61172, #51633, #68449, #102552, #7961, #94725, #25845, #60047 ),
 .UNSPECIFIED., .F., .F.,
 ( 4, 2, 2, 2, 2, 2, 4 ),
 ( 0.000000000000000000, 0.2500000000000193179, 0.5000000000000386358, 0.6250000000000289768, 0.7500000000000193179, 0.8750000000000096589, 1.000000000000000000 ),
 .UNSPECIFIED. ) ;
#8913 = B_SPLINE_SURFACE_WITH_KNOTS ( 'NONE', 5, 5, ( 
 ( #43827, #70722, #104834, #60091, #96438, #25892, #103726, #18592, #51680 ),
 ( #190, #10781, #26454, #34312, #28121, #62314, #95880, #86370, #103152 ),
 ( #69052, #52790, #19716, #9117, #19142, #35982, #78535, #53349, #731 ),
 ( #9655, #94206, #2409, #10215, #35421, #53919, #27029, #68492, #88053 ),
 ( #44393, #1846, #43281, #1280, #102592, #44954, #94771, #77430, #76880 ),
 ( #87494, #77974, #61217, #34863, #95332, #70172, #104283, #79100, #36526 ) ),
 .UNSPECIFIED., .F., .F., .F.,
 ( 6, 6 ),
 ( 6, 3, 6 ),
 ( 25.26539776070000087, 42.22154025839999747 ),
 ( 0.000000000000000000, 1.000000000000000000, 2.000000000000000000 ),
 .UNSPECIFIED. ) ;
#8914 = CARTESIAN_POINT ( 'NONE',  ( -11.02152004010000041, 1388.222241134549904, 201.9217105854090164 ) ) ;
#8915 = CARTESIAN_POINT ( 'NONE',  ( 8.331628387504050437, 1425.215661044880108, 210.8086245623740069 ) ) ;
#8916 = CARTESIAN_POINT ( 'NONE',  ( -35.77265797339989462, 1450.098916315730094, 136.2386353496389688 ) ) ;
#8917 = CARTESIAN_POINT ( 'NONE',  ( -10.90853107422250012, 1462.746370323140127, 207.3438040333890058 ) ) ;
#8918 = FACE_OUTER_BOUND ( 'NONE', #22344, .T. ) ;
#8919 = AXIS2_PLACEMENT_3D ( 'NONE', #74998, #109147, #74451 ) ;
#8920 = CARTESIAN_POINT ( 'NONE',  ( -8.941769890295299561, 1384.291477174050215, 218.6298190130140142 ) ) ;
#8921 = CARTESIAN_POINT ( 'NONE',  ( 11.87922074009999918, 1433.306015784339934, 150.2908134751979787 ) ) ;
#8922 = CARTESIAN_POINT ( 'NONE',  ( 13.21926163380000041, 1460.466222979229997, 248.0989693098979956 ) ) ;
#8923 = B_SPLINE_SURFACE_WITH_KNOTS ( 'NONE', 5, 5, ( 
 ( #95875, #19713, #44951, #19140, #79098, #94769 ),
 ( #88051, #69606, #37072, #3498, #87492, #96436 ),
 ( #53345, #43824, #10779, #71269, #80183, #103724 ),
 ( #45508, #28679, #28117, #62311, #103150, #36524 ),
 ( #27026, #46051, #70718, #27569, #2407, #11880 ),
 ( #61752, #37625, #26452, #11336, #60645, #18046 ) ),
 .UNSPECIFIED., .F., .F., .F.,
 ( 6, 6 ),
 ( 6, 6 ),
 ( 55.36927774709999994, 55.41785034089999584 ),
 ( 0.000000000000000000, 2.000000000000000000 ),
 .UNSPECIFIED. ) ;
#8924 = CARTESIAN_POINT ( 'NONE',  ( 12.61115941410569974, 1416.521607925270018, 196.2004978253030174 ) ) ;
#8925 = EDGE_CURVE ( 'NONE', #77302, #83385, #53046, .T. ) ;
#8926 = CARTESIAN_POINT ( 'NONE',  ( 18.27002674530000093, 1430.510071776790028, 200.9389885209290014 ) ) ;
#8927 = AXIS2_PLACEMENT_3D ( 'NONE', #105724, #2724, #20036 ) ;
#8928 = CARTESIAN_POINT ( 'NONE',  ( 11.16314367537479946, 1421.171381915769871, 200.1196691949539854 ) ) ;
#8929 = CARTESIAN_POINT ( 'NONE',  ( 6.531329447192200099, 1466.275421158679819, 216.6368425205710082 ) ) ;
#8930 = CARTESIAN_POINT ( 'NONE',  ( 22.71803131159999722, 1409.706390560829959, 209.2188350014689888 ) ) ;
#8931 = CARTESIAN_POINT ( 'NONE',  ( 11.89222639830229156, 1398.265657350177207, 214.3730992004363713 ) ) ;
#8932 = CARTESIAN_POINT ( 'NONE',  ( -30.01282678429459594, 1510.000041106939989, 208.7873087230510123 ) ) ;
#8933 = AXIS2_PLACEMENT_3D ( 'NONE', #6540, #38479, #64265 ) ;
#8934 = CARTESIAN_POINT ( 'NONE',  ( 18.41411251730000131, 1430.349327995130125, 223.8639151150979956 ) ) ;
#8935 = CARTESIAN_POINT ( 'NONE',  ( 1.644415622395181353, 1478.048958850599092, 198.8242942082682418 ) ) ;
#8936 = CARTESIAN_POINT ( 'NONE',  ( -41.53484662709239927, 1442.119007197383553, 135.5124903905762892 ) ) ;
#8937 = CARTESIAN_POINT ( 'NONE',  ( -1.842963900900000063, 1515.551704191689851, 205.2922257884789872 ) ) ;
#8938 = CARTESIAN_POINT ( 'NONE',  ( 16.48401273470000206, 1408.913060387329779, 216.3372448727180313 ) ) ;
#8939 = CARTESIAN_POINT ( 'NONE',  ( 16.50821395286810045, 1494.476688879279891, 193.0250025734499957 ) ) ;
#8940 = CARTESIAN_POINT ( 'NONE',  ( -2.285487619494999567, 1517.001127920769704, 213.1661676502270097 ) ) ;
#8941 = B_SPLINE_CURVE_WITH_KNOTS ( 'NONE', 5,
 ( #109382, #101488, #69048, #16376, #49476, #41053, #94204, #67390, #83598 ),
 .UNSPECIFIED., .F., .F.,
 ( 6, 3, 6 ),
 ( 0.000000000000000000, 0.5000001178084170217, 1.000000000000000000 ),
 .UNSPECIFIED. ) ;
#8942 = CARTESIAN_POINT ( 'NONE',  ( -18.95612632361009631, 1419.023425851569982, 208.8707427548719977 ) ) ;
#8943 = CARTESIAN_POINT ( 'NONE',  ( 0.1654384182819229887, 1483.018567707959846, 181.9647163855690053 ) ) ;
#8945 = ORIENTED_EDGE ( 'NONE', *, *, #64378, .T. ) ;
#8944 = CARTESIAN_POINT ( 'NONE',  ( 3.414905379839999977, 1441.318761073790029, 218.0249493360389863 ) ) ;
#8946 = DIRECTION ( 'NONE',  ( 1.755985294532469921E-16, -1.000000000000000000, 1.338183447452831989E-16 ) ) ;
#8947 = DIRECTION ( 'NONE',  ( 0.000000000000000000, 0.000000000000000000, 1.000000000000000000 ) ) ;
#8948 = CARTESIAN_POINT ( 'NONE',  ( 12.03449236470000017, 1491.353386475389925, 206.6667661057590237 ) ) ;
#8949 = EDGE_CURVE ( 'NONE', #36007, #82949, #56748, .T. ) ;
#8950 = CARTESIAN_POINT ( 'NONE',  ( -31.87595007833786553, 1525.042412244735488, 216.1377694412481674 ) ) ;
#8951 = CARTESIAN_POINT ( 'NONE',  ( -109.8948805359999881, 1384.905360643249878, 297.0284598854590286 ) ) ;
#8952 = ORIENTED_EDGE ( 'NONE', *, *, #84469, .F. ) ;
#8953 = CARTESIAN_POINT ( 'NONE',  ( -5.932239102140000497, 1391.913060387289988, 203.1292509007990077 ) ) ;
#8954 = CARTESIAN_POINT ( 'NONE',  ( -14.44996707430120075, 1380.126493376779763, 208.9404713352460021 ) ) ;
#8955 = CARTESIAN_POINT ( 'NONE',  ( -17.63393957150000091, 1415.931784855930118, 211.9458465498180146 ) ) ;
#8956 = CARTESIAN_POINT ( 'NONE',  ( 13.68046382411920092, 1499.825599652919891, 226.3926818705750179 ) ) ;
#8957 = B_SPLINE_CURVE_WITH_KNOTS ( 'NONE', 3,
 ( #23154, #101503, #42182, #83077, #6370, #86382, #87505, #27041, #77443, #68505, #1861, #53930, #78546, #103741, #61229, #2420 ),
 .UNSPECIFIED., .F., .F.,
 ( 4, 3, 3, 3, 3, 4 ),
 ( 4.019724148039999889, 6.150493503467039602, 8.416124416742510661, 10.70624330608290009, 12.92002759199360007, 13.77031185580000106 ),
 .UNSPECIFIED. ) ;
#8958 = B_SPLINE_CURVE_WITH_KNOTS ( 'NONE', 3,
 ( #62933, #98117, #3554, #89726, #20856, #13001, #81312, #22484, #56684, #14102 ),
 .UNSPECIFIED., .F., .F.,
 ( 4, 2, 2, 2, 4 ),
 ( 0.000000000000000000, 0.0007403986298595412272, 0.001480797259719082454, 0.002221195889578623898, 0.002961594519438164909 ),
 .UNSPECIFIED. ) ;
#8959 = CARTESIAN_POINT ( 'NONE',  ( -6.860676238782120073, 1434.586309434399936, 214.3896270283869967 ) ) ;
#8960 = DIRECTION ( 'NONE',  ( -0.9455185755993178454, 0.000000000000000000, 0.3255681544571537578 ) ) ;
#8961 = VECTOR ( 'NONE', #102574, 1000.000000000000000 ) ;
#8962 = CARTESIAN_POINT ( 'NONE',  ( -17.97414461820000042, 1423.929594390560169, 208.2618829023350031 ) ) ;
#8963 = CARTESIAN_POINT ( 'NONE',  ( -22.75273496409615603, 1512.187213306747481, 183.6728937936775310 ) ) ;
#8964 = CARTESIAN_POINT ( 'NONE',  ( -11.29271012839999955, 1391.598770344190143, 204.5551124859889853 ) ) ;
#8965 = CARTESIAN_POINT ( 'NONE',  ( -86.18995079829420547, 1385.180302516739857, 289.8088348423220282 ) ) ;
#8966 = CARTESIAN_POINT ( 'NONE',  ( -11.61119566721579943, 1391.913060387289988, 210.3328882169209919 ) ) ;
#8967 = CARTESIAN_POINT ( 'NONE',  ( 11.52984783759620058, 1422.027592033300152, 208.2049052604949964 ) ) ;
#8968 = EDGE_LOOP ( 'NONE', ( #93280, #43730, #95274, #90349 ) ) ;
#8969 = CARTESIAN_POINT ( 'NONE',  ( -15.80810346846800130, 1409.717633941269924, 226.1408703758089871 ) ) ;
#8971 = EDGE_LOOP ( 'NONE', ( #100836, #92993, #66469, #85333 ) ) ;
#8970 = PLANE ( 'NONE',  #41264 ) ;
#8972 = CARTESIAN_POINT ( 'NONE',  ( -19.78987248279999989, 1467.442824718890051, 207.1782906715690160 ) ) ;
#8973 = ORIENTED_EDGE ( 'NONE', *, *, #64103, .F. ) ;
#8974 = CARTESIAN_POINT ( 'NONE',  ( 23.61148526040000206, 1508.482535357130018, 222.5984954199980166 ) ) ;
#8975 = CARTESIAN_POINT ( 'NONE',  ( -9.692061980449999226, 1363.802329763670059, 207.6218459616989946 ) ) ;
#8976 = CARTESIAN_POINT ( 'NONE',  ( 10.47043688597563182, 1517.051704408389924, 197.0050518223378333 ) ) ;
#8977 = VECTOR ( 'NONE', #45922, 1000.000000000000000 ) ;
#8978 = CARTESIAN_POINT ( 'NONE',  ( 35.43993441567700131, 1457.286910017509399, 269.5376372890260654 ) ) ;
#8979 = CARTESIAN_POINT ( 'NONE',  ( 15.90990255763500016, 1512.830284628050094, 198.1616908427670296 ) ) ;
#8980 = CARTESIAN_POINT ( 'NONE',  ( 18.99548197422359763, 1437.728065295126953, 213.2617020504292498 ) ) ;
#8981 = CARTESIAN_POINT ( 'NONE',  ( 1.624355357520000043, 1415.847779888729974, 232.6127382033980098 ) ) ;
#8982 = CARTESIAN_POINT ( 'NONE',  ( 4.439133174170000196, 1445.351637362389738, 201.2425731753489799 ) ) ;
#8983 = FACE_OUTER_BOUND ( 'NONE', #35747, .T. ) ;
#8984 = CARTESIAN_POINT ( 'NONE',  ( -8.624710350820000926, 1367.191948709370081, 207.6218459616989946 ) ) ;
#8985 = CARTESIAN_POINT ( 'NONE',  ( -2.009517772400000180, 1455.098376589789950, 199.1884203155790090 ) ) ;
#8986 = EDGE_CURVE ( 'NONE', #105450, #67100, #31339, .T. ) ;
#8987 = CARTESIAN_POINT ( 'NONE',  ( 0.7355686427760019797, 1517.012231669750008, 205.8548062402470009 ) ) ;
#8989 = ADVANCED_FACE ( 'NONE', ( #16806 ), #63, .F. ) ;
#8988 = CARTESIAN_POINT ( 'NONE',  ( 3.684086215580000268, 1446.644899200540067, 159.4624503042980166 ) ) ;
#8990 = CARTESIAN_POINT ( 'NONE',  ( -1.776356839399999804E-15, 1414.661898229710005, 209.1218459616989946 ) ) ;
#8991 = CARTESIAN_POINT ( 'NONE',  ( 13.63581072969999930, 1474.110335124630183, 269.6067227616979949 ) ) ;
#8993 = ORIENTED_EDGE ( 'NONE', *, *, #70906, .F. ) ;
#8992 = CARTESIAN_POINT ( 'NONE',  ( -0.01467710756120139959, 1495.315433949589988, 220.4548505147990056 ) ) ;
#8994 = FACE_OUTER_BOUND ( 'NONE', #63743, .T. ) ;
#8995 = EDGE_LOOP ( 'NONE', ( #65890, #56124, #29561, #106090 ) ) ;
#8996 = CARTESIAN_POINT ( 'NONE',  ( -16.78772373697407971, 1513.520094851864087, 222.2831617812080935 ) ) ;
#8997 = CARTESIAN_POINT ( 'NONE',  ( -23.22702229119999728, 1430.350733269630155, 202.9151551450079864 ) ) ;
#8999 = CARTESIAN_POINT ( 'NONE',  ( 17.38493044761679940, 1410.884709072750184, 192.4605050727279831 ) ) ;
#8998 = CARTESIAN_POINT ( 'NONE',  ( -10.74422203838610024, 1424.967024678149983, 139.7076782565099791 ) ) ;
#9000 = CARTESIAN_POINT ( 'NONE',  ( -3.445407572115000150, 1516.764084769670262, 211.4198948937369948 ) ) ;
#9001 = CARTESIAN_POINT ( 'NONE',  ( 28.88831231914572584, 1510.032855735962585, 201.0268679937729530 ) ) ;
#9002 = VECTOR ( 'NONE', #23161, 1000.000000000000114 ) ;
#9003 = CARTESIAN_POINT ( 'NONE',  ( -20.24918891140000099, 1453.165958253630151, 208.5428146401309846 ) ) ;
#9004 = CARTESIAN_POINT ( 'NONE',  ( -12.32239476379200127, 1378.308289425619932, 209.4637424472300040 ) ) ;
#9005 = CARTESIAN_POINT ( 'NONE',  ( 17.48970627280642987, 1459.983305242940560, 228.4052134740612416 ) ) ;
#9006 = ITEM_DEFINED_TRANSFORMATION ( 'NONE', 'NONE', #11032,  #21632 ) ;
#9007 = CARTESIAN_POINT ( 'NONE',  ( 4.106634628316339963, 1508.551704408389924, 213.5130254241009879 ) ) ;
#9008 = CARTESIAN_POINT ( 'NONE',  ( -35.58396791106149948, 1437.290684582510039, 136.5355017401039959 ) ) ;
#9009 = ORIENTED_EDGE ( 'NONE', *, *, #10940, .F. ) ;
#9010 = CARTESIAN_POINT ( 'NONE',  ( 7.539262298278820218, 1397.225239789469924, 197.6719658297510023 ) ) ;
#9011 = CARTESIAN_POINT ( 'NONE',  ( 9.762886224428157789, 1460.688233213919830, 206.5243166130410088 ) ) ;
#9012 = AXIS2_PLACEMENT_3D ( 'NONE', #16795, #50999, #84582 ) ;
#9013 = CARTESIAN_POINT ( 'NONE',  ( -17.43253919180000011, 1460.024831443229914, 228.2391352219980263 ) ) ;
#9014 = VERTEX_POINT ( 'NONE', #1725 ) ;
#9016 = ORIENTED_EDGE ( 'NONE', *, *, #2859, .F. ) ;
#9015 = COLOUR_RGB ( '', 0.40784314, 0.44705882, 0.49803922) ;
#9017 = CARTESIAN_POINT ( 'NONE',  ( -29.26524805770378990, 1509.935219952241368, 211.6937577894515528 ) ) ;
#9018 = CARTESIAN_POINT ( 'NONE',  ( -9.267034430364599729, 1423.582047745190039, 146.9531713541019826 ) ) ;
#9019 = CARTESIAN_POINT ( 'NONE',  ( -14.16245236182539813, 1380.070782178959917, 210.9945578494510130 ) ) ;
#9020 = CARTESIAN_POINT ( 'NONE',  ( -10.88843716487655122, 1417.951816079329774, 198.2287934583217179 ) ) ;
#9021 = EDGE_CURVE ( 'NONE', #43805, #104880, #77316, .T. ) ;
#9022 = AXIS2_PLACEMENT_3D ( 'NONE', #90895, #73009, #100399 ) ;
#9023 = CARTESIAN_POINT ( 'NONE',  ( 156.6846457583332892, 1526.382868172863937, 77.25240589481997233 ) ) ;
#9024 = CARTESIAN_POINT ( 'NONE',  ( -4.487249791936469556, 1509.038615938009798, 212.6094384014929801 ) ) ;
#9025 = FACE_OUTER_BOUND ( 'NONE', #69526, .T. ) ;
#9026 = EDGE_CURVE ( 'NONE', #27470, #42229, #53227, .T. ) ;
#9027 = CARTESIAN_POINT ( 'NONE',  ( 9.970943783957169515, 1451.601728650610085, 207.6130147570040094 ) ) ;
#9028 = FACE_OUTER_BOUND ( 'NONE', #12738, .T. ) ;
#9029 = CARTESIAN_POINT ( 'NONE',  ( -105.9631781526499879, 1384.892373102839883, 296.9815194618109899 ) ) ;
#9030 = ORIENTED_EDGE ( 'NONE', *, *, #64583, .F. ) ;
#9031 = CARTESIAN_POINT ( 'NONE',  ( 0.7376675027960020170, 1517.104497701820037, 203.3349981924270082 ) ) ;
#9032 = CARTESIAN_POINT ( 'NONE',  ( -0.7468175536419978666, 1517.006509894990131, 209.1289748073840258 ) ) ;
#9033 = VERTEX_POINT ( 'NONE', #103034 ) ;
#9035 = EDGE_CURVE ( 'NONE', #101156, #61195, #15440, .T. ) ;
#9034 = CARTESIAN_POINT ( 'NONE',  ( 11.80100415298899996, 1428.281167224610044, 148.2341325577170039 ) ) ;
#9036 = CARTESIAN_POINT ( 'NONE',  ( 3.029820084536003488, 1511.989325512496180, 217.0244469535358576 ) ) ;
#9037 = EDGE_LOOP ( 'NONE', ( #2252, #63462, #110091, #45254 ) ) ;
#9038 = CARTESIAN_POINT ( 'NONE',  ( -13.15726448929999925, 1414.996444518330009, 220.4820292908979980 ) ) ;
#9039 = CARTESIAN_POINT ( 'NONE',  ( 7.053034928242810864, 1429.189209343189987, 215.4664347411579968 ) ) ;
#9040 = DIRECTION ( 'NONE',  ( 0.000000000000000000, 1.000000000000000000, 0.000000000000000000 ) ) ;
#9041 = CARTESIAN_POINT ( 'NONE',  ( -31.64580750758035066, 1523.313115944345554, 221.9353285379001193 ) ) ;
#9042 = CARTESIAN_POINT ( 'NONE',  ( -5.465716833969999300, 1421.576913351030043, 186.4279755057980026 ) ) ;
#9043 = CARTESIAN_POINT ( 'NONE',  ( -7.613833802559419439, 1446.707927629628557, 154.1417109755026331 ) ) ;
#9044 = CARTESIAN_POINT ( 'NONE',  ( -21.62164173379369814, 1522.051704408389924, 210.2163513719069954 ) ) ;
#9045 = CARTESIAN_POINT ( 'NONE',  ( 5.989307772389999229, 1494.629795928590056, 219.4239502688990058 ) ) ;
#9046 = CARTESIAN_POINT ( 'NONE',  ( -37.70074109930000361, 1379.690292948239858, 220.7037071814589808 ) ) ;
#9047 = CARTESIAN_POINT ( 'NONE',  ( -15.62174622799999923, 1462.582522095329978, 223.1630036629979941 ) ) ;
#9048 = EDGE_CURVE ( 'NONE', #50471, #21520, #10100, .T. ) ;
#9050 = DIRECTION ( 'NONE',  ( -0.7074300732568279404, -0.02470400251969399191, -0.7063514732138288510 ) ) ;
#9049 = CARTESIAN_POINT ( 'NONE',  ( 17.80012153870000091, 1459.332523128830189, 228.1679591816979951 ) ) ;
#9051 = CARTESIAN_POINT ( 'NONE',  ( 15.54603130660830068, 1507.439213079509955, 225.8362344188779787 ) ) ;
#9052 = AXIS2_PLACEMENT_3D ( 'NONE', #105947, #29226, #97530 ) ;
#9053 = CARTESIAN_POINT ( 'NONE',  ( -6.328696556262070949, 1422.647538939597780, 139.1419529473191972 ) ) ;
#9054 = B_SPLINE_SURFACE_WITH_KNOTS ( 'NONE', 5, 5, ( 
 ( #99432, #75374, #66973, #23281, #101084, #24382 ),
 ( #57477, #22710, #30594, #64782, #14879, #39551 ),
 ( #98892, #22160, #56360, #90492, #13767, #47951 ),
 ( #73725, #56908, #91041, #82658, #5949, #74276 ),
 ( #52386, #76454, #51254, #77023, #94916, #8683 ),
 ( #27164, #876, #95468, #61348, #18732, #93248 ) ),
 .UNSPECIFIED., .F., .F., .F.,
 ( 6, 6 ),
 ( 6, 6 ),
 ( 44.26078367470000074, 48.30090647720000163 ),
 ( 0.000000000000000000, 2.000000000000000000 ),
 .UNSPECIFIED. ) ;
#9055 = CARTESIAN_POINT ( 'NONE',  ( -0.03226023477341029982, 1410.297896964309984, 185.0217421575940193 ) ) ;
#9056 = ORIENTED_EDGE ( 'NONE', *, *, #43961, .T. ) ;
#9057 = EDGE_CURVE ( 'NONE', #59173, #36566, #25975, .T. ) ;
#9058 = CARTESIAN_POINT ( 'NONE',  ( 18.17529663798200090, 1424.501927100039893, 223.8627669670750038 ) ) ;
#9059 = CARTESIAN_POINT ( 'NONE',  ( -21.08095450300509555, 1525.506916460691400, 234.2045005059986238 ) ) ;
#9060 = CARTESIAN_POINT ( 'NONE',  ( -2.898382840419457818, 1484.352318093022632, 183.3103537128903895 ) ) ;
#9061 = CARTESIAN_POINT ( 'NONE',  ( -14.62523883179999906, 1415.865102022439942, 213.8037711709790187 ) ) ;
#9062 = EDGE_CURVE ( 'NONE', #80364, #48449, #35863, .T. ) ;
#9064 = ORIENTED_EDGE ( 'NONE', *, *, #20118, .F. ) ;
#9063 = CARTESIAN_POINT ( 'NONE',  ( -0.6915095762680909530, 1515.131927850350166, 204.7941551768030308 ) ) ;
#9065 = CARTESIAN_POINT ( 'NONE',  ( 0.9069153359830000038, 1434.997135647769937, 189.4159220886979824 ) ) ;
#9066 = AXIS2_PLACEMENT_3D ( 'NONE', #89631, #98025, #46558 ) ;
#9067 = CARTESIAN_POINT ( 'NONE',  ( -2.140640208939999845, 1508.551704408389924, 220.0635243260990137 ) ) ;
#9068 = CARTESIAN_POINT ( 'NONE',  ( -11.82648314689999935, 1429.505905138129947, 149.6875397860980001 ) ) ;
#9069 = CARTESIAN_POINT ( 'NONE',  ( -5.386185223340929973, 1432.347042777500064, 154.6076275972019971 ) ) ;
#9070 = CARTESIAN_POINT ( 'NONE',  ( 2.915041327195820209, 1446.157008382559980, 199.4325186832650161 ) ) ;
#9071 = EDGE_CURVE ( 'NONE', #77131, #81034, #56940, .T. ) ;
#9072 = CARTESIAN_POINT ( 'NONE',  ( 7.121584085660000341, 1409.161751583630121, 222.2855843900980233 ) ) ;
#9073 = DIRECTION ( 'NONE',  ( -5.980589973904019347E-17, 1.000000000000000000, -1.736889445713099699E-16 ) ) ;
#9074 = CARTESIAN_POINT ( 'NONE',  ( -14.97406874466500071, 1513.863307887919973, 223.8916988856670116 ) ) ;
#9075 = EDGE_CURVE ( 'NONE', #61499, #97372, #94651, .T. ) ;
#9076 = CARTESIAN_POINT ( 'NONE',  ( 13.36463437909999996, 1410.400759883430055, 228.3459572537979909 ) ) ;
#9078 = CARTESIAN_POINT ( 'NONE',  ( -10.85282564929999971, 1480.164835466490103, 213.9155123631190065 ) ) ;
#9077 = CARTESIAN_POINT ( 'NONE',  ( -20.56562140180000142, 1508.015221763929958, 228.3467905896980028 ) ) ;
#9079 = CARTESIAN_POINT ( 'NONE',  ( -2.519788581729999866, 1470.392735159189897, 216.0597033484689860 ) ) ;
#9080 = CARTESIAN_POINT ( 'NONE',  ( 4.608417506514999928, 1516.691389976299888, 206.6316000176769876 ) ) ;
#9081 = CARTESIAN_POINT ( 'NONE',  ( 23.65302801580000036, 1410.800135283929876, 267.0034940390980296 ) ) ;
#9082 = FACE_OUTER_BOUND ( 'NONE', #40093, .T. ) ;
#9083 = ADVANCED_FACE ( 'NONE', ( #27445 ), #6954, .F. ) ;
#9084 = CARTESIAN_POINT ( 'NONE',  ( 18.33825317269999999, 1449.737352364420076, 190.9873845589980021 ) ) ;
#9085 = CARTESIAN_POINT ( 'NONE',  ( -0.2681387158619999433, 1507.638498121229759, 237.3507797630980178 ) ) ;
#9086 = CARTESIAN_POINT ( 'NONE',  ( -15.60330020924029881, 1418.235805516329947, 203.0264043510670149 ) ) ;
#9087 = CARTESIAN_POINT ( 'NONE',  ( -41.15025406726699231, 1443.128258067170009, 136.8582507510139976 ) ) ;
#9088 = CARTESIAN_POINT ( 'NONE',  ( -7.598474438054299895, 1407.528248760620045, 198.4581846281600122 ) ) ;
#9089 = AXIS2_PLACEMENT_3D ( 'NONE', #58599, #92186, #68663 ) ;
#9090 = CARTESIAN_POINT ( 'NONE',  ( -16.16040309870000158, 1417.154526695929917, 206.7693472903190184 ) ) ;
#9091 = CARTESIAN_POINT ( 'NONE',  ( -13.45920590230000080, 1444.312827231819938, 187.2388222693979856 ) ) ;
#9092 = CARTESIAN_POINT ( 'NONE',  ( -16.39250384509999847, 1431.113060387329824, 219.3475551130979966 ) ) ;
#9093 = B_SPLINE_SURFACE_WITH_KNOTS ( 'NONE', 5, 5, ( 
 ( #100123, #109093, #49191, #92820, #84958, #7712 ),
 ( #67649, #91719, #6064, #23407, #48643, #109632 ),
 ( #40217, #74398, #92271, #32375, #110176, #75498 ),
 ( #49740, #16091, #74946, #50298, #31815, #108523 ),
 ( #83867, #66555, #101757, #100659, #14993, #58687 ),
 ( #66003, #84426, #23943, #57598, #40768, #7170 ),
 ( #32905, #83320, #76026, #67098, #41871, #101201 ),
 ( #42418, #24497, #76575, #33448, #82771, #8252 ),
 ( #58139, #6615, #25045, #110727, #59247, #93366 ) ),
 .UNSPECIFIED., .F., .F., .F.,
 ( 6, 3, 6 ),
 ( 6, 6 ),
 ( 3.230686157760149779, 5.552647417019999310, 7.874608676279850172 ),
 ( -0.0004440811798492790030, 2.000000000000000000 ),
 .UNSPECIFIED. ) ;
#9094 = CARTESIAN_POINT ( 'NONE',  ( -8.646868171490730504, 1437.292463641849736, 208.9934304095080222 ) ) ;
#9095 = CARTESIAN_POINT ( 'NONE',  ( -6.040745412617011922, 1457.036252898433759, 228.2768262899412548 ) ) ;
#9096 = EDGE_LOOP ( 'NONE', ( #21527, #43332, #22041, #56274, #86967, #11281, #70964, #12579, #104621, #8811, #66466, #53503, #23609, #20853, #13401 ) ) ;
#9097 = CARTESIAN_POINT ( 'NONE',  ( -2.412416396784999861, 1511.982868782460173, 201.5319981951469970 ) ) ;
#9098 = CARTESIAN_POINT ( 'NONE',  ( -14.86811171559539879, 1409.432266289319841, 210.5260528434040168 ) ) ;
#9099 = CARTESIAN_POINT ( 'NONE',  ( 10.55886014504109838, 1481.314177749799910, 208.6326544899590090 ) ) ;
#9100 = SPHERICAL_SURFACE ( 'NONE', #109916, 2.000000000680000056 ) ;
#9101 = CARTESIAN_POINT ( 'NONE',  ( -14.63733634519999960, 1474.309184518629991, 267.4468043569979727 ) ) ;
#9102 = CARTESIAN_POINT ( 'NONE',  ( -31.25788889088906686, 1523.954924407801172, 196.3501115357356923 ) ) ;
#9103 = CARTESIAN_POINT ( 'NONE',  ( -14.78589604906941624, 1514.559375976630236, 192.8644648269931281 ) ) ;
#9104 = CARTESIAN_POINT ( 'NONE',  ( -24.56423024638272778, 1444.748822478129341, 210.9347104645846116 ) ) ;
#9105 = CARTESIAN_POINT ( 'NONE',  ( -62.97033459889760110, 1384.684685141620093, 285.7574506432820272 ) ) ;
#9106 = CARTESIAN_POINT ( 'NONE',  ( -24.40236318204969379, 1436.401018377404853, 210.7321041510820692 ) ) ;
#9107 = AXIS2_PLACEMENT_3D ( 'NONE', #43754, #9583, #61143 ) ;
#9108 = CARTESIAN_POINT ( 'NONE',  ( -14.22405469409999945, 1409.409775322530095, 225.3473850829980165 ) ) ;
#9109 = CARTESIAN_POINT ( 'NONE',  ( 12.13275115577349972, 1416.073666497539989, 223.4459935694849833 ) ) ;
#9110 = EDGE_CURVE ( 'NONE', #12333, #10428, #15263, .T. ) ;
#9111 = CARTESIAN_POINT ( 'NONE',  ( -26.40673502673280026, 1495.359935024549941, 211.4908345026910013 ) ) ;
#9112 = CARTESIAN_POINT ( 'NONE',  ( 8.648576441527131564, 1470.685138533134250, 214.4961241725896741 ) ) ;
#9113 = CARTESIAN_POINT ( 'NONE',  ( 21.84020450222056908, 1523.382868172864164, 234.9798068779740277 ) ) ;
#9114 = CARTESIAN_POINT ( 'NONE',  ( -23.67432059500000108, 1410.661424214930094, 207.0403095298379981 ) ) ;
#9115 = EDGE_CURVE ( 'NONE', #43749, #7780, #71276, .T. ) ;
#9116 = VECTOR ( 'NONE', #68148, 1000.000000000000114 ) ;
#9117 = CARTESIAN_POINT ( 'NONE',  ( 15.60349182690000092, 1415.087797054229895, 201.7328695000580012 ) ) ;
#9118 = CARTESIAN_POINT ( 'NONE',  ( 13.13561839920526886, 1517.051704408389924, 209.9352119836111683 ) ) ;
#9119 = CARTESIAN_POINT ( 'NONE',  ( 10.47542077232779967, 1481.052741024980151, 207.7774047151940238 ) ) ;
#9120 = CARTESIAN_POINT ( 'NONE',  ( -6.112144431844329873, 1451.758908031599958, 207.3773668546839986 ) ) ;
#9121 = CARTESIAN_POINT ( 'NONE',  ( 11.52930592674979948, 1434.731876196460007, 225.7086000943210138 ) ) ;
#9122 = CARTESIAN_POINT ( 'NONE',  ( -3.945788320325708032, 1515.565606825038003, 210.3713667179344782 ) ) ;
#9123 = CARTESIAN_POINT ( 'NONE',  ( 16.50820874103769853, 1494.476754866449937, 193.0249925670599964 ) ) ;
#9126 = CARTESIAN_POINT ( 'NONE',  ( 10.93238010538601657, 1414.913060581095351, 222.2496003354920333 ) ) ;
#9125 = AXIS2_PLACEMENT_3D ( 'NONE', #43513, #75997, #92794 ) ;
#9124 = CARTESIAN_POINT ( 'NONE',  ( -22.91694383419999781, 1410.643289684830052, 211.0883591864180175 ) ) ;
#9127 = CARTESIAN_POINT ( 'NONE',  ( 11.72537925141179826, 1426.703358321739870, 143.3352947567420017 ) ) ;
#9128 = CYLINDRICAL_SURFACE ( 'NONE', #3956, 2.000000000000003109 ) ;
#9129 = CARTESIAN_POINT ( 'NONE',  ( -10.98820255369999899, 1490.057925297589918, 212.1172194307789880 ) ) ;
#9130 = CARTESIAN_POINT ( 'NONE',  ( 5.964116108761399637, 1447.836085667069938, 200.8032929224230259 ) ) ;
#9131 = CARTESIAN_POINT ( 'NONE',  ( -21.05711716160357838, 1526.748660780343471, 184.6313866553786625 ) ) ;
#9132 = EDGE_CURVE ( 'NONE', #30026, #54321, #54879, .T. ) ;
#9133 = APPLICATION_CONTEXT ( 'automotive_design' ) ;
#9134 = CIRCLE ( 'NONE', #25248, 1.000000000039237946 ) ;
#9135 = CARTESIAN_POINT ( 'NONE',  ( -0.7553264739829980146, 1516.745833913490060, 203.3462208547369983 ) ) ;
#9136 = CARTESIAN_POINT ( 'NONE',  ( -4.295246787833081115, 1398.041196492937843, 221.3918056679002575 ) ) ;
#9137 = CARTESIAN_POINT ( 'NONE',  ( 15.36767543323500007, 1514.414736986979960, 193.7450394534670295 ) ) ;
#9138 = FACE_OUTER_BOUND ( 'NONE', #28278, .T. ) ;
#9139 = CARTESIAN_POINT ( 'NONE',  ( -17.99923967009999970, 1410.894937295029877, 195.2567800406980041 ) ) ;
#9140 = CARTESIAN_POINT ( 'NONE',  ( 6.510813747272850449, 1506.316984162309836, 218.8516934173640323 ) ) ;
#9141 = CARTESIAN_POINT ( 'NONE',  ( 40.85596413570220165, 1446.221434197089820, 136.5631368516420139 ) ) ;
#9143 = ORIENTED_EDGE ( 'NONE', *, *, #10415, .F. ) ;
#9142 = CARTESIAN_POINT ( 'NONE',  ( -61.41519970972449727, 1379.731749473010041, 268.3043120641129917 ) ) ;
#9144 = ORIENTED_EDGE ( 'NONE', *, *, #30536, .F. ) ;
#9145 = CARTESIAN_POINT ( 'NONE',  ( 11.95088893593300128, 1433.527687467219948, 149.9885903255629955 ) ) ;
#9146 = CARTESIAN_POINT ( 'NONE',  ( 27.86052284579999849, 1509.876774252430096, 216.4221030366980187 ) ) ;
#9147 = ORIENTED_EDGE ( 'NONE', *, *, #481, .F. ) ;
#9148 = CARTESIAN_POINT ( 'NONE',  ( 2.522951803030079727E-08, 1397.914279477030050, 222.1218461579910297 ) ) ;
#9149 = CARTESIAN_POINT ( 'NONE',  ( -10.30780163688080009, 1448.538669356370065, 207.8996510353259737 ) ) ;
#9150 = CARTESIAN_POINT ( 'NONE',  ( 3.982959088878939902, 1515.551843419129909, 206.2722828609170165 ) ) ;
#9152 = CARTESIAN_POINT ( 'NONE',  ( 2.409586283469999923, 1426.663880916129983, 144.1938086916980239 ) ) ;
#9151 = CARTESIAN_POINT ( 'NONE',  ( 11.33251049156513623, 1390.913060387289988, 208.6449207241230965 ) ) ;
#9153 = CARTESIAN_POINT ( 'NONE',  ( 18.56073619233890071, 1498.114107680659799, 229.6370383981259806 ) ) ;
#9154 = VECTOR ( 'NONE', #86328, 1000.000000000000114 ) ;
#9155 = ADVANCED_FACE ( 'NONE', ( #12291 ), #42614, .T. ) ;
#9156 = CARTESIAN_POINT ( 'NONE',  ( 3.154888307769999845, 1507.639342598330131, 181.4414887542980068 ) ) ;
#9157 = CARTESIAN_POINT ( 'NONE',  ( -5.061321235330000334, 1415.087745006229852, 192.8151508637980101 ) ) ;
#9158 = CARTESIAN_POINT ( 'NONE',  ( -21.62164173379369814, 1519.551704408389924, 210.2163513719069954 ) ) ;
#9159 = SHAPE_REPRESENTATION_RELATIONSHIP ( 'NONE' , 'NONE' ,  #105979, #89391 ) ;
#9160 = CARTESIAN_POINT ( 'NONE',  ( -4.608146819384999482, 1516.677239312369920, 211.4179708211670174 ) ) ;
#9161 = CARTESIAN_POINT ( 'NONE',  ( 14.34456629291880070, 1416.134159100540046, 196.9681562124789878 ) ) ;
#9162 = CARTESIAN_POINT ( 'NONE',  ( 11.86050315890000029, 1431.927500028019949, 150.3837318091979967 ) ) ;
#9163 = CARTESIAN_POINT ( 'NONE',  ( 6.166911752485000342, 1513.656171171930055, 201.5360455003170159 ) ) ;
#9164 = VERTEX_POINT ( 'NONE', #64387 ) ;
#9165 = CARTESIAN_POINT ( 'NONE',  ( 13.99694514614609808, 1435.072495206890153, 149.0791654432190114 ) ) ;
#9166 = ADVANCED_FACE ( 'NONE', ( #89559 ), #106905, .T. ) ;
#9167 = ORIENTED_EDGE ( 'NONE', *, *, #96517, .F. ) ;
#9168 = ORIENTED_EDGE ( 'NONE', *, *, #76837, .T. ) ;
#9169 = CARTESIAN_POINT ( 'NONE',  ( 12.96262155038025554, 1444.899173449604177, 169.4271127342331908 ) ) ;
#9170 = CARTESIAN_POINT ( 'NONE',  ( -0.4726074384389999938, 1465.085986095130011, 236.9699255896980219 ) ) ;
#9171 = CARTESIAN_POINT ( 'NONE',  ( -8.046540862050292731, 1474.840790622590930, 202.7137200846936196 ) ) ;
#9172 = CARTESIAN_POINT ( 'NONE',  ( -4.034908597844999889, 1517.068717944079935, 216.4577469658269990 ) ) ;
#9173 = CARTESIAN_POINT ( 'NONE',  ( -8.100270648889271285, 1511.553914495710615, 212.8212201628993228 ) ) ;
#9174 = AXIS2_PLACEMENT_3D ( 'NONE', #108504, #98985, #107949 ) ;
#9175 = CARTESIAN_POINT ( 'NONE',  ( -19.05441023136656753, 1442.634723914723963, 210.8671806021638702 ) ) ;
#9176 = CARTESIAN_POINT ( 'NONE',  ( -48.43983358086703106, 1379.682889511459052, 236.6015797132022840 ) ) ;
#9177 = CARTESIAN_POINT ( 'NONE',  ( 5.063121802906949550E-14, 1380.105522877180192, 207.5503168488490076 ) ) ;
#9178 =( BOUNDED_CURVE ( )  B_SPLINE_CURVE ( 3, ( #74524, #101886, #76706, #40894 ),
 .UNSPECIFIED., .F., .F. ) 
 B_SPLINE_CURVE_WITH_KNOTS ( ( 4, 4 ),
 ( 6.031750314274309410, 6.430153894057509589 ),
 .UNSPECIFIED. ) 
 CURVE ( )  GEOMETRIC_REPRESENTATION_ITEM ( )  RATIONAL_B_SPLINE_CURVE ( ( 1.000000000000000000, 0.9868165636486558867, 0.9868165636486558867, 1.000000000000000000 ) ) 
 REPRESENTATION_ITEM ( '' )  );
#9179 = B_SPLINE_CURVE_WITH_KNOTS ( 'NONE', 3,
 ( #26257, #86177, #9469, #41002, #43634, #78332, #1643 ),
 .UNSPECIFIED., .F., .F.,
 ( 4, 3, 4 ),
 ( -89.14624201249999658, -56.86225756220769512, -20.47911906334890375 ),
 .UNSPECIFIED. ) ;
#9180 = ORIENTED_EDGE ( 'NONE', *, *, #94626, .F. ) ;
#9181 = CARTESIAN_POINT ( 'NONE',  ( -4.043366258305000294, 1516.951766529250108, 206.2549880390970145 ) ) ;
#9182 = ORIENTED_EDGE ( 'NONE', *, *, #12447, .T. ) ;
#9183 = CARTESIAN_POINT ( 'NONE',  ( 19.84271301760869832, 1440.913060387330006, 215.4053540786730139 ) ) ;
#9184 = FACE_OUTER_BOUND ( 'NONE', #30103, .T. ) ;
#9185 = ADVANCED_FACE ( 'NONE', ( #19592 ), #100805, .F. ) ;
#9186 = ORIENTED_EDGE ( 'NONE', *, *, #15352, .T. ) ;
#9187 = CARTESIAN_POINT ( 'NONE',  ( -5.555854370870000558, 1409.107075097130291, 188.5359587977980027 ) ) ;
#9188 = CARTESIAN_POINT ( 'NONE',  ( 7.181020144905000180, 1512.881909847370025, 216.0859015499169971 ) ) ;
#9190 = EDGE_LOOP ( 'NONE', ( #3813, #84021, #28525, #19183 ) ) ;
#9189 = CARTESIAN_POINT ( 'NONE',  ( -11.24049413600000058, 1414.988015881329829, 195.7612515219979912 ) ) ;
#9191 = CARTESIAN_POINT ( 'NONE',  ( 21.58388069929999986, 1429.957715527830032, 219.4703653642980044 ) ) ;
#9192 = CARTESIAN_POINT ( 'NONE',  ( -15.59788086836899978, 1508.551704408389924, 210.3719525949329920 ) ) ;
#9193 = B_SPLINE_CURVE_WITH_KNOTS ( 'NONE', 5,
 ( #11023, #95024, #54154, #62569, #19960, #9365 ),
 .UNSPECIFIED., .F., .F.,
 ( 6, 6 ),
 ( 0.000000000000000000, 1.000000000000000000 ),
 .UNSPECIFIED. ) ;
#9194 = CARTESIAN_POINT ( 'NONE',  ( 19.66678637211940028, 1521.951704408389787, 202.3500283489059939 ) ) ;
#9195 = DIRECTION ( 'NONE',  ( -0.8672669759446666182, 0.000000000000000000, -0.4978433412588673113 ) ) ;
#9196 = ADVANCED_FACE ( 'NONE', ( #49781 ), #7219, .F. ) ;
#9197 = CARTESIAN_POINT ( 'NONE',  ( 19.55988977460000200, 1474.636381753090063, 214.0184790771390055 ) ) ;
#9199 = CARTESIAN_POINT ( 'NONE',  ( -4.032397940005000514, 1516.981965530290154, 214.9074288837770155 ) ) ;
#9198 = STYLED_ITEM ( 'NONE', ( #94942 ), #110798 ) ;
#9200 = EDGE_CURVE ( 'NONE', #42647, #23415, #12230, .T. ) ;
#9201 = CARTESIAN_POINT ( 'NONE',  ( -2.620874085839509871, 1429.130643781209983, 200.1242597526310192 ) ) ;
#9202 = CARTESIAN_POINT ( 'NONE',  ( -8.456465142934458612, 1517.151704408390060, 195.1434824822571841 ) ) ;
#9203 = CARTESIAN_POINT ( 'NONE',  ( -7.722171335595510833, 1517.036116044630262, 208.7506064649060136 ) ) ;
#9204 = CARTESIAN_POINT ( 'NONE',  ( 5.788436334164999586, 1517.116049120239950, 211.4102033778369787 ) ) ;
#9205 = CARTESIAN_POINT ( 'NONE',  ( 2.375285482014719999E-15, 1391.913060387289988, 209.1218459572589836 ) ) ;
#9206 = VECTOR ( 'NONE', #65941, 1000.000000000000000 ) ;
#9207 = CARTESIAN_POINT ( 'NONE',  ( -18.13278339737094669, 1486.179330754719786, 188.5833977309001739 ) ) ;
#9209 = VERTEX_POINT ( 'NONE', #58181 ) ;
#9208 = CARTESIAN_POINT ( 'NONE',  ( -96.40267507759999432, 1388.053540364059927, 309.6952036672590225 ) ) ;
#9210 = CARTESIAN_POINT ( 'NONE',  ( -61.96478079158669772, 1385.056723827129872, 284.1920504743239917 ) ) ;
#9211 = CARTESIAN_POINT ( 'NONE',  ( 34.21123855309999584, 1452.338600522630031, 254.6787333579979986 ) ) ;
#9212 = CARTESIAN_POINT ( 'NONE',  ( 3.524967334472002278, 1450.792428028305494, 184.0702269475962680 ) ) ;
#9213 = CARTESIAN_POINT ( 'NONE',  ( -11.79165762230000070, 1429.416862815430022, 146.4064176768980019 ) ) ;
#9214 = CARTESIAN_POINT ( 'NONE',  ( -8.160870615792729765, 1509.019321687440197, 236.3691303609340082 ) ) ;
#9215 = EDGE_CURVE ( 'NONE', #106390, #59861, #28790, .T. ) ;
#9216 = CARTESIAN_POINT ( 'NONE',  ( -23.83643911649999936, 1446.361787448990071, 213.8673211433680024 ) ) ;
#9217 = CIRCLE ( 'NONE', #98637, 7.500000000000000000 ) ;
#9219 = CARTESIAN_POINT ( 'NONE',  ( 17.27890247157979786, 1409.608338727829960, 222.4184771258499893 ) ) ;
#9218 = DIRECTION ( 'NONE',  ( -0.7067700363771035610, 0.03085824620770448445, 0.7067700363771036720 ) ) ;
#9220 = CARTESIAN_POINT ( 'NONE',  ( -10.32568877401340224, 1448.475227332080067, 208.0351690947539964 ) ) ;
#9221 = CARTESIAN_POINT ( 'NONE',  ( -108.9104367519260137, 1382.394069908770007, 310.7972601483250514 ) ) ;
#9222 = ORIENTED_EDGE ( 'NONE', *, *, #46216, .F. ) ;
#9223 = CARTESIAN_POINT ( 'NONE',  ( 0.7376675027960020170, 1517.104497701820037, 203.3349981924270082 ) ) ;
#9224 = CARTESIAN_POINT ( 'NONE',  ( -11.86647391014470010, 1508.441731521209931, 217.8507656475659928 ) ) ;
#9225 = EDGE_CURVE ( 'NONE', #33248, #66491, #48837, .T. ) ;
#9226 = CARTESIAN_POINT ( 'NONE',  ( 27.70374302159999758, 1507.991978481930119, 207.6872388016580260 ) ) ;
#9227 = CARTESIAN_POINT ( 'NONE',  ( 12.70878548640000005, 1419.800077408030120, 223.4159102764979821 ) ) ;
#9228 = CARTESIAN_POINT ( 'NONE',  ( 5.387463376540000404, 1432.539377501929948, 154.6119119043980277 ) ) ;
#9229 = CARTESIAN_POINT ( 'NONE',  ( -4.363122647530000009, 1423.854802298929826, 178.2623905312979957 ) ) ;
#9230 = CARTESIAN_POINT ( 'NONE',  ( -20.35720354223120054, 1509.285576857579827, 188.5733128882430094 ) ) ;
#9231 = AXIS2_PLACEMENT_3D ( 'NONE', #86726, #23230, #75324 ) ;
#9232 = CARTESIAN_POINT ( 'NONE',  ( 33.30036996651080017, 1435.821070638500032, 135.9642379680810222 ) ) ;
#9233 = CARTESIAN_POINT ( 'NONE',  ( 36.78992615597000082, 1449.659024602699901, 136.2786194408189715 ) ) ;
#9234 = CARTESIAN_POINT ( 'NONE',  ( -41.27798004816977340, 1455.501545579069443, 269.0951446923482990 ) ) ;
#9235 = CARTESIAN_POINT ( 'NONE',  ( -110.0482598020000040, 1385.373316571109854, 296.9711117078589950 ) ) ;
#9236 = DIRECTION ( 'NONE',  ( 0.000000000000000000, 1.000000000000000000, 0.000000000000000000 ) ) ;
#9237 = CARTESIAN_POINT ( 'NONE',  ( -21.15380500792108975, 1525.425686270225015, 183.9878966353793146 ) ) ;
#9238 = CARTESIAN_POINT ( 'NONE',  ( 10.10004869885203682, 1411.254281879943164, 137.0999999980979851 ) ) ;
#9239 = ORIENTED_EDGE ( 'NONE', *, *, #33959, .T. ) ;
#9240 = CARTESIAN_POINT ( 'NONE',  ( -6.832964021560000489, 1409.413060387330006, 271.1218459616979999 ) ) ;
#9241 = CARTESIAN_POINT ( 'NONE',  ( 3.560575673166030075, 1456.106869275790132, 219.1309344377709749 ) ) ;
#9242 = CARTESIAN_POINT ( 'NONE',  ( -4.369728397509249795, 1508.879004046169939, 213.2412249928949848 ) ) ;
#9243 = CARTESIAN_POINT ( 'NONE',  ( 16.84953930043489834, 1504.811272959099824, 188.1836725605500078 ) ) ;
#9244 = CARTESIAN_POINT ( 'NONE',  ( 11.01434323564089546, 1425.013952765832983, 138.3678689716161614 ) ) ;
#9246 = CARTESIAN_POINT ( 'NONE',  ( 31.03088476499726411, 1523.982201850120191, 196.3745419238240686 ) ) ;
#9245 = CARTESIAN_POINT ( 'NONE',  ( 11.40024098090000138, 1502.471351942989941, 210.6161612907290248 ) ) ;
#9247 = DIRECTION ( 'NONE',  ( 0.5030436214085290958, 0.000000000000000000, 0.8642610224695965737 ) ) ;
#9248 = DIRECTION ( 'NONE',  ( 0.000000000000000000, 0.000000000000000000, -1.000000000000000000 ) ) ;
#9249 = DIRECTION ( 'NONE',  ( -4.212667542703050259E-16, 6.855153903361010419E-22, -1.000000000000000000 ) ) ;
#9250 = AXIS2_PLACEMENT_3D ( 'NONE', #52199, #76835, #51089 ) ;
#9251 = CARTESIAN_POINT ( 'NONE',  ( -13.22973741984542784, 1419.796952795795278, 228.0648478904874139 ) ) ;
#9252 = CARTESIAN_POINT ( 'NONE',  ( -37.66849514949689848, 1445.052233488579986, 137.0436250779820000 ) ) ;
#9253 = CARTESIAN_POINT ( 'NONE',  ( -7.851774706560000539, 1482.164398796690193, 201.8541463733390060 ) ) ;
#9254 = CARTESIAN_POINT ( 'NONE',  ( 24.93943963239999917, 1435.368420818290133, 135.8598268128979782 ) ) ;
#9255 = CARTESIAN_POINT ( 'NONE',  ( -11.04150331276600028, 1396.298638179350064, 208.3126073074500084 ) ) ;
#9256 = ORIENTED_EDGE ( 'NONE', *, *, #66126, .F. ) ;
#9257 = CARTESIAN_POINT ( 'NONE',  ( -17.33055221583169825, 1410.741059433489909, 225.8597740937110245 ) ) ;
#9258 = CARTESIAN_POINT ( 'NONE',  ( -4.440280304591389893, 1489.606077279609735, 216.0962888374899933 ) ) ;
#9259 = ORIENTED_EDGE ( 'NONE', *, *, #91873, .T. ) ;
#9260 = ORIENTED_EDGE ( 'NONE', *, *, #18756, .T. ) ;
#9261 = CARTESIAN_POINT ( 'NONE',  ( -0.1973361429370009967, 1494.452141646590007, 217.5167685628690037 ) ) ;
#9262 = CARTESIAN_POINT ( 'NONE',  ( -15.26295761389349792, 1416.044054022097953, 206.4503499115064926 ) ) ;
#9264 = CARTESIAN_POINT ( 'NONE',  ( 1.250280881337970218, 1456.664103658099975, 219.6692350580109974 ) ) ;
#9263 = CARTESIAN_POINT ( 'NONE',  ( 10.66298931770000102, 1425.717966165029793, 91.92307070169779593 ) ) ;
#9265 = CARTESIAN_POINT ( 'NONE',  ( -10.98202954919999996, 1433.094628001990031, 151.7694013171979748 ) ) ;
#9266 = CARTESIAN_POINT ( 'NONE',  ( -109.9705007746040053, 1384.459140194019938, 311.4363103139680220 ) ) ;
#9267 = CARTESIAN_POINT ( 'NONE',  ( -0.7251570665222378809, 1526.278758871496620, 241.9800489742292484 ) ) ;
#9268 = CARTESIAN_POINT ( 'NONE',  ( 2.740701793870000014, 1426.136123009330049, 188.7843822941989913 ) ) ;
#9269 = FACE_BOUND ( 'NONE', #47033, .T. ) ;
#9270 = CARTESIAN_POINT ( 'NONE',  ( 3.202543372079999617, 1449.460684387319816, 183.9015485015980005 ) ) ;
#9271 = CARTESIAN_POINT ( 'NONE',  ( 9.925983360900000108, 1364.303202023270160, 207.6218459616989946 ) ) ;
#9273 = ORIENTED_EDGE ( 'NONE', *, *, #70145, .T. ) ;
#9272 = CARTESIAN_POINT ( 'NONE',  ( -1.063679629813300442, 1465.068952270626824, 237.9910131846521892 ) ) ;
#9274 = ORIENTED_EDGE ( 'NONE', *, *, #31202, .F. ) ;
#9275 = LINE ( 'NONE', #35566, #1501 ) ;
#9276 = CARTESIAN_POINT ( 'NONE',  ( -21.54678038960369690, 1506.340315034190098, 209.2559991757600244 ) ) ;
#9277 = CARTESIAN_POINT ( 'NONE',  ( 2.658194159920000229E-12, 1471.586156922030113, 269.6149382602980040 ) ) ;
#9278 = CARTESIAN_POINT ( 'NONE',  ( 7.900179536920721723, 1500.382728750624892, 200.8993804518913748 ) ) ;
#9279 = CARTESIAN_POINT ( 'NONE',  ( -3.493700197999999979, 1486.025447731730083, 182.1170718226980227 ) ) ;
#9280 = CARTESIAN_POINT ( 'NONE',  ( -32.28368668151615850, 1524.972383263452684, 201.2030582732907931 ) ) ;
#9281 = CARTESIAN_POINT ( 'NONE',  ( -0.9866390672850040566, 1475.553619744739990, 197.7149975239109949 ) ) ;
#9282 = LINE ( 'NONE', #43994, #26918 ) ;
#9283 = CARTESIAN_POINT ( 'NONE',  ( -22.78047381600000065, 1519.913060387329779, 203.9569696715980172 ) ) ;
#9284 = CARTESIAN_POINT ( 'NONE',  ( 8.653423937779999520, 1367.169888897630017, 207.6218459616989946 ) ) ;
#9285 = CARTESIAN_POINT ( 'NONE',  ( 3.125347622798469782, 1407.037771531689941, 196.1218459610850005 ) ) ;
#9286 = CARTESIAN_POINT ( 'NONE',  ( -12.14280743485850067, 1406.971422057159998, 268.4212961918660199 ) ) ;
#9287 = DIRECTION ( 'NONE',  ( -0.1070030146457285891, 0.000000000000000000, 0.9942586961433760306 ) ) ;
#9288 = ORIENTED_EDGE ( 'NONE', *, *, #54322, .F. ) ;
#9289 = CARTESIAN_POINT ( 'NONE',  ( -11.86572145370000086, 1432.317384755180001, 150.3971827880980072 ) ) ;
#9290 = CARTESIAN_POINT ( 'NONE',  ( 12.96054471030000066, 1446.716588664140090, 188.5511171461979814 ) ) ;
#9291 = ORIENTED_EDGE ( 'NONE', *, *, #29064, .T. ) ;
#9292 = VERTEX_POINT ( 'NONE', #31303 ) ;
#9293 = VECTOR ( 'NONE', #95342, 999.9999999999998863 ) ;
#9294 = CARTESIAN_POINT ( 'NONE',  ( 4.860846556981773148, 1422.361256645696585, 184.3086965326904760 ) ) ;
#9295 = CARTESIAN_POINT ( 'NONE',  ( 3.426613460960000079, 1360.656565846710009, 207.6218459616989946 ) ) ;
#9296 = CARTESIAN_POINT ( 'NONE',  ( 4.040527303974999818, 1516.815231249920089, 213.7327841816070020 ) ) ;
#9297 = CARTESIAN_POINT ( 'NONE',  ( -12.90603589790000072, 1485.480164596930081, 186.0404649208980175 ) ) ;
#9298 = ORIENTED_EDGE ( 'NONE', *, *, #75055, .F. ) ;
#9299 = CARTESIAN_POINT ( 'NONE',  ( -11.49747572423030029, 1414.913060387329779, 197.9009878255399997 ) ) ;
#9300 = CARTESIAN_POINT ( 'NONE',  ( -105.8625943240260057, 1378.913060387430050, 303.4239291982839859 ) ) ;
#9301 = CARTESIAN_POINT ( 'NONE',  ( -7.333070173014999860, 1516.955859323880077, 203.3428461583270064 ) ) ;
#9302 = CIRCLE ( 'NONE', #45062, 1.000000000000009326 ) ;
#9303 = EDGE_CURVE ( 'NONE', #104433, #80324, #43467, .T. ) ;
#9304 = CARTESIAN_POINT ( 'NONE',  ( -28.28536570780000048, 1509.154939129630066, 207.7087783032280015 ) ) ;
#9305 = EDGE_CURVE ( 'NONE', #47913, #38319, #79352, .T. ) ;
#9306 = CARTESIAN_POINT ( 'NONE',  ( 7.861206899714999530, 1512.631076693560090, 221.9328003382670147 ) ) ;
#9307 = CARTESIAN_POINT ( 'NONE',  ( -37.20406409030000106, 1384.574232116320218, 210.1855829817990013 ) ) ;
#9308 = CARTESIAN_POINT ( 'NONE',  ( -56.93619473763489935, 1384.654825375539986, 237.6350669292930036 ) ) ;
#9309 =( BOUNDED_CURVE ( )  B_SPLINE_CURVE ( 2, ( #96032, #68648, #62473 ),
 .UNSPECIFIED., .F., .T. ) 
 B_SPLINE_CURVE_WITH_KNOTS ( ( 3, 3 ),
 ( 0.1572692979053489926, 0.2337410564013850112 ),
 .UNSPECIFIED. ) 
 CURVE ( )  GEOMETRIC_REPRESENTATION_ITEM ( )  RATIONAL_B_SPLINE_CURVE ( ( 1.002044729868130091, 1.002448067003099963, 1.002760198777220113 ) ) 
 REPRESENTATION_ITEM ( '' )  );
#9310 = CARTESIAN_POINT ( 'NONE',  ( -14.47191459792289869, 1379.648775954749908, 208.1784578746709826 ) ) ;
#9311 = CARTESIAN_POINT ( 'NONE',  ( 8.002723364794999128, 1516.551704408390151, 206.0688700356170102 ) ) ;
#9313 = ORIENTED_EDGE ( 'NONE', *, *, #24203, .F. ) ;
#9312 = CARTESIAN_POINT ( 'NONE',  ( -1.757532416683340148, 1451.933574871519795, 184.1885909450070073 ) ) ;
#9314 = CARTESIAN_POINT ( 'NONE',  ( -24.16765274424039944, 1411.086006602699854, 209.4242098710629989 ) ) ;
#9315 = CARTESIAN_POINT ( 'NONE',  ( 27.00673397879999982, 1508.127684930929945, 214.8638446572979888 ) ) ;
#9316 = CARTESIAN_POINT ( 'NONE',  ( 19.96912209102779912, 1487.432069230659863, 226.3893998912439827 ) ) ;
#9317 = CARTESIAN_POINT ( 'NONE',  ( -25.58013815969999882, 1435.410414332659911, 135.7415235870979870 ) ) ;
#9318 = CARTESIAN_POINT ( 'NONE',  ( -7.322105105754999954, 1516.572193931679976, 211.9951753309869957 ) ) ;
#9319 = AXIS2_PLACEMENT_3D ( 'NONE', #50389, #61007, #101850 ) ;
#9320 = CARTESIAN_POINT ( 'NONE',  ( -68.46677781809999885, 1379.747208428909971, 279.4303135323589800 ) ) ;
#9321 = EDGE_CURVE ( 'NONE', #58739, #84614, #29952, .T. ) ;
#9322 = CARTESIAN_POINT ( 'NONE',  ( -6.076016578960000913, 1450.645075640589994, 208.7037629494849966 ) ) ;
#9323 = CARTESIAN_POINT ( 'NONE',  ( -30.11859361092962573, 1525.055402519452173, 221.6904485361513366 ) ) ;
#9324 = CARTESIAN_POINT ( 'NONE',  ( -5.013429394184999666, 1517.123342927159911, 207.9998951881570122 ) ) ;
#9325 = EDGE_LOOP ( 'NONE', ( #32015, #106924, #77408, #2309 ) ) ;
#9326 = CARTESIAN_POINT ( 'NONE',  ( 2.500000000000000000, 1433.874165682790135, 157.5407159993979747 ) ) ;
#9327 = DIRECTION ( 'NONE',  ( 0.02091224828123190022, 0.9990482215818557998, 0.03827961371219716635 ) ) ;
#9328 = AXIS2_PLACEMENT_3D ( 'NONE', #89705, #12986, #47169 ) ;
#9329 = CARTESIAN_POINT ( 'NONE',  ( -59.22773397600000322, 1384.821783028959999, 279.9294092910590166 ) ) ;
#9331 = EDGE_LOOP ( 'NONE', ( #14216, #40534, #21718, #96011 ) ) ;
#9330 = B_SPLINE_CURVE_WITH_KNOTS ( 'NONE', 3,
 ( #33684, #9590, #51065, #66782, #67879, #33139 ),
 .UNSPECIFIED., .F., .F.,
 ( 4, 2, 4 ),
 ( -0.2938203139006840270, -0.1489810209828570098, -1.348803076839377724E-06 ),
 .UNSPECIFIED. ) ;
#9332 = CARTESIAN_POINT ( 'NONE',  ( -15.66293008586210078, 1385.292435055019951, 219.5539821970690184 ) ) ;
#9333 = CARTESIAN_POINT ( 'NONE',  ( -9.983110113756229254, 1492.881261275560064, 201.9487339551459968 ) ) ;
#9334 = CARTESIAN_POINT ( 'NONE',  ( 12.22653077411650102, 1434.139770046449939, 149.8861139874390176 ) ) ;
#9335 = CARTESIAN_POINT ( 'NONE',  ( -4.069613198648311503, 1440.892824350064529, 185.0069551270901229 ) ) ;
#9336 = CARTESIAN_POINT ( 'NONE',  ( -23.79097876124399846, 1507.893941173470012, 222.8398483086459976 ) ) ;
#9337 = CARTESIAN_POINT ( 'NONE',  ( -1.943613794290000030, 1409.147975346630119, 186.8816397165979879 ) ) ;
#9338 = CARTESIAN_POINT ( 'NONE',  ( 0.4346943641293429805, 1517.051704428850144, 201.3992661435559910 ) ) ;
#9339 = CARTESIAN_POINT ( 'NONE',  ( -19.53786426059057746, 1522.382868172863937, 181.5239794925695946 ) ) ;
#9341 = CARTESIAN_POINT ( 'NONE',  ( -3.266559724300000411, 1419.654073176930069, 186.2489323254980036 ) ) ;
#9340 = CARTESIAN_POINT ( 'NONE',  ( 1.713317409674999903, 1516.660388280709867, 213.7298676393670291 ) ) ;
#9342 = CARTESIAN_POINT ( 'NONE',  ( -8.861482052969998691, 1384.950957082100103, 218.6848127019790127 ) ) ;
#9343 = CARTESIAN_POINT ( 'NONE',  ( 0.7526715501680020237, 1516.710624944440042, 216.8354948044169817 ) ) ;
#9344 = ORIENTED_EDGE ( 'NONE', *, *, #22570, .T. ) ;
#9345 = CARTESIAN_POINT ( 'NONE',  ( -1.128757599205000073, 1516.608208975040043, 201.4108789544669946 ) ) ;
#9346 = EDGE_CURVE ( 'NONE', #75555, #49951, #75400, .T. ) ;
#9347 = CARTESIAN_POINT ( 'NONE',  ( -0.7210096769089999746, 1490.513422156730030, 181.4676356941980089 ) ) ;
#9348 = ORIENTED_EDGE ( 'NONE', *, *, #25465, .F. ) ;
#9349 = CARTESIAN_POINT ( 'NONE',  ( 17.00812965271749988, 1492.794527032730002, 195.6196781557690088 ) ) ;
#9350 = CARTESIAN_POINT ( 'NONE',  ( -4.363122647530000009, 1421.971318475729959, 172.2701767054979882 ) ) ;
#9351 = EDGE_CURVE ( 'NONE', #49199, #46121, #60022, .T. ) ;
#9352 = CARTESIAN_POINT ( 'NONE',  ( -103.9882530059674366, 1389.939798169118376, 304.1779183652306529 ) ) ;
#9353 = CARTESIAN_POINT ( 'NONE',  ( 2.993128258680000098, 1442.239305041489843, 217.5960754105989849 ) ) ;
#9354 = CARTESIAN_POINT ( 'NONE',  ( -34.09113935470863055, 1523.429859730330008, 198.4929744671656522 ) ) ;
#9355 = DIRECTION ( 'NONE',  ( -1.000000000000000000, -8.350994020400001099E-15, -2.004238564900000104E-13 ) ) ;
#9356 = CARTESIAN_POINT ( 'NONE',  ( 14.38488119590115488, 1507.535237583830849, 232.5758862642972247 ) ) ;
#9357 = CARTESIAN_POINT ( 'NONE',  ( 11.79165762230000070, 1429.416862815430022, 146.4064176768980019 ) ) ;
#9358 = CARTESIAN_POINT ( 'NONE',  ( 16.14995240670000243, 1471.299568758330224, 195.1298844619979889 ) ) ;
#9359 = CARTESIAN_POINT ( 'NONE',  ( 39.73140103348869445, 1440.913060368030074, 258.9046876989520456 ) ) ;
#9361 = CARTESIAN_POINT ( 'NONE',  ( -2.793439186891359949, 1486.025328193850100, 182.0741020391329812 ) ) ;
#9360 = CARTESIAN_POINT ( 'NONE',  ( 15.27152964737910068, 1506.433683733550197, 193.3098315259690025 ) ) ;
#9362 = CARTESIAN_POINT ( 'NONE',  ( 11.31406713481371362, 1433.949558832472121, 151.5135725724176439 ) ) ;
#9363 = ORIENTED_EDGE ( 'NONE', *, *, #61122, .T. ) ;
#9364 = CARTESIAN_POINT ( 'NONE',  ( 1.556187358146779998, 1415.184612915219986, 191.2576310833790103 ) ) ;
#9365 = CARTESIAN_POINT ( 'NONE',  ( 28.15443155984639745, 1509.896245780209938, 217.4026704617729990 ) ) ;
#9366 = CARTESIAN_POINT ( 'NONE',  ( -27.72455330040000021, 1507.994297257130029, 210.5349572574680224 ) ) ;
#9367 = CARTESIAN_POINT ( 'NONE',  ( 4.060573924520632261, 1410.431253889573782, 186.0508650619275954 ) ) ;
#9368 = CARTESIAN_POINT ( 'NONE',  ( -3.813754118949360894, 1426.014263033397583, 186.0222677740474069 ) ) ;
#9369 = CARTESIAN_POINT ( 'NONE',  ( 2.109961980403928905, 1410.360755918536825, 231.8875558583745828 ) ) ;
#9370 = CARTESIAN_POINT ( 'NONE',  ( -11.23993869538120016, 1470.374453574730069, 210.9407000820530129 ) ) ;
#9371 = CARTESIAN_POINT ( 'NONE',  ( -2.993067780513550158, 1487.214450571009820, 219.9661333581329927 ) ) ;
#9372 = CARTESIAN_POINT ( 'NONE',  ( -16.83567051276560278, 1418.884454701650156, 201.2565205294370116 ) ) ;
#9373 = CARTESIAN_POINT ( 'NONE',  ( -65.51159983505390016, 1383.789895811200040, 289.1595459118140070 ) ) ;
#9374 = CARTESIAN_POINT ( 'NONE',  ( 20.90601844020000044, 1451.753496920530097, 144.3735648103979941 ) ) ;
#9375 = DIRECTION ( 'NONE',  ( 0.000000000000000000, 1.000000000000000000, 0.000000000000000000 ) ) ;
#9376 = CARTESIAN_POINT ( 'NONE',  ( -2.725458657727350076, 1516.549587951120202, 201.4124141148399758 ) ) ;
#9378 = EDGE_LOOP ( 'NONE', ( #36220, #15546, #34385 ) ) ;
#9377 = CARTESIAN_POINT ( 'NONE',  ( 10.52289893411149890, 1452.116717517039888, 208.3553807036720116 ) ) ;
#9379 = CARTESIAN_POINT ( 'NONE',  ( -18.69043176373318715, 1458.332274568611865, 227.3714872367983162 ) ) ;
#9380 = CARTESIAN_POINT ( 'NONE',  ( -79.49322724790000905, 1384.792572819600082, 282.9493281527590511 ) ) ;
#9381 = CARTESIAN_POINT ( 'NONE',  ( -0.4920987264512118320, 1416.537162660588820, 233.7617262382077854 ) ) ;
#9382 = ORIENTED_EDGE ( 'NONE', *, *, #50002, .F. ) ;
#9383 = VERTEX_POINT ( 'NONE', #25650 ) ;
#9384 = CARTESIAN_POINT ( 'NONE',  ( 11.79002570591860000, 1447.121451514569799, 187.8029540059399949 ) ) ;
#9385 = CARTESIAN_POINT ( 'NONE',  ( 18.02093535799999913, 1424.326836137830014, 225.1991050518980160 ) ) ;
#9386 = CARTESIAN_POINT ( 'NONE',  ( 40.27144807147075767, 1443.454046232561950, 137.0977477732117222 ) ) ;
#9388 = CARTESIAN_POINT ( 'NONE',  ( 4.896309118140000471, 1485.934254991190073, 218.7196314378989825 ) ) ;
#9387 = CARTESIAN_POINT ( 'NONE',  ( 19.67719249089999778, 1452.817890304029788, 209.0349214551060015 ) ) ;
#9389 = CARTESIAN_POINT ( 'NONE',  ( 8.561878008634579373, 1436.589096639300124, 208.1469354389350030 ) ) ;
#9390 = CARTESIAN_POINT ( 'NONE',  ( -107.3889684650000049, 1382.148098258449863, 298.1845384890590367 ) ) ;
#9391 = CARTESIAN_POINT ( 'NONE',  ( -0.5697963391879999895, 1450.893162800530263, 181.2886238165980046 ) ) ;
#9392 = DIRECTION ( 'NONE',  ( 0.000000000000000000, 0.000000000000000000, -1.000000000000000000 ) ) ;
#9393 = CARTESIAN_POINT ( 'NONE',  ( 4.000901505650000800, 1409.052774946530008, 187.0792394566980192 ) ) ;
#9394 = CARTESIAN_POINT ( 'NONE',  ( -0.0001187281342228439996, 1508.967929526819944, 179.3767679645770272 ) ) ;
#9395 = CARTESIAN_POINT ( 'NONE',  ( -7.134031852310000588, 1442.025630767510165, 154.4960303242980046 ) ) ;
#9396 = CARTESIAN_POINT ( 'NONE',  ( 11.10313694099999893, 1434.937812064100171, 151.7082819323979948 ) ) ;
#9397 = CARTESIAN_POINT ( 'NONE',  ( -14.65253846807509852, 1421.518381437140079, 203.5747437415320178 ) ) ;
#9398 = AXIS2_PLACEMENT_3D ( 'NONE', #36338, #70531, #71649 ) ;
#9399 = CARTESIAN_POINT ( 'NONE',  ( -2.038535907758979970, 1450.880163189499854, 184.1774945304460118 ) ) ;
#9400 = CARTESIAN_POINT ( 'NONE',  ( 1.358136954149999909, 1466.377669086430160, 235.0851390371979903 ) ) ;
#9401 = ORIENTED_EDGE ( 'NONE', *, *, #110707, .F. ) ;
#9402 = CARTESIAN_POINT ( 'NONE',  ( -13.48707387329999818, 1506.009490401690073, 209.0918298080249826 ) ) ;
#9403 = CARTESIAN_POINT ( 'NONE',  ( -4.284681050939999736, 1482.348681575889941, 231.1486602034989915 ) ) ;
#9404 = CARTESIAN_POINT ( 'NONE',  ( -42.28243328599999273, 1442.407792791449992, 269.8809849862979604 ) ) ;
#9405 = CARTESIAN_POINT ( 'NONE',  ( -26.80104139319950107, 1446.506287351420042, 137.4021342824260046 ) ) ;
#9406 = CARTESIAN_POINT ( 'NONE',  ( 11.89522282729999958, 1434.541161981840105, 151.0452005854980086 ) ) ;
#9407 = CARTESIAN_POINT ( 'NONE',  ( -6.733221321159999384, 1470.315040358090073, 190.1905927392990066 ) ) ;
#9408 = CARTESIAN_POINT ( 'NONE',  ( 4.329338606958539337, 1515.069000070079937, 210.7431442201590244 ) ) ;
#9409 = DIRECTION ( 'NONE',  ( 0.8775825618903714265, 0.000000000000000000, -0.4794255386042053368 ) ) ;
#9410 = CARTESIAN_POINT ( 'NONE',  ( -11.60674135321730027, 1507.508082919659955, 207.5537295141489835 ) ) ;
#9411 = CARTESIAN_POINT ( 'NONE',  ( -7.555873979100000248, 1418.426267280130105, 231.8714557520980009 ) ) ;
#9412 = B_SPLINE_CURVE_WITH_KNOTS ( 'NONE', 3,
 ( #60309, #94428, #17147, #93335 ),
 .UNSPECIFIED., .F., .F.,
 ( 4, 4 ),
 ( 2.359153149548954932E-13, 0.0008464750159282172573 ),
 .UNSPECIFIED. ) ;
#9413 = CARTESIAN_POINT ( 'NONE',  ( -108.8041703540000071, 1388.049276877389957, 310.6816495622589969 ) ) ;
#9414 = CARTESIAN_POINT ( 'NONE',  ( -0.08237014995780950199, 1486.172125964604220, 181.8174796312961803 ) ) ;
#9415 = CARTESIAN_POINT ( 'NONE',  ( -4.977374762485336390, 1359.949827183397247, 207.6218459616987673 ) ) ;
#9416 = CARTESIAN_POINT ( 'NONE',  ( -46.13232427859189499, 1439.830690899319961, 268.2051409423269774 ) ) ;
#9417 = CARTESIAN_POINT ( 'NONE',  ( -3.603587107540000112, 1436.962766753449841, 185.5233392668979775 ) ) ;
#9418 = CARTESIAN_POINT ( 'NONE',  ( -8.131798216469999119, 1423.938023408190020, 210.2346984346590091 ) ) ;
#9419 = ORIENTED_EDGE ( 'NONE', *, *, #81848, .F. ) ;
#9420 = CARTESIAN_POINT ( 'NONE',  ( -2.480427292634999947, 1516.872851364150165, 209.8797317620669673 ) ) ;
#9421 = DIRECTION ( 'NONE',  ( 0.000000000000000000, 0.000000000000000000, 1.000000000000000000 ) ) ;
#9422 = CARTESIAN_POINT ( 'NONE',  ( 19.26390258110135534, 1456.145399297611448, 225.0436448590560587 ) ) ;
#9423 = CARTESIAN_POINT ( 'NONE',  ( 7.534131688341251021, 1425.533913774680059, 212.1852849544380035 ) ) ;
#9424 = CARTESIAN_POINT ( 'NONE',  ( -25.31835743630890079, 1452.013124259819961, 135.5916582954220075 ) ) ;
#9425 = ORIENTED_EDGE ( 'NONE', *, *, #21553, .T. ) ;
#9426 = CARTESIAN_POINT ( 'NONE',  ( -15.00920760809999877, 1488.805759878829804, 193.8727931445979777 ) ) ;
#9428 = CARTESIAN_POINT ( 'NONE',  ( 13.98962170100000080, 1452.815214894029850, 195.1980501640979924 ) ) ;
#9427 = CARTESIAN_POINT ( 'NONE',  ( -2.458536830555473340, 1524.871836253796118, 175.9019916315544094 ) ) ;
#9429 = CARTESIAN_POINT ( 'NONE',  ( 6.768867072198900381, 1426.907320758384230, 213.7789536137680386 ) ) ;
#9430 = CARTESIAN_POINT ( 'NONE',  ( -4.325405441727872002, 1515.219201590508419, 207.2788837474028014 ) ) ;
#9431 = DIRECTION ( 'NONE',  ( 0.000000000000000000, -0.9989866842452286289, 0.04500671839541338370 ) ) ;
#9432 = FACE_OUTER_BOUND ( 'NONE', #80516, .T. ) ;
#9433 = ORIENTED_EDGE ( 'NONE', *, *, #74106, .F. ) ;
#9434 = CARTESIAN_POINT ( 'NONE',  ( -3.016912340155930128, 1409.850859107569931, 270.0717562529079601 ) ) ;
#9435 = CARTESIAN_POINT ( 'NONE',  ( -2.491655763544999846, 1516.977504706749869, 208.3867361609839861 ) ) ;
#9436 = CARTESIAN_POINT ( 'NONE',  ( 4.721853743513210411, 1416.907067146989903, 231.6953472553319955 ) ) ;
#9437 = CARTESIAN_POINT ( 'NONE',  ( -0.2886430721605260930, 1507.883296045167526, 237.4859371806405477 ) ) ;
#9439 = ORIENTED_EDGE ( 'NONE', *, *, #63060, .T. ) ;
#9438 = CARTESIAN_POINT ( 'NONE',  ( -9.209502321770001387, 1366.683160837839978, 207.6218459616989946 ) ) ;
#9440 = ORIENTED_EDGE ( 'NONE', *, *, #54124, .F. ) ;
#9441 = CARTESIAN_POINT ( 'NONE',  ( -22.80095230299680154, 1409.739651980310100, 209.6803998413979855 ) ) ;
#9442 = CARTESIAN_POINT ( 'NONE',  ( -0.5472265402873980333, 1409.436775872690077, 185.2931106816229772 ) ) ;
#9443 = CARTESIAN_POINT ( 'NONE',  ( -22.08523692261532290, 1523.530935881284904, 233.8225055907671788 ) ) ;
#9444 = CARTESIAN_POINT ( 'NONE',  ( -4.665393456780000392, 1427.510941591930077, 123.0297916884979941 ) ) ;
#9445 = CARTESIAN_POINT ( 'NONE',  ( -15.86142964305496328, 1436.287026273651236, 149.0794767532250376 ) ) ;
#9446 = CARTESIAN_POINT ( 'NONE',  ( -17.82322816519999975, 1420.841307626830030, 225.8555466793980031 ) ) ;
#9447 = ADVANCED_FACE ( 'NONE', ( #51988 ), #99825, .T. ) ;
#9448 = CARTESIAN_POINT ( 'NONE',  ( 29.93888874088349894, 1467.326863092750045, 268.9541358474360209 ) ) ;
#9449 = CARTESIAN_POINT ( 'NONE',  ( -4.904755620210820233, 1466.423659703103340, 234.4687970439992455 ) ) ;
#9450 = CARTESIAN_POINT ( 'NONE',  ( -4.989533930479999491, 1429.437332217889889, 202.3857892670889953 ) ) ;
#9451 = CARTESIAN_POINT ( 'NONE',  ( -3.267291643295000103, 1516.842852731759876, 205.6749038603869906 ) ) ;
#9452 = ORIENTED_EDGE ( 'NONE', *, *, #17385, .F. ) ;
#9453 = DIRECTION ( 'NONE',  ( 0.03489949670250328678, 0.9993908270190956511, -1.802540234690167715E-19 ) ) ;
#9454 = CARTESIAN_POINT ( 'NONE',  ( -6.541070373676360461, 1517.051704644259871, 205.4524592699869743 ) ) ;
#9455 = CARTESIAN_POINT ( 'NONE',  ( 23.52858676739999666, 1410.126050507929904, 208.3803572285970063 ) ) ;
#9456 = ORIENTED_EDGE ( 'NONE', *, *, #45256, .T. ) ;
#9457 = CARTESIAN_POINT ( 'NONE',  ( 2.487921644133460397, 1508.551704408389924, 204.1347675643650348 ) ) ;
#9459 = EDGE_CURVE ( 'NONE', #48606, #17250, #22917, .T. ) ;
#9458 = CARTESIAN_POINT ( 'NONE',  ( 26.74166369658919962, 1451.062954263790061, 136.3717679156470126 ) ) ;
#9460 = CARTESIAN_POINT ( 'NONE',  ( -15.01814846036320006, 1514.214451730469818, 194.3960741685959874 ) ) ;
#9461 = CARTESIAN_POINT ( 'NONE',  ( 12.37893659083640152, 1501.369140013739980, 212.0434529887650115 ) ) ;
#9462 = CARTESIAN_POINT ( 'NONE',  ( 7.500748375389999723, 1423.062354593270129, 195.6521519453989697 ) ) ;
#9463 = CARTESIAN_POINT ( 'NONE',  ( 18.11184817270000025, 1410.042143777230194, 194.0622353138979861 ) ) ;
#9464 = CARTESIAN_POINT ( 'NONE',  ( 27.48389906189999721, 1444.324653571829913, 168.8435737885979790 ) ) ;
#9465 = CARTESIAN_POINT ( 'NONE',  ( 2.927892279132241260, 1439.671353555214864, 184.0067670968116715 ) ) ;
#9467 = CARTESIAN_POINT ( 'NONE',  ( -18.74856935563128957, 1424.596591154755515, 224.6369667799821741 ) ) ;
#9466 = CARTESIAN_POINT ( 'NONE',  ( 29.91208173166741702, 1525.042337199240137, 196.0615906098655898 ) ) ;
#9468 = CARTESIAN_POINT ( 'NONE',  ( 1.211734507026360097, 1452.507822344910210, 183.4303198485629878 ) ) ;
#9469 = CARTESIAN_POINT ( 'NONE',  ( 19.29501924868120000, 1492.614329036100116, 228.8343218840969939 ) ) ;
#9470 = CARTESIAN_POINT ( 'NONE',  ( -9.293841415499999314, 1383.221401683169915, 218.3140282643789760 ) ) ;
#9471 = CARTESIAN_POINT ( 'NONE',  ( 16.68463225900990210, 1445.052233488270076, 162.0935120915889911 ) ) ;
#9472 = EDGE_LOOP ( 'NONE', ( #17245, #79198, #16852, #33950, #105720, #69505, #60397, #79187, #106401 ) ) ;
#9473 = CARTESIAN_POINT ( 'NONE',  ( 12.92134813639719937, 1416.521607925270018, 221.7330053757000030 ) ) ;
#9474 = LINE ( 'NONE', #34121, #89213 ) ;
#9475 = CARTESIAN_POINT ( 'NONE',  ( -0.4819983852477000563, 1409.558626638459828, 232.9244056882299958 ) ) ;
#9476 = CARTESIAN_POINT ( 'NONE',  ( -12.37283350289999895, 1389.341656536749952, 203.7773294880390154 ) ) ;
#9477 = CARTESIAN_POINT ( 'NONE',  ( 0.02783439897821873149, 1421.066780746317590, 193.7160764248625071 ) ) ;
#9478 = CARTESIAN_POINT ( 'NONE',  ( 0.02610324308704914387, 1506.535970896533854, 231.1903710126655653 ) ) ;
#9479 = CARTESIAN_POINT ( 'NONE',  ( -12.48077398090000045, 1459.371347868330076, 243.9198229205979942 ) ) ;
#9480 = CARTESIAN_POINT ( 'NONE',  ( -2.906507337806380153, 1458.419515837879999, 184.4676491233109914 ) ) ;
#9481 = CARTESIAN_POINT ( 'NONE',  ( 11.18751708150000113, 1433.873588989760037, 151.6203832400979934 ) ) ;
#9482 = CARTESIAN_POINT ( 'NONE',  ( 7.553102823739999749, 1458.344558665030036, 234.3916895749979687 ) ) ;
#9483 = CARTESIAN_POINT ( 'NONE',  ( 12.81744069099580052, 1415.938742849230039, 196.5159729447089774 ) ) ;
#9484 = CARTESIAN_POINT ( 'NONE',  ( -9.666683979049999209, 1423.817746360030014, 192.3656247972989775 ) ) ;
#9485 = CARTESIAN_POINT ( 'NONE',  ( 10.94894508182309956, 1424.836538624790137, 201.4990293608930187 ) ) ;
#9486 = CARTESIAN_POINT ( 'NONE',  ( -3.304926999371979868, 1524.538969332612623, 176.3724890512824004 ) ) ;
#9487 = CARTESIAN_POINT ( 'NONE',  ( -13.70191729650000134, 1486.504808716829984, 185.2020610571979944 ) ) ;
#9488 = CARTESIAN_POINT ( 'NONE',  ( 12.63310190591395887, 1398.287565835977830, 206.0545710329436133 ) ) ;
#9489 = CARTESIAN_POINT ( 'NONE',  ( 1.928731171289999935, 1466.614202310529890, 234.5248722603980127 ) ) ;
#9490 = CARTESIAN_POINT ( 'NONE',  ( 22.95381948220000012, 1410.909818696329921, 213.5977567476680008 ) ) ;
#9491 = CARTESIAN_POINT ( 'NONE',  ( 2.499999999999999112, 1447.900700312901108, 170.5263301090720915 ) ) ;
#9492 = CARTESIAN_POINT ( 'NONE',  ( 25.00977876991279913, 1436.598012848749931, 137.9330263815630246 ) ) ;
#9493 = CARTESIAN_POINT ( 'NONE',  ( -12.10555811194709896, 1383.861219994169915, 218.7921266527899888 ) ) ;
#9494 = CARTESIAN_POINT ( 'NONE',  ( -16.61337446934520301, 1463.629612318100044, 220.4655171191939758 ) ) ;
#9495 = CARTESIAN_POINT ( 'NONE',  ( 4.622842844184999578, 1516.901952101700090, 213.1523604828169880 ) ) ;
#9497 =( BOUNDED_CURVE ( )  B_SPLINE_CURVE ( 3, ( #27395, #86756, #61578, #3883 ),
 .UNSPECIFIED., .F., .F. ) 
 B_SPLINE_CURVE_WITH_KNOTS ( ( 4, 4 ),
 ( 4.712388980384689674, 6.283185307179586232 ),
 .UNSPECIFIED. ) 
 CURVE ( )  GEOMETRIC_REPRESENTATION_ITEM ( )  RATIONAL_B_SPLINE_CURVE ( ( 1.000000000000000000, 0.8047378541243649375, 0.8047378541243649375, 1.000000000000000000 ) ) 
 REPRESENTATION_ITEM ( '' )  );
#9496 = CARTESIAN_POINT ( 'NONE',  ( -13.96277354420170091, 1421.421066752219986, 206.6487300726359990 ) ) ;
#9498 = CARTESIAN_POINT ( 'NONE',  ( 8.883945244656709761, 1451.594843122180009, 211.7725949629070215 ) ) ;
#9499 = B_SPLINE_CURVE_WITH_KNOTS ( 'NONE', 5,
 ( #21781, #28008, #71151, #11231, #80067, #89012, #80626, #96323, #106913 ),
 .UNSPECIFIED., .F., .F.,
 ( 6, 3, 6 ),
 ( 0.000000000000000000, 0.5050532947643375792, 1.000000000000000000 ),
 .UNSPECIFIED. ) ;
#9501 = VERTEX_POINT ( 'NONE', #18351 ) ;
#9500 = CARTESIAN_POINT ( 'NONE',  ( 4.124127541549999165, 1440.791920158089852, 218.1322488136489994 ) ) ;
#9502 = CARTESIAN_POINT ( 'NONE',  ( -1.121268592569999889, 1416.831305870130109, 228.0850991587980161 ) ) ;
#9503 = CARTESIAN_POINT ( 'NONE',  ( -16.68463225827361995, 1445.052233488289630, 162.0935120918203154 ) ) ;
#9504 = CARTESIAN_POINT ( 'NONE',  ( -24.68077630836099701, 1437.736159206269804, 210.5119845322900005 ) ) ;
#9505 = CARTESIAN_POINT ( 'NONE',  ( -32.05521452193857357, 1525.253996226948402, 217.0243583754457859 ) ) ;
#9506 = CARTESIAN_POINT ( 'NONE',  ( 20.33509540109970004, 1432.834541216450134, 214.7556705994980177 ) ) ;
#9507 = ORIENTED_EDGE ( 'NONE', *, *, #110602, .F. ) ;
#9508 = CARTESIAN_POINT ( 'NONE',  ( -38.60856581307790236, 1443.613625294319945, 137.1750438966080026 ) ) ;
#9509 = CARTESIAN_POINT ( 'NONE',  ( -13.79678095129150073, 1390.295210315099894, 211.7643565397299881 ) ) ;
#9510 = CARTESIAN_POINT ( 'NONE',  ( -0.5805478584864469660, 1457.956445091640035, 229.5817085807559863 ) ) ;
#9511 = CARTESIAN_POINT ( 'NONE',  ( -2.825698915363265229, 1367.725220571654063, 208.9256954109638968 ) ) ;
#9512 = CARTESIAN_POINT ( 'NONE',  ( -107.7718053235308275, 1380.453959893709680, 309.7418186890203060 ) ) ;
#9513 = CARTESIAN_POINT ( 'NONE',  ( 1.842963787330042180, 1515.551704408389469, 213.0801841379113455 ) ) ;
#9514 = CARTESIAN_POINT ( 'NONE',  ( -12.28855864720000035, 1378.253615876029926, 210.0769071395779974 ) ) ;
#9515 = CARTESIAN_POINT ( 'NONE',  ( -11.54008407269999914, 1391.635629144820086, 205.2048422470390108 ) ) ;
#9516 = CARTESIAN_POINT ( 'NONE',  ( -69.45868144126460209, 1385.109595529130047, 264.7776320710389655 ) ) ;
#9517 = CARTESIAN_POINT ( 'NONE',  ( -17.07255110680000243, 1412.953535666930065, 191.8935328429979847 ) ) ;
#9518 = CARTESIAN_POINT ( 'NONE',  ( 10.42928995599340070, 1426.801324560409967, 208.9238221840179790 ) ) ;
#9519 = ORIENTED_EDGE ( 'NONE', *, *, #98132, .F. ) ;
#9520 = CARTESIAN_POINT ( 'NONE',  ( -15.69557462584969798, 1410.567954306330194, 226.7002212045480007 ) ) ;
#9522 = ORIENTED_EDGE ( 'NONE', *, *, #65731, .F. ) ;
#9521 = CARTESIAN_POINT ( 'NONE',  ( -0.2285350204260230278, 1437.936383516839896, 227.6814155838589784 ) ) ;
#9523 = CARTESIAN_POINT ( 'NONE',  ( 0.000000000000000000, 1443.913060387330006, 126.8032249175980155 ) ) ;
#9524 = ORIENTED_EDGE ( 'NONE', *, *, #104087, .F. ) ;
#9525 = CARTESIAN_POINT ( 'NONE',  ( 26.60754018289999934, 1509.169817829930025, 216.8086175352880218 ) ) ;
#9526 = CARTESIAN_POINT ( 'NONE',  ( -6.672014541987599578, 1363.744075657580197, 209.6218459617148824 ) ) ;
#9527 = DIRECTION ( 'NONE',  ( -1.755985294532469921E-16, 1.000000000000000000, -1.338183447452831989E-16 ) ) ;
#9528 = DIRECTION ( 'NONE',  ( -0.9786619618251632957, 0.000000000000000000, -0.2054769195713296581 ) ) ;
#9529 = CARTESIAN_POINT ( 'NONE',  ( 13.42479616400980014, 1453.338203267170002, 224.7140346886050111 ) ) ;
#9530 = CARTESIAN_POINT ( 'NONE',  ( 6.170313737849999924, 1397.182081568630110, 220.3579539676979948 ) ) ;
#9531 = DIRECTION ( 'NONE',  ( 1.000000000000000000, 0.000000000000000000, 0.000000000000000000 ) ) ;
#9532 = CARTESIAN_POINT ( 'NONE',  ( -6.951883559441813354, 1516.584123404785487, 211.9369655874735940 ) ) ;
#9533 = DIRECTION ( 'NONE',  ( -0.9455185755993178454, 0.000000000000000000, 0.3255681544571537578 ) ) ;
#9534 = CARTESIAN_POINT ( 'NONE',  ( -8.696701630030000629, 1367.135748871429996, 207.6218459616989946 ) ) ;
#9535 = CARTESIAN_POINT ( 'NONE',  ( -13.29425504400375857, 1516.551188142741921, 225.9939214950833559 ) ) ;
#9536 = CARTESIAN_POINT ( 'NONE',  ( -0.7578858299649979813, 1516.872851364150165, 206.6414186775969881 ) ) ;
#9537 = CARTESIAN_POINT ( 'NONE',  ( 3.123967384229999755, 1446.720974403119953, 162.7331095090980000 ) ) ;
#9538 = CARTESIAN_POINT ( 'NONE',  ( -2.500000000000000000, 1438.363963900590079, 157.6955293123980084 ) ) ;
#9539 = CARTESIAN_POINT ( 'NONE',  ( -3.163205911649999980, 1497.502928199090093, 198.2885394267989909 ) ) ;
#9541 = VERTEX_POINT ( 'NONE', #105144 ) ;
#9540 = CARTESIAN_POINT ( 'NONE',  ( -1.029084866039999824, 1496.468087385590024, 221.4697290446989939 ) ) ;
#9542 = CARTESIAN_POINT ( 'NONE',  ( 11.17472318946589382, 1414.941152333678701, 222.2292738415587223 ) ) ;
#9543 = ORIENTED_EDGE ( 'NONE', *, *, #30975, .F. ) ;
#9544 = CARTESIAN_POINT ( 'NONE',  ( 12.45246148929999919, 1410.452081827329948, 259.9010045688979744 ) ) ;
#9545 = CARTESIAN_POINT ( 'NONE',  ( -23.67770893750000027, 1410.915352782729997, 207.0119029875280035 ) ) ;
#9547 = CARTESIAN_POINT ( 'NONE',  ( 16.16924758266979723, 1409.477698513250061, 193.1979172417030099 ) ) ;
#9546 = CARTESIAN_POINT ( 'NONE',  ( -10.66999429222479989, 1425.355950166579987, 113.0095011697890044 ) ) ;
#9548 = CARTESIAN_POINT ( 'NONE',  ( 4.624099291334999862, 1516.962555622980062, 212.3771868965270073 ) ) ;
#9549 = CARTESIAN_POINT ( 'NONE',  ( 18.38538203976483487, 1509.674347933654644, 185.4157845068922086 ) ) ;
#9550 = CARTESIAN_POINT ( 'NONE',  ( -18.64672481370000057, 1416.851343898729965, 208.5597484337050105 ) ) ;
#9551 = CARTESIAN_POINT ( 'NONE',  ( -21.01921848810000171, 1409.015076449529943, 267.0603558840980440 ) ) ;
#9552 = CARTESIAN_POINT ( 'NONE',  ( -13.31507528231309934, 1379.509187062359842, 208.4414898241909953 ) ) ;
#9553 = CARTESIAN_POINT ( 'NONE',  ( 40.26002446930366574, 1457.179217869769673, 269.7777131889765769 ) ) ;
#9554 = CARTESIAN_POINT ( 'NONE',  ( 2.759035106590659758, 1508.551704408389924, 214.0956385152369990 ) ) ;
#9555 = CARTESIAN_POINT ( 'NONE',  ( -39.08845109511560878, 1439.842738404589909, 136.7133373061289774 ) ) ;
#9556 = EDGE_LOOP ( 'NONE', ( #60132, #58744, #68346, #47480, #38210 ) ) ;
#9557 = CARTESIAN_POINT ( 'NONE',  ( 7.598730086320700572, 1396.178413889069816, 217.5432070791739818 ) ) ;
#9558 = CARTESIAN_POINT ( 'NONE',  ( 10.49207437818910016, 1461.076854184230115, 208.4973394663880129 ) ) ;
#9559 = CARTESIAN_POINT ( 'NONE',  ( -16.77882483980000217, 1459.813925007329772, 228.5196583047979857 ) ) ;
#9560 = EDGE_LOOP ( 'NONE', ( #91036, #35192, #42344 ) ) ;
#9561 = ORIENTED_EDGE ( 'NONE', *, *, #6246, .T. ) ;
#9562 = CARTESIAN_POINT ( 'NONE',  ( -29.33944776771571483, 1509.939423613863028, 211.5188534573150321 ) ) ;
#9563 = CARTESIAN_POINT ( 'NONE',  ( -6.384249706610589215, 1425.832386075969907, 153.2928965425799959 ) ) ;
#9564 = VERTEX_POINT ( 'NONE', #95634 ) ;
#9565 = CARTESIAN_POINT ( 'NONE',  ( -14.22198381479079998, 1380.226902504789905, 210.5888445733199887 ) ) ;
#9566 = B_SPLINE_CURVE_WITH_KNOTS ( 'NONE', 5,
 ( #62670, #26813, #10013, #28477, #53140, #2200, #61001, #11137, #62105 ),
 .UNSPECIFIED., .F., .F.,
 ( 6, 3, 6 ),
 ( 0.000000000000000000, 0.5000000000000000000, 1.000000000000000000 ),
 .UNSPECIFIED. ) ;
#9567 = CARTESIAN_POINT ( 'NONE',  ( -9.360141924177080242, 1418.479953072925355, 196.8921625633495012 ) ) ;
#9568 = DIRECTION ( 'NONE',  ( -0.000000000000000000, -1.000000000000000000, -0.000000000000000000 ) ) ;
#9569 = DIRECTION ( 'NONE',  ( -0.6709778558543639804, 0.000000000000000000, 0.7414773880254746929 ) ) ;
#9570 = CARTESIAN_POINT ( 'NONE',  ( 6.081399314780780330, 1508.610505977490220, 201.8017946903299844 ) ) ;
#9571 = CARTESIAN_POINT ( 'NONE',  ( 9.251643635294589885, 1451.133743409539875, 209.4001945862339937 ) ) ;
#9572 = DIRECTION ( 'NONE',  ( 0.8672669759446699489, -0.000000000000000000, 0.4978433412588613716 ) ) ;
#9573 = CARTESIAN_POINT ( 'NONE',  ( -98.94755837794630793, 1384.870786900800113, 296.0572709506019464 ) ) ;
#9574 = VERTEX_POINT ( 'NONE', #53099 ) ;
#9575 = CARTESIAN_POINT ( 'NONE',  ( 1.124289655455000148, 1517.184063036290127, 202.5579304082170040 ) ) ;
#9576 = CARTESIAN_POINT ( 'NONE',  ( -2.480427292634999947, 1516.872851364150165, 209.8797317620669673 ) ) ;
#9577 = VERTEX_POINT ( 'NONE', #37387 ) ;
#9578 = CARTESIAN_POINT ( 'NONE',  ( 18.72979941119999836, 1454.437773883689943, 204.5413093961989830 ) ) ;
#9579 = CARTESIAN_POINT ( 'NONE',  ( 4.597999444932870716, 1511.399594748111213, 217.5114347307018363 ) ) ;
#9580 = ORIENTED_EDGE ( 'NONE', *, *, #46851, .T. ) ;
#9581 = CARTESIAN_POINT ( 'NONE',  ( -1.441435334883619968, 1455.080613134490022, 183.7350912049300007 ) ) ;
#9582 = ADVANCED_FACE ( 'NONE', ( #63718 ), #47130, .T. ) ;
#9583 = DIRECTION ( 'NONE',  ( -0.000000000000000000, -1.000000000000000000, -0.000000000000000000 ) ) ;
#9584 = CARTESIAN_POINT ( 'NONE',  ( 0.000000000000000000, 1524.340287715038357, 233.4544294405183678 ) ) ;
#9585 = CARTESIAN_POINT ( 'NONE',  ( -1.713536632167919960, 1469.335432983970122, 219.0203854141810211 ) ) ;
#9586 = CARTESIAN_POINT ( 'NONE',  ( -6.449257186580000578, 1423.216257312029938, 186.7332274999980086 ) ) ;
#9587 = CARTESIAN_POINT ( 'NONE',  ( 2.245205672760550275, 1410.074017455439844, 269.8657980300729946 ) ) ;
#9588 = CARTESIAN_POINT ( 'NONE',  ( 4.487249775049700240, 1509.038615934839981, 206.6339108193819811 ) ) ;
#9589 = CARTESIAN_POINT ( 'NONE',  ( -12.78943302956389871, 1502.708798875820094, 209.0180534851929792 ) ) ;
#9590 = CARTESIAN_POINT ( 'NONE',  ( 5.839375649711069372, 1441.004146644160073, 154.6877193062889830 ) ) ;
#9591 = CARTESIAN_POINT ( 'NONE',  ( -30.40156113259999771, 1379.643953478429921, 214.3104896918690088 ) ) ;
#9592 = AXIS2_PLACEMENT_3D ( 'NONE', #30355, #99753, #48285 ) ;
#9593 = CARTESIAN_POINT ( 'NONE',  ( 0.03068904745159911282, 1410.176690693337150, 233.2117524165238081 ) ) ;
#9595 = CARTESIAN_POINT ( 'NONE',  ( 9.468383857098320533, 1468.845280592710196, 203.0453074138920044 ) ) ;
#9594 = CARTESIAN_POINT ( 'NONE',  ( 17.69067153579999996, 1458.123849909530009, 230.3917265491979833 ) ) ;
#9596 = CARTESIAN_POINT ( 'NONE',  ( -4.452653756150430020, 1423.820617467126112, 184.3121917427432663 ) ) ;
#9597 = CARTESIAN_POINT ( 'NONE',  ( 17.82218026611110062, 1417.888996552500203, 225.0117082750950033 ) ) ;
#9598 = CARTESIAN_POINT ( 'NONE',  ( -2.499952405548359735, 1420.058982578270161, 97.99576999742468786 ) ) ;
#9599 = ORIENTED_EDGE ( 'NONE', *, *, #78365, .T. ) ;
#9600 = CARTESIAN_POINT ( 'NONE',  ( 18.13455101590619734, 1424.499683988459992, 223.9684704944369855 ) ) ;
#9601 = FACE_OUTER_BOUND ( 'NONE', #109689, .T. ) ;
#9602 = CARTESIAN_POINT ( 'NONE',  ( -3.030506966135566582, 1485.909268244792202, 182.3458070157814745 ) ) ;
#9603 = CARTESIAN_POINT ( 'NONE',  ( -14.44692751430000044, 1415.677402202029953, 213.4243480473190289 ) ) ;
#9605 = ORIENTED_EDGE ( 'NONE', *, *, #32338, .F. ) ;
#9604 = CARTESIAN_POINT ( 'NONE',  ( 1.842962231260000028, 1515.064792882589927, 204.7923971856590128 ) ) ;
#9606 = CARTESIAN_POINT ( 'NONE',  ( 17.11050544153610176, 1414.913527275050001, 210.6493517936639819 ) ) ;
#9607 = CARTESIAN_POINT ( 'NONE',  ( -24.49494333239999833, 1443.910508108940121, 210.9673953710880028 ) ) ;
#9608 = CARTESIAN_POINT ( 'NONE',  ( -10.89448555409999919, 1427.255301856029973, 149.7563259081979936 ) ) ;
#9609 = CARTESIAN_POINT ( 'NONE',  ( 20.71343476517534299, 1522.382868172863937, 238.3377464195763764 ) ) ;
#9610 = B_SPLINE_CURVE_WITH_KNOTS ( 'NONE', 3,
 ( #71338, #96498, #19778, #53979, #27635, #11939, #18659, #37691, #106546, #87557, #55067, #71894, #80801, #95944, #97601, #46119, #88112, #4107, #20871 ),
 .UNSPECIFIED., .F., .F.,
 ( 4, 3, 3, 3, 3, 3, 4 ),
 ( -7.430926493242850484, -7.167859904195459819, -6.108952779777689912, -5.238805666324060084, -4.533344564236309715, -3.758780901387599460, -3.046684027039999521 ),
 .UNSPECIFIED. ) ;
#9611 = DIRECTION ( 'NONE',  ( 0.4794255386042041711, 0.000000000000000000, 0.8775825618903720926 ) ) ;
#9612 = CARTESIAN_POINT ( 'NONE',  ( 3.512785867830420180E-12, 1395.913060387330006, 198.1220674046479928 ) ) ;
#9613 = DIRECTION ( 'NONE',  ( -0.000000000000000000, -1.000000000000000000, -0.000000000000000000 ) ) ;
#9614 = CARTESIAN_POINT ( 'NONE',  ( -15.82925655696500122, 1512.053076656670100, 221.8543121690670148 ) ) ;
#9615 = CARTESIAN_POINT ( 'NONE',  ( 16.73302193210000155, 1412.751708530930046, 226.5522076595979968 ) ) ;
#9616 = EDGE_CURVE ( 'NONE', #16269, #20056, #63179, .T. ) ;
#9617 = CARTESIAN_POINT ( 'NONE',  ( -9.861282131150000296, 1479.534343986590102, 214.8159920528989915 ) ) ;
#9618 = CARTESIAN_POINT ( 'NONE',  ( -16.12484297499999997, 1459.082000229730056, 229.9878769759980059 ) ) ;
#9619 = CARTESIAN_POINT ( 'NONE',  ( -2.493699806765000027, 1516.858326417339867, 206.6451124560869914 ) ) ;
#9620 = CARTESIAN_POINT ( 'NONE',  ( 30.24521524950000284, 1414.226558136529775, 268.0936365245980255 ) ) ;
#9621 = B_SPLINE_CURVE_WITH_KNOTS ( 'NONE', 4,
 ( #71813, #77555, #51239, #20243, #54444 ),
 .UNSPECIFIED., .F., .F.,
 ( 5, 5 ),
 ( 3.613988937050000239, 5.260361675040000407 ),
 .UNSPECIFIED. ) ;
#9622 = CARTESIAN_POINT ( 'NONE',  ( 19.69322412969999903, 1430.301618381130083, 194.7952341051980056 ) ) ;
#9623 = CARTESIAN_POINT ( 'NONE',  ( -23.25337057739999835, 1434.173748762760169, 214.1890449410079782 ) ) ;
#9624 = CARTESIAN_POINT ( 'NONE',  ( 8.167113615893089928, 1506.588258981613308, 229.6708076605581823 ) ) ;
#9625 = CARTESIAN_POINT ( 'NONE',  ( 32.86802468363458729, 1523.481610118014942, 217.2040256692604885 ) ) ;
#9626 = CARTESIAN_POINT ( 'NONE',  ( 19.64599270300000100, 1476.662575758389949, 214.0395835971089866 ) ) ;
#9627 = CYLINDRICAL_SURFACE ( 'NONE', #49757, 2.000000000000001776 ) ;
#9628 = DIRECTION ( 'NONE',  ( 1.000000000000000000, -0.000000000000000000, 1.224646799147353207E-16 ) ) ;
#9629 = CARTESIAN_POINT ( 'NONE',  ( -13.81487708659999925, 1442.792748204340114, 188.4458667950979986 ) ) ;
#9630 = CARTESIAN_POINT ( 'NONE',  ( -5.906252883828099876, 1484.773058574589868, 198.7863962546840071 ) ) ;
#9631 = CARTESIAN_POINT ( 'NONE',  ( -30.20925072189999838, 1435.551608164450045, 135.6183629175980059 ) ) ;
#9632 = FACE_OUTER_BOUND ( 'NONE', #4105, .T. ) ;
#9633 = ORIENTED_EDGE ( 'NONE', *, *, #53706, .F. ) ;
#9634 = DIRECTION ( 'NONE',  ( 0.02622235658550479270, -0.9995718917029567940, -0.01297772447215353626 ) ) ;
#9635 = CARTESIAN_POINT ( 'NONE',  ( -14.89768408183259929, 1409.433298979099845, 208.1358299322530172 ) ) ;
#9636 = CARTESIAN_POINT ( 'NONE',  ( -11.77719994041109963, 1507.564759742010210, 208.2431318171160228 ) ) ;
#9637 = CARTESIAN_POINT ( 'NONE',  ( 31.23437356469446868, 1523.382868172864164, 221.8968241038843416 ) ) ;
#9638 = CARTESIAN_POINT ( 'NONE',  ( -23.72712553860000284, 1471.175367018230190, 267.6119644152980186 ) ) ;
#9639 = CARTESIAN_POINT ( 'NONE',  ( 29.74901212038063747, 1525.343727714918259, 196.2390656498153305 ) ) ;
#9640 = CARTESIAN_POINT ( 'NONE',  ( 0.1617910656812470149, 1420.267555168729814, 183.6005827977619731 ) ) ;
#9641 = CARTESIAN_POINT ( 'NONE',  ( -24.34146701290755033, 1444.633454629505877, 211.2257049224041054 ) ) ;
#9642 = CARTESIAN_POINT ( 'NONE',  ( -83.32488467863339565, 1384.631840452700089, 305.8394389779119820 ) ) ;
#9643 = CARTESIAN_POINT ( 'NONE',  ( -16.02315411856420013, 1384.943691493999950, 200.7859781080500170 ) ) ;
#9644 = CARTESIAN_POINT ( 'NONE',  ( 17.03853110007430161, 1423.468938760780247, 227.1882557915390066 ) ) ;
#9645 = CARTESIAN_POINT ( 'NONE',  ( 11.73070209459999802, 1414.913060387329779, 220.5399151727980041 ) ) ;
#9646 = CARTESIAN_POINT ( 'NONE',  ( 14.24758728489999982, 1463.294432896430180, 223.4356431231979911 ) ) ;
#9647 = CARTESIAN_POINT ( 'NONE',  ( -14.45097772706500017, 1514.857962383129916, 193.8743388492669908 ) ) ;
#9648 = ADVANCED_FACE ( 'NONE', ( #53664 ), #46916, .T. ) ;
#9649 = DIRECTION ( 'NONE',  ( 0.4794255386042031719, 0.000000000000000000, 0.8775825618903726477 ) ) ;
#9650 = CARTESIAN_POINT ( 'NONE',  ( -3.549614846889999953, 1507.276796483229873, 180.9705030601980127 ) ) ;
#9651 = EDGE_CURVE ( 'NONE', #4978, #73756, #52579, .T. ) ;
#9652 = CARTESIAN_POINT ( 'NONE',  ( -23.44454018040000065, 1410.653275362629984, 206.2180064241879904 ) ) ;
#9653 = EDGE_CURVE ( 'NONE', #103213, #52345, #90033, .T. ) ;
#9654 = ADVANCED_FACE ( 'NONE', ( #89442 ), #28434, .F. ) ;
#9655 = CARTESIAN_POINT ( 'NONE',  ( 15.42960845380000023, 1414.913060387329779, 204.2857382735780050 ) ) ;
#9656 = CARTESIAN_POINT ( 'NONE',  ( 4.389420737370000047, 1486.156988616190120, 218.9715652691990044 ) ) ;
#9657 = CARTESIAN_POINT ( 'NONE',  ( 10.43856162392300035, 1480.982005454859973, 207.5364568915489940 ) ) ;
#9658 = EDGE_CURVE ( 'NONE', #86873, #91513, #59333, .T. ) ;
#9659 = DIRECTION ( 'NONE',  ( 1.755985294532469921E-16, -1.000000000000000000, 1.338183447452831989E-16 ) ) ;
#9660 = EDGE_CURVE ( 'NONE', #27509, #15707, #23201, .T. ) ;
#9661 = CARTESIAN_POINT ( 'NONE',  ( 19.14951757210000238, 1460.484328893590146, 220.2380389338990199 ) ) ;
#9662 = CARTESIAN_POINT ( 'NONE',  ( 16.50400130224743833, 1525.907212628473644, 181.9890130758377609 ) ) ;
#9663 = CARTESIAN_POINT ( 'NONE',  ( 9.992001554966840615, 1491.422527301840319, 188.4943246010310247 ) ) ;
#9665 = CARTESIAN_POINT ( 'NONE',  ( -8.762022473709999204, 1382.501695996660146, 200.2807315899889886 ) ) ;
#9664 = SPHERICAL_SURFACE ( 'NONE', #90796, 7.299999999999999822 ) ;
#9666 = CARTESIAN_POINT ( 'NONE',  ( -4.993299335669999728, 1391.657172340389934, 203.5222458180090257 ) ) ;
#9667 = DIRECTION ( 'NONE',  ( 0.000000000000000000, 1.000000000000000000, 0.000000000000000000 ) ) ;
#9668 = CARTESIAN_POINT ( 'NONE',  ( -11.24552814110000121, 1490.344885738790026, 211.0486739485690180 ) ) ;
#9669 = CARTESIAN_POINT ( 'NONE',  ( 9.735382849826228480, 1450.705275490849999, 205.3287227118019871 ) ) ;
#9670 = AXIS2_PLACEMENT_3D ( 'NONE', #30927, #13556, #81877 ) ;
#9671 = EDGE_CURVE ( 'NONE', #60117, #40901, #8520, .T. ) ;
#9672 = CARTESIAN_POINT ( 'NONE',  ( -3.034926079678203159, 1369.200812461396481, 210.6218459616991936 ) ) ;
#9673 = CARTESIAN_POINT ( 'NONE',  ( -6.557909920764999789, 1516.908489800550115, 203.3441005368270282 ) ) ;
#9674 = CARTESIAN_POINT ( 'NONE',  ( -5.960248613831936382, 1398.090355469260885, 220.6805375304444965 ) ) ;
#9675 = CARTESIAN_POINT ( 'NONE',  ( -3.827178453834580552, 1440.905424146408222, 156.3821726451605514 ) ) ;
#9676 = FACE_BOUND ( 'NONE', #110772, .T. ) ;
#9677 = CARTESIAN_POINT ( 'NONE',  ( 2.326513286163319538, 1476.258183507229887, 197.8633931498989966 ) ) ;
#9678 = CARTESIAN_POINT ( 'NONE',  ( 6.386763885830579746, 1505.038503483219984, 219.3374787946009974 ) ) ;
#9679 = CARTESIAN_POINT ( 'NONE',  ( -9.315479902914303167, 1422.891722004452731, 210.7235706083796458 ) ) ;
#9680 = VECTOR ( 'NONE', #109241, 1000.000000000000000 ) ;
#9682 = ORIENTED_EDGE ( 'NONE', *, *, #65339, .F. ) ;
#9681 = CARTESIAN_POINT ( 'NONE',  ( -61.47253991419999863, 1379.746604392980089, 268.2739652322590018 ) ) ;
#9683 = ORIENTED_EDGE ( 'NONE', *, *, #47980, .F. ) ;
#9684 = CARTESIAN_POINT ( 'NONE',  ( 11.62114210317369967, 1433.932828604870110, 151.1840183943909892 ) ) ;
#9685 = CARTESIAN_POINT ( 'NONE',  ( 21.37469332459763649, 1525.408327360768681, 184.8352391485183546 ) ) ;
#9686 = ORIENTED_EDGE ( 'NONE', *, *, #102204, .T. ) ;
#9687 = CARTESIAN_POINT ( 'NONE',  ( -107.2728094030000108, 1379.016579441009753, 308.4876107606589812 ) ) ;
#9688 = CARTESIAN_POINT ( 'NONE',  ( -3.487592468881668406, 1508.603735221695615, 213.8522301334431290 ) ) ;
#9689 = CARTESIAN_POINT ( 'NONE',  ( 2.898098007870020254, 1515.492902828930028, 204.9850961497120352 ) ) ;
#9691 = CARTESIAN_POINT ( 'NONE',  ( 6.984406781949999754, 1427.831049039629988, 123.0297916884979941 ) ) ;
#9690 = LINE ( 'NONE', #18082, #3237 ) ;
#9692 = CARTESIAN_POINT ( 'NONE',  ( 17.44907805046609894, 1488.410848430800115, 229.8778797731829968 ) ) ;
#9693 = ADVANCED_FACE ( 'NONE', ( #91641 ), #49109, .F. ) ;
#9694 = CARTESIAN_POINT ( 'NONE',  ( 1.654058768690000125, 1488.174163428330075, 181.9749823065980081 ) ) ;
#9695 = CARTESIAN_POINT ( 'NONE',  ( -5.332221971070000066, 1416.518532928429977, 191.7600702370979775 ) ) ;
#9696 = CARTESIAN_POINT ( 'NONE',  ( -24.16428115052429959, 1444.791601846139883, 211.5724956969189918 ) ) ;
#9697 = B_SPLINE_SURFACE_WITH_KNOTS ( 'NONE', 5, 5, ( 
 ( #26931, #2311, #62779, #86276, #19050, #62212 ),
 ( #18499, #36422, #44857, #27468, #53253, #87393 ),
 ( #104735, #85719, #79009, #52695, #51587, #86831 ),
 ( #95783, #70615, #28024, #19617, #35889, #11246 ),
 ( #53818, #45407, #79547, #2849, #36973, #71165 ),
 ( #43189, #77341, #5021, #38080, #71733, #80083 ),
 ( #96893, #38621, #45944, #22346, #5585, #21239 ),
 ( #63316, #97436, #64953, #99067, #54899, #20703 ),
 ( #13402, #97970, #89578, #89026, #72257, #12870 ) ),
 .UNSPECIFIED., .F., .F., .F.,
 ( 6, 3, 6 ),
 ( 6, 6 ),
 ( 3.012462719602379657, 5.172868947549999596, 7.333275175507620425 ),
 ( -0.0004258868076247550446, 2.000000000000000000 ),
 .UNSPECIFIED. ) ;
#9698 = CARTESIAN_POINT ( 'NONE',  ( 2.880592928985000079, 1516.859514182039902, 211.9868180862470126 ) ) ;
#9699 = EDGE_CURVE ( 'NONE', #76507, #8045, #25751, .T. ) ;
#9700 = CARTESIAN_POINT ( 'NONE',  ( 37.28324835979699969, 1436.551445510500116, 134.0999999968369991 ) ) ;
#9701 = CARTESIAN_POINT ( 'NONE',  ( -8.466661967441870829, 1424.048519636140099, 207.5723062640520027 ) ) ;
#9702 = CARTESIAN_POINT ( 'NONE',  ( 6.382129819174999774, 1514.500328598809801, 201.2525669677770281 ) ) ;
#9703 = ORIENTED_EDGE ( 'NONE', *, *, #110394, .T. ) ;
#9704 = CARTESIAN_POINT ( 'NONE',  ( 14.13658382577439987, 1436.257447983569818, 150.1576428853639982 ) ) ;
#9705 = CARTESIAN_POINT ( 'NONE',  ( -0.5620977654635980203, 1416.851343899799986, 227.7685710128770040 ) ) ;
#9706 = EDGE_LOOP ( 'NONE', ( #64760, #57250, #40275, #29766 ) ) ;
#9707 = EDGE_CURVE ( 'NONE', #85866, #47741, #21782, .T. ) ;
#9708 = ORIENTED_EDGE ( 'NONE', *, *, #52348, .F. ) ;
#9709 = CARTESIAN_POINT ( 'NONE',  ( -7.380526870715000243, 1511.503799556579906, 215.6010310885870069 ) ) ;
#9710 = CARTESIAN_POINT ( 'NONE',  ( 16.60142420124314455, 1513.050501378471836, 197.0834984225024016 ) ) ;
#9711 = LINE ( 'NONE', #60138, #52833 ) ;
#9712 = CARTESIAN_POINT ( 'NONE',  ( 5.004442038985000174, 1516.690345681169902, 216.8349637732169697 ) ) ;
#9713 = CARTESIAN_POINT ( 'NONE',  ( 9.720721973410000771, 1462.346955765789971, 208.4427505688250051 ) ) ;
#9714 = EDGE_CURVE ( 'NONE', #1439, #99476, #28568, .T. ) ;
#9715 = CARTESIAN_POINT ( 'NONE',  ( -19.09068663893856055, 1441.686046601835869, 210.1346042266184782 ) ) ;
#9716 = CARTESIAN_POINT ( 'NONE',  ( -34.04422864232062551, 1379.637802395616518, 217.1019886382790389 ) ) ;
#9717 = CARTESIAN_POINT ( 'NONE',  ( 2.949954862130000244, 1464.477966747790106, 199.7317119218890014 ) ) ;
#9718 = CARTESIAN_POINT ( 'NONE',  ( 0.9826203254349998861, 1507.899765146830077, 237.3510063151980205 ) ) ;
#9719 = ORIENTED_EDGE ( 'NONE', *, *, #12532, .F. ) ;
#9720 = CARTESIAN_POINT ( 'NONE',  ( -2.880592967115000125, 1516.859514182039902, 206.2568738160869941 ) ) ;
#9722 = EDGE_LOOP ( 'NONE', ( #100361, #31184, #38666, #29350, #80475, #97891, #7341 ) ) ;
#9721 = B_SPLINE_CURVE_WITH_KNOTS ( 'NONE', 3,
 ( #53192, #29083, #87334, #10630, #63267, #17889, #86218, #43678, #69453, #88975 ),
 .UNSPECIFIED., .F., .F.,
 ( 4, 2, 2, 2, 4 ),
 ( -1.402821835648833217E-05, 0.0002466997669630880004, 0.0005074277522826644042, 0.0007681557376022407537, 0.001028883722921816995 ),
 .UNSPECIFIED. ) ;
#9723 = CARTESIAN_POINT ( 'NONE',  ( 20.81437694473750000, 1440.913060387330006, 221.3077511967070166 ) ) ;
#9724 = CARTESIAN_POINT ( 'NONE',  ( -19.11260742820000047, 1509.007777199430166, 230.1654993297979956 ) ) ;
#9725 = EDGE_LOOP ( 'NONE', ( #39679, #102762, #71434 ) ) ;
#9726 = CARTESIAN_POINT ( 'NONE',  ( -6.648420388365120282, 1508.610128767860033, 202.0257353737460164 ) ) ;
#9727 = CARTESIAN_POINT ( 'NONE',  ( -14.73086949309999838, 1409.427473685330142, 191.7357518190979988 ) ) ;
#9728 = CARTESIAN_POINT ( 'NONE',  ( -24.34449756709999946, 1441.851259293030125, 211.7501733141479860 ) ) ;
#9730 = VERTEX_POINT ( 'NONE', #23865 ) ;
#9729 = CARTESIAN_POINT ( 'NONE',  ( 5.161277877375379575, 1424.205378946189967, 193.2953230041809718 ) ) ;
#9731 = CARTESIAN_POINT ( 'NONE',  ( -6.067071732141870122, 1511.169205552290123, 201.5628721129530163 ) ) ;
#9732 = CARTESIAN_POINT ( 'NONE',  ( -12.00019380695538018, 1433.679412593930692, 147.5877376356537809 ) ) ;
#9733 = CARTESIAN_POINT ( 'NONE',  ( 15.12003195112067111, 1517.151704408390060, 199.7262892757531745 ) ) ;
#9734 = CARTESIAN_POINT ( 'NONE',  ( -2.409034624560000282, 1511.999350511789999, 211.5308805862590020 ) ) ;
#9736 = CARTESIAN_POINT ( 'NONE',  ( 31.34137657934008558, 1512.187213306747481, 196.3411265156547358 ) ) ;
#9735 = CARTESIAN_POINT ( 'NONE',  ( 21.33281718256687753, 1523.429859730330008, 180.4846393450492599 ) ) ;
#9737 = B_SPLINE_SURFACE_WITH_KNOTS ( 'NONE', 5, 1, ( 
 ( #98764, #71963 ),
 ( #19849, #79787 ),
 ( #20393, #107167 ),
 ( #97124, #55693 ),
 ( #12563, #3643 ),
 ( #36667, #54597 ) ),
 .UNSPECIFIED., .F., .F., .F.,
 ( 6, 6 ),
 ( 2, 2 ),
 ( 0.000000000000000000, 11.48860674278019900 ),
 ( -1.500000000000000000, 1.500000000000000000 ),
 .UNSPECIFIED. ) ;
#9738 = CARTESIAN_POINT ( 'NONE',  ( -5.776491133374999976, 1516.858301627840092, 214.9045953718370185 ) ) ;
#9739 = CARTESIAN_POINT ( 'NONE',  ( 23.54053115110000149, 1409.992431845630108, 209.4961337924339944 ) ) ;
#9740 = CARTESIAN_POINT ( 'NONE',  ( -20.47737311789999737, 1507.835268392529997, 189.6592733436979756 ) ) ;
#9741 = CARTESIAN_POINT ( 'NONE',  ( 28.04656794799999986, 1508.051246012029878, 208.1255033510109911 ) ) ;
#9742 = CARTESIAN_POINT ( 'NONE',  ( -3.251888867474999945, 1516.793978928989873, 211.6142896211370044 ) ) ;
#9743 = EDGE_CURVE ( 'NONE', #101207, #68013, #22146, .T. ) ;
#9744 = CARTESIAN_POINT ( 'NONE',  ( -11.81773885611420027, 1482.251074316360018, 207.7669157962629924 ) ) ;
#9745 = CARTESIAN_POINT ( 'NONE',  ( 29.86281881105859171, 1525.137906803762689, 222.1296981937806549 ) ) ;
#9747 = ORIENTED_EDGE ( 'NONE', *, *, #74069, .F. ) ;
#9746 = CARTESIAN_POINT ( 'NONE',  ( -89.08896662849998904, 1386.751329644390125, 292.3648858342590415 ) ) ;
#9748 = CARTESIAN_POINT ( 'NONE',  ( 35.25153999819999484, 1460.998002025230107, 264.2530495828980293 ) ) ;
#9749 = CARTESIAN_POINT ( 'NONE',  ( 10.93679547204000002, 1490.434980368090010, 209.9321327948960061 ) ) ;
#9750 = CARTESIAN_POINT ( 'NONE',  ( -7.549016801754999229, 1510.423579818969984, 213.5498276941069946 ) ) ;
#9751 = CARTESIAN_POINT ( 'NONE',  ( -6.840494606030000035, 1507.559926465930175, 235.7307567964980137 ) ) ;
#9752 = CARTESIAN_POINT ( 'NONE',  ( -19.24704176450000048, 1456.292361409630075, 227.8736337451979921 ) ) ;
#9753 = CIRCLE ( 'NONE', #50926, 1.999999609710441106 ) ;
#9754 = EDGE_CURVE ( 'NONE', #30213, #97183, #73196, .T. ) ;
#9756 = CARTESIAN_POINT ( 'NONE',  ( 17.99954443082109989, 1410.904693892220166, 222.9872220945560173 ) ) ;
#9755 = CARTESIAN_POINT ( 'NONE',  ( 11.86923165449999829, 1432.580340585790054, 150.3965903347979918 ) ) ;
#9757 = CARTESIAN_POINT ( 'NONE',  ( -8.884856068493249381, 1449.032530459529880, 211.3463590648900094 ) ) ;
#9758 = CARTESIAN_POINT ( 'NONE',  ( -109.3809973283789958, 1382.669152972790243, 311.0761981651330643 ) ) ;
#9759 = EDGE_LOOP ( 'NONE', ( #36585, #80782, #71298, #34062, #26929 ) ) ;
#9760 = CARTESIAN_POINT ( 'NONE',  ( -2.294209667535000108, 1516.603620185149794, 203.3509623682169831 ) ) ;
#9761 = CARTESIAN_POINT ( 'NONE',  ( 0.3391062976460000322, 1405.843521269830035, 267.2349199626979726 ) ) ;
#9762 = CIRCLE ( 'NONE', #24037, 1.999999999999998668 ) ;
#9763 = CARTESIAN_POINT ( 'NONE',  ( 28.96739426325766331, 1526.189892541618974, 197.4412433453230733 ) ) ;
#9764 = CIRCLE ( 'NONE', #81209, 2.000000000000001776 ) ;
#9765 = CARTESIAN_POINT ( 'NONE',  ( -4.986743168611350200E-06, 1473.589451234700164, 270.3925711489580408 ) ) ;
#9766 = DIRECTION ( 'NONE',  ( -0.000000000000000000, -1.000000000000000000, -0.000000000000000000 ) ) ;
#9767 = CARTESIAN_POINT ( 'NONE',  ( 22.03465957474552539, 1522.382868172863937, 182.8300405912328301 ) ) ;
#9768 = CARTESIAN_POINT ( 'NONE',  ( -20.13259443705889851, 1508.866006816849904, 188.8141325411800153 ) ) ;
#9769 = CARTESIAN_POINT ( 'NONE',  ( -38.50736833418749683, 1440.913060392829948, 257.0794435389950081 ) ) ;
#9770 = EDGE_CURVE ( 'NONE', #11785, #49802, #2553, .T. ) ;
#9771 = CARTESIAN_POINT ( 'NONE',  ( 9.862951377358559313, 1519.551704408389924, 189.8497022443989977 ) ) ;
#9772 = CARTESIAN_POINT ( 'NONE',  ( -0.5718103630240639612, 1450.893092329450155, 154.2421351031399865 ) ) ;
#9773 = CARTESIAN_POINT ( 'NONE',  ( -1.682023246740000033, 1431.030650798590159, 200.9066206319189973 ) ) ;
#9774 = CARTESIAN_POINT ( 'NONE',  ( 10.60784606965410148, 1480.939836828909847, 210.5430849895140284 ) ) ;
#9775 = CARTESIAN_POINT ( 'NONE',  ( -22.04658257820682721, 1524.075000532257263, 184.4787014209232154 ) ) ;
#9776 = DIRECTION ( 'NONE',  ( 2.775557561562887961E-17, -0.7071067811865475727, -0.7071067811865475727 ) ) ;
#9777 = ORIENTED_EDGE ( 'NONE', *, *, #25491, .T. ) ;
#9778 = MANIFOLD_SOLID_BREP ( 'Stock-MAS-682-1', #44953 ) ;
#9780 = ADVANCED_FACE ( 'NONE', ( #88094 ), #59760, .T. ) ;
#9779 = CARTESIAN_POINT ( 'NONE',  ( 2.500000195207620290, 1448.894380947069976, 182.3534016008459844 ) ) ;
#9781 = CARTESIAN_POINT ( 'NONE',  ( 2.500000000000000000, 1425.929641634319978, 183.3886485707629959 ) ) ;
#9782 = CARTESIAN_POINT ( 'NONE',  ( 3.629220049600000220, 1485.493215689190038, 199.0019176958990101 ) ) ;
#9783 = CARTESIAN_POINT ( 'NONE',  ( -26.02647937380000087, 1444.708500955269983, 212.3004752285879988 ) ) ;
#9784 = CARTESIAN_POINT ( 'NONE',  ( -0.5400825333060000899, 1417.004123502529865, 234.1403136323979766 ) ) ;
#9785 = CARTESIAN_POINT ( 'NONE',  ( 11.85479774020000043, 1501.321054691989957, 210.0448065485869904 ) ) ;
#9786 = CARTESIAN_POINT ( 'NONE',  ( -29.39269380490000216, 1509.939475872329922, 211.4205234510380080 ) ) ;
#9787 = CYLINDRICAL_SURFACE ( 'NONE', #94977, 2.000000000000002220 ) ;
#9788 = CARTESIAN_POINT ( 'NONE',  ( -6.126746181595000174, 1514.923664147150021, 217.2480802176870043 ) ) ;
#9789 = CARTESIAN_POINT ( 'NONE',  ( -17.54299231450000107, 1415.063410489729904, 207.9622084005079898 ) ) ;
#9790 = CARTESIAN_POINT ( 'NONE',  ( -7.027952441359999192, 1482.449581481789892, 201.0380530320790058 ) ) ;
#9791 = CARTESIAN_POINT ( 'NONE',  ( 18.91040668671516300, 1416.839570625551914, 209.9480928164305453 ) ) ;
#9792 = EDGE_CURVE ( 'NONE', #19741, #34413, #3218, .T. ) ;
#9793 = CARTESIAN_POINT ( 'NONE',  ( -9.302637435961308654, 1396.237915646910096, 203.1362697860550099 ) ) ;
#9794 = ORIENTED_EDGE ( 'NONE', *, *, #102136, .F. ) ;
#9795 = VECTOR ( 'NONE', #48472, 1000.000000000000000 ) ;
#9796 = CARTESIAN_POINT ( 'NONE',  ( -16.62504627205539975, 1409.593993787780164, 225.4105808336230155 ) ) ;
#9797 = EDGE_CURVE ( 'NONE', #21883, #49707, #108007, .T. ) ;
#9798 = CARTESIAN_POINT ( 'NONE',  ( 9.804877192300001099, 1442.756953654919926, 148.8379299677979759 ) ) ;
#9799 = VERTEX_POINT ( 'NONE', #2452 ) ;
#9800 = ORIENTED_EDGE ( 'NONE', *, *, #74922, .T. ) ;
#9801 = CARTESIAN_POINT ( 'NONE',  ( -1.821463311390000062, 1495.107949858190068, 217.3487309858989818 ) ) ;
#9802 = CARTESIAN_POINT ( 'NONE',  ( -14.93413738244312228, 1416.108689801689025, 205.2226948075607709 ) ) ;
#9804 = CARTESIAN_POINT ( 'NONE',  ( -9.977180581269040616, 1439.208816910850146, 209.0674583647880240 ) ) ;
#9803 = FACE_OUTER_BOUND ( 'NONE', #51013, .T. ) ;
#9805 = FACE_OUTER_BOUND ( 'NONE', #79545, .T. ) ;
#9806 = CARTESIAN_POINT ( 'NONE',  ( -11.85865206170000086, 1433.007128070730232, 150.2761877906980033 ) ) ;
#9807 = EDGE_CURVE ( 'NONE', #63160, #70030, #7861, .T. ) ;
#9808 = CARTESIAN_POINT ( 'NONE',  ( -2.566714976521826230, 1420.724238763095173, 185.6155453858885664 ) ) ;
#9809 = CARTESIAN_POINT ( 'NONE',  ( 7.618847152659999900, 1425.153911876999928, 211.9847758557390023 ) ) ;
#9810 = FACE_OUTER_BOUND ( 'NONE', #68119, .T. ) ;
#9811 = FACE_BOUND ( 'NONE', #91771, .T. ) ;
#9812 = CARTESIAN_POINT ( 'NONE',  ( -105.6263533753079997, 1379.015674155129773, 306.1169297802109668 ) ) ;
#9813 = CARTESIAN_POINT ( 'NONE',  ( 8.063859222158944462, 1365.091964226176060, 208.3718459617061285 ) ) ;
#9814 = ADVANCED_FACE ( 'NONE', ( #11381 ), #36029, .T. ) ;
#9816 = ORIENTED_EDGE ( 'NONE', *, *, #47982, .T. ) ;
#9815 = CARTESIAN_POINT ( 'NONE',  ( 5.082331142230000154, 1453.684120746589770, 217.0135184815189859 ) ) ;
#9817 = EDGE_LOOP ( 'NONE', ( #71992, #5466, #79082, #2669 ) ) ;
#9818 = DIRECTION ( 'NONE',  ( -0.9993902469148121526, -0.03489947669269360953, 0.001077449825718530298 ) ) ;
#9819 = DIRECTION ( 'NONE',  ( 0.3953879427268398583, -0.03432097994341943431, 0.9178727826240195009 ) ) ;
#9820 = CARTESIAN_POINT ( 'NONE',  ( -8.571939095150000286E-11, 1471.791680839530045, 269.8654495162979856 ) ) ;
#9821 = CARTESIAN_POINT ( 'NONE',  ( 13.51519562106584971, 1434.954339805268546, 146.6368354188692820 ) ) ;
#9822 =( BOUNDED_CURVE ( )  B_SPLINE_CURVE ( 3, ( #43569, #75527, #101787, #103448 ),
 .UNSPECIFIED., .F., .F. ) 
 B_SPLINE_CURVE_WITH_KNOTS ( ( 4, 4 ),
 ( 4.613321846721008868, 4.741587033746983870 ),
 .UNSPECIFIED. ) 
 CURVE ( )  GEOMETRIC_REPRESENTATION_ITEM ( )  RATIONAL_B_SPLINE_CURVE ( ( 1.000000000000000000, 0.9986294733265421719, 0.9986294733265421719, 1.000000000000000000 ) ) 
 REPRESENTATION_ITEM ( '' )  );
#9823 = CARTESIAN_POINT ( 'NONE',  ( -1.368191914778909890, 1419.344528075180278, 185.2221190139939893 ) ) ;
#9824 = CARTESIAN_POINT ( 'NONE',  ( -31.97162612955063565, 1524.678541297860875, 201.5730793974714743 ) ) ;
#9825 = CARTESIAN_POINT ( 'NONE',  ( -2.890649542061729971, 1475.035107952139924, 198.0572108960010098 ) ) ;
#9826 = CARTESIAN_POINT ( 'NONE',  ( 22.63948220110000165, 1410.626538726429999, 206.7101357973980100 ) ) ;
#9827 = CARTESIAN_POINT ( 'NONE',  ( -2.500000000000000000, 1448.505996463670044, 160.4897366963279808 ) ) ;
#9828 = CARTESIAN_POINT ( 'NONE',  ( 10.33932082004445974, 1368.375147307815269, 209.6218459617033432 ) ) ;
#9829 = CARTESIAN_POINT ( 'NONE',  ( 14.11499368570000001, 1408.887749557829920, 212.0299715937679821 ) ) ;
#9830 = CARTESIAN_POINT ( 'NONE',  ( -0.7754390136715150206, 1405.775973440009921, 268.4837770662310277 ) ) ;
#9831 = CARTESIAN_POINT ( 'NONE',  ( -14.00371981653700004, 1435.086289393800143, 149.1230187904150171 ) ) ;
#9832 = ORIENTED_EDGE ( 'NONE', *, *, #45377, .F. ) ;
#9833 = CARTESIAN_POINT ( 'NONE',  ( -11.87502386937130083, 1433.007271227619867, 149.9804723889419904 ) ) ;
#9834 = CARTESIAN_POINT ( 'NONE',  ( 13.39320068580000012, 1444.488385957100036, 187.9681878425980130 ) ) ;
#9835 = B_SPLINE_SURFACE_WITH_KNOTS ( 'NONE', 5, 4, ( 
 ( #5318, #21541, #80928, #55197, #89324 ),
 ( #82013, #106668, #4226, #81454, #64150 ),
 ( #22630, #37825, #63605, #38903, #29402 ),
 ( #97722, #107779, #14258, #20992, #29957 ),
 ( #55752, #89871, #4759, #48448, #12062 ),
 ( #73085, #82586, #107225, #65244, #63070 ) ),
 .UNSPECIFIED., .F., .F., .F.,
 ( 6, 6 ),
 ( 5, 5 ),
 ( 0.000000000000000000, 111.1101480259999903 ),
 ( 25.81581217359999769, 39.03307591160000101 ),
 .UNSPECIFIED. ) ;
#9836 = VECTOR ( 'NONE', #110241, 1000.000000000000000 ) ;
#9837 = EDGE_LOOP ( 'NONE', ( #84872, #51705, #24866, #31398 ) ) ;
#9838 = ORIENTED_EDGE ( 'NONE', *, *, #33719, .T. ) ;
#9839 = CARTESIAN_POINT ( 'NONE',  ( -4.172050517839999806, 1455.094832059689907, 200.6673091711190011 ) ) ;
#9840 = CARTESIAN_POINT ( 'NONE',  ( -8.082564370840000123, 1362.241991287400197, 207.6218459616989946 ) ) ;
#9842 = EDGE_CURVE ( 'NONE', #3898, #73081, #4583, .T. ) ;
#9841 = AXIS2_PLACEMENT_3D ( 'NONE', #57177, #48770, #75072 ) ;
#9843 = CARTESIAN_POINT ( 'NONE',  ( 5.784638319815000429, 1516.939574742129935, 213.7356083271170064 ) ) ;
#9844 = CARTESIAN_POINT ( 'NONE',  ( 4.542415389984999941, 1511.388520542559945, 217.4923749357569989 ) ) ;
#9845 = ORIENTED_EDGE ( 'NONE', *, *, #74031, .T. ) ;
#9846 = CARTESIAN_POINT ( 'NONE',  ( -69.36674279230000195, 1374.746858117589909, 280.1513224085589968 ) ) ;
#9847 = CARTESIAN_POINT ( 'NONE',  ( -105.8174845808659938, 1378.913060387339783, 303.6992540374549776 ) ) ;
#9848 = CARTESIAN_POINT ( 'NONE',  ( -1.131796848745000084, 1516.659138130710289, 203.3488676535569937 ) ) ;
#9849 = CARTESIAN_POINT ( 'NONE',  ( -28.34445769270000071, 1509.155937271930043, 208.0685711019380051 ) ) ;
#9850 = B_SPLINE_SURFACE_WITH_KNOTS ( 'NONE', 5, 5, ( 
 ( #89454, #20571, #54770, #46929, #12188, #32305, #22217, #90544, #81585 ),
 ( #107899, #66488, #39605, #98397, #98942, #56415, #82707, #108459, #4889 ),
 ( #74872, #14927, #47463, #39030, #13822, #13272, #5996, #23337, #73209 ),
 ( #89997, #65379, #100049, #40148, #107353, #48008, #30649, #31741, #82146 ),
 ( #64835, #65927, #99482, #5445, #57529, #91653, #49122, #6550, #74331 ),
 ( #21670, #83255, #73775, #31192, #23876, #40701, #22764, #48572, #100595 ) ),
 .UNSPECIFIED., .F., .F., .F.,
 ( 6, 6 ),
 ( 6, 3, 6 ),
 ( 44.88737144639999599, 53.51437230290000002 ),
 ( 0.000000000000000000, 1.000000000000000000, 2.000000000000000000 ),
 .UNSPECIFIED. ) ;
#9851 = DIRECTION ( 'NONE',  ( -1.755985294532469921E-16, 1.000000000000000000, -1.338183447452831989E-16 ) ) ;
#9852 = CARTESIAN_POINT ( 'NONE',  ( -89.15245910350000713, 1385.190331364289932, 292.2648985219589690 ) ) ;
#9853 = CARTESIAN_POINT ( 'NONE',  ( -50.36207809872559693, 1384.621281085180044, 225.8468432978239662 ) ) ;
#9854 = CARTESIAN_POINT ( 'NONE',  ( 9.691985945171570194, 1462.686535208950090, 208.0124194077490074 ) ) ;
#9855 = CARTESIAN_POINT ( 'NONE',  ( 9.803834995107230554, 1522.051704408389924, 221.6221720662910002 ) ) ;
#9857 = ORIENTED_EDGE ( 'NONE', *, *, #83689, .T. ) ;
#9856 = CARTESIAN_POINT ( 'NONE',  ( -9.205317785249999218, 1445.523818337909915, 184.6644746700980022 ) ) ;
#9858 = DIRECTION ( 'NONE',  ( 0.4794255386041804123, 0.000000000000000000, -0.8775825618903850822 ) ) ;
#9859 = CARTESIAN_POINT ( 'NONE',  ( 28.11157287220000001, 1508.133875833430011, 210.2394161656980032 ) ) ;
#9860 = CARTESIAN_POINT ( 'NONE',  ( 19.38471501534730024, 1467.100108073059801, 225.4733628320850300 ) ) ;
#9861 = CARTESIAN_POINT ( 'NONE',  ( -25.59041975919999601, 1436.636834531569775, 137.1827113295979927 ) ) ;
#9862 = CARTESIAN_POINT ( 'NONE',  ( 3.268235720634999897, 1516.890356958860139, 211.9874346545169885 ) ) ;
#9863 = CARTESIAN_POINT ( 'NONE',  ( -68.59837639049999325, 1379.747520377230103, 279.7248781293590127 ) ) ;
#9864 = CARTESIAN_POINT ( 'NONE',  ( 9.273172440071220990, 1436.467920671469983, 210.7384122601949912 ) ) ;
#9865 = CARTESIAN_POINT ( 'NONE',  ( -30.25956561551428692, 1524.775785348137561, 221.7839847446165606 ) ) ;
#9867 = CARTESIAN_POINT ( 'NONE',  ( 13.84584525154450141, 1499.900191053290200, 227.7510545287100001 ) ) ;
#9866 = CIRCLE ( 'NONE', #70828, 7.999657266239995401 ) ;
#9868 = CARTESIAN_POINT ( 'NONE',  ( 0.7374508827770021036, 1516.978425811520083, 207.9881927911069965 ) ) ;
#9869 = ORIENTED_EDGE ( 'NONE', *, *, #94615, .F. ) ;
#9870 = CARTESIAN_POINT ( 'NONE',  ( 5.992819232552550446, 1405.413060387330006, 220.0916279853276762 ) ) ;
#9871 = FACE_OUTER_BOUND ( 'NONE', #80006, .T. ) ;
#9872 = CARTESIAN_POINT ( 'NONE',  ( -19.17332639309999820, 1385.003280231690042, 220.5251654938589922 ) ) ;
#9873 = ORIENTED_EDGE ( 'NONE', *, *, #15782, .F. ) ;
#9874 = CARTESIAN_POINT ( 'NONE',  ( -18.64720036659560165, 1385.281482332319911, 220.4066171626870130 ) ) ;
#9875 = CARTESIAN_POINT ( 'NONE',  ( 7.012921545474999796, 1509.051704408389924, 209.1218459511669892 ) ) ;
#9876 = CARTESIAN_POINT ( 'NONE',  ( 11.62509077527690060, 1435.026956746350152, 151.3666508164980087 ) ) ;
#9877 = CARTESIAN_POINT ( 'NONE',  ( 4.603045327887139493, 1488.403330520399777, 234.9096270858480011 ) ) ;
#9878 = CARTESIAN_POINT ( 'NONE',  ( -22.95450442767450028, 1508.996452064000096, 225.0504402230399990 ) ) ;
#9879 = CARTESIAN_POINT ( 'NONE',  ( -1.881591706919999885, 1409.481719852029983, 186.4035628224980030 ) ) ;
#9880 = CARTESIAN_POINT ( 'NONE',  ( 4.429742651635811157, 1508.551704408389924, 213.9240872047329844 ) ) ;
#9881 = CARTESIAN_POINT ( 'NONE',  ( -0.09674472009071061196, 1420.453443083549928, 182.7061723080140041 ) ) ;
#9882 = EDGE_CURVE ( 'NONE', #51216, #90273, #20818, .T. ) ;
#9884 = CARTESIAN_POINT ( 'NONE',  ( -2.534204888539999700, 1421.318133561829882, 184.2270942479979965 ) ) ;
#9883 = CARTESIAN_POINT ( 'NONE',  ( -5.776491133374999976, 1516.858301627840092, 214.9045953718370185 ) ) ;
#9885 = CARTESIAN_POINT ( 'NONE',  ( -8.866353092783899825, 1385.153809896229859, 218.6758262535360018 ) ) ;
#9886 = CARTESIAN_POINT ( 'NONE',  ( 18.32525213847251777, 1425.583872255219831, 224.3060837807782946 ) ) ;
#9887 = ORIENTED_EDGE ( 'NONE', *, *, #78622, .T. ) ;
#9888 = CARTESIAN_POINT ( 'NONE',  ( -12.86029672965840120, 1416.218865267220053, 196.5491407428460207 ) ) ;
#9889 = CARTESIAN_POINT ( 'NONE',  ( -16.32510252680000207, 1490.513422153330112, 186.1369888929979766 ) ) ;
#9890 = VERTEX_POINT ( 'NONE', #9705 ) ;
#9891 = CARTESIAN_POINT ( 'NONE',  ( 2.632631803615880450, 1417.642869435429930, 234.7516633181379859 ) ) ;
#9892 = CARTESIAN_POINT ( 'NONE',  ( -8.331757017630000206, 1505.205016750989898, 208.8972188790260134 ) ) ;
#9893 = CARTESIAN_POINT ( 'NONE',  ( -16.81223434880759982, 1414.913060387349788, 207.5743820648510223 ) ) ;
#9894 = UNCERTAINTY_MEASURE_WITH_UNIT (LENGTH_MEASURE( 1.000000000000000082E-05 ), #22054, 'distance_accuracy_value', 'NONE');
#9895 = DIRECTION ( 'NONE',  ( -0.5896169998278202318, 0.8072987820615146193, 0.02490923515557254622 ) ) ;
#9896 = CARTESIAN_POINT ( 'NONE',  ( -32.39315898239558322, 1526.178928173327904, 201.3122567411319324 ) ) ;
#9897 = FACE_OUTER_BOUND ( 'NONE', #68520, .T. ) ;
#9898 = EDGE_CURVE ( 'NONE', #5600, #34770, #37901, .T. ) ;
#9899 = CARTESIAN_POINT ( 'NONE',  ( -2.713767578570000172, 1447.666021099130148, 156.1534018598979969 ) ) ;
#9900 = CARTESIAN_POINT ( 'NONE',  ( -28.62254820377545528, 1526.345556099435726, 220.1905584258470867 ) ) ;
#9901 = LINE ( 'NONE', #22957, #48489 ) ;
#9902 = CARTESIAN_POINT ( 'NONE',  ( -9.804877192300001099, 1442.756953654919926, 148.8379299677979759 ) ) ;
#9903 = CARTESIAN_POINT ( 'NONE',  ( 17.64666381520000016, 1438.546942878890150, 190.9554714633979984 ) ) ;
#9905 = DIRECTION ( 'NONE',  ( 1.755985294532464991E-16, -1.000000000000000000, 1.338183447452830017E-16 ) ) ;
#9904 = CARTESIAN_POINT ( 'NONE',  ( -2.140897214623600053, 1421.480990132170064, 193.7252737798519888 ) ) ;
#9906 = CARTESIAN_POINT ( 'NONE',  ( 6.742044244646490547, 1509.032357808383040, 202.0097227829280655 ) ) ;
#9907 = VERTEX_POINT ( 'NONE', #72933 ) ;
#9908 = CARTESIAN_POINT ( 'NONE',  ( 1.551584912920709991, 1415.778512721559764, 190.5885286268029972 ) ) ;
#9909 = CARTESIAN_POINT ( 'NONE',  ( 23.40737871429999828, 1430.466916175329970, 206.2070977998880039 ) ) ;
#9910 = CARTESIAN_POINT ( 'NONE',  ( -11.90004737883514885, 1434.917734999592540, 147.6452089151140683 ) ) ;
#9911 = CARTESIAN_POINT ( 'NONE',  ( 9.651066088509999474, 1425.440658930580184, 195.4941615409990163 ) ) ;
#9912 = CARTESIAN_POINT ( 'NONE',  ( -6.647330431358690284, 1519.551704408389924, 184.4413780136169976 ) ) ;
#9913 = CARTESIAN_POINT ( 'NONE',  ( 33.91369266730000476, 1450.440660192670066, 136.2454535554979884 ) ) ;
#9914 = DIRECTION ( 'NONE',  ( 0.000000000000000000, 1.000000000000000000, 0.000000000000000000 ) ) ;
#9915 = DIRECTION ( 'NONE',  ( 0.01668530547205106240, -0.7071067811868640973, -0.7069098956591685079 ) ) ;
#9916 = CARTESIAN_POINT ( 'NONE',  ( -4.038582019099999698, 1515.598601288489817, 209.1218459616829932 ) ) ;
#9917 = CARTESIAN_POINT ( 'NONE',  ( -96.51683378141680691, 1383.766218890880054, 310.1534002763809781 ) ) ;
#9918 = AXIS2_PLACEMENT_3D ( 'NONE', #31273, #23417, #33456 ) ;
#9919 = DIRECTION ( 'NONE',  ( -0.9126757963125582407, 0.3056501852620481241, 0.2712947752436700721 ) ) ;
#9920 = CARTESIAN_POINT ( 'NONE',  ( -15.31956810097295296, 1506.436298843622581, 224.8905146749963819 ) ) ;
#9921 = CARTESIAN_POINT ( 'NONE',  ( -23.35503329776611636, 1410.253263646306095, 210.2532719333120781 ) ) ;
#9923 = VERTEX_POINT ( 'NONE', #105992 ) ;
#9922 = CARTESIAN_POINT ( 'NONE',  ( 10.35952170215530010, 1451.661118394300047, 207.3115203362889929 ) ) ;
#9924 = CARTESIAN_POINT ( 'NONE',  ( -1.547463840030000037, 1414.913060387329779, 225.9340782259980074 ) ) ;
#9925 = CARTESIAN_POINT ( 'NONE',  ( -65.46515651720000051, 1380.024545039450004, 282.7246703598589761 ) ) ;
#9926 = EDGE_CURVE ( 'NONE', #70320, #30342, #29781, .T. ) ;
#9927 = CARTESIAN_POINT ( 'NONE',  ( 20.32615318336489807, 1509.499165376259953, 230.1903333978989963 ) ) ;
#9928 = VERTEX_POINT ( 'NONE', #56123 ) ;
#9929 = EDGE_LOOP ( 'NONE', ( #45291, #37348, #100870, #105757 ) ) ;
#9930 = CARTESIAN_POINT ( 'NONE',  ( 18.96125632730090160, 1509.596089392960039, 231.8852599957560017 ) ) ;
#9931 = CARTESIAN_POINT ( 'NONE',  ( -4.772349923247530157, 1461.586223916219978, 228.1255533131570132 ) ) ;
#9932 = CARTESIAN_POINT ( 'NONE',  ( 37.67547422206740748, 1438.363447988549979, 136.5885122490469996 ) ) ;
#9934 = CARTESIAN_POINT ( 'NONE',  ( 5.161034791280000533, 1485.814572579490005, 218.5690567784690188 ) ) ;
#9933 = PLANE ( 'NONE',  #92465 ) ;
#9935 = ADVANCED_FACE ( 'NONE', ( #107073 ), #37671, .T. ) ;
#9936 = CARTESIAN_POINT ( 'NONE',  ( 11.75869035456349998, 1517.051704408389924, 227.2994842691620079 ) ) ;
#9937 = CARTESIAN_POINT ( 'NONE',  ( -109.6436185679999937, 1384.428537382530067, 297.1050702840590247 ) ) ;
#9938 = EDGE_CURVE ( 'NONE', #39550, #98801, #103308, .T. ) ;
#9939 = CARTESIAN_POINT ( 'NONE',  ( -11.44352787233476043, 1434.730410361278018, 151.4668307198162438 ) ) ;
#9940 = CARTESIAN_POINT ( 'NONE',  ( -20.21110395610000054, 1486.183523693229972, 190.5939432119980097 ) ) ;
#9941 = CARTESIAN_POINT ( 'NONE',  ( 1.519174826900000053, 1408.966111141229931, 186.7972504656979993 ) ) ;
#9942 = CARTESIAN_POINT ( 'NONE',  ( 4.677467455710000444, 1423.717330411029934, 184.5524840891980034 ) ) ;
#9943 = CARTESIAN_POINT ( 'NONE',  ( -7.492225609940000197, 1440.568648358839937, 154.1013270938980213 ) ) ;
#9944 = CARTESIAN_POINT ( 'NONE',  ( 8.249347533650759345, 1435.329610800189812, 206.3473214876380268 ) ) ;
#9945 = CARTESIAN_POINT ( 'NONE',  ( -15.49276695593840181, 1421.101837051059874, 203.4317233017570175 ) ) ;
#9946 = EDGE_CURVE ( 'NONE', #60953, #95904, #32538, .T. ) ;
#9947 = CARTESIAN_POINT ( 'NONE',  ( 2.867004424349999752E-15, 1452.913060387330006, 152.5211338456980172 ) ) ;
#9948 = CARTESIAN_POINT ( 'NONE',  ( 3.535327672168380175, 1487.160996015089950, 197.6951163816430039 ) ) ;
#9949 = ORIENTED_EDGE ( 'NONE', *, *, #91847, .F. ) ;
#9950 = CARTESIAN_POINT ( 'NONE',  ( -18.64646848361585896, 1416.843574578169637, 208.5596655484202131 ) ) ;
#9951 = CARTESIAN_POINT ( 'NONE',  ( 18.27173588000000137, 1474.555276297389810, 194.7671755014989969 ) ) ;
#9952 = CARTESIAN_POINT ( 'NONE',  ( -40.91723400889999596, 1454.696300030829889, 269.9723865689980471 ) ) ;
#9953 = DIRECTION ( 'NONE',  ( 0.1402804634178727861, 0.9901118076173351934, 0.000000000000000000 ) ) ;
#9954 = CARTESIAN_POINT ( 'NONE',  ( 11.96661585360000046, 1440.449248668989867, 150.8629738177980073 ) ) ;
#9955 = CARTESIAN_POINT ( 'NONE',  ( -14.16989796120989986, 1420.440730658529901, 227.4201728071160176 ) ) ;
#9956 = CARTESIAN_POINT ( 'NONE',  ( 10.03739716579999808, 1408.913060387329779, 194.4246222393980190 ) ) ;
#9957 = CARTESIAN_POINT ( 'NONE',  ( 2.845478396016010159, 1409.147963385939875, 230.8055523966380065 ) ) ;
#9958 = CARTESIAN_POINT ( 'NONE',  ( -11.65521739912845156, 1507.535655403029295, 207.9035470747624004 ) ) ;
#9959 = CARTESIAN_POINT ( 'NONE',  ( -4.836546735790000717, 1417.127067430429861, 232.4758270233980113 ) ) ;
#9960 = AXIS2_PLACEMENT_3D ( 'NONE', #16842, #8463, #102517 ) ;
#9961 =( BOUNDED_SURFACE ( )  B_SPLINE_SURFACE ( 3, 2, ( 
 ( #10162, #79049, #77922 ),
 ( #35929, #19658, #19090 ),
 ( #26402, #28064, #43230 ),
 ( #70113, #69553, #45451 ),
 ( #60595, #2351, #71209 ),
 ( #2896, #104225, #105330 ),
 ( #95278, #78479, #43771 ),
 ( #27514, #37015, #94156 ),
 ( #61699, #17426, #53862 ),
 ( #35366, #36466, #680 ) ),
 .UNSPECIFIED., .F., .F., .T. ) 
 B_SPLINE_SURFACE_WITH_KNOTS ( ( 4, 2, 2, 2, 4 ),
 ( 3, 3 ),
 ( 0.000000000000000000, 0.3926990816987241395, 0.7853981633974482790, 1.178097245096172418, 1.570796326794896558 ),
 ( 0.000000000000000000, 1.000000000000000000 ),
 .UNSPECIFIED. ) 
 GEOMETRIC_REPRESENTATION_ITEM ( )  RATIONAL_B_SPLINE_SURFACE ( (
 ( 1.000000000000000000, 0.7763623250684335009, 1.000000000000000000),
 ( 1.000000000000000000, 0.7763684247036998221, 1.000000000000000000),
 ( 1.000000000000000000, 0.7746454561794836602, 1.000000000000000000),
 ( 1.000000000000000000, 0.7679730451975640415, 1.000000000000000000),
 ( 1.000000000000000000, 0.7630177051946724909, 1.000000000000000000),
 ( 1.000000000000000000, 0.7504512394528233266, 1.000000000000000000),
 ( 1.000000000000000000, 0.7428408967931069418, 1.000000000000000000),
 ( 1.000000000000000000, 0.7259222650906337337, 1.000000000000000000),
 ( 1.000000000000000000, 0.7166207884822691776, 1.000000000000000000),
 ( 1.000000000000000000, 0.7071067811865863195, 1.000000000000000000) ) ) 
 REPRESENTATION_ITEM ( '' )  SURFACE ( )  );
#9962 = CARTESIAN_POINT ( 'NONE',  ( -9.082109893440000192, 1460.473744250790105, 214.5004399023289920 ) ) ;
#9963 = CARTESIAN_POINT ( 'NONE',  ( -2.380813228419999650, 1360.502616939890004, 207.6218459616989946 ) ) ;
#9964 = CARTESIAN_POINT ( 'NONE',  ( -46.03694284678339699, 1438.255879967419787, 266.9758360327800233 ) ) ;
#9965 = CARTESIAN_POINT ( 'NONE',  ( -3.084747516479999785, 1428.738071243629975, 185.6021225283980129 ) ) ;
#9966 = ORIENTED_EDGE ( 'NONE', *, *, #23721, .T. ) ;
#9967 = CARTESIAN_POINT ( 'NONE',  ( -8.754460142190000127, 1423.123606144270070, 210.6600973048190042 ) ) ;
#9968 = VERTEX_POINT ( 'NONE', #90816 ) ;
#9969 = CARTESIAN_POINT ( 'NONE',  ( -2.286472924554999953, 1516.883361325900069, 209.8798303522490016 ) ) ;
#9970 = DIRECTION ( 'NONE',  ( 1.000000000000000000, 0.000000000000000000, 0.000000000000000000 ) ) ;
#9971 = EDGE_CURVE ( 'NONE', #98841, #36566, #1819, .T. ) ;
#9972 = CARTESIAN_POINT ( 'NONE',  ( 19.26056229662549413, 1456.232671275964321, 224.9627812116155781 ) ) ;
#9973 = CARTESIAN_POINT ( 'NONE',  ( 7.503182177443590284, 1425.966042803340088, 212.3089147954889881 ) ) ;
#9974 = CARTESIAN_POINT ( 'NONE',  ( 0.5135640108309369456, 1496.071902881799815, 221.4546726054459782 ) ) ;
#9975 = ORIENTED_EDGE ( 'NONE', *, *, #53523, .T. ) ;
#9976 = CARTESIAN_POINT ( 'NONE',  ( -13.97534115310000047, 1452.817890303329932, 195.2694346246979933 ) ) ;
#9978 = CARTESIAN_POINT ( 'NONE',  ( -14.77306020744990001, 1514.147575501819802, 224.0927055486180279 ) ) ;
#9977 = CARTESIAN_POINT ( 'NONE',  ( 5.068064628910000202, 1505.106222020589939, 220.8372522273990057 ) ) ;
#9979 = EDGE_CURVE ( 'NONE', #93351, #6492, #101916, .T. ) ;
#9980 = CARTESIAN_POINT ( 'NONE',  ( 7.329930013194999816, 1516.881930554049859, 201.4037113026670056 ) ) ;
#9981 = CARTESIAN_POINT ( 'NONE',  ( -16.85913248346849969, 1508.551704408389924, 212.7777254685370281 ) ) ;
#9982 = CARTESIAN_POINT ( 'NONE',  ( 4.617353517619999792, 1460.098150474590057, 228.0971968620989969 ) ) ;
#9983 = CARTESIAN_POINT ( 'NONE',  ( -9.526124601274780446, 1440.436526369470130, 205.9994947568980024 ) ) ;
#9984 = EDGE_LOOP ( 'NONE', ( #89008, #49247, #90211, #108020 ) ) ;
#9985 = CARTESIAN_POINT ( 'NONE',  ( -4.780671213366310290, 1410.433596435060053, 269.6173310763380186 ) ) ;
#9986 = CARTESIAN_POINT ( 'NONE',  ( 5.772978278544999675, 1516.659138130710289, 207.9900491214870044 ) ) ;
#9987 = CARTESIAN_POINT ( 'NONE',  ( 4.696240690070100143, 1417.218906874169988, 231.8673332382849992 ) ) ;
#9988 = CARTESIAN_POINT ( 'NONE',  ( -18.20496907859999780, 1430.287838494730067, 193.4343735864979976 ) ) ;
#9990 = ORIENTED_EDGE ( 'NONE', *, *, #76663, .F. ) ;
#9989 = CARTESIAN_POINT ( 'NONE',  ( -5.236338392940000475, 1368.774323667059889, 207.6218459616989946 ) ) ;
#9991 = ORIENTED_EDGE ( 'NONE', *, *, #87778, .T. ) ;
#9992 = CARTESIAN_POINT ( 'NONE',  ( -23.72163544602249630, 1410.855579502579985, 210.2587994297539922 ) ) ;
#9993 = CARTESIAN_POINT ( 'NONE',  ( -4.229370274619999925, 1423.902571003530056, 184.2263527321979950 ) ) ;
#9994 = CARTESIAN_POINT ( 'NONE',  ( 3.686304469464770861, 1424.203457939092914, 183.9872173849159083 ) ) ;
#9995 = CARTESIAN_POINT ( 'NONE',  ( 2.500020115319840031, 1419.382923540379807, 144.1035841389490031 ) ) ;
#9996 = CARTESIAN_POINT ( 'NONE',  ( -19.67328662190290345, 1464.359412933360090, 193.5541274441619919 ) ) ;
#9997 = CARTESIAN_POINT ( 'NONE',  ( -18.41394400640000129, 1420.837661492430016, 224.8930013675980035 ) ) ;
#9998 = VECTOR ( 'NONE', #104191, 1000.000000000000114 ) ;
#9999 = CARTESIAN_POINT ( 'NONE',  ( 38.77362862126869913, 1459.095958665629951, 269.1610570729100118 ) ) ;
#10000 = CARTESIAN_POINT ( 'NONE',  ( -5.032517913996907843, 1466.392609142821584, 234.4269938085604394 ) ) ;
#10001 = CARTESIAN_POINT ( 'NONE',  ( -11.44665353847253186, 1425.798163151176823, 139.1345268192609126 ) ) ;
#10002 = CARTESIAN_POINT ( 'NONE',  ( -0.7572979743539989261, 1516.829948096479939, 205.6721984920870057 ) ) ;
#10003 = ORIENTED_EDGE ( 'NONE', *, *, #22726, .F. ) ;
#10004 = CARTESIAN_POINT ( 'NONE',  ( 1.167418783940000093, 1444.307247415689972, 215.3110397704089962 ) ) ;
#10005 = CARTESIAN_POINT ( 'NONE',  ( 1.483850069390550086, 1475.343092926309737, 182.4989731883329966 ) ) ;
#10006 = CARTESIAN_POINT ( 'NONE',  ( 23.58069158640000040, 1410.392965674430116, 208.0807130311279991 ) ) ;
#10007 = ORIENTED_EDGE ( 'NONE', *, *, #58613, .F. ) ;
#10008 = CARTESIAN_POINT ( 'NONE',  ( 3.865424752145830034, 1508.610338626970133, 204.7110934638159847 ) ) ;
#10009 = CARTESIAN_POINT ( 'NONE',  ( 25.32246794855759831, 1452.028780111509832, 135.3106647663209969 ) ) ;
#10010 = B_SPLINE_SURFACE_WITH_KNOTS ( 'NONE', 5, 5, ( 
 ( #44122, #44679, #104007, #27304, #79375, #20003 ),
 ( #103441, #54195, #36814, #28973, #71570, #105691 ),
 ( #78257, #88322, #79927, #51967, #86108, #9402 ),
 ( #63698, #98911, #91060, #88872, #89965, #48537 ),
 ( #30615, #64802, #21638, #90512, #73176, #55291 ),
 ( #81019, #29504, #47429, #21087, #97809, #81552 ) ),
 .UNSPECIFIED., .F., .F., .F.,
 ( 6, 6 ),
 ( 6, 6 ),
 ( 7.080340024990000813, 12.74512986790000113 ),
 ( 0.000000000000000000, 2.000000000000000000 ),
 .UNSPECIFIED. ) ;
#10011 = CARTESIAN_POINT ( 'NONE',  ( 31.34137657934019927, 1501.977400791986611, 221.9025654077410081 ) ) ;
#10012 = CARTESIAN_POINT ( 'NONE',  ( -8.711610717349350286E-16, 1387.020289398270052, 218.3670623203690013 ) ) ;
#10013 = CARTESIAN_POINT ( 'NONE',  ( -18.63787277242401075, 1508.244465050728877, 229.7911781032966303 ) ) ;
#10014 = CARTESIAN_POINT ( 'NONE',  ( 18.33790473009999999, 1409.718233535930040, 195.1838260118980202 ) ) ;
#10015 = CARTESIAN_POINT ( 'NONE',  ( -3.490466736259999703, 1496.905313612590135, 198.4270292345989901 ) ) ;
#10016 = CARTESIAN_POINT ( 'NONE',  ( 3.374891144018687505, 1439.690136908176555, 184.4234125476535269 ) ) ;
#10018 = CARTESIAN_POINT ( 'NONE',  ( -21.84936520677460337, 1429.838685647439434, 218.4389703241229199 ) ) ;
#10017 = CARTESIAN_POINT ( 'NONE',  ( -3.208637323093683769, 1515.551704408389924, 205.2922258736341519 ) ) ;
#10019 = CARTESIAN_POINT ( 'NONE',  ( 8.774939133739998454, 1409.219488014130093, 228.7704650873980086 ) ) ;
#10020 = DIRECTION ( 'NONE',  ( -0.9455185755993178454, 0.000000000000000000, 0.3255681544571537578 ) ) ;
#10021 = CARTESIAN_POINT ( 'NONE',  ( -9.959589622450000235, 1382.751681251990021, 218.0704319110489848 ) ) ;
#10022 = CARTESIAN_POINT ( 'NONE',  ( -3.449149233875000053, 1516.947419719950176, 213.7456339395970133 ) ) ;
#10023 = CARTESIAN_POINT ( 'NONE',  ( 2.744860781518606352, 1525.790286462510267, 240.9440847703890256 ) ) ;
#10024 = ORIENTED_EDGE ( 'NONE', *, *, #50153, .F. ) ;
#10025 = CARTESIAN_POINT ( 'NONE',  ( -17.37965410361753982, 1465.838514868465154, 219.1858979602013164 ) ) ;
#10026 = CARTESIAN_POINT ( 'NONE',  ( -2.940338105849999994, 1463.323050212790122, 228.6636231251989955 ) ) ;
#10027 = CARTESIAN_POINT ( 'NONE',  ( -0.2712437013090800431, 1408.932510966370273, 231.9264321468249932 ) ) ;
#10028 = AXIS2_PLACEMENT_3D ( 'NONE', #72051, #2630, #72576 ) ;
#10029 = AXIS2_PLACEMENT_3D ( 'NONE', #12417, #46602, #4045 ) ;
#10030 = CARTESIAN_POINT ( 'NONE',  ( -21.12854634993719927, 1507.715432715349834, 209.4790063854959783 ) ) ;
#10031 = DIRECTION ( 'NONE',  ( 0.8090169943749551118, 0.000000000000000000, 0.5877852522924625900 ) ) ;
#10032 = CARTESIAN_POINT ( 'NONE',  ( -4.328818125147580353, 1515.088876468550097, 207.8567422199149917 ) ) ;
#10033 = CARTESIAN_POINT ( 'NONE',  ( -6.509745555140000306, 1455.357238135929947, 219.6133830849979915 ) ) ;
#10034 = DIRECTION ( 'NONE',  ( -0.9942586961433758086, 0.000000000000000000, -0.1070030146457303932 ) ) ;
#10035 = CARTESIAN_POINT ( 'NONE',  ( 11.86680595310000008, 1433.219746834359967, 150.3047385607980004 ) ) ;
#10036 = CARTESIAN_POINT ( 'NONE',  ( 20.41675352909999930, 1440.913060387330006, 219.6133834379979817 ) ) ;
#10037 = DIRECTION ( 'NONE',  ( 0.9980318515193558060, 0.000000000000000000, 0.06270903725019710828 ) ) ;
#10038 = B_SPLINE_CURVE_WITH_KNOTS ( 'NONE', 3,
 ( #20130, #63820, #55959, #97934, #71130, #47013, #106347, #80602, #81676, #62173, #28544, #105251, #81138, #4982, #72225, #20665, #96299, #63281, #54866, #105818, #45370, #88453, #11741, #62743, #3368, #27988, #19579, #11206, #96862, #46471, #21758, #89543, #45910, #80046, #37494, #2814, #71698, #72760, #38581, #53781, #38048, #64368, #55411 ),
 .UNSPECIFIED., .F., .F.,
 ( 4, 3, 3, 3, 3, 3, 3, 3, 3, 3, 3, 3, 3, 3, 4 ),
 ( 0.7655572723410000169, 0.9910019214004439636, 1.224379696603769885, 1.462078613819520090, 1.704827352795679873, 1.793853281190000093, 2.038466587732339796, 2.281256468177419894, 2.316155491850000026, 2.583989317132500130, 2.855920919038569927, 3.139267318828499853, 3.387490792979999554, 3.680707183893040302, 3.835724788489999426 ),
 .UNSPECIFIED. ) ;
#10039 = CARTESIAN_POINT ( 'NONE',  ( -17.69729716890000049, 1420.080679157370014, 207.3677048410189911 ) ) ;
#10040 = CARTESIAN_POINT ( 'NONE',  ( 9.627620378001870094, 1463.988716367230154, 211.0622702830050059 ) ) ;
#10041 = CARTESIAN_POINT ( 'NONE',  ( -12.25055778059999945, 1486.242977004730164, 184.4831925055979980 ) ) ;
#10042 = CARTESIAN_POINT ( 'NONE',  ( -6.520294809802511971, 1509.032998946479893, 201.8615409552149913 ) ) ;
#10043 = CARTESIAN_POINT ( 'NONE',  ( -21.72141783274009796, 1509.710993503089867, 231.6292274468669916 ) ) ;
#10044 = CARTESIAN_POINT ( 'NONE',  ( 24.89847827690000059, 1430.363150105230034, 209.6261949212619982 ) ) ;
#10045 = CARTESIAN_POINT ( 'NONE',  ( -15.99542386634146851, 1420.238047865418366, 209.6726076052734982 ) ) ;
#10046 = DIRECTION ( 'NONE',  ( 0.1070030146457445069, 0.000000000000000000, 0.9942586961433742543 ) ) ;
#10047 = CARTESIAN_POINT ( 'NONE',  ( -13.22271691091419932, 1383.860216996029976, 218.9433012605030058 ) ) ;
#10048 = CARTESIAN_POINT ( 'NONE',  ( 22.24401333792100033, 1475.958618154809983, 209.7631869422630189 ) ) ;
#10049 = CARTESIAN_POINT ( 'NONE',  ( 4.040527303974999818, 1516.815231249920089, 213.7327841816070020 ) ) ;
#10050 = CARTESIAN_POINT ( 'NONE',  ( 2173.981453289206911, -8382.262153571264207, -1556.947849745907888 ) ) ;
#10051 = CARTESIAN_POINT ( 'NONE',  ( 9.173643782033812144, 1450.994954104630096, 210.2665090766199683 ) ) ;
#10053 = EDGE_LOOP ( 'NONE', ( #8259, #3877, #19761, #84650 ) ) ;
#10052 = CARTESIAN_POINT ( 'NONE',  ( 3.991437517280000513, 1441.662116857989986, 217.1481707352390060 ) ) ;
#10054 = CARTESIAN_POINT ( 'NONE',  ( -1.341974385850000173, 1416.832348306829999, 228.0804724305980073 ) ) ;
#10055 = CARTESIAN_POINT ( 'NONE',  ( -8.325264604675567170, 1386.880005921131669, 199.8668364905755368 ) ) ;
#10056 = EDGE_CURVE ( 'NONE', #76758, #20056, #98578, .T. ) ;
#10057 = CARTESIAN_POINT ( 'NONE',  ( -5.487972707081399726, 1440.608688506979888, 154.7779097410979716 ) ) ;
#10059 = ORIENTED_EDGE ( 'NONE', *, *, #8351, .T. ) ;
#10058 = CARTESIAN_POINT ( 'NONE',  ( -32.38114538885245963, 1523.604703353109699, 216.1203639561433363 ) ) ;
#10060 = CARTESIAN_POINT ( 'NONE',  ( 3.217406951622789890, 1424.184472523990053, 188.9579968088540056 ) ) ;
#10061 = EDGE_LOOP ( 'NONE', ( #103361, #87408, #19164 ) ) ;
#10062 = CARTESIAN_POINT ( 'NONE',  ( -14.37394065297739942, 1380.292840319920060, 209.5077344925099965 ) ) ;
#10063 = CARTESIAN_POINT ( 'NONE',  ( -15.66638209299999929, 1416.825421876430028, 219.1964221495979928 ) ) ;
#10064 = CARTESIAN_POINT ( 'NONE',  ( -1.086003861333974196, 1508.993070980561242, 238.8005286751018446 ) ) ;
#10065 = CARTESIAN_POINT ( 'NONE',  ( -2.941554235803736539, 1368.542299806011442, 210.4699219221472219 ) ) ;
#10066 = CARTESIAN_POINT ( 'NONE',  ( -0.7593982673170009967, 1430.316802068590050, 217.4503154216889982 ) ) ;
#10067 = CARTESIAN_POINT ( 'NONE',  ( -10.52582819352379850, 1471.840167648990018, 206.9753088315659966 ) ) ;
#10068 = CARTESIAN_POINT ( 'NONE',  ( 14.76663485449640056, 1409.428722639259831, 206.8871449305759711 ) ) ;
#10069 = CARTESIAN_POINT ( 'NONE',  ( -11.65327852769999950, 1391.913060471080144, 207.1342100345190147 ) ) ;
#10070 = CARTESIAN_POINT ( 'NONE',  ( -71.11683232987380165, 1385.117871785510260, 268.1819042305770040 ) ) ;
#10071 = CARTESIAN_POINT ( 'NONE',  ( -17.63837303440000426, 1411.935330354230018, 193.4048893071979762 ) ) ;
#10072 = CARTESIAN_POINT ( 'NONE',  ( -65.00001850430001582, 1379.749314314899948, 272.6104031607590059 ) ) ;
#10073 = ORIENTED_EDGE ( 'NONE', *, *, #7158, .T. ) ;
#10074 = CARTESIAN_POINT ( 'NONE',  ( 11.26469520917990152, 1491.013796966650261, 207.1901082836730268 ) ) ;
#10075 = ADVANCED_FACE ( 'NONE', ( #98668 ), #75687, .F. ) ;
#10077 = ORIENTED_EDGE ( 'NONE', *, *, #19715, .T. ) ;
#10076 = CARTESIAN_POINT ( 'NONE',  ( -3.381226883360950008, 1438.609729080699935, 227.4063576580390134 ) ) ;
#10078 = DIRECTION ( 'NONE',  ( -0.02701649886402238826, 0.9995674067478985680, -0.01162360341768371545 ) ) ;
#10079 = ORIENTED_EDGE ( 'NONE', *, *, #91961, .F. ) ;
#10080 = CARTESIAN_POINT ( 'NONE',  ( -13.13561839920526886, 1522.051704408389924, 208.3084799397878157 ) ) ;
#10081 = CARTESIAN_POINT ( 'NONE',  ( -8.572405811665989361, 1363.936666048608004, 207.6218459616988241 ) ) ;
#10082 = CARTESIAN_POINT ( 'NONE',  ( -2.599202470067710102, 1495.843114574169931, 197.0638286399839672 ) ) ;
#10083 = EDGE_CURVE ( 'NONE', #59101, #68673, #63773, .T. ) ;
#10084 = CARTESIAN_POINT ( 'NONE',  ( 35.06721089139576719, 1457.701433636751972, 269.5324293830444731 ) ) ;
#10085 = CYLINDRICAL_SURFACE ( 'NONE', #48110, 1.999999999999994449 ) ;
#10086 = CARTESIAN_POINT ( 'NONE',  ( -28.25086642335310216, 1508.135711581739997, 208.8579954535609886 ) ) ;
#10087 = CARTESIAN_POINT ( 'NONE',  ( 8.456465142934460388, 1522.051704408389924, 223.1002094411418284 ) ) ;
#10088 = CARTESIAN_POINT ( 'NONE',  ( -7.075104946580074383, 1516.558315471130072, 211.6107311714952175 ) ) ;
#10089 = DIRECTION ( 'NONE',  ( -1.755985294532469921E-16, 1.000000000000000000, -1.338183447452831989E-16 ) ) ;
#10090 = CARTESIAN_POINT ( 'NONE',  ( -4.517103278720104420, 1368.953374755371897, 210.6218459616991936 ) ) ;
#10091 = CARTESIAN_POINT ( 'NONE',  ( -19.58495063083499943, 1485.885833950319920, 202.2948491896230223 ) ) ;
#10092 = FACE_OUTER_BOUND ( 'NONE', #55577, .T. ) ;
#10093 = CARTESIAN_POINT ( 'NONE',  ( -2.493699806765000027, 1516.858326417339867, 206.6451124560869914 ) ) ;
#10094 = DIRECTION ( 'NONE',  ( 5.980589973904019347E-17, -1.000000000000000000, 1.736889445713099699E-16 ) ) ;
#10095 = DIRECTION ( 'NONE',  ( -0.9990982087154917091, 0.04245902717575712748, -1.878255039611807006E-05 ) ) ;
#10096 = CARTESIAN_POINT ( 'NONE',  ( 14.00875066949999947, 1416.819760216229952, 196.3921940529979793 ) ) ;
#10098 = ORIENTED_EDGE ( 'NONE', *, *, #17104, .F. ) ;
#10097 = CARTESIAN_POINT ( 'NONE',  ( -3.156992497350000093, 1496.318815817190170, 220.0352492536989928 ) ) ;
#10099 = B_SPLINE_CURVE_WITH_KNOTS ( 'NONE', 3,
 ( #81766, #31922, #21842, #66661 ),
 .UNSPECIFIED., .F., .F.,
 ( 4, 4 ),
 ( -21.94916620480000091, -5.186424823540001228 ),
 .UNSPECIFIED. ) ;
#10100 = CIRCLE ( 'NONE', #80187, 830.3529813948301808 ) ;
#10101 = DIRECTION ( 'NONE',  ( -0.9786619618251657382, 0.000000000000000000, 0.2054769195713179730 ) ) ;
#10102 = ORIENTED_EDGE ( 'NONE', *, *, #29058, .F. ) ;
#10103 = DIRECTION ( 'NONE',  ( 1.836970198721029688E-16, 1.000000000000000000, -7.703719777548939991E-34 ) ) ;
#10104 = CARTESIAN_POINT ( 'NONE',  ( -27.16947874219999903, 1488.689296590230015, 207.4688266076479692 ) ) ;
#10106 = CARTESIAN_POINT ( 'NONE',  ( 16.57702714126169852, 1410.724566313010200, 191.7206609563160100 ) ) ;
#10105 = CARTESIAN_POINT ( 'NONE',  ( -10.45732730569119795, 1425.117602760000182, 121.9097720391450110 ) ) ;
#10107 = CARTESIAN_POINT ( 'NONE',  ( -1.701729858475000023, 1516.969638403840008, 212.0041719496170174 ) ) ;
#10108 = EDGE_CURVE ( 'NONE', #63621, #79273, #58409, .T. ) ;
#10109 = CARTESIAN_POINT ( 'NONE',  ( 12.44492264844295448, 1509.471699171668433, 181.7748644473435604 ) ) ;
#10110 = CARTESIAN_POINT ( 'NONE',  ( -22.11623627239999834, 1489.468502498230009, 207.6017525449580035 ) ) ;
#10111 = CARTESIAN_POINT ( 'NONE',  ( -33.66409354169999801, 1434.352089750010236, 250.0355534200980401 ) ) ;
#10112 = CARTESIAN_POINT ( 'NONE',  ( 17.56822049365750260, 1509.536650904990211, 232.8514770280130222 ) ) ;
#10113 = CARTESIAN_POINT ( 'NONE',  ( 28.70934402868200408, 1509.343126748570285, 209.4988959437390292 ) ) ;
#10114 = CARTESIAN_POINT ( 'NONE',  ( -5.263807122380000258, 1391.914765277889956, 214.5215612962889793 ) ) ;
#10115 = CARTESIAN_POINT ( 'NONE',  ( 33.12914009259999659, 1451.756166416729911, 134.7383383604980054 ) ) ;
#10116 = ORIENTED_EDGE ( 'NONE', *, *, #82206, .T. ) ;
#10117 = CARTESIAN_POINT ( 'NONE',  ( 11.14207291371160125, 1397.935304532519922, 216.8346386145179849 ) ) ;
#10119 = AXIS2_PLACEMENT_3D ( 'NONE', #88643, #64001, #56680 ) ;
#10118 = CARTESIAN_POINT ( 'NONE',  ( 9.146190246725058870, 1461.862305004799964, 205.8338018421410140 ) ) ;
#10120 = CARTESIAN_POINT ( 'NONE',  ( -18.47628410029999912, 1457.312873679730046, 229.4267097870979910 ) ) ;
#10121 = ORIENTED_EDGE ( 'NONE', *, *, #96826, .T. ) ;
#10122 = VERTEX_POINT ( 'NONE', #14658 ) ;
#10123 = CARTESIAN_POINT ( 'NONE',  ( -29.23325473176074851, 1509.933901906174697, 211.7644991624144097 ) ) ;
#10124 = CARTESIAN_POINT ( 'NONE',  ( -2.298816259811510054, 1486.462377102800019, 220.8289805423670202 ) ) ;
#10126 = EDGE_LOOP ( 'NONE', ( #95739, #97752, #42264, #66882, #51027, #20805, #34361 ) ) ;
#10125 = B_SPLINE_CURVE_WITH_KNOTS ( 'NONE', 5,
 ( #46570, #80149, #37041, #38140, #20771, #71799, #44926, #3470, #47108, #63387, #97502, #54971, #54431, #89097, #12385, #53318, #79073, #63921, #80705, #62853, #37597, #105918, #4014, #95849, #36495, #106452, #11309, #71235, #29735, #53889 ),
 .UNSPECIFIED., .F., .F.,
 ( 6, 3, 3, 3, 3, 3, 3, 3, 3, 6 ),
 ( 0.000000000000000000, 0.007519188799632491732, 0.01525432589305721759, 0.03846436772750950334, 0.06167440956112346662, 0.1235555043535759567, 0.2624078012577487629, 0.4012600981619215967, 0.5405650403839840079, 1.000000000000000000 ),
 .UNSPECIFIED. ) ;
#10127 = CARTESIAN_POINT ( 'NONE',  ( -1.069244773279999894, 1410.308942914629824, 185.3176740583979836 ) ) ;
#10128 = CARTESIAN_POINT ( 'NONE',  ( 9.484196478038136036, 1446.608455646244693, 153.5742700972787986 ) ) ;
#10129 = LINE ( 'NONE', #70078, #9998 ) ;
#10130 = CARTESIAN_POINT ( 'NONE',  ( -9.474342455649999550, 1470.475897465230219, 232.9250315801980094 ) ) ;
#10131 = CARTESIAN_POINT ( 'NONE',  ( -12.78776258890000150, 1416.851343894929869, 195.7518694485980006 ) ) ;
#10132 =( BOUNDED_CURVE ( )  B_SPLINE_CURVE ( 3, ( #94748, #7437, #58406, #33728 ),
 .UNSPECIFIED., .F., .F. ) 
 B_SPLINE_CURVE_WITH_KNOTS ( ( 4, 4 ),
 ( 4.152341638222174502, 5.272436418961190085 ),
 .UNSPECIFIED. ) 
 CURVE ( )  GEOMETRIC_REPRESENTATION_ITEM ( )  RATIONAL_B_SPLINE_CURVE ( ( 1.000000000000000000, 0.8981532913012172381, 0.8981532913012172381, 1.000000000000000000 ) ) 
 REPRESENTATION_ITEM ( '' )  );
#10133 = CARTESIAN_POINT ( 'NONE',  ( 6.361972252410000195, 1462.343751617889893, 207.5519484895090159 ) ) ;
#10134 = CARTESIAN_POINT ( 'NONE',  ( -96.48208606500890028, 1384.862543659289940, 295.4255336162560184 ) ) ;
#10135 = ORIENTED_EDGE ( 'NONE', *, *, #78317, .T. ) ;
#10136 = CARTESIAN_POINT ( 'NONE',  ( -6.943602691585000208, 1516.858069504249897, 202.1807456543569685 ) ) ;
#10137 = CARTESIAN_POINT ( 'NONE',  ( -3.460866208815000178, 1517.020847257979995, 208.3861469975149987 ) ) ;
#10138 = ORIENTED_EDGE ( 'NONE', *, *, #14374, .T. ) ;
#10139 = CARTESIAN_POINT ( 'NONE',  ( 11.86259848306839970, 1432.091341794900018, 149.9768531085499887 ) ) ;
#10140 = CARTESIAN_POINT ( 'NONE',  ( 13.18251122944204390, 1444.726075940572173, 187.2757804206736978 ) ) ;
#10141 = VERTEX_POINT ( 'NONE', #75142 ) ;
#10142 = CARTESIAN_POINT ( 'NONE',  ( -15.73091603027213914, 1506.446781340835969, 193.7509379680487314 ) ) ;
#10143 = CARTESIAN_POINT ( 'NONE',  ( -7.116759930024330494, 1508.500068961840043, 219.5125775166329731 ) ) ;
#10144 = CARTESIAN_POINT ( 'NONE',  ( 6.924875051240000801, 1507.862635227430019, 235.4241313661979973 ) ) ;
#10145 = CARTESIAN_POINT ( 'NONE',  ( -3.774544273728137611, 1488.811965616022462, 219.3433275354165062 ) ) ;
#10146 = CARTESIAN_POINT ( 'NONE',  ( -5.151887371179999953, 1423.035654755729865, 185.3911223247979763 ) ) ;
#10147 = CARTESIAN_POINT ( 'NONE',  ( 4.814684546780449992, 1410.439504313829957, 269.6173903879380305 ) ) ;
#10148 = CARTESIAN_POINT ( 'NONE',  ( 9.167247559838790139, 1450.084797855079842, 208.2842279015860072 ) ) ;
#10149 = CARTESIAN_POINT ( 'NONE',  ( -12.71213581786250124, 1502.313795877750181, 210.3224788360479920 ) ) ;
#10150 = CARTESIAN_POINT ( 'NONE',  ( 11.16440858570000039, 1492.931605700189948, 213.3458366114890055 ) ) ;
#10151 = CARTESIAN_POINT ( 'NONE',  ( -32.76203973510000367, 1379.634334059360071, 215.8302746649189885 ) ) ;
#10152 = CARTESIAN_POINT ( 'NONE',  ( 0.03022822327178078736, 1410.187553064696885, 233.2131390692366892 ) ) ;
#10154 = DIRECTION ( 'NONE',  ( -0.6736849260863841948, 0.000000000000000000, 0.7390186874254148774 ) ) ;
#10153 = CARTESIAN_POINT ( 'NONE',  ( -21.15335024929999719, 1505.792763867390022, 209.1590586292889782 ) ) ;
#10155 = CARTESIAN_POINT ( 'NONE',  ( 15.17327376946160022, 1507.614846715330032, 226.3720743403030156 ) ) ;
#10156 = CARTESIAN_POINT ( 'NONE',  ( -9.966727850805121136, 1439.480327375449860, 208.4309914983489875 ) ) ;
#10157 = CARTESIAN_POINT ( 'NONE',  ( -5.360126306917530670, 1422.242609447140012, 144.1609271584179908 ) ) ;
#10158 = VERTEX_POINT ( 'NONE', #92457 ) ;
#10159 = CARTESIAN_POINT ( 'NONE',  ( 11.47403709129999960, 1414.639208232530109, 262.6648722416979922 ) ) ;
#10160 = DIRECTION ( 'NONE',  ( 0.000000000000000000, 1.000000000000000000, 0.000000000000000000 ) ) ;
#10161 = CIRCLE ( 'NONE', #60283, 1.999999999999999556 ) ;
#10162 = CARTESIAN_POINT ( 'NONE',  ( -20.71343476517555260, 1522.382868172863937, 179.9059455038196802 ) ) ;
#10163 = CARTESIAN_POINT ( 'NONE',  ( 4.253676957470000630, 1505.389161788490128, 221.1607250897990014 ) ) ;
#10164 = CARTESIAN_POINT ( 'NONE',  ( 204.2714532754872323, 1524.382868172863937, 194.5341519463041777 ) ) ;
#10165 =( BOUNDED_SURFACE ( )  B_SPLINE_SURFACE ( 3, 2, ( 
 ( #91144, #82748, #37996 ),
 ( #39074, #29581, #105764 ),
 ( #64318, #72710, #55914 ),
 ( #98439, #63235, #56454 ),
 ( #97881, #54812, #55361 ),
 ( #3869, #12231, #46421 ),
 ( #21156, #29049, #72179 ),
 ( #81628, #97341, #89494 ),
 ( #90032, #12788, #88939 ),
 ( #14421, #46966, #57019 ),
 ( #106833, #81087, #4404 ),
 ( #73251, #107390, #13866 ),
 ( #30687, #22812, #64874 ),
 ( #98981, #90589, #48051 ),
 ( #82188, #5488, #73816 ),
 ( #107945, #31237, #65420 ),
 ( #99527, #92797, #108500 ),
 ( #49164, #91694, #100100 ) ),
 .UNSPECIFIED., .F., .F., .F. ) 
 B_SPLINE_SURFACE_WITH_KNOTS ( ( 4, 2, 2, 2, 2, 2, 2, 2, 4 ),
 ( 3, 3 ),
 ( -1.056814893231837992E-05, 4.513480273177641422E-05, 0.0001008377543958712084, 0.0002122436577240607966, 0.0004350554643804399732, 0.0008806790776931983263, 0.001326302691005956571, 0.001549114497662335693, 0.001771926304318715032 ),
 ( 0.000000000000000000, 1.000000000000000000 ),
 .UNSPECIFIED. ) 
 GEOMETRIC_REPRESENTATION_ITEM ( )  RATIONAL_B_SPLINE_SURFACE ( (
 ( 1.000000000000000000, 0.8674263646877330425, 1.000000000000000000),
 ( 1.000000000000000000, 0.8678218641029733504, 1.000000000000000000),
 ( 1.000000000000000000, 0.8697758742242241992, 1.000000000000000000),
 ( 1.000000000000000000, 0.8728331949133366630, 1.000000000000000000),
 ( 1.000000000000000000, 0.8743688320447627893, 1.000000000000000000),
 ( 1.000000000000000000, 0.8789934887300921984, 1.000000000000000000),
 ( 1.000000000000000000, 0.8821003874863629912, 1.000000000000000000),
 ( 1.000000000000000000, 0.8914624349615335452, 1.000000000000000000),
 ( 1.000000000000000000, 0.8977612400248787816, 1.000000000000000000),
 ( 1.000000000000000000, 0.9165107280359201525, 1.000000000000000000),
 ( 1.000000000000000000, 0.9288478704676672582, 1.000000000000000000),
 ( 1.000000000000000000, 0.9506413689712427395, 1.000000000000000000),
 ( 1.000000000000000000, 0.9600128686476009365, 1.000000000000000000),
 ( 1.000000000000000000, 0.9692757131723997999, 1.000000000000000000),
 ( 1.000000000000000000, 0.9715763504693073482, 1.000000000000000000),
 ( 1.000000000000000000, 0.9742738933835981552, 1.000000000000000000),
 ( 1.000000000000000000, 0.9746552859465718033, 1.000000000000000000),
 ( 1.000000000000000000, 0.9740159740112075415, 1.000000000000000000) ) ) 
 REPRESENTATION_ITEM ( '' )  SURFACE ( )  );
#10167 = VERTEX_POINT ( 'NONE', #100323 ) ;
#10166 = CARTESIAN_POINT ( 'NONE',  ( 0.1187972039649769912, 1515.157712620099801, 204.7948303746160263 ) ) ;
#10168 = CARTESIAN_POINT ( 'NONE',  ( -15.86842751682814701, 1415.926969301026702, 209.7305162940345440 ) ) ;
#10169 = CARTESIAN_POINT ( 'NONE',  ( -24.31100006580000183, 1442.893711221979856, 212.2583796852279931 ) ) ;
#10170 = CARTESIAN_POINT ( 'NONE',  ( -16.28210776099999890, 1416.583347678280006, 208.7674903396639934 ) ) ;
#10171 = CARTESIAN_POINT ( 'NONE',  ( 1.804110352077529900, 1431.051163599219990, 199.8239164788810172 ) ) ;
#10172 = CARTESIAN_POINT ( 'NONE',  ( -10.50426069749999947, 1440.655587673750006, 187.1572747102979974 ) ) ;
#10173 = LINE ( 'NONE', #691, #62937 ) ;
#10174 = CARTESIAN_POINT ( 'NONE',  ( 13.15712928874680010, 1428.815432648289971, 222.5930086189890176 ) ) ;
#10175 = CARTESIAN_POINT ( 'NONE',  ( -15.24995208726499918, 1513.868118914750085, 224.0843299309669874 ) ) ;
#10176 = CARTESIAN_POINT ( 'NONE',  ( 7.345502919380000328, 1415.074004183030183, 230.9439570329979858 ) ) ;
#10177 = CARTESIAN_POINT ( 'NONE',  ( -10.12886798639999952, 1479.735562891690051, 213.4664817790389861 ) ) ;
#10178 = CARTESIAN_POINT ( 'NONE',  ( -16.73813953200000171, 1460.714426248530117, 228.2661735262979903 ) ) ;
#10179 = CARTESIAN_POINT ( 'NONE',  ( 2.282915183265000092, 1516.876240617270014, 206.6278256496669883 ) ) ;
#10180 = CARTESIAN_POINT ( 'NONE',  ( 31.73325210529999296, 1415.263605584930247, 267.4236301385980710 ) ) ;
#10181 = VECTOR ( 'NONE', #85748, 1000.000000000000114 ) ;
#10182 = CARTESIAN_POINT ( 'NONE',  ( 37.66849513895419932, 1445.052233489950140, 137.0436250799990034 ) ) ;
#10183 = DIRECTION ( 'NONE',  ( -4.481801771516530428E-20, -1.000000000000000000, -2.868959329816139585E-18 ) ) ;
#10184 = CARTESIAN_POINT ( 'NONE',  ( 25.82017203379999870, 1508.004933221630154, 200.5938135955979931 ) ) ;
#10185 = CARTESIAN_POINT ( 'NONE',  ( -22.99624282800000330, 1433.297116904619998, 215.2097649112580200 ) ) ;
#10186 = CARTESIAN_POINT ( 'NONE',  ( -12.32335714446040065, 1378.400099640540020, 208.6449807495420146 ) ) ;
#10187 = CARTESIAN_POINT ( 'NONE',  ( 17.37724426307448411, 1525.394057003702756, 237.0493741307235780 ) ) ;
#10188 = CARTESIAN_POINT ( 'NONE',  ( -1.433829655579999862, 1450.688199285750215, 182.8043069899979969 ) ) ;
#10189 = CARTESIAN_POINT ( 'NONE',  ( 10.41132050455483160, 1522.051704408389924, 228.7775216444308342 ) ) ;
#10190 = CARTESIAN_POINT ( 'NONE',  ( 19.53786426059019021, 1511.187213306747708, 181.5239794925693388 ) ) ;
#10191 = B_SPLINE_CURVE_WITH_KNOTS ( 'NONE', 5,
 ( #48136, #107465, #11764, #47039, #29118, #90108, #5573, #73330, #97958, #89013, #81702, #30202, #13391, #47578, #81163, #4478, #30761, #3390, #31311, #56535, #38608 ),
 .UNSPECIFIED., .F., .F.,
 ( 6, 3, 3, 3, 3, 3, 6 ),
 ( 0.000000000000000000, 0.4999938077254366120, 0.6403281941878481431, 0.8201641551007432529, 0.9100821355580290817, 0.9550411257862527759, 1.000000000000000000 ),
 .UNSPECIFIED. ) ;
#10192 = CARTESIAN_POINT ( 'NONE',  ( -13.11337116420000015, 1442.804475998300177, 187.4630894580980112 ) ) ;
#10193 = CARTESIAN_POINT ( 'NONE',  ( -7.595232024581050290, 1384.066046907910049, 219.0217700005140102 ) ) ;
#10194 = CARTESIAN_POINT ( 'NONE',  ( 18.13448186070239743, 1429.411014922339973, 207.6636477268740180 ) ) ;
#10195 = FACE_OUTER_BOUND ( 'NONE', #61696, .T. ) ;
#10196 = VERTEX_POINT ( 'NONE', #39870 ) ;
#10197 = CARTESIAN_POINT ( 'NONE',  ( -2.966690011115000303, 1511.639769324940062, 201.4286129170669710 ) ) ;
#10198 = CARTESIAN_POINT ( 'NONE',  ( -14.09333513740220134, 1409.405210495020128, 204.1816249279730187 ) ) ;
#10199 = CARTESIAN_POINT ( 'NONE',  ( -13.36486944082299999, 1507.695946242639820, 209.3487293561690024 ) ) ;
#10200 = CARTESIAN_POINT ( 'NONE',  ( -33.05470698740527524, 1442.773887286368563, 154.3540262795430067 ) ) ;
#10201 = CIRCLE ( 'NONE', #31695, 2.000000000000003109 ) ;
#10202 = CARTESIAN_POINT ( 'NONE',  ( -42.11994550690000239, 1455.888674964030088, 268.8741266023980074 ) ) ;
#10203 = CARTESIAN_POINT ( 'NONE',  ( -29.79244516855506220, 1525.556089352344543, 196.8434918795948931 ) ) ;
#10204 = CARTESIAN_POINT ( 'NONE',  ( -16.43158050010680071, 1420.644938884899830, 203.2808245233400157 ) ) ;
#10205 = CARTESIAN_POINT ( 'NONE',  ( -24.06692873656430010, 1444.368885470432588, 212.0869959726532272 ) ) ;
#10206 = CARTESIAN_POINT ( 'NONE',  ( -70.52881574989599756, 1384.661057111879927, 295.6545454185069843 ) ) ;
#10207 = CARTESIAN_POINT ( 'NONE',  ( -16.57194402519859722, 1384.944668023739723, 200.8899537780140179 ) ) ;
#10208 = DIRECTION ( 'NONE',  ( -0.6736849260863841948, 0.000000000000000000, 0.7390186874254148774 ) ) ;
#10209 = CARTESIAN_POINT ( 'NONE',  ( 13.00742463789999981, 1414.913060387329779, 218.5570036086780021 ) ) ;
#10210 = CARTESIAN_POINT ( 'NONE',  ( -28.29378357199729876, 1508.482245365549943, 208.8393840306729885 ) ) ;
#10211 = CARTESIAN_POINT ( 'NONE',  ( -27.24430363784859921, 1507.989586464290142, 211.0156678195309894 ) ) ;
#10212 = DIRECTION ( 'NONE',  ( -0.6736849260863839728, 0.000000000000000000, 0.7390186874254150995 ) ) ;
#10213 = CARTESIAN_POINT ( 'NONE',  ( -7.789308819770000447, 1507.432058219530063, 181.7020214070979875 ) ) ;
#10214 = CARTESIAN_POINT ( 'NONE',  ( -23.00682135910000170, 1409.716476292929883, 208.3124398812599907 ) ) ;
#10215 = CARTESIAN_POINT ( 'NONE',  ( 16.30669509790000049, 1415.087745006229852, 204.0605247263480067 ) ) ;
#10216 = CARTESIAN_POINT ( 'NONE',  ( 3.305606196530000318, 1485.263013345289892, 219.7395598687990059 ) ) ;
#10217 = CARTESIAN_POINT ( 'NONE',  ( 4.461246620899999904, 1423.870484961680177, 193.5243008840990058 ) ) ;
#10218 = CARTESIAN_POINT ( 'NONE',  ( -11.93818408299999945, 1433.480074519959999, 149.8972116839979947 ) ) ;
#10219 = CARTESIAN_POINT ( 'NONE',  ( 10.26657504319999958, 1453.676195443890037, 189.9132845388990063 ) ) ;
#10220 = CARTESIAN_POINT ( 'NONE',  ( -7.167019251197560337, 1508.551563895499839, 214.6350865074379897 ) ) ;
#10221 = CARTESIAN_POINT ( 'NONE',  ( 4.803828466469020064, 1471.771541183390127, 187.6888343885629808 ) ) ;
#10223 = CARTESIAN_POINT ( 'NONE',  ( -10.39382043080000173, 1382.190468632969896, 201.2536150431689919 ) ) ;
#10222 = CARTESIAN_POINT ( 'NONE',  ( -22.38213066169999976, 1410.189388595030096, 211.7294389034280186 ) ) ;
#10224 = CARTESIAN_POINT ( 'NONE',  ( -4.992905603179999652, 1391.642136302990139, 203.5786559967189930 ) ) ;
#10225 = CARTESIAN_POINT ( 'NONE',  ( -19.53786426059057746, 1512.187213306747481, 181.5239794925695946 ) ) ;
#10226 = CARTESIAN_POINT ( 'NONE',  ( -12.07474050270000099, 1489.840319478090123, 211.0992678051489690 ) ) ;
#10227 = CARTESIAN_POINT ( 'NONE',  ( -23.58466550250000182, 1425.864548988530032, 211.0897696391780016 ) ) ;
#10228 = AXIS2_PLACEMENT_3D ( 'NONE', #75333, #50664, #76978 ) ;
#10229 = CARTESIAN_POINT ( 'NONE',  ( -4.533972341721243637, 1368.949167378611946, 210.6218459616991936 ) ) ;
#10230 = CARTESIAN_POINT ( 'NONE',  ( 2.480187016714999970, 1517.025470194390209, 204.4964864072570094 ) ) ;
#10231 = CARTESIAN_POINT ( 'NONE',  ( -30.68434753601961162, 1526.000688113729211, 201.3936004808175255 ) ) ;
#10232 = CARTESIAN_POINT ( 'NONE',  ( -14.59646112059999901, 1484.617543311429927, 186.9027180520979812 ) ) ;
#10233 = CARTESIAN_POINT ( 'NONE',  ( 1.591349661450000008, 1508.276900102130185, 237.0058671888980086 ) ) ;
#10234 = FACE_OUTER_BOUND ( 'NONE', #84043, .T. ) ;
#10235 = CARTESIAN_POINT ( 'NONE',  ( 40.01268977396789950, 1445.988963729020043, 136.7986924672030113 ) ) ;
#10238 = ORIENTED_EDGE ( 'NONE', *, *, #63890, .F. ) ;
#10237 = CARTESIAN_POINT ( 'NONE',  ( -64.35649047367049036, 1379.742209816759896, 273.6236211245889649 ) ) ;
#10236 = CIRCLE ( 'NONE', #99653, 1.000000000000000888 ) ;
#10239 = ORIENTED_EDGE ( 'NONE', *, *, #48250, .F. ) ;
#10240 = CARTESIAN_POINT ( 'NONE',  ( 11.84597236525540076, 1433.773622760579883, 150.7447557071740221 ) ) ;
#10241 = CARTESIAN_POINT ( 'NONE',  ( 20.72500064272757214, 1525.697947650400920, 184.6549703297900464 ) ) ;
#10242 = ORIENTED_EDGE ( 'NONE', *, *, #91847, .T. ) ;
#10243 = CARTESIAN_POINT ( 'NONE',  ( -1.682067311822292632, 1456.930731614571641, 199.7658281152051529 ) ) ;
#10244 = CARTESIAN_POINT ( 'NONE',  ( -109.9849727219999949, 1384.916905217840167, 311.4561123622590344 ) ) ;
#10246 = DIRECTION ( 'NONE',  ( 0.2054769195713296304, -0.000000000000000000, 0.9786619618251631847 ) ) ;
#10245 = CARTESIAN_POINT ( 'NONE',  ( 16.84159957015370068, 1450.438998685270235, 190.2947511461639749 ) ) ;
#10247 = CARTESIAN_POINT ( 'NONE',  ( 7.848979634317430509, 1522.051704408389924, 215.9448598632019980 ) ) ;
#10248 = CARTESIAN_POINT ( 'NONE',  ( 7.252303098479999655, 1488.166944670630073, 183.5694544787980078 ) ) ;
#10249 = CARTESIAN_POINT ( 'NONE',  ( -1.811578048269999908, 1468.887281251189961, 219.1129677655590058 ) ) ;
#10250 = CARTESIAN_POINT ( 'NONE',  ( 4.363122647530000009, 1423.854802298929826, 179.4243885131980107 ) ) ;
#10251 = CARTESIAN_POINT ( 'NONE',  ( 1.135460316954999938, 1516.790374942449944, 212.3751473514870156 ) ) ;
#10252 = CARTESIAN_POINT ( 'NONE',  ( 14.32414760831999878, 1416.073666499230058, 196.9890948053629813 ) ) ;
#10253 = CARTESIAN_POINT ( 'NONE',  ( -4.507044386543670456, 1426.351334971300048, 208.6001660766199848 ) ) ;
#10254 = CARTESIAN_POINT ( 'NONE',  ( 6.910053031764999965, 1514.330398624150121, 201.0829441462669820 ) ) ;
#10255 = VERTEX_POINT ( 'NONE', #31459 ) ;
#10256 = CARTESIAN_POINT ( 'NONE',  ( 14.17148602175130101, 1435.193163544880008, 149.2585390295329830 ) ) ;
#10257 = VERTEX_POINT ( 'NONE', #100852 ) ;
#10258 = VERTEX_POINT ( 'NONE', #65639 ) ;
#10259 = ORIENTED_EDGE ( 'NONE', *, *, #29592, .F. ) ;
#10260 = CARTESIAN_POINT ( 'NONE',  ( -8.207084992775001808, 1512.038636172079805, 215.4514803347070142 ) ) ;
#10261 = CARTESIAN_POINT ( 'NONE',  ( -2.763419390480000182, 1466.129840014930096, 235.1610046648980017 ) ) ;
#10262 = DIRECTION ( 'NONE',  ( 1.755985294532464991E-16, -1.000000000000000000, 1.338183447452830017E-16 ) ) ;
#10263 = AXIS2_PLACEMENT_3D ( 'NONE', #19096, #70671, #79055 ) ;
#10264 = CARTESIAN_POINT ( 'NONE',  ( -4.240938962173256499, 1509.032014554845546, 205.3774795649941893 ) ) ;
#10265 = CARTESIAN_POINT ( 'NONE',  ( 9.878689728610000387, 1462.081439766189987, 209.0598259307259923 ) ) ;
#10266 = CARTESIAN_POINT ( 'NONE',  ( 11.27370387821760112, 1422.118576165349850, 210.3076253712490029 ) ) ;
#10267 = CARTESIAN_POINT ( 'NONE',  ( -22.74071171259225821, 1379.610629053026287, 210.0440409253812675 ) ) ;
#10268 = CARTESIAN_POINT ( 'NONE',  ( 4.259522660623400014, 1446.576511802210007, 159.6066588128159935 ) ) ;
#10269 = CARTESIAN_POINT ( 'NONE',  ( 0.5005539547930000221, 1508.988185698529833, 238.8806144467979777 ) ) ;
#10270 = VERTEX_POINT ( 'NONE', #6802 ) ;
#10271 = CARTESIAN_POINT ( 'NONE',  ( -3.461995196814999787, 1516.906233342200039, 206.2559344154570056 ) ) ;
#10272 = ORIENTED_EDGE ( 'NONE', *, *, #73711, .F. ) ;
#10273 = CARTESIAN_POINT ( 'NONE',  ( 31.61825852761390010, 1440.913060387330006, 255.2595036761919971 ) ) ;
#10274 = CARTESIAN_POINT ( 'NONE',  ( -15.56111295170000020, 1509.395558335530040, 184.1751395816980050 ) ) ;
#10275 = VERTEX_POINT ( 'NONE', #42078 ) ;
#10276 = CARTESIAN_POINT ( 'NONE',  ( 25.24523437353879984, 1450.837001535949867, 137.6108059648960023 ) ) ;
#10277 = CARTESIAN_POINT ( 'NONE',  ( -14.62683816560000061, 1410.356143933229987, 190.5625663710980007 ) ) ;
#10278 = CARTESIAN_POINT ( 'NONE',  ( -24.37050012060000270, 1442.224872846740027, 212.1537385428579796 ) ) ;
#10279 = CARTESIAN_POINT ( 'NONE',  ( 2.950090637770019786, 1423.648712310149904, 192.7546880243370140 ) ) ;
#10280 = CARTESIAN_POINT ( 'NONE',  ( 0.0002634086548581413153, 1396.454024644930314, 196.7541624207434552 ) ) ;
#10281 = CARTESIAN_POINT ( 'NONE',  ( 25.98561784903089844, 1441.261220175989820, 138.2899391456000160 ) ) ;
#10282 = CARTESIAN_POINT ( 'NONE',  ( -13.80523795290000066, 1434.979592755129943, 149.2726119245979817 ) ) ;
#10283 = CARTESIAN_POINT ( 'NONE',  ( 17.95374924460000088, 1435.124687891739995, 145.3138471459980110 ) ) ;
#10285 = DIRECTION ( 'NONE',  ( -3.884000507300682969E-06, 0.9999999999895848868, -2.396820608630749728E-06 ) ) ;
#10284 = CARTESIAN_POINT ( 'NONE',  ( 21.98490254032972047, 1525.713797967456912, 182.9410524212044606 ) ) ;
#10286 = AXIS2_PLACEMENT_3D ( 'NONE', #107278, #80981, #64763 ) ;
#10287 = CARTESIAN_POINT ( 'NONE',  ( -0.7376675409259989546, 1517.104497701820037, 214.9086937099069985 ) ) ;
#10288 = CARTESIAN_POINT ( 'NONE',  ( -3.035907725099100229, 1428.901055825690037, 200.2600137390959958 ) ) ;
#10289 = CARTESIAN_POINT ( 'NONE',  ( 6.067071694012949656, 1511.169205552290123, 216.6808197893799957 ) ) ;
#10291 = EDGE_CURVE ( 'NONE', #28591, #43475, #83402, .T. ) ;
#10290 = CARTESIAN_POINT ( 'NONE',  ( -17.22592475670000312, 1443.913060387330006, 162.9227486557980171 ) ) ;
#10292 = CARTESIAN_POINT ( 'NONE',  ( 7.337793712495000342, 1517.145312756229941, 211.9940546803969994 ) ) ;
#10293 = EDGE_CURVE ( 'NONE', #6840, #110498, #24412, .T. ) ;
#10294 = CARTESIAN_POINT ( 'NONE',  ( -11.76331282408339973, 1482.371198147200175, 207.3261823526030128 ) ) ;
#10295 = CARTESIAN_POINT ( 'NONE',  ( 31.00891611928376790, 1524.547873515805122, 221.8102696095544673 ) ) ;
#10297 = ORIENTED_EDGE ( 'NONE', *, *, #49035, .F. ) ;
#10296 = CARTESIAN_POINT ( 'NONE',  ( -96.24445620069998597, 1386.506167415560185, 310.5622141132590173 ) ) ;
#10298 = CARTESIAN_POINT ( 'NONE',  ( -16.49871405536275404, 1525.320849883625669, 237.0413307544871202 ) ) ;
#10299 = CARTESIAN_POINT ( 'NONE',  ( 14.70061896480000030, 1464.437658295830033, 244.5173669037980346 ) ) ;
#10300 = EDGE_CURVE ( 'NONE', #92224, #33528, #41529, .T. ) ;
#10301 = CARTESIAN_POINT ( 'NONE',  ( 31.12456774391179692, 1525.960063244516959, 217.0912716842395866 ) ) ;
#10302 = CARTESIAN_POINT ( 'NONE',  ( -11.74015320060000001, 1428.979986575930070, 144.1938086916980239 ) ) ;
#10303 = EDGE_CURVE ( 'NONE', #48574, #82445, #54822, .T. ) ;
#10304 = CARTESIAN_POINT ( 'NONE',  ( -5.389426750931309407, 1508.548281180689855, 236.7560892007110169 ) ) ;
#10305 = CARTESIAN_POINT ( 'NONE',  ( -22.44033291929999763, 1451.339077370430005, 219.6664876968980025 ) ) ;
#10306 = CIRCLE ( 'NONE', #49725, 1.000000000000003775 ) ;
#10308 = CARTESIAN_POINT ( 'NONE',  ( 17.70873813924769991, 1409.985199876030038, 222.7474336651429780 ) ) ;
#10307 = LINE ( 'NONE', #44480, #82344 ) ;
#10309 = CARTESIAN_POINT ( 'NONE',  ( 0.1710941751449999992, 1506.802866779329861, 186.9387561868979901 ) ) ;
#10310 = CARTESIAN_POINT ( 'NONE',  ( -107.9019887798300061, 1382.633163608059931, 310.5403456482189881 ) ) ;
#10311 = VERTEX_POINT ( 'NONE', #109289 ) ;
#10312 = CARTESIAN_POINT ( 'NONE',  ( -0.7553264739829980146, 1516.745833913490060, 203.3462208547369983 ) ) ;
#10313 = CARTESIAN_POINT ( 'NONE',  ( -9.821428347282159521, 1508.436132293389846, 218.8451730364450043 ) ) ;
#10314 = CARTESIAN_POINT ( 'NONE',  ( 27.74496033939999862, 1507.996570538830156, 207.7306165369780047 ) ) ;
#10315 = CARTESIAN_POINT ( 'NONE',  ( 13.17363969167560178, 1472.364508107560141, 270.4167824513199889 ) ) ;
#10316 = CARTESIAN_POINT ( 'NONE',  ( 22.52609212299890018, 1509.699688857919909, 227.3081665486540146 ) ) ;
#10317 = EDGE_CURVE ( 'NONE', #94490, #64525, #92348, .T. ) ;
#10318 = CARTESIAN_POINT ( 'NONE',  ( 3.826592460210000102, 1468.046643628590118, 218.3510257011089948 ) ) ;
#10319 = CARTESIAN_POINT ( 'NONE',  ( -0.5374665116262267173, 1469.511926925009675, 219.1609941224751879 ) ) ;
#10320 = FACE_OUTER_BOUND ( 'NONE', #84943, .T. ) ;
#10321 = CARTESIAN_POINT ( 'NONE',  ( 35.72414125057429857, 1450.114973065470167, 136.2375792952020106 ) ) ;
#10322 = CARTESIAN_POINT ( 'NONE',  ( -7.709487050242899819, 1516.551695078709827, 211.8815864275139802 ) ) ;
#10323 = CARTESIAN_POINT ( 'NONE',  ( -1.393502785639999964, 1429.966547008989892, 200.2027313623789837 ) ) ;
#10324 = CARTESIAN_POINT ( 'NONE',  ( -31.81407709660785699, 1512.187213306747481, 196.2902540610632229 ) ) ;
#10325 = CARTESIAN_POINT ( 'NONE',  ( 2.994526374120000334, 1506.310361900689941, 220.7972505012990041 ) ) ;
#10326 = EDGE_CURVE ( 'NONE', #62781, #95904, #82969, .T. ) ;
#10327 = DIRECTION ( 'NONE',  ( 1.836970198721029688E-16, 1.000000000000000000, -2.953460612019999929E-19 ) ) ;
#10328 = ORIENTED_EDGE ( 'NONE', *, *, #55141, .F. ) ;
#10329 = CARTESIAN_POINT ( 'NONE',  ( -20.14739811709999984, 1412.328483943929996, 271.1218459616979999 ) ) ;
#10330 = ADVANCED_FACE ( 'NONE', ( #91916 ), #30119, .F. ) ;
#10331 = CARTESIAN_POINT ( 'NONE',  ( -0.8073792788704451384, 1450.884866113202406, 181.3631603842342486 ) ) ;
#10332 = CARTESIAN_POINT ( 'NONE',  ( 10.32070371839930090, 1469.846300739589879, 207.1845276051559779 ) ) ;
#10333 = CARTESIAN_POINT ( 'NONE',  ( -0.4667605481589999772, 1416.135518339629925, 233.5066626509980097 ) ) ;
#10334 = CARTESIAN_POINT ( 'NONE',  ( 12.26027809410000025, 1500.839094156290230, 209.5442590651630326 ) ) ;
#10335 = CARTESIAN_POINT ( 'NONE',  ( -32.74318896774710907, 1524.667648926107177, 196.1902622063078070 ) ) ;
#10336 = FACE_OUTER_BOUND ( 'NONE', #40350, .T. ) ;
#10337 = CARTESIAN_POINT ( 'NONE',  ( -22.01162841000270021, 1384.855953449889967, 221.8868375699159969 ) ) ;
#10338 = CARTESIAN_POINT ( 'NONE',  ( -18.63578313170000200, 1416.568813547830132, 208.5538819738139864 ) ) ;
#10339 = CARTESIAN_POINT ( 'NONE',  ( 11.87158682754100170, 1432.747848164100105, 149.9813451862029865 ) ) ;
#10340 = CARTESIAN_POINT ( 'NONE',  ( 26.16070222434640158, 1436.533894928910058, 136.8495626736880126 ) ) ;
#10341 = CARTESIAN_POINT ( 'NONE',  ( -8.061180465434720332, 1396.194563012580147, 201.5581022159940119 ) ) ;
#10343 = VERTEX_POINT ( 'NONE', #640 ) ;
#10342 = B_SPLINE_CURVE_WITH_KNOTS ( 'NONE', 5,
 ( #57880, #75231, #42721, #33200, #66836, #68489 ),
 .UNSPECIFIED., .F., .F.,
 ( 6, 6 ),
 ( 0.000000000000000000, 1.000000000000000000 ),
 .UNSPECIFIED. ) ;
#10344 = B_SPLINE_CURVE_WITH_KNOTS ( 'NONE', 3,
 ( #102451, #59939, #94056, #17324, #61592, #27969, #105235, #70008, #27410, #11722, #95725, #19557, #103565, #20111, #87330, #60487, #62153, #62723, #43672, #70557, #96844, #77825, #104675, #78377, #1133, #1684, #104122, #95177, #54304, #26867, #35825, #45350, #18990, #35263, #71111, #69448, #96280, #53763, #88432, #61055, #87897, #3351, #18433, #11188, #53188, #52633 ),
 .UNSPECIFIED., .F., .F.,
 ( 4, 3, 3, 3, 3, 3, 3, 3, 3, 3, 3, 3, 3, 3, 3, 4 ),
 ( 8.670147881838009580E-05, 0.4789285211775260453, 0.9744792269830828690, 1.259346753059999990, 1.776261645606839856, 2.325059878702980143, 2.711818916799999979, 3.323520562006709866, 4.028423604586089724, 4.918128909075430322, 5.564709931820000399, 7.179393063629159855, 8.369582197274629820, 9.352558316332389765, 10.31444422860000110, 10.41999860509999998 ),
 .UNSPECIFIED. ) ;
#10345 = CARTESIAN_POINT ( 'NONE',  ( -17.19883865694049874, 1410.595981660250118, 225.9965367844259845 ) ) ;
#10346 = CARTESIAN_POINT ( 'NONE',  ( 2.493947715939999643, 1442.756953654919926, 150.6345094620980092 ) ) ;
#10347 = EDGE_LOOP ( 'NONE', ( #30085, #63176, #104924, #82385 ) ) ;
#10348 = CARTESIAN_POINT ( 'NONE',  ( -6.753153240240000521, 1472.181002690289915, 210.7318518582290210 ) ) ;
#10349 = PLANE ( 'NONE',  #47502 ) ;
#10350 = DIRECTION ( 'NONE',  ( 0.4794255386042096112, 0.000000000000000000, -0.8775825618903690950 ) ) ;
#10352 = DIRECTION ( 'NONE',  ( 0.03234404824097146525, -0.9989938922171894831, -0.03106550910795196491 ) ) ;
#10351 = PLANE ( 'NONE',  #35331 ) ;
#10353 = CARTESIAN_POINT ( 'NONE',  ( 1.448679645196929933, 1507.129709964000085, 181.1126013477120011 ) ) ;
#10354 = B_SPLINE_CURVE_WITH_KNOTS ( 'NONE', 5,
 ( #56953, #14364, #82694, #40132, #108445, #100030 ),
 .UNSPECIFIED., .F., .F.,
 ( 6, 6 ),
 ( -105.4335682549999973, -86.05908199089999755 ),
 .UNSPECIFIED. ) ;
#10355 = CARTESIAN_POINT ( 'NONE',  ( -8.635302540649998804, 1451.543452603389824, 205.3798752934189906 ) ) ;
#10356 = CIRCLE ( 'NONE', #40808, 1.999999999999998224 ) ;
#10357 = CARTESIAN_POINT ( 'NONE',  ( -109.9782865922809947, 1384.547503231000064, 311.4425668244260237 ) ) ;
#10358 = CARTESIAN_POINT ( 'NONE',  ( 7.574305215059999874, 1424.934277763670025, 212.0912061558890116 ) ) ;
#10359 = CARTESIAN_POINT ( 'NONE',  ( 20.10528729609999843, 1430.878053336090034, 215.1856554784289983 ) ) ;
#10360 = CARTESIAN_POINT ( 'NONE',  ( -5.399591253687431092, 1511.369014876797792, 201.1386261298281397 ) ) ;
#10361 = CARTESIAN_POINT ( 'NONE',  ( 2.500000876580000142, 1448.997560968779908, 182.3441048618979892 ) ) ;
#10362 = CARTESIAN_POINT ( 'NONE',  ( 9.984115569242678845, 1365.258395869462220, 210.6218459616987957 ) ) ;
#10364 = ORIENTED_EDGE ( 'NONE', *, *, #29516, .T. ) ;
#10363 = CARTESIAN_POINT ( 'NONE',  ( -8.808667343012501760, 1463.337573556750840, 235.3868218242529906 ) ) ;
#10365 = VERTEX_POINT ( 'NONE', #87390 ) ;
#10366 = CARTESIAN_POINT ( 'NONE',  ( -40.70526361830000184, 1444.199272583730135, 137.0833898022980009 ) ) ;
#10367 = CARTESIAN_POINT ( 'NONE',  ( 1.442233445782429957, 1490.976481901869874, 236.0750500844659996 ) ) ;
#10368 = CARTESIAN_POINT ( 'NONE',  ( -1.454166803559999943, 1473.250322698830132, 270.4288814092980147 ) ) ;
#10369 = CARTESIAN_POINT ( 'NONE',  ( -7.656028705865000283, 1510.967342883699985, 213.6171158279370275 ) ) ;
#10370 = CARTESIAN_POINT ( 'NONE',  ( -0.5747759660569999873, 1486.512367523630019, 181.7356503477979857 ) ) ;
#10371 = CARTESIAN_POINT ( 'NONE',  ( -32.05523756949325787, 1525.253972588462375, 201.2193331634007905 ) ) ;
#10372 = CARTESIAN_POINT ( 'NONE',  ( -3.152270375085599596, 1474.954422185709745, 198.1306180807430053 ) ) ;
#10373 = CARTESIAN_POINT ( 'NONE',  ( 22.53878436229999949, 1411.058442725530085, 206.1986151520480064 ) ) ;
#10374 = SHAPE_REPRESENTATION_RELATIONSHIP ( 'NONE' , 'NONE' ,  #60858, #51910 ) ;
#10375 = CARTESIAN_POINT ( 'NONE',  ( -2.500000000000000000, 1448.758219214420023, 157.1656513902149754 ) ) ;
#10376 = CARTESIAN_POINT ( 'NONE',  ( -13.04464049575494045, 1434.926819199586134, 149.8863372439509760 ) ) ;
#10377 = CARTESIAN_POINT ( 'NONE',  ( 15.38805437926849784, 1409.450423087220088, 203.9135902043169892 ) ) ;
#10378 = CARTESIAN_POINT ( 'NONE',  ( 5.717839861821480532E-05, 1405.749489006759859, 267.5370922816329653 ) ) ;
#10379 = CARTESIAN_POINT ( 'NONE',  ( -13.85777447298269927, 1434.981442650969939, 148.6210011382069922 ) ) ;
#10380 = ORIENTED_EDGE ( 'NONE', *, *, #84388, .F. ) ;
#10381 = CARTESIAN_POINT ( 'NONE',  ( 3.585180483099999815, 1424.862442824429991, 185.0085506464979801 ) ) ;
#10382 = CARTESIAN_POINT ( 'NONE',  ( 13.42038842620000061, 1444.421388250450264, 187.7727034152979968 ) ) ;
#10383 = ORIENTED_EDGE ( 'NONE', *, *, #26874, .F. ) ;
#10384 = AXIS2_PLACEMENT_3D ( 'NONE', #14433, #32892, #16081 ) ;
#10385 = ORIENTED_EDGE ( 'NONE', *, *, #71431, .T. ) ;
#10386 = EDGE_CURVE ( 'NONE', #44146, #86029, #84680, .T. ) ;
#10387 = CARTESIAN_POINT ( 'NONE',  ( -3.757047865440000134, 1455.840493388089953, 200.4411851703590060 ) ) ;
#10388 = CARTESIAN_POINT ( 'NONE',  ( -9.830395177430000686, 1365.769828494180047, 207.6218459616989946 ) ) ;
#10389 = AXIS2_PLACEMENT_3D ( 'NONE', #106748, #40100, #64790 ) ;
#10390 = EDGE_CURVE ( 'NONE', #24504, #34701, #106666, .T. ) ;
#10391 = CARTESIAN_POINT ( 'NONE',  ( -4.611879723454999969, 1516.858533673840157, 213.7437437946470027 ) ) ;
#10392 = CARTESIAN_POINT ( 'NONE',  ( 2.541812758945000361, 1512.177707669779920, 216.7470359957769972 ) ) ;
#10393 = B_SPLINE_SURFACE_WITH_KNOTS ( 'NONE', 3, 5, ( 
 ( #72844, #14008, #22952, #107529, #21292, #15104 ),
 ( #64457, #99661, #99113, #39217, #73393, #48753 ),
 ( #81765, #57710, #108074, #4535, #38669, #6169 ),
 ( #98572, #91282, #56590, #14563, #100237, #63905 ) ),
 .UNSPECIFIED., .F., .F., .F.,
 ( 4, 4 ),
 ( 6, 6 ),
 ( 5.479556543930000245, 5.505627295709999203 ),
 ( 0.000000000000000000, 1.000000000000000000 ),
 .UNSPECIFIED. ) ;
#10394 = CIRCLE ( 'NONE', #103406, 29.51505616007316135 ) ;
#10395 = ORIENTED_EDGE ( 'NONE', *, *, #108900, .F. ) ;
#10396 = CARTESIAN_POINT ( 'NONE',  ( -77.77200720220001529, 1379.656469662929794, 291.9281914769590003 ) ) ;
#10397 = CIRCLE ( 'NONE', #40764, 1.000000000000000888 ) ;
#10398 = CARTESIAN_POINT ( 'NONE',  ( -105.8561346205080014, 1378.913060387450059, 303.4563273789140112 ) ) ;
#10399 = CARTESIAN_POINT ( 'NONE',  ( -0.7553264739829980146, 1516.745833913490060, 203.3462208547369983 ) ) ;
#10400 = ADVANCED_FACE ( 'NONE', ( #97431 ), #109774, .T. ) ;
#10401 = CARTESIAN_POINT ( 'NONE',  ( -28.07231162100000077, 1508.101920006030241, 207.7749232119980149 ) ) ;
#10402 = FACE_OUTER_BOUND ( 'NONE', #40963, .T. ) ;
#10403 = CARTESIAN_POINT ( 'NONE',  ( -98.86683315710000386, 1385.218296336320009, 296.2584199137589849 ) ) ;
#10405 = B_SPLINE_SURFACE_WITH_KNOTS ( 'NONE', 5, 5, ( 
 ( #93733, #17012, #16470, #104236, #10738, #109471, #67482, #8638, #44911 ),
 ( #44345, #101586, #79058, #36476, #7550, #24872, #70673, #78488, #1802 ),
 ( #61709, #57971, #92106, #41704, #32749, #4537, #71218, #81767, #88546 ),
 ( #64459, #105342, #46554, #29181, #47095, #89080, #12915, #47639, #19667 ),
 ( #81222, #72846, #80133, #98022, #12368, #72307, #80689, #96949, #63907 ),
 ( #3452, #29722, #46001, #13449, #56040, #20215, #37580, #21843, #4000 ),
 ( #54414, #38671, #55501, #30268, #28631, #98575, #106980, #62836, #5070 ),
 ( #53872, #90167, #11831, #38126, #63372, #39219, #106438, #104788, #28074 ),
 ( #105902, #62262, #96391, #71783, #21294, #89627, #88011, #11293, #97487 ) ),
 .UNSPECIFIED., .F., .F., .F.,
 ( 6, 3, 6 ),
 ( 6, 3, 6 ),
 ( 9.902195898209999569, 12.38020728900000123, 16.40090783169999966 ),
 ( 0.000000000000000000, 0.5000000000000000000, 1.000000000000000000 ),
 .UNSPECIFIED. ) ;
#10404 = CARTESIAN_POINT ( 'NONE',  ( -59.39287138243709308, 1384.669285364579991, 242.7124994448570021 ) ) ;
#10406 = CARTESIAN_POINT ( 'NONE',  ( 1.126138108584999964, 1517.208444099459939, 201.3951612445669923 ) ) ;
#10407 = CARTESIAN_POINT ( 'NONE',  ( -6.316132940400000173, 1409.300553759430159, 230.7650132070980078 ) ) ;
#10409 = ORIENTED_EDGE ( 'NONE', *, *, #44865, .T. ) ;
#10408 = CARTESIAN_POINT ( 'NONE',  ( -7.322107218450000232, 1446.343164073429989, 185.2693503152979986 ) ) ;
#10410 = CARTESIAN_POINT ( 'NONE',  ( -27.68994704303559828, 1508.175463917300021, 210.5782600342069770 ) ) ;
#10411 = CARTESIAN_POINT ( 'NONE',  ( 0.000000000000000000, 1508.913060387330006, 224.7618459619980058 ) ) ;
#10412 = CARTESIAN_POINT ( 'NONE',  ( -26.04564454490000003, 1383.846902489159902, 224.1106665064590118 ) ) ;
#10413 = CARTESIAN_POINT ( 'NONE',  ( -14.47516141776405618, 1416.049748536053812, 214.4146204850279673 ) ) ;
#10414 = CARTESIAN_POINT ( 'NONE',  ( -24.94579848589999926, 1435.368615134259926, 135.7553688025980136 ) ) ;
#10415 = EDGE_CURVE ( 'NONE', #79870, #95724, #4284, .T. ) ;
#10416 = CARTESIAN_POINT ( 'NONE',  ( -3.252530653725000054, 1516.827328999679821, 212.0018028951869837 ) ) ;
#10417 = CARTESIAN_POINT ( 'NONE',  ( -66.38361129989999654, 1379.743368401719863, 275.3027083311590104 ) ) ;
#10418 = CARTESIAN_POINT ( 'NONE',  ( 0.006240583433823138071, 1508.657668050519987, 238.1872277698262224 ) ) ;
#10419 = CARTESIAN_POINT ( 'NONE',  ( -29.70307219812743682, 1525.408337840049626, 221.9454045032637737 ) ) ;
#10421 = EDGE_CURVE ( 'NONE', #67895, #11716, #87271, .T. ) ;
#10420 = CARTESIAN_POINT ( 'NONE',  ( -11.60004869885203682, 1424.140773631476577, 136.0101406523738490 ) ) ;
#10422 = CARTESIAN_POINT ( 'NONE',  ( 3.261652286895000419, 1516.939580991450157, 209.1085619926769823 ) ) ;
#10423 = ORIENTED_EDGE ( 'NONE', *, *, #56955, .T. ) ;
#10424 = CARTESIAN_POINT ( 'NONE',  ( 2.500000000000000000, 1439.114301455650093, 157.7261946041980138 ) ) ;
#10425 = CARTESIAN_POINT ( 'NONE',  ( -6.492126169470000541, 1412.832739453629983, 231.4048330429980069 ) ) ;
#10426 = CARTESIAN_POINT ( 'NONE',  ( -62.06510066419999561, 1384.932470540059967, 284.7693340512589657 ) ) ;
#10427 = EDGE_CURVE ( 'NONE', #77064, #46523, #89022, .T. ) ;
#10428 = VERTEX_POINT ( 'NONE', #62775 ) ;
#10429 = CARTESIAN_POINT ( 'NONE',  ( -19.06873360288100017, 1385.279875393399834, 220.5578134822330014 ) ) ;
#10430 = CARTESIAN_POINT ( 'NONE',  ( -3.246589359020000121, 1430.595539088089936, 201.4224038467990283 ) ) ;
#10431 = CARTESIAN_POINT ( 'NONE',  ( 11.76920103414339991, 1434.891807205950045, 151.2471915141129841 ) ) ;
#10432 = CARTESIAN_POINT ( 'NONE',  ( 8.124014794800109129, 1488.402311747539898, 234.1398025081960270 ) ) ;
#10433 = DIRECTION ( 'NONE',  ( -0.8090169943749481174, 0.000000000000000000, 0.5877852522924721379 ) ) ;
#10434 = CARTESIAN_POINT ( 'NONE',  ( 3.436085222180000454, 1486.341472188189982, 198.7604664416990090 ) ) ;
#10435 = CARTESIAN_POINT ( 'NONE',  ( 11.09565341729999943, 1425.086740399749942, 203.0248198978989933 ) ) ;
#10436 = CARTESIAN_POINT ( 'NONE',  ( -0.07532719850957350638, 1420.449570258260110, 182.6937329275319826 ) ) ;
#10437 = ADVANCED_FACE ( 'NONE', ( #5017 ), #13194, .T. ) ;
#10439 = CARTESIAN_POINT ( 'NONE',  ( -3.185236608319999885, 1421.319945421930015, 185.4942751512979839 ) ) ;
#10438 = CARTESIAN_POINT ( 'NONE',  ( -0.7386049428049979992, 1517.122674412569950, 215.6839400395269877 ) ) ;
#10440 = CARTESIAN_POINT ( 'NONE',  ( 18.63864990469999938, 1509.044553701730138, 187.9652674623980033 ) ) ;
#10441 = CARTESIAN_POINT ( 'NONE',  ( 0.02955819112566610354, 1517.051704408389924, 193.2356110507530218 ) ) ;
#10442 = ORIENTED_EDGE ( 'NONE', *, *, #110315, .T. ) ;
#10443 = CARTESIAN_POINT ( 'NONE',  ( 6.942354273414999888, 1516.905946377369901, 201.4030824261969883 ) ) ;
#10444 = CARTESIAN_POINT ( 'NONE',  ( -19.88572122277579979, 1484.728771715989751, 191.0592865161910083 ) ) ;
#10445 = ORIENTED_EDGE ( 'NONE', *, *, #95112, .T. ) ;
#10446 = CARTESIAN_POINT ( 'NONE',  ( 4.015231150059999088, 1421.847071512329876, 183.7162519361979776 ) ) ;
#10447 = ADVANCED_FACE ( 'NONE', ( #81711 ), #49884, .F. ) ;
#10448 = FILL_AREA_STYLE_COLOUR ( '', #31521 ) ;
#10449 = CARTESIAN_POINT ( 'NONE',  ( 7.580297983975060383, 1511.034527886640262, 203.1778469106609748 ) ) ;
#10450 = CARTESIAN_POINT ( 'NONE',  ( 3.087555757030000070, 1443.150514725890162, 217.4716940151990059 ) ) ;
#10451 = CARTESIAN_POINT ( 'NONE',  ( -33.17484411121699139, 1525.713797967457140, 200.8635405475165499 ) ) ;
#10452 = CARTESIAN_POINT ( 'NONE',  ( -18.05542497264810109, 1416.825784014559986, 209.4840452940109969 ) ) ;
#10453 = CARTESIAN_POINT ( 'NONE',  ( -4.293785995879999540, 1447.009251615389985, 154.3906955766980218 ) ) ;
#10454 = CARTESIAN_POINT ( 'NONE',  ( -18.55308284270000030, 1424.846930163729894, 224.9900042346980058 ) ) ;
#10455 = CARTESIAN_POINT ( 'NONE',  ( -14.59275605859999914, 1436.244805951940180, 149.8708530261979774 ) ) ;
#10456 = CARTESIAN_POINT ( 'NONE',  ( -0.5919877880829009786, 1487.510302489449941, 230.8834977925120029 ) ) ;
#10457 = CARTESIAN_POINT ( 'NONE',  ( 0.02955819112566610354, 1517.051704408389924, 193.2356110507530218 ) ) ;
#10459 = CARTESIAN_POINT ( 'NONE',  ( -19.08015071520780737, 1440.747599611412397, 209.7861252745999252 ) ) ;
#10458 = CARTESIAN_POINT ( 'NONE',  ( 0.5679639878839999323, 1416.568813547830132, 190.4860628299979908 ) ) ;
#10460 = CARTESIAN_POINT ( 'NONE',  ( 0.5623041700042573643, 1416.835806650143240, 190.4756569920872664 ) ) ;
#10461 = ORIENTED_EDGE ( 'NONE', *, *, #65289, .T. ) ;
#10462 = CARTESIAN_POINT ( 'NONE',  ( 1.135155432552129806, 1507.593744646030018, 186.1936170170519915 ) ) ;
#10463 = CARTESIAN_POINT ( 'NONE',  ( -4.487359741654690204, 1509.034536824670113, 212.2379826147090114 ) ) ;
#10464 = EDGE_CURVE ( 'NONE', #44860, #89357, #58741, .T. ) ;
#10465 = CARTESIAN_POINT ( 'NONE',  ( -23.74108624850000027, 1436.296627321610003, 212.5883426267580205 ) ) ;
#10466 = CARTESIAN_POINT ( 'NONE',  ( 17.17241001986483795, 1512.187213306747481, 179.6185504016043240 ) ) ;
#10467 = AXIS2_PLACEMENT_3D ( 'NONE', #91065, #31158, #65896 ) ;
#10468 = CARTESIAN_POINT ( 'NONE',  ( -3.547964652322029178, 1426.008885103042758, 185.9028156952102506 ) ) ;
#10469 = ADVANCED_FACE ( 'NONE', ( #40273 ), #66061, .T. ) ;
#10470 = CARTESIAN_POINT ( 'NONE',  ( -13.70772824027479864, 1507.648153509909889, 184.2587339175119894 ) ) ;
#10471 = CARTESIAN_POINT ( 'NONE',  ( -11.24296408042640039, 1470.377897305100078, 210.9233862662850072 ) ) ;
#10472 = AXIS2_PLACEMENT_3D ( 'NONE', #61075, #77839, #109787 ) ;
#10473 = ADVANCED_FACE ( 'NONE', ( #91231 ), #39067, .F. ) ;
#10474 = CARTESIAN_POINT ( 'NONE',  ( -10.90534521260189926, 1489.991766825829927, 212.3803483885259880 ) ) ;
#10475 = CARTESIAN_POINT ( 'NONE',  ( -4.326992699989999913, 1515.158586642790169, 209.1218459619010162 ) ) ;
#10476 = CARTESIAN_POINT ( 'NONE',  ( -81.44223561470580819, 1383.775960391189983, 304.5617243241840129 ) ) ;
#10477 = CIRCLE ( 'NONE', #26538, 1.999999999999998668 ) ;
#10478 = DIRECTION ( 'NONE',  ( 0.000000000000000000, 0.000000000000000000, 1.000000000000000000 ) ) ;
#10480 = DIRECTION ( 'NONE',  ( 0.000000000000000000, 0.000000000000000000, 1.000000000000000000 ) ) ;
#10479 =( BOUNDED_SURFACE ( )  B_SPLINE_SURFACE ( 3, 2, ( 
 ( #21079, #12701, #73167 ),
 ( #30605, #46885, #106752 ),
 ( #30041, #64233, #22172 ),
 ( #56370, #102207, #93258 ),
 ( #68094, #16522, #94347 ),
 ( #33899, #100554, #68639 ),
 ( #17065, #50713, #49626 ),
 ( #9267, #51830, #23834 ),
 ( #43427, #75384, #83760 ),
 ( #84843, #77030, #84309 ) ),
 .UNSPECIFIED., .F., .F., .F. ) 
 B_SPLINE_SURFACE_WITH_KNOTS ( ( 4, 2, 2, 2, 4 ),
 ( 3, 3 ),
 ( 0.000000000000000000, 0.3926990816987241395, 0.7853981633974482790, 1.178097245096172418, 1.570796326794896558 ),
 ( 0.000000000000000000, 1.000000000000000000 ),
 .UNSPECIFIED. ) 
 GEOMETRIC_REPRESENTATION_ITEM ( )  RATIONAL_B_SPLINE_SURFACE ( (
 ( 1.000000000000000000, 0.7763623250684347221, 1.000000000000000000),
 ( 1.000000000000000000, 0.7763684247035179675, 1.000000000000000000),
 ( 1.000000000000000000, 0.7746454561797311289, 1.000000000000000000),
 ( 1.000000000000000000, 0.7679730451973156846, 1.000000000000000000),
 ( 1.000000000000000000, 0.7630177051950743916, 1.000000000000000000),
 ( 1.000000000000000000, 0.7504512394524318619, 1.000000000000000000),
 ( 1.000000000000000000, 0.7428408967929591711, 1.000000000000000000),
 ( 1.000000000000000000, 0.7259222650907819485, 1.000000000000000000),
 ( 1.000000000000000000, 0.7166207884821568230, 1.000000000000000000),
 ( 1.000000000000000000, 0.7071067811865867636, 1.000000000000000000) ) ) 
 REPRESENTATION_ITEM ( '' )  SURFACE ( )  );
#10481 = CARTESIAN_POINT ( 'NONE',  ( -2.204892687444989896, 1516.527839230000154, 201.4129835103060202 ) ) ;
#10483 = VERTEX_POINT ( 'NONE', #11112 ) ;
#10482 = DIRECTION ( 'NONE',  ( 0.03489949670250328678, 0.9993908270190956511, 0.000000000000000000 ) ) ;
#10484 = CARTESIAN_POINT ( 'NONE',  ( 17.15874754026939897, 1507.620489270460212, 193.8380741321440155 ) ) ;
#10485 = CARTESIAN_POINT ( 'NONE',  ( -63.74074695120000911, 1380.989849089459995, 283.7619814212590086 ) ) ;
#10486 = CARTESIAN_POINT ( 'NONE',  ( 20.21913194945920011, 1509.384053626160039, 230.0320258892189997 ) ) ;
#10487 = EDGE_LOOP ( 'NONE', ( #50130, #15215, #12191, #47685 ) ) ;
#10488 = EDGE_LOOP ( 'NONE', ( #19052, #32248, #15479, #68975 ) ) ;
#10489 = CARTESIAN_POINT ( 'NONE',  ( 17.41906133238040155, 1508.769966748330035, 231.1703520980719873 ) ) ;
#10490 = CARTESIAN_POINT ( 'NONE',  ( -31.81407709660785699, 1522.382868172863937, 196.2902540610632229 ) ) ;
#10491 = CARTESIAN_POINT ( 'NONE',  ( 13.01686712407386359, 1442.959643518457597, 169.4188180632390015 ) ) ;
#10493 = CARTESIAN_POINT ( 'NONE',  ( -6.526375087349999937, 1473.529235870629918, 262.4989463880980338 ) ) ;
#10492 = CARTESIAN_POINT ( 'NONE',  ( 20.42904319129999635, 1470.816572149729836, 208.8910212311110115 ) ) ;
#10494 = CARTESIAN_POINT ( 'NONE',  ( 8.644428848947828925, 1437.072346058449739, 209.1799678029250060 ) ) ;
#10495 = CARTESIAN_POINT ( 'NONE',  ( -109.7136633519999975, 1383.888121385389923, 297.1243086093589909 ) ) ;
#10496 = CARTESIAN_POINT ( 'NONE',  ( -0.1934954855810029906, 1481.263391716890055, 229.6341570919989863 ) ) ;
#10497 = DIRECTION ( 'NONE',  ( 0.7071067811860475283, 8.350994033320553495E-15, 0.7071067811870476172 ) ) ;
#10498 = AXIS2_PLACEMENT_3D ( 'NONE', #77449, #95897, #62330 ) ;
#10499 = CARTESIAN_POINT ( 'NONE',  ( -2.363918620589999797, 1443.448698872290151, 218.8950620034389942 ) ) ;
#10500 = CARTESIAN_POINT ( 'NONE',  ( 4.738395335269999897, 1421.880050881929947, 185.2211201735979955 ) ) ;
#10501 = CARTESIAN_POINT ( 'NONE',  ( -11.88948492470000140, 1437.278290821260043, 151.6406834257980165 ) ) ;
#10502 = CARTESIAN_POINT ( 'NONE',  ( 11.88948418939999918, 1437.278291760409957, 151.6406840026980092 ) ) ;
#10503 = CARTESIAN_POINT ( 'NONE',  ( -11.17515840243070002, 1423.345794038340046, 204.2560692912300055 ) ) ;
#10504 = CARTESIAN_POINT ( 'NONE',  ( 1.399926847669999974, 1507.072115598929940, 236.8180522793980174 ) ) ;
#10505 = CARTESIAN_POINT ( 'NONE',  ( -16.18755144487676745, 1409.478342139989536, 193.2473228669673233 ) ) ;
#10506 = ORIENTED_EDGE ( 'NONE', *, *, #47269, .T. ) ;
#10507 = CARTESIAN_POINT ( 'NONE',  ( 5.940539707516006906, 1519.551704408389924, 189.0391861794638828 ) ) ;
#10508 = CARTESIAN_POINT ( 'NONE',  ( 18.40700370933230090, 1472.577248366799722, 195.0927350935599804 ) ) ;
#10509 = CARTESIAN_POINT ( 'NONE',  ( -37.60287116660000351, 1456.179137436829706, 270.1614696094979990 ) ) ;
#10510 = CARTESIAN_POINT ( 'NONE',  ( -23.70839420758922245, 1436.152046287332951, 211.9671219878686657 ) ) ;
#10511 = CARTESIAN_POINT ( 'NONE',  ( 12.00000000000000000, 1443.913060387330006, 150.5878346084980137 ) ) ;
#10512 = CARTESIAN_POINT ( 'NONE',  ( -14.17566286230000117, 1463.287831902929838, 223.4212262942980090 ) ) ;
#10513 = CARTESIAN_POINT ( 'NONE',  ( 4.329448776040000446, 1515.064792882589927, 210.9648081929590262 ) ) ;
#10514 = CARTESIAN_POINT ( 'NONE',  ( 2.924457912680139771, 1409.899976016270102, 231.5199593976699930 ) ) ;
#10515 = CARTESIAN_POINT ( 'NONE',  ( -6.942344730043687129, 1516.810037862407626, 201.4055939276168488 ) ) ;
#10516 = CARTESIAN_POINT ( 'NONE',  ( -6.236116630490000645, 1418.000551928829964, 232.4301535818979971 ) ) ;
#10517 = CARTESIAN_POINT ( 'NONE',  ( -7.649433525730000127, 1459.248781285089990, 215.2925678204190092 ) ) ;
#10518 = CARTESIAN_POINT ( 'NONE',  ( -2.488105171088486500, 1359.506461065921940, 207.6218459616987673 ) ) ;
#10519 = CARTESIAN_POINT ( 'NONE',  ( -45.07081559816839444, 1434.497539603230052, 268.7802826201569815 ) ) ;
#10520 = CARTESIAN_POINT ( 'NONE',  ( -11.87328871660000118, 1482.014094933990009, 208.6022274357210051 ) ) ;
#10521 = ORIENTED_EDGE ( 'NONE', *, *, #30249, .T. ) ;
#10522 = CARTESIAN_POINT ( 'NONE',  ( -8.467016979619998551, 1423.717407386009882, 209.4627668193359966 ) ) ;
#10523 = ORIENTED_EDGE ( 'NONE', *, *, #70667, .F. ) ;
#10524 = CARTESIAN_POINT ( 'NONE',  ( 7.724874613184999461, 1517.139320148880188, 209.8621665372610039 ) ) ;
#10525 = EDGE_CURVE ( 'NONE', #40567, #36571, #27896, .T. ) ;
#10526 = CARTESIAN_POINT ( 'NONE',  ( -11.16643434163729864, 1471.372555858320084, 206.7508257846899937 ) ) ;
#10527 = CARTESIAN_POINT ( 'NONE',  ( -21.33082462610000007, 1509.431344384229988, 190.3781974747980144 ) ) ;
#10528 = CARTESIAN_POINT ( 'NONE',  ( -13.06548816099999932, 1410.400106175530027, 189.7504201498980194 ) ) ;
#10529 = CARTESIAN_POINT ( 'NONE',  ( -18.64588652299999794, 1416.828040475229955, 208.5593769277110141 ) ) ;
#10530 = B_SPLINE_SURFACE_WITH_KNOTS ( 'NONE', 5, 5, ( 
 ( #69326, #93386, #50850, #103434, #83889, #32929 ),
 ( #16653, #24517, #84979, #58707, #92839, #8273 ),
 ( #42438, #110748, #34039, #68230, #63154, #37361 ),
 ( #28964, #9942, #44114, #86646, #54187, #78813 ),
 ( #79920, #87779, #88864, #62035, #106214, #78249 ),
 ( #96721, #27854, #3233, #2682, #1563, #36807 ),
 ( #3785, #52516, #71561, #72098, #27297, #35695 ),
 ( #70998, #97253, #36252, #87208, #20529, #69884 ),
 ( #62606, #12148, #80469, #19995, #44672, #104000 ),
 ( #18325, #53071, #10500, #105680, #61478, #2128 ),
 ( #54735, #70440, #46340, #37917, #29495, #63689 ),
 ( #105116, #104559, #96158, #11059, #19435, #95605 ) ),
 .UNSPECIFIED., .F., .F., .F.,
 ( 6, 3, 3, 6 ),
 ( 6, 6 ),
 ( 5.632673649860000076, 8.026914679749999948, 9.819017978390000678, 13.16393005930000015 ),
 ( 0.000000000000000000, 2.000000000000000000 ),
 .UNSPECIFIED. ) ;
#10531 = ORIENTED_EDGE ( 'NONE', *, *, #68384, .F. ) ;
#10532 = DIRECTION ( 'NONE',  ( -1.755985294532469921E-16, 1.000000000000000000, -1.338183447452831989E-16 ) ) ;
#10534 = CARTESIAN_POINT ( 'NONE',  ( 10.13545575494789830, 1453.511789163979984, 212.2748783515349942 ) ) ;
#10533 = DIRECTION ( 'NONE',  ( 5.551115123126445838E-17, -0.7071067811865475727, -0.7071067811865475727 ) ) ;
#10535 = CARTESIAN_POINT ( 'NONE',  ( 1.925781382208645587, 1487.138807670421329, 219.7730072395593766 ) ) ;
#10536 = CARTESIAN_POINT ( 'NONE',  ( -19.02872918048390005, 1508.494693425979904, 209.9678762690199960 ) ) ;
#10537 = ADVANCED_FACE ( 'NONE', ( #20570 ), #32875, .T. ) ;
#10538 = CARTESIAN_POINT ( 'NONE',  ( 7.261898129199999552, 1472.764678900990020, 216.9089656813590068 ) ) ;
#10539 = CARTESIAN_POINT ( 'NONE',  ( 17.68711869539999881, 1428.828027849089949, 204.9896315466789929 ) ) ;
#10540 = EDGE_LOOP ( 'NONE', ( #38923, #76186, #77766, #108705 ) ) ;
#10541 = CARTESIAN_POINT ( 'NONE',  ( -28.16679250621550068, 1415.942106301169815, 270.3408856473929518 ) ) ;
#10542 = CARTESIAN_POINT ( 'NONE',  ( 2.477975315464999717, 1516.839862955080207, 207.9852983471170091 ) ) ;
#10543 = CARTESIAN_POINT ( 'NONE',  ( 10.83349776640000073, 1418.147168774629790, 229.8848599606979803 ) ) ;
#10544 = CARTESIAN_POINT ( 'NONE',  ( 9.357230663576631358, 1435.432546474700075, 208.4556945073640009 ) ) ;
#10545 = EDGE_CURVE ( 'NONE', #66863, #24877, #71239, .T. ) ;
#10547 = VERTEX_POINT ( 'NONE', #98396 ) ;
#10546 = CARTESIAN_POINT ( 'NONE',  ( -6.615182365728785818, 1366.249946645814816, 208.3718459617061285 ) ) ;
#10548 = ORIENTED_EDGE ( 'NONE', *, *, #16459, .F. ) ;
#10549 = CARTESIAN_POINT ( 'NONE',  ( -22.84135781497329987, 1409.740462049710004, 209.6362336836220095 ) ) ;
#10550 = FACE_OUTER_BOUND ( 'NONE', #65360, .T. ) ;
#10551 = CARTESIAN_POINT ( 'NONE',  ( -9.910697518993066168, 1439.577035592592665, 153.0464723132166966 ) ) ;
#10552 = B_SPLINE_CURVE_WITH_KNOTS ( 'NONE', 3,
 ( #40590, #68028, #23774, #66375, #24864, #99930, #59067, #93190, #16458, #50653, #14826, #57424, #100493, #91549, #8082, #102138, #90985, #48464, #108899, #82602, #57961, #5892, #92094, #27114, #2491, #51766, #53432, #35502, #85900, #273, #34399, #26543, #77515, #17565, #61298, #87579, #87006, #103814, #36069, #60169, #52331, #95964, #70254, #102674, #93724, #816, #9207, #104361, #19225, #43367, #1360, #36608 ),
 .UNSPECIFIED., .F., .F.,
 ( 4, 2, 2, 1, 1, 1, 1, 1, 2, 2, 2, 2, 1, 1, 1, 1, 1, 2, 2, 2, 2, 1, 1, 1, 1, 2, 2, 2, 1, 1, 1, 1, 2, 2, 4 ),
 ( 0.000000000000000000, 0.2499999999998676614, 0.3749999999998021583, 0.4374999999997692957, 0.4687499999997517541, 0.4843749999997438715, 0.4921874999997398747, 0.4960937499997377653, 0.4980468749997370437, 0.4999999999997362110, 0.6249999999996997957, 0.6874999999996812550, 0.7187499999996714850, 0.7343749999996661559, 0.7421874999996637134, 0.7460937499996643796, 0.7480468749996647126, 0.7490234374996664890, 0.7499999999996681543, 0.8124999999997845057, 0.8437499999998424594, 0.8593749999998731015, 0.8671874999998884226, 0.8710937499998943068, 0.8730468749998955280, 0.8740234374998968603, 0.8749999999998980815, 0.9062499999999307221, 0.9218749999999444888, 0.9296874999999530376, 0.9335937499999571454, 0.9355468749999610312, 0.9365234374999620304, 0.9374999999999629186, 1.000000000000000000 ),
 .UNSPECIFIED. ) ;
#10553 = CARTESIAN_POINT ( 'NONE',  ( -0.01532161567281509901, 1408.960427760659968, 186.0999207095659926 ) ) ;
#10554 = CIRCLE ( 'NONE', #30189, 26.00000000000000711 ) ;
#10555 = CIRCLE ( 'NONE', #60705, 1.999999999999999556 ) ;
#10556 = CARTESIAN_POINT ( 'NONE',  ( -18.76327566866549645, 1416.196255291290072, 207.5730052496820122 ) ) ;
#10557 = CARTESIAN_POINT ( 'NONE',  ( -22.89689784409999973, 1430.784059188729998, 215.1258104306580208 ) ) ;
#10558 = CARTESIAN_POINT ( 'NONE',  ( 35.81931705070430638, 1463.269900429220115, 267.9387327459060089 ) ) ;
#10559 = CARTESIAN_POINT ( 'NONE',  ( -8.825868239193008336, 1465.145812743426859, 232.9019923126272715 ) ) ;
#10560 = CARTESIAN_POINT ( 'NONE',  ( 9.218600481020001070, 1445.521936428739991, 184.5777863060980053 ) ) ;
#10561 = CARTESIAN_POINT ( 'NONE',  ( 5.772403774305000290, 1516.676340709600026, 205.8583240277470168 ) ) ;
#10562 = ORIENTED_EDGE ( 'NONE', *, *, #96759, .F. ) ;
#10563 = CARTESIAN_POINT ( 'NONE',  ( 21.65343676871068723, 1411.029628520915139, 216.8370129969001425 ) ) ;
#10564 = CARTESIAN_POINT ( 'NONE',  ( 1.506875757802919935, 1462.572888004679953, 183.0571693780200064 ) ) ;
#10565 = CARTESIAN_POINT ( 'NONE',  ( 23.92908890809999889, 1410.712361784030008, 208.4166298941610194 ) ) ;
#10566 = ORIENTED_EDGE ( 'NONE', *, *, #4155, .F. ) ;
#10567 = CARTESIAN_POINT ( 'NONE',  ( -3.827327205999999649, 1424.046157813729906, 127.2892455880980123 ) ) ;
#10568 = ADVANCED_FACE ( 'NONE', ( #2175 ), #41838, .T. ) ;
#10569 = CARTESIAN_POINT ( 'NONE',  ( 26.16029670472540047, 1451.268733793390084, 136.4243401975820120 ) ) ;
#10570 = DIRECTION ( 'NONE',  ( 0.0002626049189776629507, -0.0002559000790209099187, -0.9999999327769008017 ) ) ;
#10571 = CARTESIAN_POINT ( 'NONE',  ( -48.13349220509999782, 1389.567894374660000, 227.8887496536589765 ) ) ;
#10572 = ADVANCED_FACE ( 'NONE', ( #24430 ), #57528, .F. ) ;
#10573 = CARTESIAN_POINT ( 'NONE',  ( -11.56174262037960077, 1388.455307283889624, 216.7304434050078044 ) ) ;
#10574 = CARTESIAN_POINT ( 'NONE',  ( 17.83376335750000052, 1409.535829129529930, 195.1640540924980201 ) ) ;
#10575 = CARTESIAN_POINT ( 'NONE',  ( 17.11714625305219073, 1444.740067931810245, 162.7561045841208909 ) ) ;
#10576 = CARTESIAN_POINT ( 'NONE',  ( 2.609822991816500348, 1439.645108688199571, 183.4245757125495118 ) ) ;
#10578 = CARTESIAN_POINT ( 'NONE',  ( -18.59108776923753226, 1424.390149891285546, 224.8865353940923626 ) ) ;
#10577 = CARTESIAN_POINT ( 'NONE',  ( 0.8893907640070000120, 1417.383361611430018, 235.4581877438980086 ) ) ;
#10579 = CARTESIAN_POINT ( 'NONE',  ( 11.60004869885203682, 1425.894332500278097, 137.5113157688821275 ) ) ;
#10580 = EDGE_CURVE ( 'NONE', #106306, #103193, #81148, .T. ) ;
#10581 = VECTOR ( 'NONE', #36414, 1000.000000000000114 ) ;
#10582 = CARTESIAN_POINT ( 'NONE',  ( 27.85007276605439941, 1509.193792694948570, 207.4562352035727884 ) ) ;
#10583 = CARTESIAN_POINT ( 'NONE',  ( 6.559168636745000391, 1516.960844870249957, 214.1244393295569921 ) ) ;
#10584 = CARTESIAN_POINT ( 'NONE',  ( 2.472529913803048984, 1523.678648413191922, 242.8674788698241400 ) ) ;
#10585 = ORIENTED_EDGE ( 'NONE', *, *, #11168, .F. ) ;
#10586 = CARTESIAN_POINT ( 'NONE',  ( -16.91437751779999843, 1417.214263006909960, 207.5096583893090099 ) ) ;
#10587 = LINE ( 'NONE', #44758, #108873 ) ;
#10588 = CARTESIAN_POINT ( 'NONE',  ( -0.4694225489305150489, 1409.462648608420068, 232.8560743051169766 ) ) ;
#10589 = EDGE_CURVE ( 'NONE', #100027, #45257, #41257, .T. ) ;
#10590 = DIRECTION ( 'NONE',  ( 1.000000000000000000, 0.000000000000000000, 0.000000000000000000 ) ) ;
#10591 = CARTESIAN_POINT ( 'NONE',  ( 5.145309177750649887, 1422.426130283250131, 194.5914460530619863 ) ) ;
#10592 = DIRECTION ( 'NONE',  ( 0.000000000000000000, 0.000000000000000000, 1.000000000000000000 ) ) ;
#10593 = CARTESIAN_POINT ( 'NONE',  ( -19.80583356029999820, 1445.467019065099976, 219.6133833564979909 ) ) ;
#10594 = CARTESIAN_POINT ( 'NONE',  ( -14.48519483975229960, 1416.181292564900104, 203.8595933512790168 ) ) ;
#10595 = CARTESIAN_POINT ( 'NONE',  ( -12.31888605675350057, 1378.301144730269925, 209.5654755735049832 ) ) ;
#10596 = CARTESIAN_POINT ( 'NONE',  ( -45.55748378925329689, 1443.471975657500025, 268.9766690249090288 ) ) ;
#10597 = CARTESIAN_POINT ( 'NONE',  ( 25.75379067826139945, 1440.913060398739844, 220.5312563427889927 ) ) ;
#10598 = CARTESIAN_POINT ( 'NONE',  ( -14.50129934600000148, 1422.728001101090058, 196.3816483097989760 ) ) ;
#10599 = ORIENTED_EDGE ( 'NONE', *, *, #990, .F. ) ;
#10600 = EDGE_CURVE ( 'NONE', #85148, #102192, #36479, .T. ) ;
#10601 = CARTESIAN_POINT ( 'NONE',  ( 22.62861454470000311, 1507.212883763329955, 209.7205631874760172 ) ) ;
#10602 = CARTESIAN_POINT ( 'NONE',  ( -11.60387536552270049, 1481.105535834539978, 211.4044418330699955 ) ) ;
#10603 = CARTESIAN_POINT ( 'NONE',  ( -7.031825459540000267, 1486.383742291129920, 182.5071239263980090 ) ) ;
#10604 = CARTESIAN_POINT ( 'NONE',  ( 7.991873292109088922, 1398.150424849050751, 198.8685539432230200 ) ) ;
#10605 = CARTESIAN_POINT ( 'NONE',  ( -15.00563130453249983, 1509.437066463229939, 236.2075740539809772 ) ) ;
#10606 = B_SPLINE_CURVE_WITH_KNOTS ( 'NONE', 3,
 ( #105241, #35272, #104131, #27976, #44801, #61066, #44240, #87337, #62160, #18997, #17333, #69458, #10067, #1693, #53196, #2261, #51528, #60497, #36375, #70564, #105806, #29086, #107982, #21191, #12822, #88441, #38570, #80592, #47545, #72747, #56499, #81665, #37484, #11732 ),
 .UNSPECIFIED., .F., .F.,
 ( 4, 3, 3, 3, 3, 3, 3, 3, 3, 3, 3, 4 ),
 ( -1.999999989989980076, -1.861718069389969976, -1.678534718961790073, -1.493099238245260141, -1.306486601231749978, -1.118423644982459830, -0.9299498955213489904, -0.7415292143806480052, -0.5536198130809719675, -0.3674063791434580839, -0.1827794707570640220, 0.000000000000000000 ),
 .UNSPECIFIED. ) ;
#10607 = ADVANCED_FACE ( 'NONE', ( #90543 ), #67211, .F. ) ;
#10608 = AXIS2_PLACEMENT_3D ( 'NONE', #21325, #57742, #80719 ) ;
#10609 = CARTESIAN_POINT ( 'NONE',  ( 25.25968088009999946, 1449.800564152120160, 211.7062984677579891 ) ) ;
#10610 = CARTESIAN_POINT ( 'NONE',  ( -16.46732193653928533, 1420.114675349507934, 208.7316782250878191 ) ) ;
#10611 = DIRECTION ( 'NONE',  ( -0.8672669759446655080, 0.000000000000000000, -0.4978433412588692542 ) ) ;
#10612 = CARTESIAN_POINT ( 'NONE',  ( -34.42280635277390388, 1383.836280062859942, 233.0998386971220100 ) ) ;
#10613 = CARTESIAN_POINT ( 'NONE',  ( 21.01360359149740020, 1507.224983811549919, 226.0477246056319984 ) ) ;
#10614 = EDGE_CURVE ( 'NONE', #79550, #19461, #31191, .T. ) ;
#10615 = CARTESIAN_POINT ( 'NONE',  ( 5.617607972230620028, 1423.117395914830013, 104.0874243697959969 ) ) ;
#10616 = CARTESIAN_POINT ( 'NONE',  ( -234.5897387251999930, 11221.53578756869865, 2175.945776423289772 ) ) ;
#10617 = CARTESIAN_POINT ( 'NONE',  ( 0.1625026641855710219, 1484.765001907559963, 181.8896783937200041 ) ) ;
#10619 = ORIENTED_EDGE ( 'NONE', *, *, #17357, .F. ) ;
#10618 = CARTESIAN_POINT ( 'NONE',  ( 4.253777714910000007, 1442.471859903390168, 216.9083338397390150 ) ) ;
#10620 = CARTESIAN_POINT ( 'NONE',  ( -12.91247410300000276, 1445.052233488288948, 177.4417055768979026 ) ) ;
#10621 = AXIS2_PLACEMENT_3D ( 'NONE', #109777, #85660, #8960 ) ;
#10622 = CARTESIAN_POINT ( 'NONE',  ( -9.639940909925840019E-16, 1380.874075505639894, 216.4545132979889956 ) ) ;
#10623 = CARTESIAN_POINT ( 'NONE',  ( -31.34137657934000387, 1512.187213306747481, 221.9025654077414345 ) ) ;
#10625 = ORIENTED_EDGE ( 'NONE', *, *, #83893, .F. ) ;
#10624 = CARTESIAN_POINT ( 'NONE',  ( -32.79520046278567236, 1523.954924407800490, 217.1622218713099528 ) ) ;
#10626 = CARTESIAN_POINT ( 'NONE',  ( -16.83566012920760002, 1418.884382950350073, 201.2565057074210131 ) ) ;
#10627 = ORIENTED_EDGE ( 'NONE', *, *, #96163, .F. ) ;
#10628 = CARTESIAN_POINT ( 'NONE',  ( -14.35128743697329945, 1380.312783049660084, 209.6729884863009943 ) ) ;
#10629 = CARTESIAN_POINT ( 'NONE',  ( 5.440512190109999757, 1424.738065781850082, 191.9794586101990319 ) ) ;
#10630 = CARTESIAN_POINT ( 'NONE',  ( 11.54856215818386111, 1426.051318353786428, 138.9194232893295293 ) ) ;
#10631 = CARTESIAN_POINT ( 'NONE',  ( 23.35503201018713426, 1410.253263171711296, 207.9904190973228140 ) ) ;
#10632 = CARTESIAN_POINT ( 'NONE',  ( -14.65245215464970130, 1420.119839417710182, 213.8659310620899987 ) ) ;
#10633 = DIRECTION ( 'NONE',  ( -0.9995237709234254808, 0.03085824620771311644, -1.986952269380852068E-13 ) ) ;
#10634 = CARTESIAN_POINT ( 'NONE',  ( 11.81689878039349928, 1409.325715576620041, 218.2705614814449859 ) ) ;
#10635 = CARTESIAN_POINT ( 'NONE',  ( -11.32737004039999995, 1391.820807817859986, 205.2942467584589679 ) ) ;
#10636 = CARTESIAN_POINT ( 'NONE',  ( -100.3556198889290130, 1385.221765029460130, 296.3440159043000222 ) ) ;
#10637 = CARTESIAN_POINT ( 'NONE',  ( 2.933761696634608285, 1464.631290068389944, 236.6723688072773939 ) ) ;
#10638 = CARTESIAN_POINT ( 'NONE',  ( -2.470168521978398424, 1523.382868172864164, 242.8787258963054683 ) ) ;
#10639 = ORIENTED_EDGE ( 'NONE', *, *, #86258, .F. ) ;
#10640 = VECTOR ( 'NONE', #64870, 1000.000000000000114 ) ;
#10641 = CARTESIAN_POINT ( 'NONE',  ( 12.32715944251560103, 1492.190983864200007, 209.5901420063510159 ) ) ;
#10643 = ORIENTED_EDGE ( 'NONE', *, *, #89035, .T. ) ;
#10642 = CARTESIAN_POINT ( 'NONE',  ( 21.62164173114529930, 1517.051704408389924, 208.0273405545509888 ) ) ;
#10644 = DIRECTION ( 'NONE',  ( 0.07284846526757217389, 0.01356562619974717963, 0.9972507582819719607 ) ) ;
#10645 = TOROIDAL_SURFACE ( 'NONE', #66047, 2.000000000000000000, 1.000000000000000000 ) ;
#10646 = ORIENTED_EDGE ( 'NONE', *, *, #81643, .T. ) ;
#10647 = CARTESIAN_POINT ( 'NONE',  ( 25.23579092139999958, 1509.794313625030100, 223.6174824585980048 ) ) ;
#10648 = CARTESIAN_POINT ( 'NONE',  ( 3.235004757640449924, 1361.842843053408615, 210.6218459617142003 ) ) ;
#10649 = CARTESIAN_POINT ( 'NONE',  ( -11.48887253859999902, 1433.998994749410031, 151.3897975962979956 ) ) ;
#10650 = CARTESIAN_POINT ( 'NONE',  ( 33.74597417575863290, 1459.080184772059056, 269.5147043096913535 ) ) ;
#10651 = CARTESIAN_POINT ( 'NONE',  ( -33.34040796508153903, 1523.342713519623658, 222.1177029624612658 ) ) ;
#10652 = CARTESIAN_POINT ( 'NONE',  ( -28.28208339020000039, 1508.151294418729776, 209.1342425839550287 ) ) ;
#10653 = CARTESIAN_POINT ( 'NONE',  ( 31.88717309313577530, 1525.425665131969026, 201.2219480880026197 ) ) ;
#10654 = CARTESIAN_POINT ( 'NONE',  ( -6.064575543111884848, 1516.744957452581048, 213.5348771919006197 ) ) ;
#10655 = DIRECTION ( 'NONE',  ( 1.755985294532464991E-16, -1.000000000000000000, 1.338183447452830017E-16 ) ) ;
#10656 = CARTESIAN_POINT ( 'NONE',  ( -7.895287119950644694, 1368.828961991272308, 207.6218459616987673 ) ) ;
#10657 = CARTESIAN_POINT ( 'NONE',  ( -18.93704128152869970, 1430.332824596809814, 208.8580461249810014 ) ) ;
#10658 = CARTESIAN_POINT ( 'NONE',  ( -13.49160170200362963, 1516.729020965288555, 226.1741075741266229 ) ) ;
#10659 = CARTESIAN_POINT ( 'NONE',  ( -4.044321718124999521, 1517.001127920769704, 206.8363583507369867 ) ) ;
#10660 = VECTOR ( 'NONE', #26822, 1000.000000000000000 ) ;
#10661 = CARTESIAN_POINT ( 'NONE',  ( -12.97204092183419988, 1434.766546360639950, 149.2832816642720104 ) ) ;
#10662 = B_SPLINE_SURFACE_WITH_KNOTS ( 'NONE', 5, 5, ( 
 ( #42590, #76743, #55, #68926, #60515, #9530, #43698, #77852, #63825 ),
 ( #88993, #46475, #106353, #44821, #78974, #27993, #105822, #79514, #19583 ),
 ( #11745, #35853, #88458, #71704, #95750, #104698, #2818, #1713, #70037 ),
 ( #45374, #53217, #2278, #53787, #87924, #38052, #104149, #96305, #12281 ),
 ( #62178, #29639, #62748, #97938, #80607, #11211, #36937, #87356, #71134 ),
 ( #21206, #27435, #105255, #20135, #61618, #28549, #29100, #86795, #72229 ) ),
 .UNSPECIFIED., .F., .F., .F.,
 ( 6, 6 ),
 ( 6, 3, 6 ),
 ( 0.000000000000000000, 8.627065936320001072 ),
 ( 0.000000000000000000, 1.000000000000000000, 2.000000000000000000 ),
 .UNSPECIFIED. ) ;
#10663 = CARTESIAN_POINT ( 'NONE',  ( 0.000000000000000000, 1450.913060387330006, 198.0847581337980046 ) ) ;
#10664 = CARTESIAN_POINT ( 'NONE',  ( 0.2999317787290010084, 1497.191549081989933, 197.4584646491989872 ) ) ;
#10665 = CARTESIAN_POINT ( 'NONE',  ( -68.75491282716379260, 1379.747882944909861, 280.3318558483960601 ) ) ;
#10666 = B_SPLINE_CURVE_WITH_KNOTS ( 'NONE', 3,
 ( #94221, #51693, #59545, #41632, #109939, #93658, #16939, #747, #42736, #34329, #94788, #68507 ),
 .UNSPECIFIED., .F., .F.,
 ( 4, 2, 2, 2, 2, 4 ),
 ( -0.1123552069981540030, -0.09789079992753631221, -0.08345977618154098998, -0.05408602697413120164, -0.02844237633788339326, 0.000000000000000000 ),
 .UNSPECIFIED. ) ;
#10667 = CYLINDRICAL_SURFACE ( 'NONE', #83170, 2.999999999999995115 ) ;
#10668 = EDGE_LOOP ( 'NONE', ( #12851, #34431, #25475, #92898 ) ) ;
#10669 = CARTESIAN_POINT ( 'NONE',  ( 43.50118997730000103, 1438.239417958949844, 263.8966302629980305 ) ) ;
#10670 = CARTESIAN_POINT ( 'NONE',  ( -27.46043821989999856, 1488.693027618630140, 209.0953481391420041 ) ) ;
#10672 = CARTESIAN_POINT ( 'NONE',  ( 16.35901261092910275, 1409.492683085800081, 193.1285600932399973 ) ) ;
#10671 = CARTESIAN_POINT ( 'NONE',  ( -11.06108549758080173, 1426.493804035829953, 95.13674927509649137 ) ) ;
#10673 = CARTESIAN_POINT ( 'NONE',  ( 1.715704490974999885, 1516.757508073510053, 212.3732403323669757 ) ) ;
#10674 = CARTESIAN_POINT ( 'NONE',  ( 2.782332782707229946, 1396.010221589069943, 198.4612922233270069 ) ) ;
#10675 = CARTESIAN_POINT ( 'NONE',  ( -0.02955819112566620069, 1517.151704408390060, 225.0080808726450243 ) ) ;
#10676 = AXIS2_PLACEMENT_3D ( 'NONE', #58441, #84173, #67408 ) ;
#10677 = CARTESIAN_POINT ( 'NONE',  ( -26.19682245239999929, 1416.543456363630185, 259.6166969371979576 ) ) ;
#10678 = CARTESIAN_POINT ( 'NONE',  ( 2.931762418139999937, 1484.928921319690062, 220.6147940381989940 ) ) ;
#10679 = CARTESIAN_POINT ( 'NONE',  ( 28.97445500250269745, 1509.604966148099948, 209.5493756428880090 ) ) ;
#10680 = DIRECTION ( 'NONE',  ( 0.06162841671618445039, -0.9961946980917499861, 0.06162841671618458916 ) ) ;
#10681 = CARTESIAN_POINT ( 'NONE',  ( 30.22858968940000324, 1451.857573268230226, 134.8239104374980002 ) ) ;
#10682 = ORIENTED_EDGE ( 'NONE', *, *, #39103, .F. ) ;
#10683 = CARTESIAN_POINT ( 'NONE',  ( 13.90997033016400053, 1397.713899063759982, 206.9547035159640131 ) ) ;
#10684 = CARTESIAN_POINT ( 'NONE',  ( 10.08864075595840148, 1461.294693056749793, 208.2010832468129991 ) ) ;
#10685 = CARTESIAN_POINT ( 'NONE',  ( 37.88774006571860298, 1442.824633575369944, 137.1073183462559939 ) ) ;
#10686 = ORIENTED_EDGE ( 'NONE', *, *, #72040, .F. ) ;
#10687 = ORIENTED_EDGE ( 'NONE', *, *, #13231, .F. ) ;
#10688 = CYLINDRICAL_SURFACE ( 'NONE', #93101, 0.9999999999999976685 ) ;
#10689 = CARTESIAN_POINT ( 'NONE',  ( 7.184880219700001014, 1423.497618239299982, 195.4521118202989953 ) ) ;
#10690 = VERTEX_POINT ( 'NONE', #56968 ) ;
#10691 = CARTESIAN_POINT ( 'NONE',  ( -1.363527627800000142, 1415.665897350729892, 185.3780671533980069 ) ) ;
#10692 = CARTESIAN_POINT ( 'NONE',  ( 8.279338672908640007, 1446.667838523203045, 153.9572786840106176 ) ) ;
#10693 = DIRECTION ( 'NONE',  ( -1.755985294532469921E-16, 1.000000000000000000, -1.338183447452831989E-16 ) ) ;
#10694 = CARTESIAN_POINT ( 'NONE',  ( -5.653753708210000006, 1470.479446996229854, 234.4212017938980068 ) ) ;
#10695 = CARTESIAN_POINT ( 'NONE',  ( 1.957738139717299930, 1421.112252580069935, 183.1490905797940059 ) ) ;
#10696 = CARTESIAN_POINT ( 'NONE',  ( 9.201640575826802504, 1450.639316510839990, 208.3453033095780143 ) ) ;
#10697 = FACE_OUTER_BOUND ( 'NONE', #97105, .T. ) ;
#10698 = CARTESIAN_POINT ( 'NONE',  ( 15.13403569980000007, 1507.625766696829942, 226.3980367026980218 ) ) ;
#10699 = CARTESIAN_POINT ( 'NONE',  ( -0.01171164408179850049, 1516.939568781210028, 202.5649949355269825 ) ) ;
#10700 = CARTESIAN_POINT ( 'NONE',  ( 7.727327114725000001, 1517.232977404109988, 210.8318586907270173 ) ) ;
#10701 = ORIENTED_EDGE ( 'NONE', *, *, #98017, .T. ) ;
#10702 = CARTESIAN_POINT ( 'NONE',  ( 11.86131399675660170, 1432.001727244180074, 149.9720548203619899 ) ) ;
#10703 = EDGE_CURVE ( 'NONE', #15990, #37474, #100799, .T. ) ;
#10704 = AXIS2_PLACEMENT_3D ( 'NONE', #108539, #65462, #107981 ) ;
#10705 = CARTESIAN_POINT ( 'NONE',  ( 1.600048698852036821, 1411.254281879943164, 134.0999999980979851 ) ) ;
#10706 = ORIENTED_EDGE ( 'NONE', *, *, #89828, .F. ) ;
#10707 = CARTESIAN_POINT ( 'NONE',  ( -15.56138138465544607, 1506.691119431732886, 193.2904356335322689 ) ) ;
#10708 = EDGE_CURVE ( 'NONE', #110178, #49611, #84749, .T. ) ;
#10709 = CARTESIAN_POINT ( 'NONE',  ( -3.523962699983150149, 1476.511731499819916, 220.0526012347959863 ) ) ;
#10710 = CARTESIAN_POINT ( 'NONE',  ( -9.959969825530610166, 1470.547643313240087, 212.5949768734770089 ) ) ;
#10711 = CARTESIAN_POINT ( 'NONE',  ( -6.189336700450000173, 1423.191529671129956, 186.6229957612979717 ) ) ;
#10712 = AXIS2_PLACEMENT_3D ( 'NONE', #46501, #12864, #106380 ) ;
#10713 = CARTESIAN_POINT ( 'NONE',  ( 2.278116099415719908, 1409.246459464170130, 270.3712219384140099 ) ) ;
#10714 = CARTESIAN_POINT ( 'NONE',  ( -7.052967567875161770, 1427.664849047028611, 137.0999999980979851 ) ) ;
#10715 = CARTESIAN_POINT ( 'NONE',  ( -7.192114391989999689, 1473.717433820989982, 200.7095979941090036 ) ) ;
#10716 = CARTESIAN_POINT ( 'NONE',  ( 11.01187558969999891, 1492.459055990190109, 212.4069249470189789 ) ) ;
#10717 = CARTESIAN_POINT ( 'NONE',  ( -44.38987040500000347, 1379.668466784379916, 229.4021183653589731 ) ) ;
#10718 = CARTESIAN_POINT ( 'NONE',  ( 8.708214553643372824, 1424.815002788605398, 195.6916425196928913 ) ) ;
#10720 = CARTESIAN_POINT ( 'NONE',  ( 10.59718513049560151, 1469.650899207149905, 205.1638397631170108 ) ) ;
#10719 = CARTESIAN_POINT ( 'NONE',  ( -14.29847877429999947, 1503.225636699989991, 208.9837668400270161 ) ) ;
#10721 = CARTESIAN_POINT ( 'NONE',  ( -31.51240728497394628, 1379.723496874464445, 219.1466601198638386 ) ) ;
#10722 = CARTESIAN_POINT ( 'NONE',  ( 17.75620770209309995, 1415.752091378990144, 224.9496030967819991 ) ) ;
#10723 = CARTESIAN_POINT ( 'NONE',  ( -7.458171709695000651, 1513.513616978009850, 202.5644110759569969 ) ) ;
#10724 = ORIENTED_EDGE ( 'NONE', *, *, #52290, .F. ) ;
#10725 = CARTESIAN_POINT ( 'NONE',  ( 31.32742178679999512, 1440.913060387330006, 255.3819207742980097 ) ) ;
#10726 = AXIS2_PLACEMENT_3D ( 'NONE', #9936, #1012, #45780 ) ;
#10727 = CARTESIAN_POINT ( 'NONE',  ( -113.3174119514818301, 1378.913060387289988, 300.7228204909002329 ) ) ;
#10728 = EDGE_CURVE ( 'NONE', #41661, #42951, #49671, .T. ) ;
#10729 = CARTESIAN_POINT ( 'NONE',  ( 38.19123335760763638, 1450.350430573902031, 134.7938291898653915 ) ) ;
#10730 = CARTESIAN_POINT ( 'NONE',  ( -8.727481514770000004, 1384.944701276459909, 199.8872933186289913 ) ) ;
#10731 = CARTESIAN_POINT ( 'NONE',  ( 11.96188367727480006, 1407.497305617939901, 269.6154717270600258 ) ) ;
#10733 = EDGE_LOOP ( 'NONE', ( #10242, #27059, #45551 ) ) ;
#10732 = CARTESIAN_POINT ( 'NONE',  ( -1.379638663386490105, 1515.081065330719866, 204.7928232953929921 ) ) ;
#10734 = DIRECTION ( 'NONE',  ( -0.02616798426450838572, -0.9993150019883944024, 0.02616798426450848286 ) ) ;
#10735 = FACE_OUTER_BOUND ( 'NONE', #108441, .T. ) ;
#10736 = CYLINDRICAL_SURFACE ( 'NONE', #10993, 1.999999999999994893 ) ;
#10737 = CARTESIAN_POINT ( 'NONE',  ( -19.75056259240000145, 1465.177823603190063, 209.1218459616989946 ) ) ;
#10738 = CARTESIAN_POINT ( 'NONE',  ( 11.40944910053500116, 1511.843510977570077, 224.6458867293669925 ) ) ;
#10739 = CARTESIAN_POINT ( 'NONE',  ( 3.442434976254919565, 1370.269799182473889, 208.1179161451651112 ) ) ;
#10740 = CARTESIAN_POINT ( 'NONE',  ( 27.87567397839760375, 1509.925536542059945, 194.5356986537630064 ) ) ;
#10741 = CARTESIAN_POINT ( 'NONE',  ( 22.75273496409597485, 1512.187213306747481, 234.5707981297185825 ) ) ;
#10742 = DIRECTION ( 'NONE',  ( 5.898059818321139072E-14, 0.000000000000000000, 1.000000000000000000 ) ) ;
#10743 = CARTESIAN_POINT ( 'NONE',  ( 14.99625699449999949, 1410.404882082729955, 227.4791858470979946 ) ) ;
#10744 = CARTESIAN_POINT ( 'NONE',  ( 9.799773730352699275, 1469.816546466489854, 211.4317690604339930 ) ) ;
#10745 = DIRECTION ( 'NONE',  ( -7.363503285428202099E-05, 3.211508572083940804E-06, 0.9999999972837841922 ) ) ;
#10746 = AXIS2_PLACEMENT_3D ( 'NONE', #21610, #64774, #91594 ) ;
#10747 = CARTESIAN_POINT ( 'NONE',  ( -3.268859434184999913, 1516.922519270759949, 206.6438591998669949 ) ) ;
#10748 = CARTESIAN_POINT ( 'NONE',  ( 41.20202881409999662, 1425.323100257629903, 268.8974569184979941 ) ) ;
#10749 = CARTESIAN_POINT ( 'NONE',  ( -18.72407526530000155, 1458.246115540929850, 227.3156487912980026 ) ) ;
#10750 = EDGE_CURVE ( 'NONE', #437, #93985, #28444, .T. ) ;
#10751 = CARTESIAN_POINT ( 'NONE',  ( 18.17633956390000094, 1435.132278384110123, 145.0981326318980109 ) ) ;
#10752 = CARTESIAN_POINT ( 'NONE',  ( 19.87154596619999936, 1488.588627089529837, 190.3431199549980022 ) ) ;
#10753 = CARTESIAN_POINT ( 'NONE',  ( -21.44806981200000351, 1428.950306416729973, 219.4680445577980095 ) ) ;
#10754 = CARTESIAN_POINT ( 'NONE',  ( 0.7941283559409979542, 1479.063403849489987, 229.6081502463990205 ) ) ;
#10755 = CARTESIAN_POINT ( 'NONE',  ( -17.66442964079999811, 1420.867159957530021, 226.1080994653979985 ) ) ;
#10756 = CARTESIAN_POINT ( 'NONE',  ( -11.33475729453610192, 1500.341569088609958, 210.4138246906279903 ) ) ;
#10757 = CARTESIAN_POINT ( 'NONE',  ( -40.71506854697640421, 1443.618868117700003, 137.1015915340059905 ) ) ;
#10758 = EDGE_CURVE ( 'NONE', #65489, #99771, #71413, .T. ) ;
#10759 = CARTESIAN_POINT ( 'NONE',  ( -4.363122647530000009, 1432.413060387330006, 146.1721969590979882 ) ) ;
#10760 = CARTESIAN_POINT ( 'NONE',  ( -16.32619598790000026, 1416.471320734319988, 209.2727045491550086 ) ) ;
#10761 = CARTESIAN_POINT ( 'NONE',  ( -12.53380499110000024, 1442.773887285770115, 185.9733677063979940 ) ) ;
#10762 = CARTESIAN_POINT ( 'NONE',  ( -7.544607327050279366, 1384.638857144239864, 219.0792297806210058 ) ) ;
#10763 = CARTESIAN_POINT ( 'NONE',  ( -3.326017048431102679E-16, 1419.995592097834106, 171.1876449949939456 ) ) ;
#10764 = VERTEX_POINT ( 'NONE', #52433 ) ;
#10765 = CARTESIAN_POINT ( 'NONE',  ( -3.276907064705000039, 1511.440441732949921, 201.4048293130770162 ) ) ;
#10766 = CARTESIAN_POINT ( 'NONE',  ( -13.41295867642740092, 1409.381451225490082, 215.7039827110959891 ) ) ;
#10767 = CARTESIAN_POINT ( 'NONE',  ( -5.483194490039999813, 1439.280902438360044, 154.7474842100980084 ) ) ;
#10768 = CARTESIAN_POINT ( 'NONE',  ( -33.98065672744881027, 1443.913060387328869, 154.9321739644268234 ) ) ;
#10769 = CARTESIAN_POINT ( 'NONE',  ( -27.10895137460000015, 1469.515388080030107, 268.1710267444980218 ) ) ;
#10770 = CARTESIAN_POINT ( 'NONE',  ( -11.60387536552270049, 1481.105535834539978, 211.4044418330699955 ) ) ;
#10771 = CARTESIAN_POINT ( 'NONE',  ( 0.4863421998530879642, 1418.702335047680208, 184.7127968358159933 ) ) ;
#10772 = CARTESIAN_POINT ( 'NONE',  ( -73.29286402757139740, 1384.653836098580086, 298.4869674903130203 ) ) ;
#10773 = CARTESIAN_POINT ( 'NONE',  ( -34.05251678726769882, 1384.976729253169879, 208.0367919944089863 ) ) ;
#10774 = CARTESIAN_POINT ( 'NONE',  ( 17.89269544292019631, 1424.514345381910061, 226.2830465645759830 ) ) ;
#10775 = CARTESIAN_POINT ( 'NONE',  ( 17.23902921200000193, 1416.518938591829965, 215.4040154682980130 ) ) ;
#10776 = CARTESIAN_POINT ( 'NONE',  ( 15.59201085350000149, 1506.806593714529981, 224.7816022336980097 ) ) ;
#10777 = CARTESIAN_POINT ( 'NONE',  ( -5.387811863060000483, 1496.648312753189884, 199.2595355468089906 ) ) ;
#10778 = LINE ( 'NONE', #88050, #44800 ) ;
#10779 = CARTESIAN_POINT ( 'NONE',  ( -8.371286044520001468, 1384.927627653609989, 199.7749606464490171 ) ) ;
#10780 = CARTESIAN_POINT ( 'NONE',  ( 1.435281448510400182, 1482.857262105389964, 235.7275092897180002 ) ) ;
#10781 = CARTESIAN_POINT ( 'NONE',  ( 14.11509896619999971, 1414.913060387329779, 199.7393156684579765 ) ) ;
#10782 = DIRECTION ( 'NONE',  ( 0.5030436214085421964, 0.000000000000000000, 0.8642610224695890242 ) ) ;
#10783 = CIRCLE ( 'NONE', #89427, 1.999999999999921174 ) ;
#10784 = CARTESIAN_POINT ( 'NONE',  ( 3.226607219819999539, 1423.257519486769979, 193.6078189732990040 ) ) ;
#10785 = B_SPLINE_CURVE_WITH_KNOTS ( 'NONE', 5,
 ( #22243, #30110, #37983, #98425, #37433, #71631, #73237, #29035, #72165, #107379, #21697 ),
 .UNSPECIFIED., .F., .F.,
 ( 6, 5, 6 ),
 ( -167.7485006210000051, -75.51693185479999215, -75.51691072595589560 ),
 .UNSPECIFIED. ) ;
#10786 = CARTESIAN_POINT ( 'NONE',  ( 22.99745501010000126, 1409.716149210629965, 209.9703408740099917 ) ) ;
#10787 = B_SPLINE_SURFACE_WITH_KNOTS ( 'NONE', 5, 5, ( 
 ( #109416, #22597, #59015, #39440, #99323, #24811 ),
 ( #101523, #41090, #107744, #32141, #57374, #74165 ),
 ( #92047, #56800, #14224, #48410, #100981, #75267 ),
 ( #84736, #50062, #82554, #91501, #109957, #108295 ),
 ( #73616, #23174, #93142, #33235, #58457, #48966 ),
 ( #108845, #100445, #66872, #84189, #66327, #23728 ),
 ( #24276, #57914, #15319, #49513, #83637, #92585 ),
 ( #15856, #7488, #41649, #94807, #52823, #59561 ),
 ( #17514, #51156, #18625, #95363, #51712, #26486 ) ),
 .UNSPECIFIED., .F., .F., .F.,
 ( 6, 3, 6 ),
 ( 6, 6 ),
 ( 3.918736331710000353, 7.747513759300000302, 12.84118059900000119 ),
 ( 0.000000000000000000, 2.000000000000000000 ),
 .UNSPECIFIED. ) ;
#10788 = CARTESIAN_POINT ( 'NONE',  ( 4.500000000000000000, 1448.210448412289907, 182.3842140122979743 ) ) ;
#10789 = CARTESIAN_POINT ( 'NONE',  ( 19.03958482845590083, 1453.804128677390054, 200.7927815628769963 ) ) ;
#10790 = CARTESIAN_POINT ( 'NONE',  ( -16.26200603700000258, 1421.946001659629928, 227.1818636008979979 ) ) ;
#10792 = CARTESIAN_POINT ( 'NONE',  ( -13.48698396448789971, 1379.694001781489987, 211.4569706220899832 ) ) ;
#10791 = CARTESIAN_POINT ( 'NONE',  ( 11.90005888108785115, 1434.918254481208578, 147.6452161523065172 ) ) ;
#10793 = CARTESIAN_POINT ( 'NONE',  ( -0.5044665043120000192, 1413.022983338129961, 233.2877477755979783 ) ) ;
#10794 = CARTESIAN_POINT ( 'NONE',  ( -27.01380866140000236, 1450.681584507220123, 136.4483241423979791 ) ) ;
#10795 = CARTESIAN_POINT ( 'NONE',  ( -10.94181931979999867, 1491.470369003389806, 210.4086029903089923 ) ) ;
#10796 = DIRECTION ( 'NONE',  ( -0.9510565162951518658, 0.000000000000000000, 0.3090169943749528914 ) ) ;
#10797 = B_SPLINE_CURVE_WITH_KNOTS ( 'NONE', 5,
 ( #108216, #47224, #81350, #83021, #31504, #64596, #23096, #65134, #99802 ),
 .UNSPECIFIED., .F., .F.,
 ( 6, 3, 6 ),
 ( 0.000000000000000000, 0.4258937504861698975, 1.000000000000000000 ),
 .UNSPECIFIED. ) ;
#10798 = CARTESIAN_POINT ( 'NONE',  ( 10.36616749849999941, 1462.084512446189819, 211.0499673381089849 ) ) ;
#10799 = CARTESIAN_POINT ( 'NONE',  ( -4.040527342105000308, 1516.815231249920089, 204.5109077207270047 ) ) ;
#10800 = CARTESIAN_POINT ( 'NONE',  ( -16.69612950000000140, 1484.879939360330127, 188.0702094165980043 ) ) ;
#10801 = AXIS2_PLACEMENT_3D ( 'NONE', #92742, #101673, #66477 ) ;
#10802 = CARTESIAN_POINT ( 'NONE',  ( 6.392991367490600041, 1505.880701581259927, 218.9074644499650049 ) ) ;
#10803 = CARTESIAN_POINT ( 'NONE',  ( -9.710888762612963632, 1422.734008549482496, 210.6841274085994655 ) ) ;
#10805 = ORIENTED_EDGE ( 'NONE', *, *, #35036, .T. ) ;
#10804 = CARTESIAN_POINT ( 'NONE',  ( -61.35634870417439402, 1379.727770043109786, 268.3354436782490211 ) ) ;
#10806 = ORIENTED_EDGE ( 'NONE', *, *, #90107, .T. ) ;
#10807 = CARTESIAN_POINT ( 'NONE',  ( 11.59845407533470052, 1433.863182457509993, 151.1985623341290079 ) ) ;
#10808 = CARTESIAN_POINT ( 'NONE',  ( 21.59932114087395405, 1525.137906803776104, 184.7402649365362493 ) ) ;
#10809 = ORIENTED_EDGE ( 'NONE', *, *, #43900, .T. ) ;
#10810 = CARTESIAN_POINT ( 'NONE',  ( -105.6182501849999937, 1378.913057670360104, 304.5676750416590153 ) ) ;
#10811 = CARTESIAN_POINT ( 'NONE',  ( -109.6578465720000111, 1384.929364751169942, 311.3230191942589613 ) ) ;
#10812 = SHAPE_REPRESENTATION ( 'Threaded Lock Nut', ( #21632 ), #95028 ) ;
#10814 = CARTESIAN_POINT ( 'NONE',  ( 0.1700419896689999988, 1508.143047484930094, 180.7157097131980095 ) ) ;
#10813 = CARTESIAN_POINT ( 'NONE',  ( 15.87725485892149990, 1417.455994837740036, 191.3130337353669859 ) ) ;
#10815 = FACE_OUTER_BOUND ( 'NONE', #97138, .T. ) ;
#10816 = CARTESIAN_POINT ( 'NONE',  ( 1.002856167820000088, 1507.642691268429871, 181.0118679135980244 ) ) ;
#10817 = CARTESIAN_POINT ( 'NONE',  ( -105.9286161621180042, 1378.913060388629901, 305.0991713824849967 ) ) ;
#10818 = CARTESIAN_POINT ( 'NONE',  ( -24.31736970558739941, 1444.784419045710138, 211.2645309320329829 ) ) ;
#10819 = SURFACE_SIDE_STYLE ('',( #61795 ) ) ;
#10820 = CARTESIAN_POINT ( 'NONE',  ( -6.934528567894999718, 1516.588006113850042, 211.9958048218269937 ) ) ;
#10821 = CARTESIAN_POINT ( 'NONE',  ( 38.53505231964519595, 1437.347470673020098, 134.0999999971709826 ) ) ;
#10822 = CARTESIAN_POINT ( 'NONE',  ( 10.97017907350000065, 1432.399092116580050, 151.7699749429979761 ) ) ;
#10823 = CARTESIAN_POINT ( 'NONE',  ( -33.36586802512182715, 1512.187213306747481, 201.9069332299493169 ) ) ;
#10824 = VERTEX_POINT ( 'NONE', #26084 ) ;
#10825 = CARTESIAN_POINT ( 'NONE',  ( 13.81711443553279928, 1435.003621955109793, 148.8829541362160001 ) ) ;
#10826 = CARTESIAN_POINT ( 'NONE',  ( -4.682234856550000046, 1438.893385222290135, 227.1256850459990062 ) ) ;
#10827 = VERTEX_POINT ( 'NONE', #42351 ) ;
#10828 = ORIENTED_EDGE ( 'NONE', *, *, #6329, .T. ) ;
#10829 = ORIENTED_EDGE ( 'NONE', *, *, #32300, .T. ) ;
#10830 = CARTESIAN_POINT ( 'NONE',  ( -7.475494293344999264, 1511.623805160490065, 215.5182564808370103 ) ) ;
#10831 = CARTESIAN_POINT ( 'NONE',  ( 16.72494116235394301, 1513.190421814297224, 196.6872607197416585 ) ) ;
#10832 = CIRCLE ( 'NONE', #87719, 0.5000000000000032196 ) ;
#10833 = CARTESIAN_POINT ( 'NONE',  ( -0.3328314641405109575, 1452.976685807730291, 183.2631399573310205 ) ) ;
#10834 = CARTESIAN_POINT ( 'NONE',  ( 2.500000000000000000, 1439.615672362369878, 170.5246407131980106 ) ) ;
#10836 = CARTESIAN_POINT ( 'NONE',  ( 0.8459567068543710766, 1465.606436347200088, 198.1403988231419930 ) ) ;
#10835 = B_SPLINE_CURVE_WITH_KNOTS ( 'NONE', 3,
 ( #51786, #33300, #15935, #34419, #83715, #85925, #67495, #101599, #66396, #16481, #58535, #25441, #50671, #68592, #59634, #15395, #100516, #57984, #293 ),
 .UNSPECIFIED., .F., .F.,
 ( 4, 2, 2, 2, 1, 1, 1, 2, 2, 2, 4 ),
 ( 0.000000000000000000, 0.2500000000001726952, 0.3750000000002590150, 0.4375000000003022027, 0.4687500000003208545, 0.4843750000003272937, 0.4921875000003335665, 0.4960937500003307354, 0.5000000000003279599, 0.7500000000001639799, 1.000000000000000000 ),
 .UNSPECIFIED. ) ;
#10837 = CARTESIAN_POINT ( 'NONE',  ( -18.52846729114558144, 1445.641343889673180, 214.4839088109478382 ) ) ;
#10838 = CARTESIAN_POINT ( 'NONE',  ( -58.27299464524384121, 1379.718854485406837, 257.4714984816578180 ) ) ;
#10839 = CARTESIAN_POINT ( 'NONE',  ( 4.222051968967549307, 1446.225890581839849, 170.2166983236299700 ) ) ;
#10840 = CARTESIAN_POINT ( 'NONE',  ( 8.559858904628349308, 1437.030483964089854, 207.9845584131589931 ) ) ;
#10841 = ORIENTED_EDGE ( 'NONE', *, *, #32, .F. ) ;
#10842 = CARTESIAN_POINT ( 'NONE',  ( -3.462948834675000143, 1516.956048353049937, 206.8373194734570006 ) ) ;
#10843 = ORIENTED_EDGE ( 'NONE', *, *, #55441, .T. ) ;
#10844 = CARTESIAN_POINT ( 'NONE',  ( 26.08449786710409768, 1440.913060387330006, 242.4625039277019880 ) ) ;
#10845 = CIRCLE ( 'NONE', #73418, 1.999999999999998668 ) ;
#10846 = CARTESIAN_POINT ( 'NONE',  ( -20.01067436350000150, 1507.877435269729858, 188.9709114762979993 ) ) ;
#10847 = ORIENTED_EDGE ( 'NONE', *, *, #57868, .F. ) ;
#10848 = CARTESIAN_POINT ( 'NONE',  ( -6.551934178310329315, 1508.551568321310015, 202.1599716710999814 ) ) ;
#10849 = CARTESIAN_POINT ( 'NONE',  ( -14.94606559790000055, 1410.367200001129959, 190.7402031657980217 ) ) ;
#10850 = CARTESIAN_POINT ( 'NONE',  ( -57.37605527416430817, 1379.717849395646226, 260.5878764870727196 ) ) ;
#10852 = DIRECTION ( 'NONE',  ( -0.000000000000000000, 1.000000000000000000, -0.000000000000000000 ) ) ;
#10851 = CARTESIAN_POINT ( 'NONE',  ( -24.90010528310000026, 1441.007489118620015, 210.4306619436680137 ) ) ;
#10853 = CARTESIAN_POINT ( 'NONE',  ( 3.654206417870119683, 1423.822803498439953, 192.8935211664289966 ) ) ;
#10854 = CARTESIAN_POINT ( 'NONE',  ( 6.144376325710431352, 1512.187213306747481, 247.6867189913432981 ) ) ;
#10855 = CARTESIAN_POINT ( 'NONE',  ( 26.75392368510250307, 1441.320991048120050, 137.5422836279790033 ) ) ;
#10856 = CARTESIAN_POINT ( 'NONE',  ( -27.08505272378080164, 1438.263425979839894, 136.9491044588319824 ) ) ;
#10857 = CARTESIAN_POINT ( 'NONE',  ( 18.91392684480000241, 1435.157588376100193, 144.3614089622979861 ) ) ;
#10859 = CARTESIAN_POINT ( 'NONE',  ( 1.569161254424999985, 1517.051704408389924, 201.3992656178269840 ) ) ;
#10858 = CARTESIAN_POINT ( 'NONE',  ( 15.71587021594741884, 1409.995737203585577, 191.8203616610946085 ) ) ;
#10860 = CARTESIAN_POINT ( 'NONE',  ( 2.294209629405000062, 1516.603620185149794, 214.8927295341169952 ) ) ;
#10861 = FACE_OUTER_BOUND ( 'NONE', #21519, .T. ) ;
#10862 = CARTESIAN_POINT ( 'NONE',  ( 5.835879592667029492, 1511.569910118449798, 217.3960280942959855 ) ) ;
#10863 = EDGE_CURVE ( 'NONE', #109438, #104137, #99132, .T. ) ;
#10864 = CARTESIAN_POINT ( 'NONE',  ( 28.32265147949999928, 1509.673549455729926, 207.2611521497780132 ) ) ;
#10865 = CARTESIAN_POINT ( 'NONE',  ( -6.934528567894999718, 1516.588006113850042, 211.9958048218269937 ) ) ;
#10866 = CARTESIAN_POINT ( 'NONE',  ( -18.16348015480000200, 1416.820969729830040, 209.0764828567799896 ) ) ;
#10867 = CARTESIAN_POINT ( 'NONE',  ( 31.25788889089079703, 1523.954924407802764, 221.8935803876606485 ) ) ;
#10869 = VERTEX_POINT ( 'NONE', #110110 ) ;
#10868 = CARTESIAN_POINT ( 'NONE',  ( -93.52692659189999347, 1389.453883371680149, 297.6663029733589951 ) ) ;
#10870 = CIRCLE ( 'NONE', #87680, 1.999999999999999556 ) ;
#10871 = CARTESIAN_POINT ( 'NONE',  ( -17.34064570863325372, 1525.506926151471362, 236.9219808115470869 ) ) ;
#10872 = CARTESIAN_POINT ( 'NONE',  ( 20.03573726229999963, 1460.150672172730083, 240.3194873227980111 ) ) ;
#10873 = EDGE_CURVE ( 'NONE', #66359, #29914, #22974, .T. ) ;
#10874 = CARTESIAN_POINT ( 'NONE',  ( 10.19356100915574714, 1482.603900002795854, 212.2173956555756149 ) ) ;
#10875 = CARTESIAN_POINT ( 'NONE',  ( 24.25895011704442084, 1512.187213306747481, 247.1119212070236131 ) ) ;
#10876 = CARTESIAN_POINT ( 'NONE',  ( -7.324858259705050223, 1509.160117843870012, 237.2583435074130023 ) ) ;
#10877 = CARTESIAN_POINT ( 'NONE',  ( -20.63308528640000006, 1455.489145095029926, 224.0314336810980080 ) ) ;
#10879 = CARTESIAN_POINT ( 'NONE',  ( 17.23552702700579786, 1409.586384505080105, 222.3856984215319983 ) ) ;
#10878 = CARTESIAN_POINT ( 'NONE',  ( -21.65063745823909258, 1411.029531829768075, 201.4006313786291855 ) ) ;
#10880 = CARTESIAN_POINT ( 'NONE',  ( 0.2646381833610000345, 1434.810047171390124, 189.9884865742980082 ) ) ;
#10881 = CARTESIAN_POINT ( 'NONE',  ( -104.8397582023220025, 1379.985347132740117, 306.4823361143110105 ) ) ;
#10882 = ORIENTED_EDGE ( 'NONE', *, *, #12497, .T. ) ;
#10883 = CARTESIAN_POINT ( 'NONE',  ( -0.01244697378919850002, 1516.939646076049939, 203.3402601539570185 ) ) ;
#10884 = CARTESIAN_POINT ( 'NONE',  ( 0.5523900547170000896, 1406.508913882830029, 269.4985896812980286 ) ) ;
#10885 = CARTESIAN_POINT ( 'NONE',  ( 27.74968890970000146, 1508.601238174130003, 207.7069383892280143 ) ) ;
#10886 = B_SPLINE_CURVE_WITH_KNOTS ( 'NONE', 5,
 ( #83929, #90670, #82824, #7231, #6116, #75556 ),
 .UNSPECIFIED., .F., .F.,
 ( 6, 6 ),
 ( -2.000000000000000000, 0.000000000000000000 ),
 .UNSPECIFIED. ) ;
#10887 = CARTESIAN_POINT ( 'NONE',  ( 44.13013282332929776, 1446.281291277249920, 270.2165820380340051 ) ) ;
#10888 = CARTESIAN_POINT ( 'NONE',  ( 5.395424494550000283, 1433.568245638130065, 154.6346167951979851 ) ) ;
#10889 = CARTESIAN_POINT ( 'NONE',  ( -19.37335128149999974, 1466.648676094589746, 213.3177732612090267 ) ) ;
#10890 = CARTESIAN_POINT ( 'NONE',  ( -36.83756290334599726, 1440.913060387389805, 254.3462983698770472 ) ) ;
#10891 = CARTESIAN_POINT ( 'NONE',  ( 36.55810202059989678, 1449.776383268349946, 136.2665498954540055 ) ) ;
#10892 = CARTESIAN_POINT ( 'NONE',  ( 0.8295539019444626572, 1450.884091712275449, 154.2427803864302405 ) ) ;
#10893 = CARTESIAN_POINT ( 'NONE',  ( 2.303292329924660375, 1449.840026814039902, 154.2474790657759911 ) ) ;
#10894 = CARTESIAN_POINT ( 'NONE',  ( 0.6849490657429989637, 1506.697984446489954, 221.5403866999990043 ) ) ;
#10895 = CARTESIAN_POINT ( 'NONE',  ( -4.324092179320000007, 1515.269353058490196, 209.1218459616989946 ) ) ;
#10896 = VECTOR ( 'NONE', #60189, 999.9999999999998863 ) ;
#10897 = EDGE_LOOP ( 'NONE', ( #99101, #24826, #21650, #92396 ) ) ;
#10898 = CARTESIAN_POINT ( 'NONE',  ( 0.4960531524660349856, 1409.436441971110071, 185.2773250395759987 ) ) ;
#10899 = FACE_OUTER_BOUND ( 'NONE', #23564, .T. ) ;
#10900 = CARTESIAN_POINT ( 'NONE',  ( 3.281448589401000149, 1466.303082592839928, 198.5677341052449947 ) ) ;
#10901 = CIRCLE ( 'NONE', #57357, 1.999999999999999556 ) ;
#10902 = CARTESIAN_POINT ( 'NONE',  ( -1.327697533569999866, 1475.746612594030012, 269.0450429478979686 ) ) ;
#10903 = CYLINDRICAL_SURFACE ( 'NONE', #83680, 2.000000000000003553 ) ;
#10904 = CARTESIAN_POINT ( 'NONE',  ( -4.414895773965000103, 1511.801704408389924, 205.7066075212470082 ) ) ;
#10905 = CARTESIAN_POINT ( 'NONE',  ( -3.779110701619425861, 1448.294363581284188, 185.0060619559291695 ) ) ;
#10906 = CARTESIAN_POINT ( 'NONE',  ( -20.11165657711670107, 1384.861962272929986, 220.9937321937230195 ) ) ;
#10907 = CARTESIAN_POINT ( 'NONE',  ( -18.90690566160000330, 1416.819756528429934, 208.2173862770389690 ) ) ;
#10908 = DIRECTION ( 'NONE',  ( -0.7063774289747313251, 0.04540766091858282338, 0.7063774289747313251 ) ) ;
#10909 = CARTESIAN_POINT ( 'NONE',  ( 26.41104128045460087, 1435.419835122459972, 135.2945573537490134 ) ) ;
#10910 = CARTESIAN_POINT ( 'NONE',  ( -11.05338566285159807, 1396.299053120159897, 208.4942113865890292 ) ) ;
#10911 = AXIS2_PLACEMENT_3D ( 'NONE', #68341, #59935, #110308 ) ;
#10912 = CARTESIAN_POINT ( 'NONE',  ( -15.20078488979999953, 1421.481067149630007, 227.2882089291979923 ) ) ;
#10913 = CARTESIAN_POINT ( 'NONE',  ( -16.59151158838270135, 1409.592917334169897, 225.4533943397379971 ) ) ;
#10914 = CARTESIAN_POINT ( 'NONE',  ( -5.832233384169380308, 1490.191062745069985, 214.8994725848050109 ) ) ;
#10915 = ORIENTED_EDGE ( 'NONE', *, *, #31975, .T. ) ;
#10916 = CARTESIAN_POINT ( 'NONE',  ( -11.41143408916500412, 1500.995514667651150, 208.5044259995214588 ) ) ;
#10917 = CARTESIAN_POINT ( 'NONE',  ( 1.984522837200000112, 1409.916377421130164, 231.9929760013979774 ) ) ;
#10918 = CARTESIAN_POINT ( 'NONE',  ( -8.190304664959999315, 1512.060957492389889, 212.0841603871389793 ) ) ;
#10920 = CARTESIAN_POINT ( 'NONE',  ( -22.08622291482313926, 1523.382868172864164, 233.8253038720786776 ) ) ;
#10919 = CARTESIAN_POINT ( 'NONE',  ( 10.22494416990000055, 1425.155393777929930, 108.0534255276979962 ) ) ;
#10921 = CARTESIAN_POINT ( 'NONE',  ( -1.906499846882070084E-08, 1516.051704408390151, 209.1218459511669892 ) ) ;
#10922 = CARTESIAN_POINT ( 'NONE',  ( -8.154782393420001441, 1452.666828378989749, 204.3290871732590119 ) ) ;
#10923 = CARTESIAN_POINT ( 'NONE',  ( -6.942344729965000738, 1516.810037859429940, 201.4055938791270250 ) ) ;
#10924 = CARTESIAN_POINT ( 'NONE',  ( 7.528870192820000362, 1425.840869188159786, 212.2336632603989983 ) ) ;
#10925 = CARTESIAN_POINT ( 'NONE',  ( -16.53114558859999761, 1465.611456236089907, 220.7423132190989747 ) ) ;
#10926 = FACE_BOUND ( 'NONE', #14362, .T. ) ;
#10927 = CARTESIAN_POINT ( 'NONE',  ( -7.271052316819549333, 1517.051704408389924, 225.3404165491008371 ) ) ;
#10928 = CARTESIAN_POINT ( 'NONE',  ( -109.5441724309999927, 1377.044192470269991, 306.8927967050020129 ) ) ;
#10929 = CARTESIAN_POINT ( 'NONE',  ( 8.716989280790679473, 1365.703354663701930, 207.6218459616988241 ) ) ;
#10931 = VERTEX_POINT ( 'NONE', #24974 ) ;
#10930 = CARTESIAN_POINT ( 'NONE',  ( 6.261024423890000357, 1453.731044942389872, 216.1357478295089720 ) ) ;
#10932 = ORIENTED_EDGE ( 'NONE', *, *, #79903, .F. ) ;
#10933 = CARTESIAN_POINT ( 'NONE',  ( -40.27309184310000489, 1443.612070458560083, 137.1163417766980217 ) ) ;
#10934 = ADVANCED_FACE ( 'NONE', ( #95517 ), #32038, .T. ) ;
#10935 = CARTESIAN_POINT ( 'NONE',  ( 0.06029893845285259901, 1482.863300304640006, 236.3492419568210039 ) ) ;
#10936 = CARTESIAN_POINT ( 'NONE',  ( 6.553899686920000356, 1408.913060387329779, 225.8798606464979741 ) ) ;
#10937 = CARTESIAN_POINT ( 'NONE',  ( 5.514426304880457153, 1499.747148894430666, 199.1702447789172652 ) ) ;
#10938 = CARTESIAN_POINT ( 'NONE',  ( -0.6009897688609999733, 1485.972025337430068, 182.1351461919979897 ) ) ;
#10940 = EDGE_CURVE ( 'NONE', #85274, #98761, #91012, .T. ) ;
#10939 = CARTESIAN_POINT ( 'NONE',  ( -31.14814740293979511, 1525.697946996596102, 201.5095778062523948 ) ) ;
#10941 = DIRECTION ( 'NONE',  ( -5.980589973904019347E-17, 1.000000000000000000, -1.736889445713099699E-16 ) ) ;
#10942 = DIRECTION ( 'NONE',  ( 0.9455185755993178454, 0.000000000000000000, -0.3255681544571537578 ) ) ;
#10943 = EDGE_CURVE ( 'NONE', #23318, #17806, #103106, .T. ) ;
#10944 = PRESENTATION_STYLE_ASSIGNMENT (( #104998 ) ) ;
#10945 = CARTESIAN_POINT ( 'NONE',  ( 35.12833357477309448, 1435.886684291350093, 135.9061531807790004 ) ) ;
#10946 = CARTESIAN_POINT ( 'NONE',  ( 32.00871303854333405, 1435.615229631456941, 135.1257567998584364 ) ) ;
#10947 = CARTESIAN_POINT ( 'NONE',  ( 8.999538239140179030, 1407.274461440940058, 198.9439808189530083 ) ) ;
#10948 = CARTESIAN_POINT ( 'NONE',  ( 5.721593877714729399E-05, 1405.775960253769881, 268.4837777154720015 ) ) ;
#10949 = CARTESIAN_POINT ( 'NONE',  ( -14.01525996361490023, 1415.677402202029953, 204.0303134510289738 ) ) ;
#10950 = ORIENTED_EDGE ( 'NONE', *, *, #863, .F. ) ;
#10951 = DIRECTION ( 'NONE',  ( -0.6147312344637360093, -0.2401348534948875013, -0.7512927269125400098 ) ) ;
#10952 = CARTESIAN_POINT ( 'NONE',  ( 12.89029109540000029, 1442.787888345740157, 187.7063189797979987 ) ) ;
#10953 = ORIENTED_EDGE ( 'NONE', *, *, #28360, .T. ) ;
#10954 = ORIENTED_EDGE ( 'NONE', *, *, #28974, .F. ) ;
#10955 = CARTESIAN_POINT ( 'NONE',  ( -3.866699731040000199, 1454.806985439190157, 200.4000761353790097 ) ) ;
#10956 = CARTESIAN_POINT ( 'NONE',  ( -7.811405798920000088, 1367.739269854440181, 207.6218459616989946 ) ) ;
#10957 = CARTESIAN_POINT ( 'NONE',  ( -1.123101616545000070, 1517.157901477309906, 214.9105372957470195 ) ) ;
#10958 = CARTESIAN_POINT ( 'NONE',  ( 2.822464090084999988, 1512.205735116489905, 216.8958673752769926 ) ) ;
#10959 = STYLED_ITEM ( 'NONE', ( #20967 ), #51910 ) ;
#10960 = VERTEX_POINT ( 'NONE', #8185 ) ;
#10961 = CARTESIAN_POINT ( 'NONE',  ( 7.868158389100000427, 1422.937290482379922, 214.1570520181289794 ) ) ;
#10962 = CARTESIAN_POINT ( 'NONE',  ( -70.57508978779999609, 1375.676061790260064, 279.4267215269589428 ) ) ;
#10963 = CARTESIAN_POINT ( 'NONE',  ( 7.752198807150000981, 1416.823872462329973, 225.7667597232980086 ) ) ;
#10964 = CARTESIAN_POINT ( 'NONE',  ( 4.610938211375000151, 1516.815231249920089, 205.0813186281270077 ) ) ;
#10965 = CARTESIAN_POINT ( 'NONE',  ( -11.76016211164009917, 1489.518188874960060, 212.3895637392580227 ) ) ;
#10966 = CARTESIAN_POINT ( 'NONE',  ( -103.7376339979999926, 1385.115701970539931, 296.9235426477590067 ) ) ;
#10967 = CARTESIAN_POINT ( 'NONE',  ( 6.942354273414999888, 1516.905946377369901, 201.4030824261969883 ) ) ;
#10968 = CARTESIAN_POINT ( 'NONE',  ( -5.984203303400000173, 1409.122033371430007, 229.9503900095979816 ) ) ;
#10970 = EDGE_LOOP ( 'NONE', ( #105669, #63673, #71568, #13766, #92751 ) ) ;
#10969 = CARTESIAN_POINT ( 'NONE',  ( -10.46909318259999999, 1447.037035936289840, 186.8418773576979959 ) ) ;
#10971 = CARTESIAN_POINT ( 'NONE',  ( -11.75869035857540013, 1519.551704408389924, 190.9442076533970010 ) ) ;
#10972 = FACE_OUTER_BOUND ( 'NONE', #25113, .T. ) ;
#10973 = CARTESIAN_POINT ( 'NONE',  ( 20.59705046560049624, 1507.771217143799959, 227.0402443945910136 ) ) ;
#10974 = CARTESIAN_POINT ( 'NONE',  ( -17.84338787571961049, 1512.187213306747481, 180.3600277896300383 ) ) ;
#10975 = CARTESIAN_POINT ( 'NONE',  ( -25.09080907949999784, 1435.392650067190061, 135.9845614618979823 ) ) ;
#10976 = AXIS2_PLACEMENT_3D ( 'NONE', #84539, #86752, #6 ) ;
#10977 = CARTESIAN_POINT ( 'NONE',  ( -1.701729858475000023, 1516.969638403840008, 212.0041719496170174 ) ) ;
#10978 = CARTESIAN_POINT ( 'NONE',  ( -67.40081635460001053, 1379.748791505480085, 277.3949072269590488 ) ) ;
#10979 = CARTESIAN_POINT ( 'NONE',  ( 0.01526382458731936030, 1507.788721570215102, 237.5012585564631706 ) ) ;
#10980 = CARTESIAN_POINT ( 'NONE',  ( 11.84876590452089928, 1426.365912190949985, 195.4914265713040038 ) ) ;
#10981 = CARTESIAN_POINT ( 'NONE',  ( 21.47298199986007816, 1411.021785953378640, 201.3753046382076377 ) ) ;
#10982 = CARTESIAN_POINT ( 'NONE',  ( -4.037051035714999792, 1516.939819969850078, 209.1350663277499962 ) ) ;
#10983 = ORIENTED_EDGE ( 'NONE', *, *, #73548, .F. ) ;
#10984 = CARTESIAN_POINT ( 'NONE',  ( 2.500000000000000000, 1439.039897141910160, 157.7230890540980113 ) ) ;
#10985 = CARTESIAN_POINT ( 'NONE',  ( -3.071779842299999785, 1420.448432582830037, 232.9517911341980039 ) ) ;
#10986 = CARTESIAN_POINT ( 'NONE',  ( -67.04611378480001349, 1384.669946114650202, 292.1828053715589704 ) ) ;
#10987 = ORIENTED_EDGE ( 'NONE', *, *, #98959, .T. ) ;
#10989 = CIRCLE ( 'NONE', #100415, 0.9999999999998898659 ) ;
#10988 = CARTESIAN_POINT ( 'NONE',  ( -8.888758267720000106, 1385.314821192629779, 218.6605176881890031 ) ) ;
#10990 = CARTESIAN_POINT ( 'NONE',  ( -113.4000000000000057, 1378.913060387289988, 304.2218459572590064 ) ) ;
#10991 = EDGE_CURVE ( 'NONE', #96609, #110603, #39049, .T. ) ;
#10992 = CARTESIAN_POINT ( 'NONE',  ( 18.44206918373069826, 1469.011769097089882, 228.2221280545410025 ) ) ;
#10993 = AXIS2_PLACEMENT_3D ( 'NONE', #54952, #79056, #89078 ) ;
#10994 = CARTESIAN_POINT ( 'NONE',  ( -24.03031496624599583, 1509.069760856670200, 222.9704818946499927 ) ) ;
#10995 = CARTESIAN_POINT ( 'NONE',  ( -0.8265242350169998975, 1408.941923249630008, 187.0792671732980068 ) ) ;
#10996 = CARTESIAN_POINT ( 'NONE',  ( 4.802229599638190294, 1508.551704408389924, 213.5516195556409969 ) ) ;
#10997 = DIRECTION ( 'NONE',  ( 0.4090087482554189968, 0.000000000000000000, -0.9125304618754023211 ) ) ;
#10999 = CARTESIAN_POINT ( 'NONE',  ( -2.566419091909999839, 1420.628703720230078, 185.8818997532980006 ) ) ;
#10998 = CARTESIAN_POINT ( 'NONE',  ( -2.870951705914999597, 1517.111322026010157, 215.6844817927369888 ) ) ;
#11000 = CARTESIAN_POINT ( 'NONE',  ( 18.65451754129999529, 1507.632629717330019, 188.5326157632979971 ) ) ;
#11001 = CARTESIAN_POINT ( 'NONE',  ( 9.922877777048348946, 1468.601600206289959, 207.7732624088289981 ) ) ;
#11002 = ORIENTED_EDGE ( 'NONE', *, *, #66601, .T. ) ;
#11003 = CARTESIAN_POINT ( 'NONE',  ( -11.57735155928969917, 1414.971513442450032, 196.9567343561169821 ) ) ;
#11004 = CARTESIAN_POINT ( 'NONE',  ( -20.06431043899999622, 1490.513422158030153, 190.0771971858980294 ) ) ;
#11005 = ORIENTED_EDGE ( 'NONE', *, *, #51793, .F. ) ;
#11006 = AXIS2_PLACEMENT_3D ( 'NONE', #65858, #74264, #82646 ) ;
#11007 = CARTESIAN_POINT ( 'NONE',  ( 2.713698362399999731, 1421.382238371229960, 183.9342778676980004 ) ) ;
#11008 = DIRECTION ( 'NONE',  ( -0.9995237703344608260, 0.03085826527909721340, -5.905782510576255506E-07 ) ) ;
#11009 = CARTESIAN_POINT ( 'NONE',  ( 7.679927584005029395, 1511.009256124219974, 203.5019279399089953 ) ) ;
#11010 = CARTESIAN_POINT ( 'NONE',  ( 2.234896868229169886, 1424.004436568589881, 191.3087619182109904 ) ) ;
#11011 = CARTESIAN_POINT ( 'NONE',  ( -26.35750891854250000, 1508.044014828989930, 201.5443954048259911 ) ) ;
#11012 = CARTESIAN_POINT ( 'NONE',  ( -21.19079385647338754, 1525.394057003702756, 234.2786681684617349 ) ) ;
#11013 = CARTESIAN_POINT ( 'NONE',  ( 18.04709463619999710, 1415.245980412329800, 210.4308792091779878 ) ) ;
#11014 = CARTESIAN_POINT ( 'NONE',  ( -17.95904881909999773, 1424.699834624730101, 227.3705041876980033 ) ) ;
#11015 = FACE_OUTER_BOUND ( 'NONE', #96976, .T. ) ;
#11016 = CARTESIAN_POINT ( 'NONE',  ( -9.862951376772540968, 1517.051704408389924, 228.3939896807019920 ) ) ;
#11017 = CARTESIAN_POINT ( 'NONE',  ( 17.39646299289999831, 1418.986622976930221, 191.8562750549980080 ) ) ;
#11019 = CARTESIAN_POINT ( 'NONE',  ( 0.5969155455355750206, 1501.813611154769887, 186.7307704303590015 ) ) ;
#11018 = CARTESIAN_POINT ( 'NONE',  ( 12.03449227190490056, 1491.353386486839781, 206.6667661091970274 ) ) ;
#11020 = CARTESIAN_POINT ( 'NONE',  ( 27.39760735127830316, 1439.876886201499929, 137.1284513264700138 ) ) ;
#11021 = ORIENTED_EDGE ( 'NONE', *, *, #56328, .T. ) ;
#11022 = CARTESIAN_POINT ( 'NONE',  ( 1.556517342736410070, 1415.020374539499926, 191.6346848232400077 ) ) ;
#11024 = ORIENTED_EDGE ( 'NONE', *, *, #5309, .F. ) ;
#11023 = CARTESIAN_POINT ( 'NONE',  ( 26.35471571933159751, 1507.985750330240080, 216.6976075425179999 ) ) ;
#11025 = EDGE_CURVE ( 'NONE', #78418, #48402, #79305, .T. ) ;
#11026 = CARTESIAN_POINT ( 'NONE',  ( -11.89516918277866964, 1433.269309810761570, 149.9552381126513865 ) ) ;
#11027 = CARTESIAN_POINT ( 'NONE',  ( -2.363461299099999913, 1483.719072616789845, 198.7034185567990221 ) ) ;
#11028 = DIRECTION ( 'NONE',  ( 1.755985294532469921E-16, -1.000000000000000000, 1.338183447452831989E-16 ) ) ;
#11029 = LINE ( 'NONE', #79339, #100043 ) ;
#11031 = B_SPLINE_CURVE_WITH_KNOTS ( 'NONE', 3,
 ( #50729, #77594, #42329, #43445, #49645, #84862, #85413, #900, #8712, #77049, #26053, #60248 ),
 .UNSPECIFIED., .F., .F.,
 ( 4, 2, 2, 2, 2, 4 ),
 ( -0.1123552056274609995, -0.09789079770775470368, -0.08345975727710699954, -0.05408602632130809357, -0.02844277166756620234, 0.000000000000000000 ),
 .UNSPECIFIED. ) ;
#11030 = CARTESIAN_POINT ( 'NONE',  ( 13.22806383200000013, 1431.113060387329824, 222.3499097933980124 ) ) ;
#11032 = AXIS2_PLACEMENT_3D ( 'NONE', #12992, #63996, #39865 ) ;
#11033 = CARTESIAN_POINT ( 'NONE',  ( 28.49879435373766157, 1526.382868172571079, 219.8425395114742855 ) ) ;
#11034 = CARTESIAN_POINT ( 'NONE',  ( -11.30600794628579919, 1470.458368520040040, 210.5249131588269904 ) ) ;
#11035 = CARTESIAN_POINT ( 'NONE',  ( -9.980182751213080294, 1489.983213112079738, 214.0086324331080050 ) ) ;
#11036 = CARTESIAN_POINT ( 'NONE',  ( 18.32584137559999959, 1473.764089050990151, 194.8973954003990059 ) ) ;
#11037 = CARTESIAN_POINT ( 'NONE',  ( -78.11014189374911609, 1383.778372959410262, 302.3262168834259569 ) ) ;
#11038 = DIRECTION ( 'NONE',  ( 0.000000000000000000, -1.000000000000000000, 0.000000000000000000 ) ) ;
#11039 = CARTESIAN_POINT ( 'NONE',  ( -15.95383389570000077, 1506.798305147730161, 224.6865364803979901 ) ) ;
#11040 = CARTESIAN_POINT ( 'NONE',  ( -2.265367662664029780, 1516.528448466100144, 201.4129675568979962 ) ) ;
#11042 = VERTEX_POINT ( 'NONE', #9311 ) ;
#11041 = CARTESIAN_POINT ( 'NONE',  ( 21.06390421310000249, 1509.318873927029927, 189.5956816894980079 ) ) ;
#11043 = CARTESIAN_POINT ( 'NONE',  ( 4.709520687179999499, 1480.407452823689937, 228.9869292435990076 ) ) ;
#11044 = CARTESIAN_POINT ( 'NONE',  ( -89.13551699850000887, 1383.359784101189916, 292.2933295549590298 ) ) ;
#11045 = FACE_OUTER_BOUND ( 'NONE', #102902, .T. ) ;
#11046 = ORIENTED_EDGE ( 'NONE', *, *, #15472, .T. ) ;
#11047 = ORIENTED_EDGE ( 'NONE', *, *, #8057, .F. ) ;
#11048 = FACE_OUTER_BOUND ( 'NONE', #60712, .T. ) ;
#11049 = CARTESIAN_POINT ( 'NONE',  ( -110.0628159060000115, 1384.912455446979948, 296.9513137223589752 ) ) ;
#11050 = CARTESIAN_POINT ( 'NONE',  ( 13.51610093809999924, 1443.913060387330006, 169.3501091259980171 ) ) ;
#11052 = CARTESIAN_POINT ( 'NONE',  ( -38.77640752969999483, 1448.325305151830207, 259.1404898689979746 ) ) ;
#11051 = CARTESIAN_POINT ( 'NONE',  ( 18.16348015480000200, 1416.820969729830040, 209.1672090666169765 ) ) ;
#11053 = CARTESIAN_POINT ( 'NONE',  ( 8.701117752674768724, 1436.141255594499853, 208.2914523929980248 ) ) ;
#11054 = CARTESIAN_POINT ( 'NONE',  ( -11.29670609480000110, 1433.873747960979927, 151.5261222975980218 ) ) ;
#11055 = VECTOR ( 'NONE', #50568, 1000.000000000000000 ) ;
#11056 = CARTESIAN_POINT ( 'NONE',  ( 2.801507340699999737, 1486.711793625290056, 216.6331940948190038 ) ) ;
#11057 = DIRECTION ( 'NONE',  ( -1.755985294532469921E-16, 1.000000000000000000, -1.338183447452831989E-16 ) ) ;
#11058 = CARTESIAN_POINT ( 'NONE',  ( 13.30361592369999890, 1409.377632892530073, 191.9462335214980158 ) ) ;
#11059 = CARTESIAN_POINT ( 'NONE',  ( 4.132091976209999906, 1421.241915956429921, 185.3693088014979935 ) ) ;
#11060 = CARTESIAN_POINT ( 'NONE',  ( -10.72974951780000019, 1437.118219917419992, 152.1700466790979931 ) ) ;
#11061 = CARTESIAN_POINT ( 'NONE',  ( 10.13504311139999992, 1439.368087371720094, 152.9209920991980027 ) ) ;
#11062 = CARTESIAN_POINT ( 'NONE',  ( -16.13494021775330367, 1420.788389406239958, 203.3274822485300035 ) ) ;
#11063 = CARTESIAN_POINT ( 'NONE',  ( 2.738357795398948635, 1525.795403383247276, 240.9366230306859222 ) ) ;
#11064 = CARTESIAN_POINT ( 'NONE',  ( 1.971095687570000088, 1464.814373034330174, 236.1963163484979873 ) ) ;
#11065 = ORIENTED_EDGE ( 'NONE', *, *, #22765, .T. ) ;
#11066 = CARTESIAN_POINT ( 'NONE',  ( -33.91369265678890343, 1437.010538859309918, 136.5611844326260211 ) ) ;
#11067 = ADVANCED_FACE ( 'NONE', ( #17113 ), #92788, .T. ) ;
#11068 = ADVANCED_FACE ( 'NONE', ( #31062 ), #15880, .F. ) ;
#11069 = CARTESIAN_POINT ( 'NONE',  ( -21.26809730078759841, 1485.919095653640170, 201.7808411774039996 ) ) ;
#11070 = CARTESIAN_POINT ( 'NONE',  ( -37.36936258469999927, 1456.002134664930054, 270.0098740415979819 ) ) ;
#11071 = DIRECTION ( 'NONE',  ( -4.648609652910299899E-17, -1.000000000000000000, 2.252106476759999926E-16 ) ) ;
#11072 = CARTESIAN_POINT ( 'NONE',  ( 8.437694987149998527E-15, 1442.756953654919926, 155.7628527808980152 ) ) ;
#11073 = EDGE_CURVE ( 'NONE', #23627, #77339, #69114, .T. ) ;
#11074 = CARTESIAN_POINT ( 'NONE',  ( -5.923682464646780943, 1517.151704408390060, 223.8623791742500089 ) ) ;
#11075 = VECTOR ( 'NONE', #47652, 1000.000000000000000 ) ;
#11077 = EDGE_CURVE ( 'NONE', #24499, #53518, #108932, .T. ) ;
#11076 = CARTESIAN_POINT ( 'NONE',  ( 4.963802804109999300, 1497.713060387329961, 187.3310108713980071 ) ) ;
#11078 = CARTESIAN_POINT ( 'NONE',  ( 2.838492387013249907, 1409.123886199480012, 230.7524214366010256 ) ) ;
#11079 = CARTESIAN_POINT ( 'NONE',  ( 1.205197961869999945, 1507.636020686930124, 237.0931865834980101 ) ) ;
#11080 = CARTESIAN_POINT ( 'NONE',  ( -12.47269130070000109, 1419.287450240530006, 228.5775552544979803 ) ) ;
#11081 = ADVANCED_FACE ( 'NONE', ( #15691 ), #109781, .T. ) ;
#11082 = CARTESIAN_POINT ( 'NONE',  ( -8.372769162319999126, 1460.069700419990113, 216.1743697456390123 ) ) ;
#11083 = CARTESIAN_POINT ( 'NONE',  ( 9.663424421700000266, 1363.752474719049815, 207.6218459616989946 ) ) ;
#11084 = CARTESIAN_POINT ( 'NONE',  ( -44.65796480198309837, 1433.806179381780112, 269.0022936558889910 ) ) ;
#11085 = MANIFOLD_SOLID_BREP ( 'Stock-MAS-682-1', #43092 ) ;
#11086 = DIRECTION ( 'NONE',  ( -1.755985294532469921E-16, 1.000000000000000000, -1.338183447452831989E-16 ) ) ;
#11087 = ORIENTED_EDGE ( 'NONE', *, *, #2998, .F. ) ;
#11088 = CARTESIAN_POINT ( 'NONE',  ( -9.241005602170000444, 1423.079004508810158, 209.8534315543390107 ) ) ;
#11089 = EDGE_CURVE ( 'NONE', #17927, #75668, #5774, .T. ) ;
#11090 = ORIENTED_EDGE ( 'NONE', *, *, #108679, .T. ) ;
#11091 = CARTESIAN_POINT ( 'NONE',  ( 0.7533003524100010395, 1516.992029636990083, 209.8620668306199946 ) ) ;
#11092 = CARTESIAN_POINT ( 'NONE',  ( -11.66658784013729999, 1391.913060387289988, 209.7120188154370339 ) ) ;
#11093 = CARTESIAN_POINT ( 'NONE',  ( 17.56004567126451477, 1410.529979399466811, 224.8086585292313373 ) ) ;
#11094 = CARTESIAN_POINT ( 'NONE',  ( -12.30019964340000094, 1410.398530115529866, 189.3840444957980083 ) ) ;
#11095 = AXIS2_PLACEMENT_3D ( 'NONE', #75738, #33162, #91434 ) ;
#11096 = B_SPLINE_CURVE_WITH_KNOTS ( 'NONE', 3,
 ( #86803, #69483, #87366, #54877, #36398, #95209, #61626, #18470, #80057, #77858 ),
 .UNSPECIFIED., .F., .F.,
 ( 4, 2, 2, 2, 4 ),
 ( 0.000000000000000000, 0.0007403986298595332041, 0.001480797259719066408, 0.002221195889578599612, 0.002961594519438132816 ),
 .UNSPECIFIED. ) ;
#11097 = CARTESIAN_POINT ( 'NONE',  ( -27.02719243892629919, 1451.200357981530033, 136.2769546900069884 ) ) ;
#11098 = VERTEX_POINT ( 'NONE', #36370 ) ;
#11099 = DIRECTION ( 'NONE',  ( -0.6736849260863841948, 0.000000000000000000, 0.7390186874254148774 ) ) ;
#11101 = CARTESIAN_POINT ( 'NONE',  ( -28.72841836130733739, 1526.333389947941669, 198.1146668274939202 ) ) ;
#11100 = CYLINDRICAL_SURFACE ( 'NONE', #96162, 1.000000000000003775 ) ;
#11102 = EDGE_CURVE ( 'NONE', #43690, #1895, #40459, .T. ) ;
#11103 = AXIS2_PLACEMENT_3D ( 'NONE', #56938, #47433, #98369 ) ;
#11104 = CARTESIAN_POINT ( 'NONE',  ( 11.60004869885203682, 1423.972955187191246, 135.9380529689869661 ) ) ;
#11105 = CARTESIAN_POINT ( 'NONE',  ( -17.20083043329730188, 1508.455239297279832, 213.0365388520800138 ) ) ;
#11106 = CARTESIAN_POINT ( 'NONE',  ( 6.734691585760000265, 1471.477077836790158, 216.7572454896890122 ) ) ;
#11107 = EDGE_CURVE ( 'NONE', #37652, #51148, #80323, .T. ) ;
#11108 = CARTESIAN_POINT ( 'NONE',  ( 5.511665417999469900E-05, 1508.970066526555001, 238.8757070596369942 ) ) ;
#11109 = ORIENTED_EDGE ( 'NONE', *, *, #33043, .T. ) ;
#11110 = CARTESIAN_POINT ( 'NONE',  ( -22.40264917047960225, 1414.570795220049831, 269.9085733495129489 ) ) ;
#11111 = CARTESIAN_POINT ( 'NONE',  ( 2.284053471355000031, 1516.854133554269993, 207.9850318982369970 ) ) ;
#11112 = CARTESIAN_POINT ( 'NONE',  ( 20.49599333844873783, 1525.960063244516959, 233.8638087104922931 ) ) ;
#11113 = CARTESIAN_POINT ( 'NONE',  ( 9.102815358048328420, 1434.837644414159968, 206.9573682008849858 ) ) ;
#11115 = ORIENTED_EDGE ( 'NONE', *, *, #46758, .T. ) ;
#11114 = CARTESIAN_POINT ( 'NONE',  ( -7.484392838114925617, 1365.703112302720456, 208.3718459617061285 ) ) ;
#11116 = VERTEX_POINT ( 'NONE', #88437 ) ;
#11117 = ADVANCED_FACE ( 'NONE', ( #96284 ), #94096, .T. ) ;
#11118 = CARTESIAN_POINT ( 'NONE',  ( 42.90684747031818347, 1452.569395717577436, 269.0510755419506950 ) ) ;
#11119 = CARTESIAN_POINT ( 'NONE',  ( 2.015156349838810090, 1466.892420976849962, 219.9987159044960094 ) ) ;
#11120 = FACE_OUTER_BOUND ( 'NONE', #42461, .T. ) ;
#11121 = CARTESIAN_POINT ( 'NONE',  ( -0.03180497178026089888, 1409.232592949579839, 185.5579152414480291 ) ) ;
#11122 = EDGE_CURVE ( 'NONE', #72755, #61631, #108424, .T. ) ;
#11123 = CARTESIAN_POINT ( 'NONE',  ( -18.73709653282620025, 1416.134159090969888, 207.5726623008649767 ) ) ;
#11124 = CARTESIAN_POINT ( 'NONE',  ( -18.80193033609999986, 1425.815728067429973, 224.6524251216980019 ) ) ;
#11125 = CARTESIAN_POINT ( 'NONE',  ( 5.345145192925599531, 1476.109332684420224, 267.8539259984499949 ) ) ;
#11126 = CARTESIAN_POINT ( 'NONE',  ( -11.32491995773190041, 1391.913060387279984, 206.9750921995710087 ) ) ;
#11127 = CARTESIAN_POINT ( 'NONE',  ( 5.514569887500000434, 1447.126989177859969, 184.6235071523979911 ) ) ;
#11128 = CARTESIAN_POINT ( 'NONE',  ( -7.338411997524999286, 1517.170512887980067, 206.6372682748769876 ) ) ;
#11129 = ORIENTED_EDGE ( 'NONE', *, *, #81853, .T. ) ;
#11130 = CARTESIAN_POINT ( 'NONE',  ( 23.96131741799887394, 1411.110629221238696, 210.1578133893788447 ) ) ;
#11131 = CARTESIAN_POINT ( 'NONE',  ( 1.491499242636469935, 1470.574770574250124, 182.7072383254629813 ) ) ;
#11132 = ORIENTED_EDGE ( 'NONE', *, *, #70737, .T. ) ;
#11133 = CARTESIAN_POINT ( 'NONE',  ( 4.038582018736556201, 1515.598601288561440, 208.8110691765281217 ) ) ;
#11134 = CARTESIAN_POINT ( 'NONE',  ( 24.82914352958970028, 1452.046038066890105, 135.7260749457049940 ) ) ;
#11135 = CARTESIAN_POINT ( 'NONE',  ( -22.98253258309999936, 1410.218983115129959, 210.7724375874179827 ) ) ;
#11136 = CARTESIAN_POINT ( 'NONE',  ( -19.72061575229999875, 1388.557148333510213, 219.1405698173590224 ) ) ;
#11137 = CARTESIAN_POINT ( 'NONE',  ( -18.68654022863783126, 1509.565608751230002, 231.3997216384849480 ) ) ;
#11138 = CARTESIAN_POINT ( 'NONE',  ( 18.88590846800000023, 1410.068559083629907, 195.4829271619979920 ) ) ;
#11139 = CARTESIAN_POINT ( 'NONE',  ( 22.60520531310000081, 1410.200391392630081, 207.0451948584779984 ) ) ;
#11140 = CARTESIAN_POINT ( 'NONE',  ( 17.59268502629999631, 1410.455475180429858, 224.8086594958979845 ) ) ;
#11142 = CARTESIAN_POINT ( 'NONE',  ( -22.81609663431766322, 1432.397462965666591, 215.5375287057428864 ) ) ;
#11141 = CARTESIAN_POINT ( 'NONE',  ( 1.853755023460000206, 1417.534146448229876, 234.9926947069979803 ) ) ;
#11143 = DIRECTION ( 'NONE',  ( 0.000000000000000000, 0.000000000000000000, 1.000000000000000000 ) ) ;
#11144 = CARTESIAN_POINT ( 'NONE',  ( -8.129796171130001525, 1383.479577432089854, 218.6364202077689924 ) ) ;
#11145 = CARTESIAN_POINT ( 'NONE',  ( -2.289624470354999719, 1517.154223579619838, 215.6854418399169901 ) ) ;
#11146 = CARTESIAN_POINT ( 'NONE',  ( 2.708826876439114795, 1524.477587234266139, 241.9484498748172143 ) ) ;
#11147 = ORIENTED_EDGE ( 'NONE', *, *, #101594, .T. ) ;
#11148 = CARTESIAN_POINT ( 'NONE',  ( -11.03307619032269926, 1509.369276855707540, 181.1467085314911571 ) ) ;
#11149 = CARTESIAN_POINT ( 'NONE',  ( 21.61625474793598300, 1526.178928173327677, 234.4801574852378394 ) ) ;
#11150 = CARTESIAN_POINT ( 'NONE',  ( -0.4197533444684409809, 1409.214796873330215, 232.6058533239929886 ) ) ;
#11151 = ADVANCED_FACE ( 'NONE', ( #18994 ), #6512, .T. ) ;
#11152 = CARTESIAN_POINT ( 'NONE',  ( 4.277761459085749784, 1517.051704409989952, 201.7957048000489806 ) ) ;
#11153 = EDGE_CURVE ( 'NONE', #34173, #67299, #90728, .T. ) ;
#11154 =( BOUNDED_SURFACE ( )  B_SPLINE_SURFACE ( 3, 2, ( 
 ( #58782, #8909, #92920 ),
 ( #16192, #43086, #84522 ),
 ( #41978, #85062, #110270 ),
 ( #8354, #76676, #34119 ) ),
 .UNSPECIFIED., .F., .F., .F. ) 
 B_SPLINE_SURFACE_WITH_KNOTS ( ( 4, 4 ),
 ( 3, 3 ),
 ( 0.000000000000000000, 0.0002960034161023851105 ),
 ( 0.000000000000000000, 1.000000000000000000 ),
 .UNSPECIFIED. ) 
 GEOMETRIC_REPRESENTATION_ITEM ( )  RATIONAL_B_SPLINE_SURFACE ( (
 ( 1.000000000000000000, 0.8070209408750074198, 1.000000000000000000),
 ( 1.000000000000000000, 0.8071723757218278728, 1.000000000000000000),
 ( 1.000000000000000000, 0.8072480346917794147, 1.000000000000000000),
 ( 1.000000000000000000, 0.8072480644198116728, 1.000000000000000000) ) ) 
 REPRESENTATION_ITEM ( '' )  SURFACE ( )  );
#11155 = CARTESIAN_POINT ( 'NONE',  ( -36.91771901113230570, 1449.587085128020135, 136.2865250079899795 ) ) ;
#11156 = CARTESIAN_POINT ( 'NONE',  ( -4.329338606958669011, 1515.069000070069933, 207.5005477031000112 ) ) ;
#11157 = AXIS2_PLACEMENT_3D ( 'NONE', #15535, #41323, #23402 ) ;
#11158 = CARTESIAN_POINT ( 'NONE',  ( -9.562842729590000701, 1454.397736416729913, 219.6133831120980062 ) ) ;
#11159 = CARTESIAN_POINT ( 'NONE',  ( -2.151425146572340186, 1458.408547725810195, 184.2393776212050227 ) ) ;
#11160 = CARTESIAN_POINT ( 'NONE',  ( 11.85372112360000152, 1433.007143084950030, 150.3176596395979914 ) ) ;
#11161 = CARTESIAN_POINT ( 'NONE',  ( -10.02643927592029982, 1473.539698929279893, 270.1204779540980212 ) ) ;
#11162 = CARTESIAN_POINT ( 'NONE',  ( -10.76604721355800010, 1461.751042529569986, 211.3391729738050060 ) ) ;
#11163 = CARTESIAN_POINT ( 'NONE',  ( -109.1565231619999992, 1385.185641183290045, 297.1420090250589965 ) ) ;
#11164 = CARTESIAN_POINT ( 'NONE',  ( 14.09839856069999975, 1429.347419047090170, 194.9681440372989982 ) ) ;
#11165 = ORIENTED_EDGE ( 'NONE', *, *, #26080, .F. ) ;
#11166 = CARTESIAN_POINT ( 'NONE',  ( -105.5686647185313376, 1391.210135304358346, 305.6570493640687118 ) ) ;
#11167 = CARTESIAN_POINT ( 'NONE',  ( 9.797638205384430421, 1462.858754388850002, 211.9411891193020097 ) ) ;
#11168 = EDGE_CURVE ( 'NONE', #84761, #83948, #9721, .T. ) ;
#11169 = CARTESIAN_POINT ( 'NONE',  ( -5.863845177379999996, 1486.251790869430124, 182.2701570709980103 ) ) ;
#11170 = CARTESIAN_POINT ( 'NONE',  ( 6.114550669599164046, 1398.094264554022629, 197.6339483949746523 ) ) ;
#11171 = CARTESIAN_POINT ( 'NONE',  ( 12.35389624737000069, 1501.312344378229909, 211.6968100630580238 ) ) ;
#11172 = VECTOR ( 'NONE', #86312, 1000.000000000000227 ) ;
#11173 = CARTESIAN_POINT ( 'NONE',  ( 26.05067190899999829, 1469.243640230129813, 211.9776772231579969 ) ) ;
#11174 = CARTESIAN_POINT ( 'NONE',  ( -4.227540919128129460, 1441.218328383909920, 201.3833897788859986 ) ) ;
#11175 = CARTESIAN_POINT ( 'NONE',  ( -18.11157307520000259, 1509.545530455829976, 231.7129770453979916 ) ) ;
#11176 = CARTESIAN_POINT ( 'NONE',  ( -22.08626087506250002, 1383.851343771249958, 221.7312892301039824 ) ) ;
#11177 = CARTESIAN_POINT ( 'NONE',  ( -4.240941581556870510, 1509.032042628840145, 205.3774810555430008 ) ) ;
#11178 = CARTESIAN_POINT ( 'NONE',  ( 9.630115647840000292, 1408.206715791229954, 218.8876307819480189 ) ) ;
#11179 = CARTESIAN_POINT ( 'NONE',  ( -1970.025574498409924, -8382.262153571269664, 5.165967170900809258 ) ) ;
#11180 = CARTESIAN_POINT ( 'NONE',  ( 0.1641804351734459932, 1483.764984357220101, 181.9326469513949860 ) ) ;
#11182 = ORIENTED_EDGE ( 'NONE', *, *, #106394, .F. ) ;
#11181 = CARTESIAN_POINT ( 'NONE',  ( 3.962702341850000032, 1441.289781348989891, 217.4194346338989874 ) ) ;
#11183 = CARTESIAN_POINT ( 'NONE',  ( -28.84486411959998975, 1445.052233488288948, 176.6843673542979332 ) ) ;
#11184 = EDGE_CURVE ( 'NONE', #81034, #76431, #2952, .T. ) ;
#11185 = CARTESIAN_POINT ( 'NONE',  ( -8.201645939166466448, 1386.531733650833758, 199.7449378919872913 ) ) ;
#11187 = ORIENTED_EDGE ( 'NONE', *, *, #40476, .T. ) ;
#11186 = CARTESIAN_POINT ( 'NONE',  ( -34.05830400111539547, 1451.723718204009856, 134.0999999980979851 ) ) ;
#11188 = CARTESIAN_POINT ( 'NONE',  ( -2.176911324350150334, 1508.551704408389924, 220.0615420812520142 ) ) ;
#11189 = EDGE_LOOP ( 'NONE', ( #65754, #53779 ) ) ;
#11190 = CARTESIAN_POINT ( 'NONE',  ( -14.39625711568469946, 1380.260135093950112, 209.3432647037969900 ) ) ;
#11191 = CARTESIAN_POINT ( 'NONE',  ( -10.03264644813917705, 1391.913060248523607, 214.9446882421459861 ) ) ;
#11192 = EDGE_CURVE ( 'NONE', #46100, #107968, #15043, .T. ) ;
#11193 = CARTESIAN_POINT ( 'NONE',  ( -11.60004869885203682, 1426.786830457828273, 134.3786150874268799 ) ) ;
#11194 = CARTESIAN_POINT ( 'NONE',  ( 1.245014951509999968, 1431.187215948689982, 218.1259614198890233 ) ) ;
#11195 = CARTESIAN_POINT ( 'NONE',  ( 1.842963446620166756, 1515.320037063702557, 213.3925623524362720 ) ) ;
#11196 = CARTESIAN_POINT ( 'NONE',  ( 13.63037056512779976, 1409.389043413630134, 215.2370763268489782 ) ) ;
#11197 = CARTESIAN_POINT ( 'NONE',  ( 15.69667967640000050, 1457.921467858090182, 221.7535892932990009 ) ) ;
#11198 = CARTESIAN_POINT ( 'NONE',  ( -102.6473507896519948, 1385.227429346269901, 296.6858408320929925 ) ) ;
#11199 = CARTESIAN_POINT ( 'NONE',  ( -17.91710591500000049, 1430.610093325130038, 191.6993286258980049 ) ) ;
#11200 = CARTESIAN_POINT ( 'NONE',  ( -3.448830483803564828, 1518.913060387330006, 243.0842028158767789 ) ) ;
#11201 = CARTESIAN_POINT ( 'NONE',  ( 10.97216364479129780, 1490.548997753850244, 208.6390587469809930 ) ) ;
#11203 = ORIENTED_EDGE ( 'NONE', *, *, #42023, .T. ) ;
#11202 = CARTESIAN_POINT ( 'NONE',  ( -2.603171510209300266, 1438.442375251419890, 227.5216627168830144 ) ) ;
#11204 = ORIENTED_EDGE ( 'NONE', *, *, #104329, .F. ) ;
#11205 = EDGE_CURVE ( 'NONE', #61557, #98535, #69125, .T. ) ;
#11206 = CARTESIAN_POINT ( 'NONE',  ( -11.82816149695419838, 1415.492117401590122, 195.0961401479450217 ) ) ;
#11207 = CARTESIAN_POINT ( 'NONE',  ( 3.005276066430000448, 1369.205039411269809, 207.6218459616989946 ) ) ;
#11208 = EDGE_CURVE ( 'NONE', #93671, #66885, #57056, .T. ) ;
#11209 = CARTESIAN_POINT ( 'NONE',  ( 30.32292150136714071, 1462.007245838464087, 269.4743000939319018 ) ) ;
#11210 = CARTESIAN_POINT ( 'NONE',  ( -31.03088476499755899, 1523.982201850120191, 221.8691499995721870 ) ) ;
#11211 = CARTESIAN_POINT ( 'NONE',  ( 1.248675305699999960, 1397.026872654030058, 221.9424282998979834 ) ) ;
#11212 = CARTESIAN_POINT ( 'NONE',  ( 32.00451504911072931, 1524.843416604514232, 202.1266007667272788 ) ) ;
#11213 = CARTESIAN_POINT ( 'NONE',  ( 18.34590456075850184, 1416.851343895820037, 209.3831232368769975 ) ) ;
#11214 = CARTESIAN_POINT ( 'NONE',  ( 0.1921617888820000009, 1467.451472553630083, 182.6332811564979863 ) ) ;
#11215 = CARTESIAN_POINT ( 'NONE',  ( -11.26659152488946525, 1367.047083354208553, 208.3718459617010978 ) ) ;
#11216 = CARTESIAN_POINT ( 'NONE',  ( -19.52793969879499869, 1443.814312415009908, 208.8557621776470228 ) ) ;
#11217 = EDGE_CURVE ( 'NONE', #44333, #50492, #100541, .T. ) ;
#11218 = B_SPLINE_CURVE_WITH_KNOTS ( 'NONE', 3,
 ( #26367, #19622, #60563, #94682, #17955, #74335, #83259, #31745, #73779, #23341, #71739, #41260, #6554 ),
 .UNSPECIFIED., .F., .F.,
 ( 4, 3, 3, 3, 4 ),
 ( 12.29943287511600047, 12.57667482080269927, 12.78275953180000002, 13.14531714606529889, 13.22332100184470072 ),
 .UNSPECIFIED. ) ;
#11219 = CARTESIAN_POINT ( 'NONE',  ( 7.321193707744999557, 1516.534976163889951, 206.8301696586770220 ) ) ;
#11220 = CARTESIAN_POINT ( 'NONE',  ( -12.92312651603950080, 1435.712930329199935, 150.6986646158220253 ) ) ;
#11221 = CARTESIAN_POINT ( 'NONE',  ( 0.9041354861050000524, 1416.839648759230158, 190.2140800323980159 ) ) ;
#11222 = CARTESIAN_POINT ( 'NONE',  ( 22.08523692261567817, 1523.530935881284904, 233.8225055907668377 ) ) ;
#11223 = CARTESIAN_POINT ( 'NONE',  ( 12.20279393231724363, 1516.551704399888649, 226.2743875082219347 ) ) ;
#11224 = EDGE_CURVE ( 'NONE', #36047, #86670, #46999, .T. ) ;
#11225 = EDGE_CURVE ( 'NONE', #642, #5707, #71494, .T. ) ;
#11226 = CARTESIAN_POINT ( 'NONE',  ( 41.51802785006640306, 1444.090987553060131, 136.2824697322219833 ) ) ;
#11227 = ORIENTED_EDGE ( 'NONE', *, *, #98140, .F. ) ;
#11228 = CARTESIAN_POINT ( 'NONE',  ( 44.59183228759999906, 1432.587449243339961, 266.2372568909979691 ) ) ;
#11229 = CARTESIAN_POINT ( 'NONE',  ( -25.96988284309999884, 1469.243118074230097, 205.9471369671879870 ) ) ;
#11231 = CARTESIAN_POINT ( 'NONE',  ( 13.53550618839999942, 1416.067629290630066, 196.4934937118979974 ) ) ;
#11230 = CARTESIAN_POINT ( 'NONE',  ( -9.958863145267260464, 1425.240638064680070, 91.95675206801159618 ) ) ;
#11232 = CARTESIAN_POINT ( 'NONE',  ( 5.012317068235000228, 1517.020727862619879, 211.9902797687369969 ) ) ;
#11233 = FACE_OUTER_BOUND ( 'NONE', #12076, .T. ) ;
#11234 = CARTESIAN_POINT ( 'NONE',  ( -22.11712025940000004, 1419.857860618830045, 248.4077083964980091 ) ) ;
#11235 = CARTESIAN_POINT ( 'NONE',  ( 2.713049553179999851, 1486.854776021489897, 219.6015362787990171 ) ) ;
#11236 = CARTESIAN_POINT ( 'NONE',  ( 44.93136303390000563, 1440.913033067569813, 269.6838066906980202 ) ) ;
#11237 = CARTESIAN_POINT ( 'NONE',  ( -5.445054425793269814, 1494.866999379700246, 198.0707246423999948 ) ) ;
#11238 = CARTESIAN_POINT ( 'NONE',  ( 32.73687873290000283, 1450.481804922550054, 136.2800402082980042 ) ) ;
#11239 = EDGE_LOOP ( 'NONE', ( #34490, #27448, #16640, #89742 ) ) ;
#11240 = CARTESIAN_POINT ( 'NONE',  ( 11.59635154200000251, 1493.084219504590010, 213.4865999382489861 ) ) ;
#11241 = DIRECTION ( 'NONE',  ( -5.980589973904019347E-17, 1.000000000000000000, -1.736889445713099699E-16 ) ) ;
#11242 = EDGE_CURVE ( 'NONE', #99690, #97372, #64907, .T. ) ;
#11243 = CARTESIAN_POINT ( 'NONE',  ( 8.749060160640000916, 1509.218584300429939, 237.3209794345979731 ) ) ;
#11244 = ORIENTED_EDGE ( 'NONE', *, *, #359, .T. ) ;
#11245 = ORIENTED_EDGE ( 'NONE', *, *, #7783, .T. ) ;
#11246 = CARTESIAN_POINT ( 'NONE',  ( 10.33893311465990017, 1453.276181934919805, 211.5205973212629829 ) ) ;
#11247 = CARTESIAN_POINT ( 'NONE',  ( -24.08061883806700010, 1410.858032682979911, 208.7043793227939830 ) ) ;
#11248 = ORIENTED_EDGE ( 'NONE', *, *, #84962, .T. ) ;
#11249 = CARTESIAN_POINT ( 'NONE',  ( 0.2236527445229999911, 1424.317476911029871, 227.5167485599979784 ) ) ;
#11250 = CARTESIAN_POINT ( 'NONE',  ( 19.63722818192610120, 1517.151704408390060, 218.2362632616380154 ) ) ;
#11251 = EDGE_CURVE ( 'NONE', #8432, #2864, #72211, .T. ) ;
#11252 = CARTESIAN_POINT ( 'NONE',  ( -11.98374141780000102, 1442.037920581979961, 187.4992083556979878 ) ) ;
#11253 = CARTESIAN_POINT ( 'NONE',  ( -2.550769027769999919, 1470.484038555629922, 235.3001169919980100 ) ) ;
#11254 = CARTESIAN_POINT ( 'NONE',  ( 0.2538829723067779764, 1420.503732877419907, 182.7635795570130028 ) ) ;
#11255 = ORIENTED_EDGE ( 'NONE', *, *, #17225, .T. ) ;
#11256 = CARTESIAN_POINT ( 'NONE',  ( 45.84258480992210139, 1442.785980012289883, 266.4134452310810275 ) ) ;
#11257 = CARTESIAN_POINT ( 'NONE',  ( 6.430565326490000011, 1462.522017996690010, 207.8657408012490180 ) ) ;
#11258 = CARTESIAN_POINT ( 'NONE',  ( -109.1645132478509908, 1384.901512804259937, 297.1326343494729940 ) ) ;
#11259 = VERTEX_POINT ( 'NONE', #21744 ) ;
#11260 = CARTESIAN_POINT ( 'NONE',  ( 0.7369041709050019318, 1517.080322339569875, 204.1102945640870132 ) ) ;
#11261 = ORIENTED_EDGE ( 'NONE', *, *, #72032, .F. ) ;
#11262 = CARTESIAN_POINT ( 'NONE',  ( 11.86387080397740057, 1432.180192431070054, 149.9801236115920062 ) ) ;
#11263 = CARTESIAN_POINT ( 'NONE',  ( 13.16682460439568381, 1444.741529113969136, 187.2442499540229903 ) ) ;
#11264 = ORIENTED_EDGE ( 'NONE', *, *, #34941, .F. ) ;
#11265 = CARTESIAN_POINT ( 'NONE',  ( -1.438891081339280120, 1452.191228260170192, 183.8587004481619829 ) ) ;
#11266 = CARTESIAN_POINT ( 'NONE',  ( -5.996344191627310138, 1508.294791148050081, 220.1442991035219734 ) ) ;
#11267 = CARTESIAN_POINT ( 'NONE',  ( 7.116648072490000310, 1508.988559591530020, 236.4115320528979964 ) ) ;
#11268 = CARTESIAN_POINT ( 'NONE',  ( -6.984424792645270053, 1470.560553081000307, 216.4904170223669837 ) ) ;
#11269 = DIRECTION ( 'NONE',  ( 0.7071067811865474617, -6.092092863024105611E-16, -0.7071067811865474617 ) ) ;
#11270 = CARTESIAN_POINT ( 'NONE',  ( 0.9761199062051429953, 1408.566078314740025, 270.4290152450159894 ) ) ;
#11271 = CARTESIAN_POINT ( 'NONE',  ( 32.38845791999500534, 1523.456872492435195, 216.1254071228445355 ) ) ;
#11272 = CARTESIAN_POINT ( 'NONE',  ( 0.4151546846821903003, 1522.382868172863937, 173.3106345060153046 ) ) ;
#11273 = CARTESIAN_POINT ( 'NONE',  ( -2.225173971327330413, 1421.719837958959943, 193.4847570808190085 ) ) ;
#11274 = CARTESIAN_POINT ( 'NONE',  ( -30.32475187390000215, 1379.724315040820102, 214.4187306602189835 ) ) ;
#11275 = CARTESIAN_POINT ( 'NONE',  ( 0.02963793501150268836, 1410.197113369034241, 233.2142573394254157 ) ) ;
#11277 = CARTESIAN_POINT ( 'NONE',  ( 14.91819045380000119, 1434.994518313960043, 196.0939301745980003 ) ) ;
#11276 = CARTESIAN_POINT ( 'NONE',  ( -17.70278889250000276, 1504.268309054989913, 209.3612281098589847 ) ) ;
#11278 = FACE_OUTER_BOUND ( 'NONE', #35621, .T. ) ;
#11279 = CYLINDRICAL_SURFACE ( 'NONE', #38985, 2.000000000000003553 ) ;
#11280 = CARTESIAN_POINT ( 'NONE',  ( -6.338109935804999928, 1511.735270473989885, 201.5240551590069913 ) ) ;
#11281 = ORIENTED_EDGE ( 'NONE', *, *, #95346, .T. ) ;
#11282 = CARTESIAN_POINT ( 'NONE',  ( 3.444929437869999500, 1424.916853932230197, 224.8635561661979807 ) ) ;
#11283 = CARTESIAN_POINT ( 'NONE',  ( 3.138931148605959913E-16, 1391.413060387289988, 209.1218459616989946 ) ) ;
#11284 = CARTESIAN_POINT ( 'NONE',  ( -64.65699941863819333, 1385.044778570139897, 288.2599696774469749 ) ) ;
#11285 = DIRECTION ( 'NONE',  ( 0.000000000000000000, 0.000000000000000000, 1.000000000000000000 ) ) ;
#11286 = CARTESIAN_POINT ( 'NONE',  ( -15.60316731140000002, 1415.677402317759970, 209.6305779890419956 ) ) ;
#11288 = ORIENTED_EDGE ( 'NONE', *, *, #54848, .F. ) ;
#11287 = CARTESIAN_POINT ( 'NONE',  ( 12.89505231660000106, 1420.989630775359956, 203.4267439564690108 ) ) ;
#11289 = CARTESIAN_POINT ( 'NONE',  ( 0.000000000000000000, 1523.382868172864164, 209.1218459616979999 ) ) ;
#11290 = CARTESIAN_POINT ( 'NONE',  ( -24.35304516410000275, 1443.448750497869923, 211.2141737005680113 ) ) ;
#11291 = DIRECTION ( 'NONE',  ( 0.000000000000000000, 1.000000000000000000, 0.000000000000000000 ) ) ;
#11292 = CARTESIAN_POINT ( 'NONE',  ( 1.185810694231899998, 1430.833857439850135, 199.7444253494500117 ) ) ;
#11293 = CARTESIAN_POINT ( 'NONE',  ( 15.27973127913499951, 1514.812393650459853, 224.9548174513670062 ) ) ;
#11294 = CARTESIAN_POINT ( 'NONE',  ( 5.369445160534993988, 1422.349658812444204, 139.4596679017404881 ) ) ;
#11295 = CARTESIAN_POINT ( 'NONE',  ( 27.15098025384490299, 1509.861193510510248, 222.4858292230849770 ) ) ;
#11296 = B_SPLINE_CURVE_WITH_KNOTS ( 'NONE', 3,
 ( #39732, #100186, #58196, #73898 ),
 .UNSPECIFIED., .F., .F.,
 ( 4, 4 ),
 ( 0.000000000000000000, 1.000000000000000000 ),
 .UNSPECIFIED. ) ;
#11297 = CARTESIAN_POINT ( 'NONE',  ( 1.332267629549999902E-15, 1412.913060387329779, 209.1218459616989946 ) ) ;
#11298 = CARTESIAN_POINT ( 'NONE',  ( -8.407921469289998839, 1475.513060387329915, 228.4380765505979980 ) ) ;
#11299 = CARTESIAN_POINT ( 'NONE',  ( 13.58451889480000041, 1417.422108894029861, 228.5739723679979818 ) ) ;
#11300 = CARTESIAN_POINT ( 'NONE',  ( -1.393816646507355150, 1511.187213306747708, 175.1051575864439656 ) ) ;
#11301 = CARTESIAN_POINT ( 'NONE',  ( -17.14943359400000134, 1460.897694268729992, 228.2718315504980069 ) ) ;
#11302 = CARTESIAN_POINT ( 'NONE',  ( -2.300729664794999962, 1516.923170579120097, 207.4211391557370234 ) ) ;
#11303 = CARTESIAN_POINT ( 'NONE',  ( 45.70279908820000259, 1434.850533281740127, 267.6096423418979953 ) ) ;
#11304 = CARTESIAN_POINT ( 'NONE',  ( -18.68376360200000263, 1410.488798158429972, 223.5328836508979862 ) ) ;
#11305 = CARTESIAN_POINT ( 'NONE',  ( 22.16387887220000152, 1435.699526443600007, 142.3412916024980177 ) ) ;
#11306 = CARTESIAN_POINT ( 'NONE',  ( 22.45934772189999862, 1508.010250242130269, 192.8395958341980077 ) ) ;
#11307 = CARTESIAN_POINT ( 'NONE',  ( 29.34113783274351306, 1509.937680645843329, 206.7119583629535953 ) ) ;
#11308 = DIRECTION ( 'NONE',  ( -0.8090169943749402348, 0.000000000000000000, 0.5877852522924831291 ) ) ;
#11309 = CARTESIAN_POINT ( 'NONE',  ( -42.07524608051735271, 1455.849907682117873, 266.2935988973322310 ) ) ;
#11310 = CARTESIAN_POINT ( 'NONE',  ( 32.23393008293545847, 1523.462669333490567, 216.8400319009756174 ) ) ;
#11311 = CARTESIAN_POINT ( 'NONE',  ( -40.26705548447760208, 1440.962086013470071, 136.8039402764729857 ) ) ;
#11312 = LINE ( 'NONE', #27547, #99761 ) ;
#11313 = CARTESIAN_POINT ( 'NONE',  ( -15.57527174580000029, 1415.800173951010038, 208.9182627945979789 ) ) ;
#11314 = CARTESIAN_POINT ( 'NONE',  ( -17.60627216660330063, 1410.895669502700230, 193.4350316886979897 ) ) ;
#11315 = CARTESIAN_POINT ( 'NONE',  ( -7.565574591425869855, 1384.312222434259866, 219.0525576736690141 ) ) ;
#11316 = CARTESIAN_POINT ( 'NONE',  ( -32.75718327559999921, 1435.641353515060018, 135.5388831429980030 ) ) ;
#11317 = CARTESIAN_POINT ( 'NONE',  ( -7.978005036616639956, 1456.316316171971948, 227.3102628134479630 ) ) ;
#11318 = VERTEX_POINT ( 'NONE', #56495 ) ;
#11319 = CARTESIAN_POINT ( 'NONE',  ( 5.567211196089225211, 1510.484595323987833, 216.6724604399022951 ) ) ;
#11320 = CARTESIAN_POINT ( 'NONE',  ( -9.846997683718040406, 1409.256925123650035, 220.3815847126709855 ) ) ;
#11321 = CARTESIAN_POINT ( 'NONE',  ( 32.09235212274781190, 1525.402221411319260, 196.2603058525789663 ) ) ;
#11322 = CARTESIAN_POINT ( 'NONE',  ( -13.58464396841030108, 1508.551708197639755, 210.0579433922160035 ) ) ;
#11323 = CARTESIAN_POINT ( 'NONE',  ( -3.280536648517546894, 1420.304670650970138, 137.1408270732875110 ) ) ;
#11324 = CARTESIAN_POINT ( 'NONE',  ( -26.80974433740000151, 1468.951693103129855, 269.2446796842979779 ) ) ;
#11325 = CARTESIAN_POINT ( 'NONE',  ( -29.41653834772467135, 1525.790287071772127, 196.6777166491189064 ) ) ;
#11326 = CARTESIAN_POINT ( 'NONE',  ( 0.3958445684936310327, 1418.988079762759980, 184.6579903234699884 ) ) ;
#11327 = CARTESIAN_POINT ( 'NONE',  ( 19.34601893677012185, 1526.333389947941441, 233.0427900344711816 ) ) ;
#11328 = CARTESIAN_POINT ( 'NONE',  ( -85.63289024257620952, 1384.627373604930199, 306.9865616185009571 ) ) ;
#11329 = B_SPLINE_SURFACE_WITH_KNOTS ( 'NONE', 5, 1, ( 
 ( #105232, #71676 ),
 ( #20108, #10057 ),
 ( #105795, #19554 ),
 ( #45890, #86767 ),
 ( #54301, #3348 ),
 ( #103562, #2250 ) ),
 .UNSPECIFIED., .F., .F., .F.,
 ( 6, 6 ),
 ( 2, 2 ),
 ( 65.12635869110000897, 66.80154955991109489 ),
 ( 0.6126808583520000351, 3.463904696680000228 ),
 .UNSPECIFIED. ) ;
#11330 = CARTESIAN_POINT ( 'NONE',  ( -33.66923337122079829, 1384.975952570079926, 207.7792561057779892 ) ) ;
#11331 = DIRECTION ( 'NONE',  ( 0.000000000000000000, 1.000000000000000000, 0.000000000000000000 ) ) ;
#11332 = CARTESIAN_POINT ( 'NONE',  ( 20.59437597599999847, 1507.765470465330054, 227.7647620796980164 ) ) ;
#11333 = CARTESIAN_POINT ( 'NONE',  ( 14.13195592469999973, 1452.421092192730157, 222.7290593249980191 ) ) ;
#11334 = CARTESIAN_POINT ( 'NONE',  ( 2.370970874524633398, 1427.002265528473799, 137.0999999980980135 ) ) ;
#11335 = CARTESIAN_POINT ( 'NONE',  ( 3.160865630554719807, 1370.358795681657284, 206.6712751011299360 ) ) ;
#11336 = CARTESIAN_POINT ( 'NONE',  ( -8.603957690599999708, 1384.941249256889932, 199.8686546726490008 ) ) ;
#11337 = CARTESIAN_POINT ( 'NONE',  ( -24.06753813140000275, 1410.675710981530074, 208.6186337047089978 ) ) ;
#11338 = LINE ( 'NONE', #72354, #71257 ) ;
#11339 = CARTESIAN_POINT ( 'NONE',  ( -12.00387303569999986, 1415.296882282229944, 195.7718046162979704 ) ) ;
#11340 = CARTESIAN_POINT ( 'NONE',  ( -0.2498415990399980025, 1420.995056578739877, 193.6850923126989983 ) ) ;
#11341 = EDGE_CURVE ( 'NONE', #40014, #40412, #35120, .T. ) ;
#11342 = CARTESIAN_POINT ( 'NONE',  ( 22.72019863759999936, 1409.706467206729940, 211.0465802060780049 ) ) ;
#11343 = CARTESIAN_POINT ( 'NONE',  ( -106.5949931321939914, 1391.913060387289988, 305.5646014930300112 ) ) ;
#11344 = CARTESIAN_POINT ( 'NONE',  ( -3.152135748510000113, 1450.885091632490003, 188.5439271930990230 ) ) ;
#11345 = CARTESIAN_POINT ( 'NONE',  ( -5.366470797799430592, 1426.055677132399978, 152.4431534743949896 ) ) ;
#11347 = CARTESIAN_POINT ( 'NONE',  ( -12.14249633790000082, 1377.794244260820051, 206.8888716493889888 ) ) ;
#11346 = CARTESIAN_POINT ( 'NONE',  ( -11.86547436779999920, 1432.299056944690165, 150.3973009728979946 ) ) ;
#11348 = CARTESIAN_POINT ( 'NONE',  ( -5.022927195390000321, 1391.808119929889926, 203.5626871977489998 ) ) ;
#11349 = CARTESIAN_POINT ( 'NONE',  ( -101.5731991332999513, 1376.302340817389677, 292.3950450905593357 ) ) ;
#11350 = EDGE_CURVE ( 'NONE', #32684, #100188, #70840, .T. ) ;
#11351 = CARTESIAN_POINT ( 'NONE',  ( -11.80269316780000111, 1489.550427191690005, 212.2530852381789828 ) ) ;
#11352 = B_SPLINE_CURVE_WITH_KNOTS ( 'NONE', 3,
 ( #90642, #30741, #73309, #88992, #12837, #81142, #47017, #89548, #74429, #13369, #12280, #47558, #100154, #64922, #91201, #48674, #23439, #4457, #72764, #30179, #107995, #73867, #99035, #21205, #106891, #63824, #6093, #22312, #31292, #64371, #97937, #5551, #82250, #13925, #65476, #99585, #40246, #48112, #39701, #46474, #57077, #80606, #3921, #38051, #4986, #72228, #106352, #98494, #29638, #55414, #21762, #90086, #81680, #39130, #67682, #68244, #110206, #77179, #41363, #110762, #482 ),
 .UNSPECIFIED., .F., .F.,
 ( 4, 3, 3, 3, 3, 3, 3, 3, 3, 3, 3, 3, 3, 3, 3, 3, 3, 3, 3, 3, 4 ),
 ( -166.9410549240000137, -166.6317463252630091, -165.1629312876659981, -163.7366513399680059, -162.3365470994540090, -160.9755933037990019, -159.6378003704959951, -158.3210010880789866, -157.0233722586470151, -156.3417070556260171, -154.7029146182070178, -153.0275451752820004, -151.3241472847070099, -149.5649634833510220, -147.7605963360979899, -145.9029318570200076, -143.9806754146449919, -141.9771156308089815, -139.8276503982599763, -137.3711187039190236, -134.5636539103869893 ),
 .UNSPECIFIED. ) ;
#11353 = CARTESIAN_POINT ( 'NONE',  ( -23.14270888800000137, 1415.981602844629833, 211.1002275068279914 ) ) ;
#11354 = CARTESIAN_POINT ( 'NONE',  ( -5.247433916391508468, 1368.770886448055307, 210.6218459616991936 ) ) ;
#11355 = EDGE_CURVE ( 'NONE', #9890, #758, #2800, .T. ) ;
#11356 = CARTESIAN_POINT ( 'NONE',  ( -3.459156616214999591, 1516.769879638719885, 204.5118493505569859 ) ) ;
#11357 = CARTESIAN_POINT ( 'NONE',  ( -19.24890086970000169, 1426.049025734429961, 226.0195547209980305 ) ) ;
#11358 = CARTESIAN_POINT ( 'NONE',  ( -19.02807259538449713, 1485.647960197060002, 189.5790945604939850 ) ) ;
#11359 = CARTESIAN_POINT ( 'NONE',  ( 12.44781172279570036, 1501.268274303350154, 211.7240488200220341 ) ) ;
#11360 = CARTESIAN_POINT ( 'NONE',  ( -11.56191713950926925, 1421.985365140208387, 210.6398819361144206 ) ) ;
#11362 = EDGE_LOOP ( 'NONE', ( #70091, #110735, #80095, #36403 ) ) ;
#11361 = CARTESIAN_POINT ( 'NONE',  ( -65.44977854169999887, 1379.747342584589887, 275.4353169223589930 ) ) ;
#11363 = EDGE_CURVE ( 'NONE', #25815, #4737, #69839, .T. ) ;
#11364 = EDGE_LOOP ( 'NONE', ( #85491, #101188, #28723, #9456, #64918 ) ) ;
#11365 = CARTESIAN_POINT ( 'NONE',  ( 28.87050041479999862, 1509.923266469329747, 215.0239930259780010 ) ) ;
#11366 = EDGE_LOOP ( 'NONE', ( #32457, #79960, #104344, #85651 ) ) ;
#11367 = CARTESIAN_POINT ( 'NONE',  ( -105.4520934690000047, 1378.947384221549783, 304.5880789179589669 ) ) ;
#11368 = CARTESIAN_POINT ( 'NONE',  ( -109.3076610239999980, 1384.932499147180124, 311.2646262372589945 ) ) ;
#11370 = CARTESIAN_POINT ( 'NONE',  ( 22.30619483830000149, 1451.363309493629913, 221.4011829164979872 ) ) ;
#11369 = CARTESIAN_POINT ( 'NONE',  ( 1.608351468689999786, 1426.598937817530214, 144.1938086916980239 ) ) ;
#11371 = CARTESIAN_POINT ( 'NONE',  ( -0.7176848839889999887, 1417.283279384530033, 235.8571367780980097 ) ) ;
#11372 = CARTESIAN_POINT ( 'NONE',  ( -24.97479332202350122, 1451.884380675330021, 136.4887619541970025 ) ) ;
#11373 = CARTESIAN_POINT ( 'NONE',  ( -0.1544838608760010223, 1468.067337115490091, 219.5125637271989945 ) ) ;
#11374 = CARTESIAN_POINT ( 'NONE',  ( 13.47403807739999948, 1410.316254106229962, 228.2920107387979840 ) ) ;
#11375 = CARTESIAN_POINT ( 'NONE',  ( 7.336844642415000450, 1517.106845464700200, 212.5753907958570039 ) ) ;
#11376 = CARTESIAN_POINT ( 'NONE',  ( 40.21460569533279994, 1439.107902997649944, 134.0999999981339954 ) ) ;
#11377 = CARTESIAN_POINT ( 'NONE',  ( -5.314640358949040078, 1425.825096639779986, 208.2911617466580196 ) ) ;
#11378 = CARTESIAN_POINT ( 'NONE',  ( -0.5656601614563600000, 1424.194575819369902, 228.0927458373740251 ) ) ;
#11379 = EDGE_LOOP ( 'NONE', ( #13415, #5294, #10806, #73899, #41511 ) ) ;
#11380 = CARTESIAN_POINT ( 'NONE',  ( 5.140106207186420306, 1436.845544181910100, 228.7442480593620076 ) ) ;
#11381 = FACE_OUTER_BOUND ( 'NONE', #68666, .T. ) ;
#11382 = ORIENTED_EDGE ( 'NONE', *, *, #2209, .F. ) ;
#11383 = VERTEX_POINT ( 'NONE', #46455 ) ;
#11384 = ORIENTED_EDGE ( 'NONE', *, *, #44367, .F. ) ;
#11385 = CARTESIAN_POINT ( 'NONE',  ( -8.080850468484999993, 1512.335510084620182, 215.7195519849769880 ) ) ;
#11386 = CARTESIAN_POINT ( 'NONE',  ( -1.835915931920000022, 1464.997577601130160, 237.8268836853979735 ) ) ;
#11387 = CARTESIAN_POINT ( 'NONE',  ( 20.24763625415679513, 1450.973946380246161, 145.3523280452958488 ) ) ;
#11388 = CARTESIAN_POINT ( 'NONE',  ( -3.043465616510000249, 1485.522934885530049, 182.9100814775980268 ) ) ;
#11389 = CARTESIAN_POINT ( 'NONE',  ( 2.632111276144470047, 1466.096714734490206, 198.4011313589680015 ) ) ;
#11391 = ADVANCED_FACE ( 'NONE', ( #21188 ), #51388, .F. ) ;
#11390 = ADVANCED_FACE ( 'NONE', ( #3903 ), #55397, .F. ) ;
#11392 = CARTESIAN_POINT ( 'NONE',  ( -17.72975366969933830, 1447.779520654833505, 217.4447075265184139 ) ) ;
#11393 = CARTESIAN_POINT ( 'NONE',  ( -66.28715543682936584, 1379.742552331314528, 274.9634317763816398 ) ) ;
#11394 = CARTESIAN_POINT ( 'NONE',  ( 4.275908414736929508, 1446.766556631309868, 157.1258821310249800 ) ) ;
#11395 = EDGE_CURVE ( 'NONE', #22920, #8770, #79160, .T. ) ;
#11396 = CARTESIAN_POINT ( 'NONE',  ( 0.9965953362400000737, 1508.939483211730021, 238.5777243435979926 ) ) ;
#11397 = ORIENTED_EDGE ( 'NONE', *, *, #633, .T. ) ;
#11398 = CARTESIAN_POINT ( 'NONE',  ( 2.282301578035000222, 1516.836638729160086, 207.4044134838369757 ) ) ;
#11399 = ORIENTED_EDGE ( 'NONE', *, *, #59162, .T. ) ;
#11400 = CARTESIAN_POINT ( 'NONE',  ( 28.57350514777099804, 1440.913060387330006, 248.9574316567099856 ) ) ;
#11401 = B_SPLINE_CURVE_WITH_KNOTS ( 'NONE', 3,
 ( #1491, #18810, #61414, #93863, #69255, #42938 ),
 .UNSPECIFIED., .F., .F.,
 ( 4, 2, 4 ),
 ( 0.000000000000000000, 0.5000000000000000000, 1.000000000000000000 ),
 .UNSPECIFIED. ) ;
#11402 = CARTESIAN_POINT ( 'NONE',  ( -14.35518106359999990, 1509.483853030530099, 182.9676315445979924 ) ) ;
#11403 = ORIENTED_EDGE ( 'NONE', *, *, #26110, .T. ) ;
#11404 = CARTESIAN_POINT ( 'NONE',  ( -6.141356664424689527, 1509.034509698630018, 201.6091305267439964 ) ) ;
#11405 = CARTESIAN_POINT ( 'NONE',  ( -14.68857900839999964, 1409.425996869029859, 192.2200297474979891 ) ) ;
#11406 = CARTESIAN_POINT ( 'NONE',  ( -51.74412866941842282, 1379.698572072603383, 249.1812003707125882 ) ) ;
#11408 = CARTESIAN_POINT ( 'NONE',  ( 0.04987450923691939819, 1450.914802043100053, 185.2444802929140053 ) ) ;
#11407 = CARTESIAN_POINT ( 'NONE',  ( -24.49620803319999851, 1440.956469628590185, 210.9946876184580162 ) ) ;
#11409 = CARTESIAN_POINT ( 'NONE',  ( 22.39828147038580397, 1410.488771300080089, 206.2224881104899907 ) ) ;
#11410 = CARTESIAN_POINT ( 'NONE',  ( -6.099948008796559407, 1511.445028088800200, 201.4631254019980133 ) ) ;
#11411 = CARTESIAN_POINT ( 'NONE',  ( 25.91590772989999891, 1441.261220175949802, 138.4451201509980365 ) ) ;
#11412 = CARTESIAN_POINT ( 'NONE',  ( 17.17760792425680094, 1517.051704368240053, 222.7507317666290305 ) ) ;
#11413 = CARTESIAN_POINT ( 'NONE',  ( -3.606501271529999997, 1507.464096719490044, 221.5253835883989950 ) ) ;
#11415 = CARTESIAN_POINT ( 'NONE',  ( 5.469059239369999936, 1437.444982562589985, 208.6508151085089935 ) ) ;
#11414 = CARTESIAN_POINT ( 'NONE',  ( 10.13643151279999977, 1462.749890840729904, 234.3975521353980014 ) ) ;
#11416 = CARTESIAN_POINT ( 'NONE',  ( -2.289624470354999719, 1517.154223579619838, 215.6854418399169901 ) ) ;
#11417 = CARTESIAN_POINT ( 'NONE',  ( 11.73709356406289928, 1426.695943121369965, 144.1748013758129900 ) ) ;
#11418 = CARTESIAN_POINT ( 'NONE',  ( 5.854887922672690870, 1510.764648358900104, 216.6679770094980313 ) ) ;
#11419 = CYLINDRICAL_SURFACE ( 'NONE', #40830, 2.000000000000003553 ) ;
#11420 = CARTESIAN_POINT ( 'NONE',  ( -6.547556969464999987, 1516.633288330999903, 212.3841106205370011 ) ) ;
#11421 = CARTESIAN_POINT ( 'NONE',  ( -11.65753171920430020, 1482.533532356269916, 206.7098060248759737 ) ) ;
#11422 = DIRECTION ( 'NONE',  ( 0.3090169943749582204, 0.000000000000000000, 0.9510565162951499785 ) ) ;
#11424 = ORIENTED_EDGE ( 'NONE', *, *, #43339, .T. ) ;
#11423 = CARTESIAN_POINT ( 'NONE',  ( -103.6582916800000049, 1388.280209741639965, 298.0463838127590748 ) ) ;
#11425 = CARTESIAN_POINT ( 'NONE',  ( -0.7692391029760000665, 1415.628674266529742, 227.3871686175980074 ) ) ;
#11426 = CARTESIAN_POINT ( 'NONE',  ( 17.31784991639999660, 1457.605539162629839, 225.7849821470979919 ) ) ;
#11427 = CARTESIAN_POINT ( 'NONE',  ( -6.944001484987491146, 1487.611668854129675, 219.0757229943065454 ) ) ;
#11428 = CARTESIAN_POINT ( 'NONE',  ( -14.98950744470000096, 1415.677402218840143, 206.7597182584589746 ) ) ;
#11429 = CARTESIAN_POINT ( 'NONE',  ( 2.421990954390000006, 1414.535087205929813, 231.9310730028979890 ) ) ;
#11430 = CARTESIAN_POINT ( 'NONE',  ( -18.84860651810000221, 1456.786630790930076, 228.5413354239980208 ) ) ;
#11432 = CARTESIAN_POINT ( 'NONE',  ( 19.24021961950000303, 1455.885573259829926, 225.9459216509980024 ) ) ;
#11431 = CARTESIAN_POINT ( 'NONE',  ( -21.75307144610911791, 1411.033070506304966, 201.6242908587096565 ) ) ;
#11433 = CARTESIAN_POINT ( 'NONE',  ( -10.22074380055929943, 1448.827829969109871, 207.2903289465359933 ) ) ;
#11434 = CARTESIAN_POINT ( 'NONE',  ( -106.3487258514710021, 1380.529443125889884, 308.5284918366859870 ) ) ;
#11435 = ORIENTED_EDGE ( 'NONE', *, *, #56421, .T. ) ;
#11436 = CARTESIAN_POINT ( 'NONE',  ( -1.131796848745000084, 1516.659138130710289, 203.3488676535569937 ) ) ;
#11437 = CARTESIAN_POINT ( 'NONE',  ( 1.312236371940000090, 1406.790645662230190, 269.6495478408979807 ) ) ;
#11438 = CARTESIAN_POINT ( 'NONE',  ( -1.106162138419999996, 1515.349603040190004, 213.4044250793790241 ) ) ;
#11439 = CARTESIAN_POINT ( 'NONE',  ( 31.30797101508039759, 1465.106566905469890, 270.3267909516169993 ) ) ;
#11440 = CARTESIAN_POINT ( 'NONE',  ( 2.477972021390000279, 1440.426960907559987, 157.8055583485979980 ) ) ;
#11441 = CARTESIAN_POINT ( 'NONE',  ( 10.43902076892678288, 1423.422239459952834, 137.2931753684112550 ) ) ;
#11442 = CARTESIAN_POINT ( 'NONE',  ( -39.96238005862740295, 1440.913060402280053, 259.2337657365459904 ) ) ;
#11443 = CARTESIAN_POINT ( 'NONE',  ( -26.25855011770000047, 1449.905647651959953, 136.7332828859979941 ) ) ;
#11444 = CARTESIAN_POINT ( 'NONE',  ( 3.601839739459999912, 1444.840594719589944, 200.9001243581789993 ) ) ;
#11445 = FACE_OUTER_BOUND ( 'NONE', #63874, .T. ) ;
#11446 = CARTESIAN_POINT ( 'NONE',  ( 1.747352932607996179, 1465.628108031464308, 235.0395402516389822 ) ) ;
#11447 = CARTESIAN_POINT ( 'NONE',  ( -21.80586122364568169, 1523.954914175599924, 183.3405075822116430 ) ) ;
#11448 = CARTESIAN_POINT ( 'NONE',  ( 17.45961317077569674, 1413.562297865003075, 192.3730989426080669 ) ) ;
#11449 = ORIENTED_EDGE ( 'NONE', *, *, #7124, .F. ) ;
#11450 = CARTESIAN_POINT ( 'NONE',  ( -19.47651264659999626, 1426.266543402430216, 243.9198229517980110 ) ) ;
#11451 = VECTOR ( 'NONE', #64101, 1000.000000000000114 ) ;
#11452 = CARTESIAN_POINT ( 'NONE',  ( 1.159696500349999937, 1485.109384876889862, 198.4167286540990176 ) ) ;
#11453 = CARTESIAN_POINT ( 'NONE',  ( 9.406701834158939235, 1468.782307090909853, 204.4388643328819910 ) ) ;
#11454 = CARTESIAN_POINT ( 'NONE',  ( -0.8852285261829999641, 1475.753581647529927, 269.0453912508980352 ) ) ;
#11455 = CARTESIAN_POINT ( 'NONE',  ( -4.272885081469669721, 1446.730020358119873, 157.5808617883949978 ) ) ;
#11456 = CARTESIAN_POINT ( 'NONE',  ( -28.44347337880000381, 1509.158830949329968, 209.7035872210599905 ) ) ;
#11457 = CARTESIAN_POINT ( 'NONE',  ( -2.774022723599062878, 1448.257693116544715, 184.1777864073213493 ) ) ;
#11458 = CARTESIAN_POINT ( 'NONE',  ( -28.12733322275310144, 1384.835236073490023, 226.2207532044819800 ) ) ;
#11459 = VECTOR ( 'NONE', #87276, 1000.000000000000000 ) ;
#11460 = B_SPLINE_SURFACE_WITH_KNOTS ( 'NONE', 5, 5, ( 
 ( #70864, #45652, #53490, #52934, #78672, #71421 ),
 ( #105537, #37777, #72488, #29903, #64095, #98217 ),
 ( #87070, #10355, #44526, #36125, #70309, #104422 ),
 ( #10922, #109397, #39419, #48391, #100426, #92029 ),
 ( #47824, #98769, #107726, #21485, #89819, #4711 ),
 ( #39969, #15300, #83078, #30463, #81959, #56228 ),
 ( #32124, #13092, #91481, #47276, #81399, #23709 ),
 ( #65191, #22578, #74146, #56782, #23155, #108276 ),
 ( #49493, #38854, #90920, #31564, #57893, #73033 ) ),
 .UNSPECIFIED., .F., .F., .F.,
 ( 6, 3, 6 ),
 ( 6, 6 ),
 ( 13.91937871330000043, 27.07797103040000053, 31.90163864219999823 ),
 ( 0.000000000000000000, 2.000000000000000000 ),
 .UNSPECIFIED. ) ;
#11461 = CARTESIAN_POINT ( 'NONE',  ( -18.46483594369999892, 1415.628674276729953, 207.5691869113279893 ) ) ;
#11462 = CARTESIAN_POINT ( 'NONE',  ( -9.878263419269998735, 1481.129257303990016, 205.3617022385789994 ) ) ;
#11463 = CARTESIAN_POINT ( 'NONE',  ( 26.57248659439540006, 1436.418273096599933, 136.7276480538729970 ) ) ;
#11464 =( BOUNDED_SURFACE ( )  B_SPLINE_SURFACE ( 1, 2, ( 
 ( #87864, #70525, #36329, #36884, #27938, #62120, #46418, #28491, #104086 ),
 ( #18960, #45315, #2763, #37444, #103528, #78910, #61560, #80550, #35788 ) ),
 .UNSPECIFIED., .F., .T., .F. ) 
 B_SPLINE_SURFACE_WITH_KNOTS ( ( 2, 2 ),
 ( 3, 2, 2, 2, 3 ),
 ( -10000.00000000000000, 10000.00000000000000 ),
 ( 0.000000000000000000, 1.570796326794899889, 3.141592653589790007, 4.712388980384689674, 6.283185307179590673 ),
 .UNSPECIFIED. ) 
 GEOMETRIC_REPRESENTATION_ITEM ( )  RATIONAL_B_SPLINE_SURFACE ( (
 ( 1.000000000000000000, 0.7071067811865480168, 1.000000000000000000, 0.7071067811865480168, 1.000000000000000000, 0.7071067811865480168, 1.000000000000000000, 0.7071067811865480168, 1.000000000000000000),
 ( 1.000000000000000000, 0.7071067811865480168, 1.000000000000000000, 0.7071067811865480168, 1.000000000000000000, 0.7071067811865480168, 1.000000000000000000, 0.7071067811865480168, 1.000000000000000000) ) ) 
 REPRESENTATION_ITEM ( '' )  SURFACE ( )  );
#11465 = CARTESIAN_POINT ( 'NONE',  ( -9.494076726826639501, 1396.244600852259964, 214.8009319264149894 ) ) ;
#11466 = CARTESIAN_POINT ( 'NONE',  ( -15.08655487470000089, 1422.047410306030088, 227.7513007382979993 ) ) ;
#11467 = CARTESIAN_POINT ( 'NONE',  ( 30.31052258194586102, 1523.604703353109699, 195.7506062427368079 ) ) ;
#11468 = CARTESIAN_POINT ( 'NONE',  ( 2.500000000000000000, 1443.913060387330006, 150.6726614421979775 ) ) ;
#11469 = VERTEX_POINT ( 'NONE', #109644 ) ;
#11470 = CARTESIAN_POINT ( 'NONE',  ( -4.364633595095840590, 1436.783259246580201, 227.1130992530970047 ) ) ;
#11471 = CARTESIAN_POINT ( 'NONE',  ( 2.643999269920000117, 1409.509886378629972, 231.4605033490980190 ) ) ;
#11472 = CARTESIAN_POINT ( 'NONE',  ( -16.30638770610000066, 1484.820604609629981, 187.8396872195979768 ) ) ;
#11474 = CARTESIAN_POINT ( 'NONE',  ( -14.32022880866499825, 1513.136578080079744, 193.2786756054669866 ) ) ;
#11473 = CARTESIAN_POINT ( 'NONE',  ( 10.83435298340000053, 1425.666604291029898, 103.4417286516979999 ) ) ;
#11475 = FACE_OUTER_BOUND ( 'NONE', #88696, .T. ) ;
#11476 = CARTESIAN_POINT ( 'NONE',  ( -12.37499353609999986, 1442.762691980110048, 151.6327898328030130 ) ) ;
#11477 = CARTESIAN_POINT ( 'NONE',  ( -109.9873428579799963, 1384.764085902139868, 311.4531231889159812 ) ) ;
#11478 = CARTESIAN_POINT ( 'NONE',  ( 7.438538526529999473, 1425.192287214430053, 212.3736570440989908 ) ) ;
#11479 = CARTESIAN_POINT ( 'NONE',  ( -18.92738905869999755, 1503.346139545890082, 222.1981867166989844 ) ) ;
#11480 = CARTESIAN_POINT ( 'NONE',  ( 4.349085017430000200, 1508.966281798729824, 180.4853875712980198 ) ) ;
#11481 = CARTESIAN_POINT ( 'NONE',  ( 7.777794710095000674, 1511.980236064749988, 206.2293425532969877 ) ) ;
#11482 = CARTESIAN_POINT ( 'NONE',  ( -56.13014929047670165, 1379.450323875860022, 260.0068040503380189 ) ) ;
#11483 = AXIS2_PLACEMENT_3D ( 'NONE', #15466, #30637, #82132 ) ;
#11484 = CARTESIAN_POINT ( 'NONE',  ( 7.427103032054851894, 1365.589452326314131, 209.6218459617148824 ) ) ;
#11486 = EDGE_LOOP ( 'NONE', ( #66428, #28430, #29144, #64257, #109709, #71857, #74015, #1744 ) ) ;
#11485 = CARTESIAN_POINT ( 'NONE',  ( -11.45446813149230003, 1462.185551532946420, 233.9517320718034625 ) ) ;
#11487 = EDGE_LOOP ( 'NONE', ( #69112, #57440, #9452, #1174 ) ) ;
#11488 = ADVANCED_FACE ( 'NONE', ( #83880 ), #84440, .F. ) ;
#11489 = CARTESIAN_POINT ( 'NONE',  ( 8.537822598675001373, 1517.051704408389924, 212.5465662711270056 ) ) ;
#11490 = CARTESIAN_POINT ( 'NONE',  ( -12.41103214550000011, 1409.346463180030014, 190.9867524833979928 ) ) ;
#11491 = LINE ( 'NONE', #36684, #67259 ) ;
#11492 = CARTESIAN_POINT ( 'NONE',  ( -3.551846384670535262, 1441.533148028869391, 200.9985935998525974 ) ) ;
#11494 = CARTESIAN_POINT ( 'NONE',  ( -2.783288780519999950, 1486.112700186630036, 181.9037838507979927 ) ) ;
#11493 = CARTESIAN_POINT ( 'NONE',  ( -7.769784056169999786, 1383.283767220619893, 218.8591793915190067 ) ) ;
#11495 = DIRECTION ( 'NONE',  ( -0.8090169943749467851, 1.070063492533079265E-14, -0.5877852522924740253 ) ) ;
#11496 = LINE ( 'NONE', #96602, #101489 ) ;
#11497 = ADVANCED_FACE ( 'NONE', ( #7184 ), #42430, .F. ) ;
#11498 = CARTESIAN_POINT ( 'NONE',  ( -41.04864394093900160, 1445.151157643809938, 136.7380822686889985 ) ) ;
#11499 = CARTESIAN_POINT ( 'NONE',  ( -2.500000000000000000, 1448.592472799309917, 159.2571715835509849 ) ) ;
#11500 = CARTESIAN_POINT ( 'NONE',  ( -12.99570043321834589, 1434.780757546461246, 149.5535408288678241 ) ) ;
#11501 = CARTESIAN_POINT ( 'NONE',  ( -28.11559569040000284, 1443.570698335159932, 137.5389433187979762 ) ) ;
#11502 = CARTESIAN_POINT ( 'NONE',  ( -3.789557337974839957, 1406.612116051730027, 269.4941210699120120 ) ) ;
#11503 = CARTESIAN_POINT ( 'NONE',  ( 40.27287714639999905, 1443.726400947989987, 137.1298442681979850 ) ) ;
#11504 = VERTEX_POINT ( 'NONE', #67110 ) ;
#11505 = CARTESIAN_POINT ( 'NONE',  ( -20.20959865099451847, 1501.977400791986611, 236.2316688286741453 ) ) ;
#11506 = CARTESIAN_POINT ( 'NONE',  ( 21.08094518543042284, 1525.506926151471362, 234.2044941741795867 ) ) ;
#11507 = ORIENTED_EDGE ( 'NONE', *, *, #89820, .T. ) ;
#11508 = VERTEX_POINT ( 'NONE', #93378 ) ;
#11509 = CARTESIAN_POINT ( 'NONE',  ( -3.271537977250000395, 1454.292002038190049, 199.1638778798389922 ) ) ;
#11510 = CARTESIAN_POINT ( 'NONE',  ( -9.936738324559998503, 1364.340818343090177, 207.6218459616989946 ) ) ;
#11511 = CARTESIAN_POINT ( 'NONE',  ( -4.612507312034999529, 1516.886345593249871, 214.1313240375470173 ) ) ;
#11512 = CARTESIAN_POINT ( 'NONE',  ( 3.927225866655000619, 1511.005930286180046, 216.7576803329270092 ) ) ;
#11513 = ORIENTED_EDGE ( 'NONE', *, *, #92691, .T. ) ;
#11514 = CARTESIAN_POINT ( 'NONE',  ( 7.957350483939999108, 1425.611849966230011, 211.5358269577189958 ) ) ;
#11515 = CARTESIAN_POINT ( 'NONE',  ( -63.58938923220000561, 1379.821258372549892, 269.7443356278590159 ) ) ;
#11516 = EDGE_CURVE ( 'NONE', #49433, #63638, #8311, .T. ) ;
#11517 = CARTESIAN_POINT ( 'NONE',  ( -107.2050354704289958, 1378.913060387309770, 300.9024058946000082 ) ) ;
#11518 = CARTESIAN_POINT ( 'NONE',  ( -7.334957394705000411, 1517.030858226499959, 204.5055736355369902 ) ) ;
#11519 = CARTESIAN_POINT ( 'NONE',  ( -12.15405767247520075, 1489.994125339409948, 210.5239156192949963 ) ) ;
#11520 = CARTESIAN_POINT ( 'NONE',  ( -41.37929305821487702, 1435.466738718876059, 269.6357249460477306 ) ) ;
#11521 = CARTESIAN_POINT ( 'NONE',  ( 1.710012720495000194, 1517.232977404109988, 201.3945188173769907 ) ) ;
#11522 = CARTESIAN_POINT ( 'NONE',  ( -5.081689812120000482, 1409.257665803229884, 231.2512572095979806 ) ) ;
#11524 = ORIENTED_EDGE ( 'NONE', *, *, #17257, .T. ) ;
#11523 = CARTESIAN_POINT ( 'NONE',  ( -4.080430317250000272, 1447.666642389649951, 185.0612220870980025 ) ) ;
#11525 = CARTESIAN_POINT ( 'NONE',  ( -12.53380499169999851, 1445.052233488290085, 177.5748921271979839 ) ) ;
#11526 = CARTESIAN_POINT ( 'NONE',  ( -26.09031900081160060, 1440.913060473340011, 222.3459699190599963 ) ) ;
#11527 = CIRCLE ( 'NONE', #74116, 1.000000000000000888 ) ;
#11528 = FACE_OUTER_BOUND ( 'NONE', #40312, .T. ) ;
#11529 = CARTESIAN_POINT ( 'NONE',  ( 21.02608924029999926, 1456.853724928630072, 225.6706377209980303 ) ) ;
#11530 = CARTESIAN_POINT ( 'NONE',  ( 39.81566866050809494, 1428.288687989800110, 270.1753679354689552 ) ) ;
#11531 = CARTESIAN_POINT ( 'NONE',  ( 2.879642153204999833, 1516.812046502680005, 212.5681757458869754 ) ) ;
#11532 = CARTESIAN_POINT ( 'NONE',  ( -65.92707478070001059, 1379.741696281819941, 274.2307012748590296 ) ) ;
#11533 = VECTOR ( 'NONE', #14759, 1000.000000000000000 ) ;
#11534 = CARTESIAN_POINT ( 'NONE',  ( 0.01782758894743981942, 1507.551620162875224, 237.4204223254480155 ) ) ;
#11535 = CARTESIAN_POINT ( 'NONE',  ( -30.12464261468167592, 1524.523992613102337, 222.3823409144095535 ) ) ;
#11536 = CARTESIAN_POINT ( 'NONE',  ( 18.96076900870300008, 1410.937160519182044, 195.1859992452610300 ) ) ;
#11537 = CARTESIAN_POINT ( 'NONE',  ( -6.938478822895000064, 1516.719999691880048, 209.8757167055200057 ) ) ;
#11538 = ORIENTED_EDGE ( 'NONE', *, *, #36740, .F. ) ;
#11539 = CARTESIAN_POINT ( 'NONE',  ( 2.500000000000000000, 1436.420121157869971, 157.6233376561979753 ) ) ;
#11540 = CARTESIAN_POINT ( 'NONE',  ( -10.30053490859999954, 1417.902178291030168, 229.8560290380979723 ) ) ;
#11541 = CARTESIAN_POINT ( 'NONE',  ( 5.940759646534202076, 1420.421523195163218, 137.0999999980978146 ) ) ;
#11542 = ORIENTED_EDGE ( 'NONE', *, *, #32444, .T. ) ;
#11543 = CARTESIAN_POINT ( 'NONE',  ( -22.15429900546649833, 1385.267682785860188, 221.9372924518760044 ) ) ;
#11544 = CARTESIAN_POINT ( 'NONE',  ( -3.119872722899999840, 1429.296741504189868, 201.0353256376990316 ) ) ;
#11545 = CARTESIAN_POINT ( 'NONE',  ( 18.64722824082740260, 1478.712861779200011, 228.5761396551030202 ) ) ;
#11546 = CARTESIAN_POINT ( 'NONE',  ( 19.08918182269999875, 1507.695925188030060, 188.5883432463980114 ) ) ;
#11547 = CARTESIAN_POINT ( 'NONE',  ( -30.79107737087808871, 1526.107876515966609, 217.1184129874169741 ) ) ;
#11548 = CARTESIAN_POINT ( 'NONE',  ( -9.519812938348620079, 1460.017558366200092, 210.6311618255110147 ) ) ;
#11549 = CARTESIAN_POINT ( 'NONE',  ( 0.1036083437597169893, 1420.454746905719958, 182.6982413274450039 ) ) ;
#11551 = CARTESIAN_POINT ( 'NONE',  ( 22.08523867432351295, 1523.530870145309564, 184.4211813602697134 ) ) ;
#11550 = CARTESIAN_POINT ( 'NONE',  ( -2.289624470354999719, 1517.154223579619838, 215.6854418399169901 ) ) ;
#11552 = CARTESIAN_POINT ( 'NONE',  ( 19.28393622879999825, 1507.737928638330004, 188.6540313642980209 ) ) ;
#11553 = CARTESIAN_POINT ( 'NONE',  ( 16.66936639845630097, 1512.187213306747481, 180.4828114240739296 ) ) ;
#11554 = ORIENTED_EDGE ( 'NONE', *, *, #99292, .T. ) ;
#11555 = CARTESIAN_POINT ( 'NONE',  ( -12.84940689358420052, 1416.524489948229984, 196.3858981729360096 ) ) ;
#11556 = CARTESIAN_POINT ( 'NONE',  ( -0.7339482261329999258, 1499.713796587029947, 181.0788772114979963 ) ) ;
#11557 = ORIENTED_EDGE ( 'NONE', *, *, #37123, .F. ) ;
#11558 = CARTESIAN_POINT ( 'NONE',  ( -15.78436440076501768, 1512.151624459629829, 220.2511651824670196 ) ) ;
#11559 = DIRECTION ( 'NONE',  ( 0.000000000000000000, -5.238603995039999762E-10, -1.000000000000000000 ) ) ;
#11560 = CARTESIAN_POINT ( 'NONE',  ( 7.670153655591260389, 1511.304111283970087, 203.1182573986329771 ) ) ;
#11561 = CIRCLE ( 'NONE', #74167, 0.9999999999999930056 ) ;
#11562 = CARTESIAN_POINT ( 'NONE',  ( 2.911424594440000124, 1441.585781036189928, 218.2054819051689947 ) ) ;
#11563 = CARTESIAN_POINT ( 'NONE',  ( 16.31271465393231068, 1421.545148970794116, 227.2409568857196689 ) ) ;
#11564 = LINE ( 'NONE', #48910, #42464 ) ;
#11565 = CARTESIAN_POINT ( 'NONE',  ( 2.326513307799999986, 1476.258183369789776, 197.8633931413990013 ) ) ;
#11566 = CARTESIAN_POINT ( 'NONE',  ( -17.61522799909999648, 1423.733526167929767, 226.4046865996980102 ) ) ;
#11567 = CARTESIAN_POINT ( 'NONE',  ( -15.45606833479999942, 1435.037147414750052, 147.9572051551980110 ) ) ;
#11568 = CARTESIAN_POINT ( 'NONE',  ( 4.363122647530000009, 1409.354802298930053, 146.1721969590979882 ) ) ;
#11569 = CARTESIAN_POINT ( 'NONE',  ( 16.57268409019999922, 1413.521687218830039, 191.5369357848979917 ) ) ;
#11571 = CARTESIAN_POINT ( 'NONE',  ( 4.329358020582290578, 1515.068258693859889, 207.4791162324520144 ) ) ;
#11570 = CARTESIAN_POINT ( 'NONE',  ( 1.354644225578049976, 1409.895065699369752, 232.6225702936600044 ) ) ;
#11572 = CARTESIAN_POINT ( 'NONE',  ( -9.756549938588090498, 1472.065839394849945, 211.9795509805560130 ) ) ;
#11573 = VERTEX_POINT ( 'NONE', #33459 ) ;
#11574 = FACE_OUTER_BOUND ( 'NONE', #55271, .T. ) ;
#11575 = CARTESIAN_POINT ( 'NONE',  ( -30.31052258194604576, 1523.604703353109699, 195.7506062427372058 ) ) ;
#11576 = CARTESIAN_POINT ( 'NONE',  ( -24.23130831839999999, 1437.896962395750052, 211.0914046272980045 ) ) ;
#11577 = CARTESIAN_POINT ( 'NONE',  ( -3.817423482790000211, 1484.725631220790092, 198.6719352447990161 ) ) ;
#11578 = CARTESIAN_POINT ( 'NONE',  ( -18.59400683710000024, 1508.850372359329867, 229.9901379698980008 ) ) ;
#11579 = CARTESIAN_POINT ( 'NONE',  ( -3.177670542995198133, 1525.042412244750722, 241.6057155832064325 ) ) ;
#11580 = CARTESIAN_POINT ( 'NONE',  ( 18.71266994490000002, 1408.913060387329779, 210.0964815640089682 ) ) ;
#11581 = B_SPLINE_SURFACE_WITH_KNOTS ( 'NONE', 5, 5, ( 
 ( #20254, #104827, #11873, #62304, #28113, #95324 ),
 ( #80177, #77966, #1274, #70165, #35413, #11332 ),
 ( #79645, #3493, #46045, #61748, #36520, #2402 ),
 ( #2947, #71824, #105944, #19136, #53340, #70713 ),
 ( #86364, #103719, #27021, #61210, #4038, #38166 ),
 ( #72347, #30310, #99704, #106476, #98616, #21879 ) ),
 .UNSPECIFIED., .F., .F., .F.,
 ( 6, 6 ),
 ( 6, 6 ),
 ( 4.813401939820000308, 5.109425210320000410 ),
 ( 0.000000000000000000, 2.000000000000000000 ),
 .UNSPECIFIED. ) ;
#11582 = DIRECTION ( 'NONE',  ( -1.224646799147350002E-16, 1.836970198721029688E-16, 1.000000000000000000 ) ) ;
#11583 = CARTESIAN_POINT ( 'NONE',  ( -14.10735888110919944, 1509.405700215120078, 183.4262508031069956 ) ) ;
#11584 = CARTESIAN_POINT ( 'NONE',  ( -10.44425495210050059, 1490.271910750019970, 212.9366649069719983 ) ) ;
#11585 = CARTESIAN_POINT ( 'NONE',  ( -18.65941870309999828, 1468.219763198689861, 201.0822021908089994 ) ) ;
#11586 = CARTESIAN_POINT ( 'NONE',  ( -82.66607780726680232, 1383.775112911549968, 305.2794127350090321 ) ) ;
#11587 = CARTESIAN_POINT ( 'NONE',  ( -108.7284267277110104, 1383.837174741619947, 311.1014926787349850 ) ) ;
#11588 = CARTESIAN_POINT ( 'NONE',  ( -5.124785876484846625, 1391.876141467484103, 214.5965346519774926 ) ) ;
#11589 = CARTESIAN_POINT ( 'NONE',  ( -0.8697201140136210373, 1516.690597168679915, 201.4087215436879887 ) ) ;
#11591 = EDGE_LOOP ( 'NONE', ( #38777, #47710, #72689, #105048 ) ) ;
#11590 = CARTESIAN_POINT ( 'NONE',  ( 20.32974505740000026, 1508.870382120730028, 189.2250245169979905 ) ) ;
#11592 = CARTESIAN_POINT ( 'NONE',  ( -92.36490218759999493, 1379.347538457270048, 300.9928459216590113 ) ) ;
#11593 = CARTESIAN_POINT ( 'NONE',  ( -0.6434364284315916560, 1417.244662098927847, 234.6835996158768864 ) ) ;
#11594 = EDGE_LOOP ( 'NONE', ( #49100, #71110, #74495, #9348 ) ) ;
#11595 = ORIENTED_EDGE ( 'NONE', *, *, #106261, .T. ) ;
#11596 = CARTESIAN_POINT ( 'NONE',  ( 12.70666910289999940, 1441.123310893239932, 188.6801198206979961 ) ) ;
#11597 = CARTESIAN_POINT ( 'NONE',  ( 13.87302018090000111, 1509.389573182929780, 234.2955351351979800 ) ) ;
#11598 = CARTESIAN_POINT ( 'NONE',  ( 21.41971086555102133, 1512.187213306747481, 233.0798096144380906 ) ) ;
#11600 = CARTESIAN_POINT ( 'NONE',  ( -29.81189556660000051, 1458.385315375329810, 254.8364576145980038 ) ) ;
#11599 = CARTESIAN_POINT ( 'NONE',  ( 41.15573334512143333, 1434.647116362632005, 269.6315103028593398 ) ) ;
#11601 = CIRCLE ( 'NONE', #54557, 10.71315034250000053 ) ;
#11602 = CARTESIAN_POINT ( 'NONE',  ( 9.396366832618360476, 1435.725902782769936, 209.1467788222589945 ) ) ;
#11603 = CARTESIAN_POINT ( 'NONE',  ( -109.8051728760000003, 1384.892702632449982, 297.0523066442589766 ) ) ;
#11604 = DIRECTION ( 'NONE',  ( -0.4794255386042071132, 0.000000000000000000, 0.8775825618903705383 ) ) ;
#11605 = CARTESIAN_POINT ( 'NONE',  ( 12.18971934853500194, 1512.123542805230272, 223.8476153537669973 ) ) ;
#11606 = CARTESIAN_POINT ( 'NONE',  ( 6.453500081109999620, 1409.641075296729923, 187.1560900367980196 ) ) ;
#11607 = CYLINDRICAL_SURFACE ( 'NONE', #108989, 1.999999999999999556 ) ;
#11609 = CARTESIAN_POINT ( 'NONE',  ( -10.83341047090000053, 1434.513252305289825, 151.9041012880979906 ) ) ;
#11608 = VECTOR ( 'NONE', #106016, 1000.000000000000000 ) ;
#11610 = DIRECTION ( 'NONE',  ( 0.000000000000000000, 1.000000000000000000, 0.000000000000000000 ) ) ;
#11611 = CARTESIAN_POINT ( 'NONE',  ( -9.656448545818989260, 1479.372503699150002, 215.7269582878559788 ) ) ;
#11612 = AXIS2_PLACEMENT_3D ( 'NONE', #51948, #93374, #84968 ) ;
#11613 = CARTESIAN_POINT ( 'NONE',  ( -19.40246366119999877, 1452.235511427830033, 144.9801693602979640 ) ) ;
#11615 = EDGE_LOOP ( 'NONE', ( #99012, #47048, #100284, #53687 ) ) ;
#11614 = DIRECTION ( 'NONE',  ( 0.1867471702549220458, -2.391457216852619248E-16, -0.9824080081115885710 ) ) ;
#11616 = EDGE_LOOP ( 'NONE', ( #34097, #91233, #54486, #103055, #21866, #102196 ) ) ;
#11617 = FACE_OUTER_BOUND ( 'NONE', #99222, .T. ) ;
#11618 = CARTESIAN_POINT ( 'NONE',  ( 9.662212368149999620, 1493.993336057090119, 188.1975001349989896 ) ) ;
#11619 = CARTESIAN_POINT ( 'NONE',  ( -29.18142758420000149, 1466.479558604430167, 269.9486951468979896 ) ) ;
#11620 = CARTESIAN_POINT ( 'NONE',  ( -23.91170749936344464, 1435.927394111685089, 211.3044503123053914 ) ) ;
#11621 = CARTESIAN_POINT ( 'NONE',  ( 11.94206337009999963, 1438.199233188169956, 150.9847479746979957 ) ) ;
#11622 = CARTESIAN_POINT ( 'NONE',  ( -23.10442739037580040, 1411.095127590459924, 210.9251608898400150 ) ) ;
#11623 = CARTESIAN_POINT ( 'NONE',  ( -32.02808312589930040, 1522.382868172863937, 198.2787714533499752 ) ) ;
#11624 = CARTESIAN_POINT ( 'NONE',  ( 18.48251015503148764, 1457.399406872058989, 229.7677033836061185 ) ) ;
#11625 = CARTESIAN_POINT ( 'NONE',  ( -8.539526853489999070, 1458.917133117889762, 213.6780174602090199 ) ) ;
#11626 = CARTESIAN_POINT ( 'NONE',  ( 7.340269731169999368, 1361.836778001489847, 207.6218459616989946 ) ) ;
#11627 = CARTESIAN_POINT ( 'NONE',  ( -45.36516505088270179, 1434.423077423250106, 268.2311484050200079 ) ) ;
#11628 = ORIENTED_EDGE ( 'NONE', *, *, #63222, .T. ) ;
#11629 = CARTESIAN_POINT ( 'NONE',  ( -7.982037141949999359, 1424.874072662569915, 210.5243721551090061 ) ) ;
#11630 = ORIENTED_EDGE ( 'NONE', *, *, #68499, .T. ) ;
#11631 = CARTESIAN_POINT ( 'NONE',  ( 6.951517132375000685, 1517.194816588360027, 210.2467400204669730 ) ) ;
#11632 = CARTESIAN_POINT ( 'NONE',  ( 5.513435553965000402, 1508.551704408389924, 202.1089243864769855 ) ) ;
#11633 = CARTESIAN_POINT ( 'NONE',  ( -20.86040077539999871, 1508.959081886430113, 190.3921826422979962 ) ) ;
#11634 = CARTESIAN_POINT ( 'NONE',  ( -15.31473337059999906, 1410.405885239830013, 190.9489869040980068 ) ) ;
#11635 = CARTESIAN_POINT ( 'NONE',  ( -24.89775034519999863, 1442.835538705840008, 210.5176537872779932 ) ) ;
#11636 = ORIENTED_EDGE ( 'NONE', *, *, #75415, .F. ) ;
#11637 = CARTESIAN_POINT ( 'NONE',  ( 0.4834647446390000214, 1450.896177426419854, 181.9315483554979949 ) ) ;
#11638 = CIRCLE ( 'NONE', #104594, 4.941741911590025182 ) ;
#11639 = CARTESIAN_POINT ( 'NONE',  ( 3.453544825624999870, 1517.106845464700200, 201.7850012896870169 ) ) ;
#11640 = DIRECTION ( 'NONE',  ( 0.03489949670244908014, -0.9993908270190976495, 0.000000000000000000 ) ) ;
#11642 = AXIS2_PLACEMENT_3D ( 'NONE', #26209, #10532, #11099 ) ;
#11641 = CARTESIAN_POINT ( 'NONE',  ( -9.293376658228730491, 1440.013600069829863, 206.7969830623249834 ) ) ;
#11643 = ORIENTED_EDGE ( 'NONE', *, *, #56349, .T. ) ;
#11644 = CARTESIAN_POINT ( 'NONE',  ( -9.792171405701560971, 1409.347304102430144, 270.4184784957810734 ) ) ;
#11645 = CARTESIAN_POINT ( 'NONE',  ( 0.7402208603880020554, 1516.992029636990083, 208.3685455796920110 ) ) ;
#11646 = CARTESIAN_POINT ( 'NONE',  ( 3.519941190947349696, 1417.854933870999957, 233.1899663063400112 ) ) ;
#11647 = FACE_OUTER_BOUND ( 'NONE', #7794, .T. ) ;
#11649 = ORIENTED_EDGE ( 'NONE', *, *, #81444, .T. ) ;
#11648 = CARTESIAN_POINT ( 'NONE',  ( -8.624710350826600092, 1367.191948709382132, 210.6218459616987957 ) ) ;
#11650 = ORIENTED_EDGE ( 'NONE', *, *, #35181, .F. ) ;
#11651 = CARTESIAN_POINT ( 'NONE',  ( 45.58093450282833459, 1442.609263607555022, 268.9762866484336996 ) ) ;
#11652 = EDGE_CURVE ( 'NONE', #94335, #100110, #1974, .T. ) ;
#11653 = CARTESIAN_POINT ( 'NONE',  ( 0.9773820611809029835, 1467.205418092640002, 220.1532616540179959 ) ) ;
#11654 = CARTESIAN_POINT ( 'NONE',  ( 3.628618679598039076, 1424.505256609078970, 184.4894892356298328 ) ) ;
#11655 = CARTESIAN_POINT ( 'NONE',  ( -0.001500122192890200124, 1408.913112772820114, 186.4349499642330272 ) ) ;
#11656 = B_SPLINE_SURFACE_WITH_KNOTS ( 'NONE', 5, 1, ( 
 ( #28199, #62386 ),
 ( #105466, #88126 ),
 ( #11415, #3032 ),
 ( #54540, #106023 ),
 ( #19217, #37158 ),
 ( #53419, #28755 ) ),
 .UNSPECIFIED., .F., .F., .F.,
 ( 6, 6 ),
 ( 2, 2 ),
 ( 0.000000000000000000, 3.472809815250000209 ),
 ( 0.000000000000000000, 14.00000000000000000 ),
 .UNSPECIFIED. ) ;
#11657 = CARTESIAN_POINT ( 'NONE',  ( -18.68599070930379824, 1416.029511582830082, 207.5720217176579752 ) ) ;
#11658 = CARTESIAN_POINT ( 'NONE',  ( 2.500000000000000000, 1439.114301455650093, 157.7261946041980138 ) ) ;
#11659 = CARTESIAN_POINT ( 'NONE',  ( -14.30536636630000125, 1420.164009348430000, 221.8419782042979875 ) ) ;
#11660 = CARTESIAN_POINT ( 'NONE',  ( 12.60885230210000074, 1416.021639796329964, 222.8465216075979924 ) ) ;
#11661 = CARTESIAN_POINT ( 'NONE',  ( 9.350144766380001471, 1445.503299043049992, 184.2959263576980220 ) ) ;
#11662 = CARTESIAN_POINT ( 'NONE',  ( -0.01327257453019850021, 1516.940252185109784, 206.2479269295770052 ) ) ;
#11663 = ORIENTED_EDGE ( 'NONE', *, *, #71431, .F. ) ;
#11664 = CARTESIAN_POINT ( 'NONE',  ( 3.357570129570000450, 1437.173063345790069, 227.3648210081989873 ) ) ;
#11665 = CARTESIAN_POINT ( 'NONE',  ( 1.513134720104279962, 1459.713768463400129, 183.1823380342580094 ) ) ;
#11666 = ORIENTED_EDGE ( 'NONE', *, *, #45955, .T. ) ;
#11667 = CARTESIAN_POINT ( 'NONE',  ( 17.79624440539630470, 1458.182673695933318, 228.6901989447007679 ) ) ;
#11668 = CARTESIAN_POINT ( 'NONE',  ( 24.26879693951600103, 1452.060463742079946, 136.4940726181909838 ) ) ;
#11669 = CARTESIAN_POINT ( 'NONE',  ( 16.19492570339999915, 1409.478599654730033, 224.8086529783979870 ) ) ;
#11670 = CARTESIAN_POINT ( 'NONE',  ( -28.25951253750000092, 1389.755799385790169, 221.3495615508589935 ) ) ;
#11671 = CARTESIAN_POINT ( 'NONE',  ( -14.28029386204369899, 1390.367275669339961, 209.8449220790990069 ) ) ;
#11672 = CARTESIAN_POINT ( 'NONE',  ( 21.49042858359999641, 1409.827641821229918, 203.4051265432880200 ) ) ;
#11673 = CARTESIAN_POINT ( 'NONE',  ( 12.29654148988069373, 1445.052233488290085, 164.4841150006940325 ) ) ;
#11674 = CARTESIAN_POINT ( 'NONE',  ( 3.356639108386120895, 1439.689563386633836, 184.4108225802596053 ) ) ;
#11675 = CARTESIAN_POINT ( 'NONE',  ( 11.30915027500000036, 1490.769366722990071, 205.5036971762389726 ) ) ;
#11676 = CARTESIAN_POINT ( 'NONE',  ( 21.67251142306619016, 1453.432672215584944, 220.8666736850036614 ) ) ;
#11677 = CARTESIAN_POINT ( 'NONE',  ( 2.500000000000000000, 1439.481493058779961, 163.2933130068350067 ) ) ;
#11678 = CARTESIAN_POINT ( 'NONE',  ( -2.483322492024999661, 1517.139039350860003, 215.6851008610869940 ) ) ;
#11679 = CARTESIAN_POINT ( 'NONE',  ( 2.664386649655714479, 1523.844782250841263, 242.1314419845511452 ) ) ;
#11680 = ORIENTED_EDGE ( 'NONE', *, *, #13962, .T. ) ;
#11681 = CYLINDRICAL_SURFACE ( 'NONE', #70614, 4.000000000000000888 ) ;
#11682 = CARTESIAN_POINT ( 'NONE',  ( 21.19880661589004589, 1526.382868172863937, 233.5487980989310870 ) ) ;
#11683 = CARTESIAN_POINT ( 'NONE',  ( -0.5147827871106269715, 1410.238466821279872, 233.1669068061830217 ) ) ;
#11684 = EDGE_CURVE ( 'NONE', #59426, #4978, #2148, .T. ) ;
#11685 = FACE_OUTER_BOUND ( 'NONE', #17840, .T. ) ;
#11686 = AXIS2_PLACEMENT_3D ( 'NONE', #91042, #23827, #15973 ) ;
#11687 = EDGE_CURVE ( 'NONE', #12956, #71433, #3015, .T. ) ;
#11688 = CARTESIAN_POINT ( 'NONE',  ( -40.06635116240170191, 1445.481206507490015, 136.8845248586889909 ) ) ;
#11689 = ADVANCED_FACE ( 'NONE', ( #25058 ), #15551, .T. ) ;
#11690 = CARTESIAN_POINT ( 'NONE',  ( -4.327853128026350582, 1515.125728221830059, 208.3398689723839823 ) ) ;
#11691 = FACE_OUTER_BOUND ( 'NONE', #3679, .T. ) ;
#11692 = CARTESIAN_POINT ( 'NONE',  ( 40.83414858899995892, 1456.643249355430044, 266.3275291775977962 ) ) ;
#11693 = ADVANCED_FACE ( 'NONE', ( #25613 ), #59805, .F. ) ;
#11694 = CARTESIAN_POINT ( 'NONE',  ( 11.87081876380000089, 1433.087150165419871, 150.2039343203979911 ) ) ;
#11695 = CARTESIAN_POINT ( 'NONE',  ( -44.92381742691460289, 1442.155912586060140, 269.6913903957949969 ) ) ;
#11696 = B_SPLINE_SURFACE_WITH_KNOTS ( 'NONE', 5, 4, ( 
 ( #107388, #37994, #64871, #97877, #89491 ),
 ( #81626, #23377, #90030, #39645, #82186 ),
 ( #106831, #100097, #5485, #30124, #22809 ),
 ( #98436, #29577, #98979, #22253, #46964 ),
 ( #73814, #38529, #81085, #21707, #55912 ),
 ( #107942, #57568, #21154, #31234, #40188 ) ),
 .UNSPECIFIED., .F., .F., .F.,
 ( 6, 6 ),
 ( 5, 5 ),
 ( -0.0001726411652746099863, 52.98902693510000006 ),
 ( 25.78146411700000229, 39.23969207129999859 ),
 .UNSPECIFIED. ) ;
#11697 = CARTESIAN_POINT ( 'NONE',  ( -17.84692692827389848, 1410.032954271290237, 195.3924044303319931 ) ) ;
#11698 = CARTESIAN_POINT ( 'NONE',  ( 2.086548178679999754, 1515.551704408389924, 212.9514660752490158 ) ) ;
#11699 = ORIENTED_EDGE ( 'NONE', *, *, #42172, .F. ) ;
#11700 = DIRECTION ( 'NONE',  ( -1.224646799147353207E-16, -6.123233995736769734E-17, -1.000000000000000000 ) ) ;
#11701 = CYLINDRICAL_SURFACE ( 'NONE', #46238, 1.999999999999999556 ) ;
#11702 = CARTESIAN_POINT ( 'NONE',  ( -2.343308028451718261, 1485.565572280186416, 182.6780017704854515 ) ) ;
#11703 = CARTESIAN_POINT ( 'NONE',  ( 5.527464195969298721, 1398.076716713788755, 197.3337701784347473 ) ) ;
#11704 = CARTESIAN_POINT ( 'NONE',  ( 1.921481516869999906, 1474.709560945429985, 234.8855729059979751 ) ) ;
#11705 = CARTESIAN_POINT ( 'NONE',  ( 25.55495559159999885, 1449.803351295099901, 210.4363185493679964 ) ) ;
#11706 = CARTESIAN_POINT ( 'NONE',  ( -16.29090474523583154, 1420.160629993541534, 209.0771752386399953 ) ) ;
#11707 = DIRECTION ( 'NONE',  ( -1.000000000000000000, -1.944759044220000059E-14, -3.085874980950000024E-15 ) ) ;
#11708 = CARTESIAN_POINT ( 'NONE',  ( -30.09804076777400184, 1383.841955765280090, 227.9062932389740297 ) ) ;
#11709 = AXIS2_PLACEMENT_3D ( 'NONE', #89745, #23072, #5188 ) ;
#11710 = CARTESIAN_POINT ( 'NONE',  ( -3.273040579383169835, 1508.551704408389924, 204.1347629179929868 ) ) ;
#11711 = CARTESIAN_POINT ( 'NONE',  ( 2.499937872101899661, 1420.083820293880080, 95.10876171418870229 ) ) ;
#11712 = EDGE_CURVE ( 'NONE', #31615, #61519, #108480, .T. ) ;
#11713 = CARTESIAN_POINT ( 'NONE',  ( -14.93718008229999938, 1416.181292664740113, 212.9156384192889959 ) ) ;
#11714 = CARTESIAN_POINT ( 'NONE',  ( -2.330134126090000368, 1515.064792882589927, 204.7923971856590128 ) ) ;
#11716 = VERTEX_POINT ( 'NONE', #102327 ) ;
#11715 = CARTESIAN_POINT ( 'NONE',  ( -6.259455327080631015, 1439.877182118289738, 154.4997780959237446 ) ) ;
#11717 = CARTESIAN_POINT ( 'NONE',  ( -1.114904039080000020, 1451.704834585230174, 183.4401667605979753 ) ) ;
#11718 = CARTESIAN_POINT ( 'NONE',  ( -9.039250672204644843, 1388.268641467896032, 200.6155552593253617 ) ) ;
#11719 = CARTESIAN_POINT ( 'NONE',  ( -20.01067139950000140, 1507.877425041529932, 188.9709217985979706 ) ) ;
#11721 = VERTEX_POINT ( 'NONE', #91731 ) ;
#11720 = CARTESIAN_POINT ( 'NONE',  ( -31.14814639457161860, 1525.697947650476863, 216.7341144156438020 ) ) ;
#11722 = CARTESIAN_POINT ( 'NONE',  ( -6.951511259182890257, 1508.551704405770124, 219.1997712163169751 ) ) ;
#11723 = VERTEX_POINT ( 'NONE', #15004 ) ;
#11724 = EDGE_CURVE ( 'NONE', #67299, #62781, #37687, .T. ) ;
#11725 = AXIS2_PLACEMENT_3D ( 'NONE', #65390, #40713, #16039 ) ;
#11726 = CARTESIAN_POINT ( 'NONE',  ( -9.612506535307179689, 1386.943031418069950, 218.1121965012910096 ) ) ;
#11727 = CARTESIAN_POINT ( 'NONE',  ( 4.172675962690000517, 1490.591284869190076, 188.6582191385990086 ) ) ;
#11728 = CARTESIAN_POINT ( 'NONE',  ( 3.340336038346551906, 1485.759119865504999, 219.3558821538616996 ) ) ;
#11729 = ADVANCED_FACE ( 'NONE', ( #1009 ), #75827, .T. ) ;
#11730 = DIRECTION ( 'NONE',  ( -0.3026086614614409420, 0.3677779883867259847, -0.8792993513398769112 ) ) ;
#11731 = CARTESIAN_POINT ( 'NONE',  ( -1.602167524609999782, 1430.706703968889997, 217.3531761583190018 ) ) ;
#11732 = CARTESIAN_POINT ( 'NONE',  ( -10.07154918488590134, 1473.228065907060000, 207.4129428866500007 ) ) ;
#11733 = CARTESIAN_POINT ( 'NONE',  ( 9.512845714357990090, 1409.245256277939916, 220.6667643274379884 ) ) ;
#11734 = CARTESIAN_POINT ( 'NONE',  ( 18.12493657479999953, 1425.163099838030121, 224.8025639441979990 ) ) ;
#11735 = CARTESIAN_POINT ( 'NONE',  ( -97.02964055224740036, 1385.213118710479876, 295.5936257578139816 ) ) ;
#11736 = CARTESIAN_POINT ( 'NONE',  ( 3.347801439296141268, 1518.913060387330006, 242.0893193391992497 ) ) ;
#11737 = CARTESIAN_POINT ( 'NONE',  ( 9.912698782267559849, 1426.220931725540140, 209.0671000446980088 ) ) ;
#11738 = CARTESIAN_POINT ( 'NONE',  ( 11.21226529693919893, 1490.925921770189916, 206.9374627972229916 ) ) ;
#11739 = ORIENTED_EDGE ( 'NONE', *, *, #78509, .F. ) ;
#11740 = ORIENTED_EDGE ( 'NONE', *, *, #16426, .T. ) ;
#11741 = CARTESIAN_POINT ( 'NONE',  ( -11.94473499059260213, 1415.666200591949973, 194.9815815898240032 ) ) ;
#11742 = CARTESIAN_POINT ( 'NONE',  ( -2.750440272224420113, 1495.796400148049997, 197.0976659292670092 ) ) ;
#11743 = CARTESIAN_POINT ( 'NONE',  ( 29.85894071568812080, 1462.352465317911765, 269.4693070817808689 ) ) ;
#11744 = CARTESIAN_POINT ( 'NONE',  ( -31.69312280309771879, 1525.713797967456685, 221.9404206525577479 ) ) ;
#11745 = CARTESIAN_POINT ( 'NONE',  ( 3.320518013340000074, 1396.029015431430025, 219.7196859380979959 ) ) ;
#11746 = CARTESIAN_POINT ( 'NONE',  ( 1.363639811660000145, 1415.765555525229956, 232.8698637559979829 ) ) ;
#11747 = CARTESIAN_POINT ( 'NONE',  ( -0.5186190627380000695, 1457.272028348329968, 183.0645885489979889 ) ) ;
#11748 = CARTESIAN_POINT ( 'NONE',  ( -9.936738324559998503, 1364.340818343090177, 207.6218459616989946 ) ) ;
#11749 = CARTESIAN_POINT ( 'NONE',  ( -6.025152189795589308, 1484.743689720570046, 198.8560543189699956 ) ) ;
#11750 = CARTESIAN_POINT ( 'NONE',  ( 2.864043418315000089, 1516.811292230880099, 206.8228319013669818 ) ) ;
#11751 = CARTESIAN_POINT ( 'NONE',  ( 8.013264357029996177, 1375.413060387289988, 209.1218459572589836 ) ) ;
#11752 = CARTESIAN_POINT ( 'NONE',  ( -8.295657568419999350, 1385.027123149139925, 218.7016715734189916 ) ) ;
#11753 = CARTESIAN_POINT ( 'NONE',  ( 0.5624686996209999901, 1416.828044802929981, 190.4759595091980202 ) ) ;
#11754 = CARTESIAN_POINT ( 'NONE',  ( 22.08622291482350519, 1523.382868172864164, 233.8253038720783366 ) ) ;
#11755 = CARTESIAN_POINT ( 'NONE',  ( -7.071828507238460126, 1490.865216771150017, 189.3536562381210047 ) ) ;
#11756 = PRODUCT_DEFINITION ( 'UNKNOWN', '', #20769, #12102 ) ;
#11757 = CARTESIAN_POINT ( 'NONE',  ( 32.85805783624304155, 1523.678648413191695, 201.0453875934054508 ) ) ;
#11758 = EDGE_LOOP ( 'NONE', ( #4939, #88177, #19008, #18202 ) ) ;
#11759 = CARTESIAN_POINT ( 'NONE',  ( 6.248994650120000216, 1409.477337451929998, 259.9484463607980160 ) ) ;
#11760 = CARTESIAN_POINT ( 'NONE',  ( -23.81087019679999628, 1469.236087444030090, 199.7892800214279987 ) ) ;
#11763 = CARTESIAN_POINT ( 'NONE',  ( 14.38276615812612036, 1514.413060387330006, 235.4493228184091720 ) ) ;
#11762 = AXIS2_PLACEMENT_3D ( 'NONE', #58510, #24327, #15914 ) ;
#11761 = CARTESIAN_POINT ( 'NONE',  ( -11.01664542227860011, 1426.516231295739999, 91.95526548305120684 ) ) ;
#11764 = CARTESIAN_POINT ( 'NONE',  ( -43.48931973434065412, 1430.236537677061960, 269.7109761710999010 ) ) ;
#11765 = CARTESIAN_POINT ( 'NONE',  ( 2.451862795619999984E-09, 1414.987262868229891, 244.5742075744979900 ) ) ;
#11766 = FACE_OUTER_BOUND ( 'NONE', #4069, .T. ) ;
#11767 = CARTESIAN_POINT ( 'NONE',  ( 4.291176059336820003, 1446.971469614359876, 154.7965853925720126 ) ) ;
#11768 = CARTESIAN_POINT ( 'NONE',  ( -23.30842551276433738, 1409.842257829955088, 208.8031236852703785 ) ) ;
#11769 = EDGE_LOOP ( 'NONE', ( #74157, #48865, #37120, #29459 ) ) ;
#11770 = DIRECTION ( 'NONE',  ( -1.755985294532469921E-16, 1.000000000000000000, -1.338183447452831989E-16 ) ) ;
#11771 = CARTESIAN_POINT ( 'NONE',  ( 14.75869785433269676, 1514.537600265056653, 225.3978362136949158 ) ) ;
#11772 = CARTESIAN_POINT ( 'NONE',  ( -4.270716320095258922, 1515.320037165259464, 206.7917118365956242 ) ) ;
#11773 = EDGE_LOOP ( 'NONE', ( #35034, #34518, #93968, #49616, #91655 ) ) ;
#11774 = ORIENTED_EDGE ( 'NONE', *, *, #64378, .F. ) ;
#11775 = CARTESIAN_POINT ( 'NONE',  ( -25.91644647850000283, 1384.822840952090019, 203.4460669693289958 ) ) ;
#11776 = CARTESIAN_POINT ( 'NONE',  ( 5.982479193689999697, 1424.279491935699980, 194.0293373055990003 ) ) ;
#11777 = EDGE_CURVE ( 'NONE', #92278, #108598, #77743, .T. ) ;
#11778 = ORIENTED_EDGE ( 'NONE', *, *, #59297, .T. ) ;
#11779 = CARTESIAN_POINT ( 'NONE',  ( 0.4959747488679999705, 1415.645648335029819, 184.8436836604979874 ) ) ;
#11780 = DIRECTION ( 'NONE',  ( -0.8090169943749465631, 0.000000000000000000, 0.5877852522924742473 ) ) ;
#11781 = EDGE_CURVE ( 'NONE', #99658, #46627, #107438, .T. ) ;
#11782 = CARTESIAN_POINT ( 'NONE',  ( 0.4808923648170000398, 1450.896267255910061, 181.2821022293979922 ) ) ;
#11783 = CARTESIAN_POINT ( 'NONE',  ( -4.734919033409999756, 1489.058994670830089, 235.5547056775980082 ) ) ;
#11784 = CARTESIAN_POINT ( 'NONE',  ( 1.668736474052739949, 1443.775022403490084, 200.3211312882999948 ) ) ;
#11785 = VERTEX_POINT ( 'NONE', #10920 ) ;
#11786 = CIRCLE ( 'NONE', #85066, 0.5000000000000004441 ) ;
#11787 = FACE_OUTER_BOUND ( 'NONE', #16017, .T. ) ;
#11788 = CARTESIAN_POINT ( 'NONE',  ( -13.15726448930059966, 1414.913060387399810, 219.9105443326110105 ) ) ;
#11789 = CARTESIAN_POINT ( 'NONE',  ( 14.10003875770000015, 1474.744286201729892, 225.3785174790980079 ) ) ;
#11790 = ORIENTED_EDGE ( 'NONE', *, *, #18010, .F. ) ;
#11791 =( BOUNDED_CURVE ( )  B_SPLINE_CURVE ( 3, ( #53001, #79298, #36734, #19917 ),
 .UNSPECIFIED., .F., .F. ) 
 B_SPLINE_CURVE_WITH_KNOTS ( ( 4, 4 ),
 ( 0.2461548770693000043, 0.5332284340196910000 ),
 .UNSPECIFIED. ) 
 CURVE ( )  GEOMETRIC_REPRESENTATION_ITEM ( )  RATIONAL_B_SPLINE_CURVE ( ( 1.000000000000000000, 0.9931441806372443004, 0.9931441806372443004, 1.000000000000000000 ) ) 
 REPRESENTATION_ITEM ( '' )  );
#11792 = CARTESIAN_POINT ( 'NONE',  ( -6.946748557085000719, 1516.983995446890049, 204.1186252050270014 ) ) ;
#11793 = ORIENTED_EDGE ( 'NONE', *, *, #103442, .F. ) ;
#11794 = CARTESIAN_POINT ( 'NONE',  ( 11.85058003275609906, 1431.258819511150023, 149.8778382379539948 ) ) ;
#11795 = EDGE_CURVE ( 'NONE', #51888, #90510, #50240, .T. ) ;
#11796 = CARTESIAN_POINT ( 'NONE',  ( 5.258165198517999350, 1511.418041552836030, 217.7311153980011795 ) ) ;
#11797 = ORIENTED_EDGE ( 'NONE', *, *, #95331, .F. ) ;
#11798 = ORIENTED_EDGE ( 'NONE', *, *, #57038, .T. ) ;
#11799 = CARTESIAN_POINT ( 'NONE',  ( 0.7800921441517267851, 1526.382868172863937, 176.7869413415625388 ) ) ;
#11800 = CARTESIAN_POINT ( 'NONE',  ( -4.802733161482000135, 1508.515565345379855, 220.0795834517809908 ) ) ;
#11801 = CARTESIAN_POINT ( 'NONE',  ( 6.266043415252799953, 1498.127554395540074, 198.6678067497960001 ) ) ;
#11802 = VECTOR ( 'NONE', #76260, 1000.000000000000000 ) ;
#11803 = CARTESIAN_POINT ( 'NONE',  ( -2.651145353956480211, 1469.068394821650145, 218.9699912446779990 ) ) ;
#11804 = CARTESIAN_POINT ( 'NONE',  ( 17.43092393268590001, 1452.304359110679798, 145.9286196276850092 ) ) ;
#11805 = CARTESIAN_POINT ( 'NONE',  ( 4.281468235900000252, 1408.076772451330044, 270.2892484966980078 ) ) ;
#11806 = CARTESIAN_POINT ( 'NONE',  ( 9.203495734806530493, 1450.275870452079971, 208.6687953531569804 ) ) ;
#11807 = CARTESIAN_POINT ( 'NONE',  ( -5.584029160970000127, 1475.430779401290010, 200.4113593926190049 ) ) ;
#11808 = CARTESIAN_POINT ( 'NONE',  ( -2.418619436219159979, 1422.249129387939774, 192.8987411397049812 ) ) ;
#11809 = CARTESIAN_POINT ( 'NONE',  ( -21.02559120289207684, 1509.697962614031894, 230.2053966973059005 ) ) ;
#11810 = DIRECTION ( 'NONE',  ( -0.9996573249755517088, -0.02617694830808747070, 0.000000000000000000 ) ) ;
#11812 = CARTESIAN_POINT ( 'NONE',  ( 14.93446018370000061, 1453.159462792729983, 195.2131447753980069 ) ) ;
#11811 = CARTESIAN_POINT ( 'NONE',  ( -13.54316952090000115, 1502.948981525290037, 209.0729592470459863 ) ) ;
#11813 = CARTESIAN_POINT ( 'NONE',  ( -68.19307365517850883, 1379.747659725522226, 279.6816280296294508 ) ) ;
#11814 = CARTESIAN_POINT ( 'NONE',  ( 17.84432149610639939, 1418.606169056330145, 225.0325621462739889 ) ) ;
#11815 = CARTESIAN_POINT ( 'NONE',  ( -6.372167638684999247, 1511.069621805459974, 201.7253008889670127 ) ) ;
#11816 = ORIENTED_EDGE ( 'NONE', *, *, #24856, .T. ) ;
#11817 = CARTESIAN_POINT ( 'NONE',  ( 40.73184307449999864, 1440.913060387330006, 268.3665355201979992 ) ) ;
#11818 = CARTESIAN_POINT ( 'NONE',  ( 21.84020450222037724, 1523.481610426287489, 183.2638850454218016 ) ) ;
#11819 = CARTESIAN_POINT ( 'NONE',  ( -71.28004258136559201, 1385.019770350649878, 296.4666894103959862 ) ) ;
#11820 = CARTESIAN_POINT ( 'NONE',  ( 18.29188182340000068, 1431.768652859389704, 209.1218459616989946 ) ) ;
#11821 = EDGE_CURVE ( 'NONE', #51048, #10343, #96385, .T. ) ;
#11822 = CARTESIAN_POINT ( 'NONE',  ( 4.664268937930000192, 1505.247554523090002, 221.0077437511990013 ) ) ;
#11823 = CARTESIAN_POINT ( 'NONE',  ( -14.75858103010000022, 1415.739699867389845, 212.8702772392690292 ) ) ;
#11825 = ORIENTED_EDGE ( 'NONE', *, *, #46098, .F. ) ;
#11824 = CARTESIAN_POINT ( 'NONE',  ( -16.66302441916570132, 1420.069697476050123, 208.3115331456619970 ) ) ;
#11826 = ADVANCED_FACE ( 'NONE', ( #46746 ), #107019, .T. ) ;
#11827 = CARTESIAN_POINT ( 'NONE',  ( -15.75920964212049569, 1415.789874363079662, 209.6894149795170961 ) ) ;
#11828 = CARTESIAN_POINT ( 'NONE',  ( -24.43616533349999997, 1442.711518362400284, 211.0968143008180107 ) ) ;
#11829 = CARTESIAN_POINT ( 'NONE',  ( -11.73709356400000026, 1426.695943121429991, 144.1748013713979901 ) ) ;
#11830 = CARTESIAN_POINT ( 'NONE',  ( 29.75012120190000076, 1509.993914123429931, 209.6841247587719863 ) ) ;
#11831 = CARTESIAN_POINT ( 'NONE',  ( 14.96248396073499976, 1513.868118914750085, 224.3717980193670201 ) ) ;
#11832 = CARTESIAN_POINT ( 'NONE',  ( 4.370200466702017117, 1370.450046576546811, 208.7619599720994472 ) ) ;
#11833 = CARTESIAN_POINT ( 'NONE',  ( 19.20880922570000138, 1509.714298116030022, 184.5747400720979954 ) ) ;
#11834 = CARTESIAN_POINT ( 'NONE',  ( 2.672403418599419656, 1457.264926085269963, 199.5268423672170286 ) ) ;
#11835 = CARTESIAN_POINT ( 'NONE',  ( 21.62164173326539895, 1522.051704408389924, 208.0273405521070060 ) ) ;
#11836 = CARTESIAN_POINT ( 'NONE',  ( 16.36321488700000160, 1415.089959694529853, 226.8952736679979978 ) ) ;
#11837 = EDGE_CURVE ( 'NONE', #23316, #93351, #82626, .T. ) ;
#11838 = CARTESIAN_POINT ( 'NONE',  ( -7.982037141949999359, 1424.874072662569915, 210.5243721551090061 ) ) ;
#11839 = CARTESIAN_POINT ( 'NONE',  ( -15.72949124279999999, 1459.406586711229920, 229.6279973257979918 ) ) ;
#11840 = CARTESIAN_POINT ( 'NONE',  ( -6.951175166914999259, 1517.170721208160103, 206.8315896683770063 ) ) ;
#11841 = CARTESIAN_POINT ( 'NONE',  ( 46.16776989860000668, 1440.913083889750169, 266.9714971360980371 ) ) ;
#11842 = CARTESIAN_POINT ( 'NONE',  ( -17.64143905099999898, 1409.529113013930100, 222.5042051235980125 ) ) ;
#11843 = CARTESIAN_POINT ( 'NONE',  ( 20.53228480110000120, 1435.642735894570023, 144.3848875112979897 ) ) ;
#11844 = CARTESIAN_POINT ( 'NONE',  ( 20.37750482680000275, 1488.586794206330069, 191.0822492793979848 ) ) ;
#11845 = EDGE_CURVE ( 'NONE', #68424, #53112, #13539, .T. ) ;
#11846 = CARTESIAN_POINT ( 'NONE',  ( 5.383702537648559883, 1431.669030977889861, 154.5771441291960286 ) ) ;
#11847 = CARTESIAN_POINT ( 'NONE',  ( 4.687651746879999415, 1478.378160227390254, 228.9010599218989910 ) ) ;
#11848 = CARTESIAN_POINT ( 'NONE',  ( -16.04920218319999847, 1423.363755928130104, 227.1130481936980061 ) ) ;
#11849 = CARTESIAN_POINT ( 'NONE',  ( 12.59194315185039947, 1426.976044800900127, 205.9677913843619876 ) ) ;
#11850 = CARTESIAN_POINT ( 'NONE',  ( -40.03876954321400206, 1439.602033950459827, 136.4880915068820002 ) ) ;
#11851 = CARTESIAN_POINT ( 'NONE',  ( -10.74459946700000046, 1409.109315431730010, 199.8441821536079885 ) ) ;
#11852 = CARTESIAN_POINT ( 'NONE',  ( -16.28543887299999682, 1416.852015342750065, 207.9358373243390190 ) ) ;
#11853 = CARTESIAN_POINT ( 'NONE',  ( -17.05103801767675265, 1409.778322827861302, 193.4350317778312842 ) ) ;
#11854 = CARTESIAN_POINT ( 'NONE',  ( -7.769784805680000517, 1383.283764732429972, 218.8591787099389876 ) ) ;
#11855 = CARTESIAN_POINT ( 'NONE',  ( 13.19909928449999903, 1434.900406568759763, 146.5971321357980059 ) ) ;
#11856 = CARTESIAN_POINT ( 'NONE',  ( -32.76525568849999814, 1436.117894521449898, 136.3349802012980092 ) ) ;
#11857 = CARTESIAN_POINT ( 'NONE',  ( -8.095121878198867194, 1456.266568741559013, 227.2460153072438516 ) ) ;
#11858 = VERTEX_POINT ( 'NONE', #74142 ) ;
#11859 = CARTESIAN_POINT ( 'NONE',  ( 6.164039417708820245, 1510.821818217313648, 216.5878453126418037 ) ) ;
#11860 = CARTESIAN_POINT ( 'NONE',  ( 8.742163716520650412E-12, 1408.913060387359792, 224.1216835645979870 ) ) ;
#11861 = DIRECTION ( 'NONE',  ( 0.8090169943749466741, 0.000000000000000000, -0.5877852522924743583 ) ) ;
#11862 = EDGE_CURVE ( 'NONE', #27986, #92844, #105715, .T. ) ;
#11863 = CARTESIAN_POINT ( 'NONE',  ( -5.506664947740000038, 1440.093543047909861, 154.7592479031980019 ) ) ;
#11864 = DIRECTION ( 'NONE',  ( 0.000000000000000000, 1.000000000000000000, 0.000000000000000000 ) ) ;
#11865 = CARTESIAN_POINT ( 'NONE',  ( -29.91790837370000133, 1467.081768096229780, 269.1810262515979844 ) ) ;
#11866 = CARTESIAN_POINT ( 'NONE',  ( -30.00906612069109869, 1525.856065479233393, 197.1249957521959288 ) ) ;
#11867 = CARTESIAN_POINT ( 'NONE',  ( 0.1632388131350529792, 1420.111806197110127, 183.8575883265500295 ) ) ;
#11868 = EDGE_CURVE ( 'NONE', #27986, #58087, #58434, .T. ) ;
#11869 = CARTESIAN_POINT ( 'NONE',  ( 2.500000000000039968, 1439.615672328189930, 182.7715275322960053 ) ) ;
#11870 = CARTESIAN_POINT ( 'NONE',  ( 7.550503318189189628, 1510.480349263560129, 203.5706572562480119 ) ) ;
#11871 = CARTESIAN_POINT ( 'NONE',  ( -35.93338201885099892, 1384.980665049489971, 209.4036774743509852 ) ) ;
#11872 = CARTESIAN_POINT ( 'NONE',  ( 16.77431906226270186, 1423.634601885720031, 228.4330072057720145 ) ) ;
#11873 = CARTESIAN_POINT ( 'NONE',  ( 21.32617020600000046, 1509.431680020230033, 227.8426432890980209 ) ) ;
#11874 = CARTESIAN_POINT ( 'NONE',  ( 14.55718211070000123, 1474.164285818730150, 224.0619686816980050 ) ) ;
#11875 = CIRCLE ( 'NONE', #92265, 8.989690721650012151 ) ;
#11876 = CARTESIAN_POINT ( 'NONE',  ( 2.131986625828341086, 1526.000688113688057, 177.5511380990155601 ) ) ;
#11877 = AXIS2_PLACEMENT_3D ( 'NONE', #47542, #82229, #12819 ) ;
#11879 = ORIENTED_EDGE ( 'NONE', *, *, #4250, .T. ) ;
#11878 = CARTESIAN_POINT ( 'NONE',  ( 6.610761729033765022, 1420.121162737279974, 222.4765268707103303 ) ) ;
#11880 = CARTESIAN_POINT ( 'NONE',  ( -9.094348614660001218, 1384.950164682069953, 199.9428816977090264 ) ) ;
#11881 = DIRECTION ( 'NONE',  ( -1.755985294532469921E-16, 1.000000000000000000, -1.338183447452831989E-16 ) ) ;
#11882 = CARTESIAN_POINT ( 'NONE',  ( -156.6846457583352503, 1526.382868172863937, 77.25240589482224607 ) ) ;
#11883 = CARTESIAN_POINT ( 'NONE',  ( -11.54717405559999932, 1415.048591087029763, 195.8252350565979896 ) ) ;
#11884 = CARTESIAN_POINT ( 'NONE',  ( 0.3865936853360019687, 1422.115159822240230, 193.5453889049990153 ) ) ;
#11885 = CARTESIAN_POINT ( 'NONE',  ( 23.93004698060000024, 1410.670645398829947, 210.2052696501280025 ) ) ;
#11886 = CARTESIAN_POINT ( 'NONE',  ( -106.9109750466100053, 1391.913060387289988, 306.4819379310129648 ) ) ;
#11887 = CARTESIAN_POINT ( 'NONE',  ( 19.00237509055349960, 1454.586986596490078, 200.6139983104000066 ) ) ;
#11888 = CARTESIAN_POINT ( 'NONE',  ( -15.07724445960000104, 1422.393410174129940, 228.4053988666979933 ) ) ;
#11890 = CARTESIAN_POINT ( 'NONE',  ( -13.57816499950000022, 1379.569537802170089, 207.8818212896190118 ) ) ;
#11889 = CARTESIAN_POINT ( 'NONE',  ( 31.23437356469446158, 1523.382868172864164, 222.8968241038843416 ) ) ;
#11891 = CARTESIAN_POINT ( 'NONE',  ( -5.030623454749999723, 1391.799616574489846, 203.7592715847190163 ) ) ;
#11892 = CARTESIAN_POINT ( 'NONE',  ( 0.3785032462900000394, 1486.990708827730032, 230.2501120783980184 ) ) ;
#11893 = CARTESIAN_POINT ( 'NONE',  ( 203.9558787908000284, -8382.262153571269664, -1760.903728536709878 ) ) ;
#11894 = LINE ( 'NONE', #97010, #58684 ) ;
#11895 = CARTESIAN_POINT ( 'NONE',  ( -0.6713814905552020207, 1419.496215425129776, 184.7333992447800313 ) ) ;
#11896 = CARTESIAN_POINT ( 'NONE',  ( 4.611879685325000366, 1516.858533673840157, 204.4999481076869756 ) ) ;
#11897 = CARTESIAN_POINT ( 'NONE',  ( -18.78018960140000360, 1425.453421275130040, 226.8344281414980230 ) ) ;
#11898 = CARTESIAN_POINT ( 'NONE',  ( -18.07364243031040019, 1485.804844989679850, 188.7995565196659982 ) ) ;
#11899 = CARTESIAN_POINT ( 'NONE',  ( -10.94209231895430179, 1492.979988125699947, 207.3926202358989883 ) ) ;
#11900 = CARTESIAN_POINT ( 'NONE',  ( -11.30108578371440586, 1422.091378380982405, 210.6376354647668734 ) ) ;
#11902 = ORIENTED_EDGE ( 'NONE', *, *, #69473, .F. ) ;
#11901 = CARTESIAN_POINT ( 'NONE',  ( -67.96720087744429861, 1379.746016284620055, 279.4351274535100060 ) ) ;
#11903 = ORIENTED_EDGE ( 'NONE', *, *, #109794, .T. ) ;
#11904 = CARTESIAN_POINT ( 'NONE',  ( 27.70972759929999896, 1508.058934375229910, 212.2396871123379753 ) ) ;
#11905 = EDGE_LOOP ( 'NONE', ( #87802, #63935, #72206, #10259 ) ) ;
#11906 = CARTESIAN_POINT ( 'NONE',  ( -105.8639003480000014, 1378.913060387289988, 305.0513551771590528 ) ) ;
#11907 = CARTESIAN_POINT ( 'NONE',  ( -109.6580479539999970, 1384.932677638599898, 311.3230131862590042 ) ) ;
#11909 = CARTESIAN_POINT ( 'NONE',  ( 15.73554083432909856, 1409.462555430399789, 192.8532499784679999 ) ) ;
#11908 = CARTESIAN_POINT ( 'NONE',  ( -2.075990293979999676E-15, 1427.305457135430061, 123.0297916884979941 ) ) ;
#11910 = DIRECTION ( 'NONE',  ( 0.000000000000000000, 2.176037128269999911E-14, 1.000000000000000000 ) ) ;
#11911 = CARTESIAN_POINT ( 'NONE',  ( -24.75919491527180227, 1451.809128946330020, 137.0711371202310147 ) ) ;
#11912 = CARTESIAN_POINT ( 'NONE',  ( -0.2597432229320009722, 1467.543909054789992, 220.2373604048989932 ) ) ;
#11913 = CARTESIAN_POINT ( 'NONE',  ( 13.31824321100000041, 1409.378143688529917, 226.7832290943979956 ) ) ;
#11914 = CARTESIAN_POINT ( 'NONE',  ( 10.99603037215820045, 1480.661475631009807, 212.0619901542429773 ) ) ;
#11915 = CARTESIAN_POINT ( 'NONE',  ( -4.996642198295000448, 1516.697242742309982, 211.9989590406970024 ) ) ;
#11916 = CARTESIAN_POINT ( 'NONE',  ( 41.14836836624020577, 1446.538313982190175, 134.0999999985649822 ) ) ;
#11917 = ORIENTED_EDGE ( 'NONE', *, *, #50275, .T. ) ;
#11918 = CARTESIAN_POINT ( 'NONE',  ( 20.75865325819999896, 1455.056399776190119, 207.3304373729289978 ) ) ;
#11919 = CARTESIAN_POINT ( 'NONE',  ( -2.187180277853430166, 1431.234802153099963, 201.0301937506220042 ) ) ;
#11920 = ORIENTED_EDGE ( 'NONE', *, *, #107543, .F. ) ;
#11921 = ORIENTED_EDGE ( 'NONE', *, *, #110238, .T. ) ;
#11922 = ORIENTED_EDGE ( 'NONE', *, *, #3615, .F. ) ;
#11923 = FACE_OUTER_BOUND ( 'NONE', #72413, .T. ) ;
#11924 = CARTESIAN_POINT ( 'NONE',  ( 4.671899514437313883, 1454.661148777524886, 217.2862335604198165 ) ) ;
#11925 = ADVANCED_FACE ( 'NONE', ( #23706 ), #22070, .F. ) ;
#11926 = CARTESIAN_POINT ( 'NONE',  ( 20.78751799560000180, 1497.558923099089952, 213.2307807641690260 ) ) ;
#11927 = CARTESIAN_POINT ( 'NONE',  ( -8.581480553229999586, 1384.925094855179850, 218.6696853789089801 ) ) ;
#11928 = CARTESIAN_POINT ( 'NONE',  ( 3.281831459213320201, 1466.303209658950209, 198.5678429405679992 ) ) ;
#11929 = AXIS2_PLACEMENT_3D ( 'NONE', #61600, #52641, #86778 ) ;
#11930 = CARTESIAN_POINT ( 'NONE',  ( -18.39846574424100112, 1508.551704408389924, 210.4158962701780240 ) ) ;
#11931 = CARTESIAN_POINT ( 'NONE',  ( -63.79925921728045779, 1379.736147238250169, 269.7686537772054294 ) ) ;
#11932 = CARTESIAN_POINT ( 'NONE',  ( 3.281831498710000350, 1466.303209520490100, 198.5678428718989892 ) ) ;
#11933 = CARTESIAN_POINT ( 'NONE',  ( 1.067730373280000089, 1508.997447140530085, 238.8264927836980007 ) ) ;
#11934 = ORIENTED_EDGE ( 'NONE', *, *, #44989, .T. ) ;
#11935 = CARTESIAN_POINT ( 'NONE',  ( -1.718203501584999904, 1516.898441858519845, 207.4215862561470090 ) ) ;
#11936 = EDGE_LOOP ( 'NONE', ( #10627, #53562, #79164, #6761, #60677 ) ) ;
#11937 = CARTESIAN_POINT ( 'NONE',  ( 25.80232757302710311, 1440.913060387330006, 241.6272588468080187 ) ) ;
#11938 = EDGE_CURVE ( 'NONE', #92390, #62647, #95890, .T. ) ;
#11939 = CARTESIAN_POINT ( 'NONE',  ( 11.71326577039419981, 1479.172152660740039, 208.0100838261020044 ) ) ;
#11940 = ORIENTED_EDGE ( 'NONE', *, *, #28441, .F. ) ;
#11941 = CARTESIAN_POINT ( 'NONE',  ( -5.984315745076109749, 1508.551704607450120, 202.1093160777899982 ) ) ;
#11942 = CARTESIAN_POINT ( 'NONE',  ( -14.39047323610000184, 1409.582260767330126, 191.0429864508980131 ) ) ;
#11943 = CARTESIAN_POINT ( 'NONE',  ( -18.46075352249601664, 1508.457339376852588, 211.1564294638567958 ) ) ;
#11945 = DIRECTION ( 'NONE',  ( 0.000000000000000000, 1.000000000000000000, 0.000000000000000000 ) ) ;
#11944 = CARTESIAN_POINT ( 'NONE',  ( -24.41028537817162203, 1440.675387093458539, 212.0168806395822401 ) ) ;
#11946 = CARTESIAN_POINT ( 'NONE',  ( 22.20862914986459558, 1410.187580636810026, 206.2522814213569973 ) ) ;
#11947 = CARTESIAN_POINT ( 'NONE',  ( -5.987023825353920969, 1511.685461860059831, 200.6544365511240073 ) ) ;
#11948 = DIRECTION ( 'NONE',  ( -3.909897602534546929E-05, -1.707468113285530796E-06, 0.9999999992341774835 ) ) ;
#11949 = FACE_OUTER_BOUND ( 'NONE', #36032, .T. ) ;
#11950 = CARTESIAN_POINT ( 'NONE',  ( -7.138635338890000348, 1509.224971056590221, 218.8819033035289863 ) ) ;
#11952 = CARTESIAN_POINT ( 'NONE',  ( -103.5801209296959939, 1379.883073482990085, 303.9981235976169955 ) ) ;
#11951 = CARTESIAN_POINT ( 'NONE',  ( 15.71037775574616191, 1410.149708096691711, 191.7130642213688247 ) ) ;
#11953 = CARTESIAN_POINT ( 'NONE',  ( -5.778372601744999670, 1516.932669162149978, 216.0673360190369863 ) ) ;
#11954 = CARTESIAN_POINT ( 'NONE',  ( -32.52419458002813002, 1524.600389084707103, 217.0761871924782156 ) ) ;
#11955 = CARTESIAN_POINT ( 'NONE',  ( 5.943999021440889763, 1511.034527886640262, 216.7021439542070027 ) ) ;
#11956 = CARTESIAN_POINT ( 'NONE',  ( 28.14152795669999918, 1508.624282194429952, 208.2673348377579998 ) ) ;
#11957 = CARTESIAN_POINT ( 'NONE',  ( -1.119439127814999990, 1517.026534522949987, 212.3908711059869745 ) ) ;
#11958 = CARTESIAN_POINT ( 'NONE',  ( -19.03312856000000153, 1434.814457748080031, 208.9576311756670179 ) ) ;
#11959 = CARTESIAN_POINT ( 'NONE',  ( -3.143710964241499983, 1483.525783009509951, 198.9295231152539998 ) ) ;
#11961 = EDGE_LOOP ( 'NONE', ( #90511, #3128 ) ) ;
#11960 = CARTESIAN_POINT ( 'NONE',  ( -113.4000000000000057, 1385.251674955540238, 297.2379167808589955 ) ) ;
#11962 = DIRECTION ( 'NONE',  ( 0.4530882417530768813, -0.7475172582776776764, 0.4857252245479219410 ) ) ;
#11963 = B_SPLINE_CURVE_WITH_KNOTS ( 'NONE', 3,
 ( #35105, #61999, #2642, #69847, #435, #26135, #78212, #27819, #95569, #96118, #34554, #28366, #77668, #68737 ),
 .UNSPECIFIED., .F., .F.,
 ( 4, 2, 2, 1, 1, 2, 2, 4 ),
 ( 0.000000000000000000, 0.1250000000000179579, 0.2500000000000359157, 0.3750000000000538458, 0.4374999999996236344, 0.4687499999994085287, 0.4999999999991934230, 1.000000000000000000 ),
 .UNSPECIFIED. ) ;
#11964 = CARTESIAN_POINT ( 'NONE',  ( 10.53938673539999904, 1467.231892115330083, 248.5638781408979696 ) ) ;
#11965 = EDGE_CURVE ( 'NONE', #45814, #48553, #41652, .T. ) ;
#11966 = CARTESIAN_POINT ( 'NONE',  ( 10.37397012400595919, 1482.317496542443223, 211.4772094469874162 ) ) ;
#11967 = CARTESIAN_POINT ( 'NONE',  ( -26.24895334306360084, 1509.829694036420051, 222.2356625040769984 ) ) ;
#11968 = CARTESIAN_POINT ( 'NONE',  ( -0.4986482637964069764, 1508.982360564700230, 238.8511999805219830 ) ) ;
#11969 = ADVANCED_FACE ( 'NONE', ( #25346 ), #56076, .T. ) ;
#11970 = CARTESIAN_POINT ( 'NONE',  ( -19.83396412799999808, 1455.741242482730058, 225.6883558546980169 ) ) ;
#11971 = B_SPLINE_CURVE_WITH_KNOTS ( 'NONE', 3,
 ( #106863, #100129, #91176, #22844, #56486, #30154, #48084, #40222, #38025, #39104, #108530, #82219, #90617, #39677, #81654, #73844, #64346, #4960, #107971, #63795, #21737, #3896, #14456, #55939, #90060, #29610, #48649, #13341, #47533, #30715, #31268, #99008, #82776, #6069, #74403, #31820, #57607, #80580, #50834, #66562, #83874, #41877, #110181, #16638, #51380, #32380, #59254, #85513, #32912 ),
 .UNSPECIFIED., .F., .F.,
 ( 4, 3, 3, 3, 3, 3, 3, 3, 3, 3, 3, 3, 3, 3, 3, 3, 4 ),
 ( -12.57638456940000005, -12.28317881097320097, -11.95680856205710008, -11.62570944449999999, -11.51472436910320063, -11.17721019326580034, -10.83638269494210071, -10.49376598036129948, -10.14927727058690010, -9.804494080889758933, -9.458815399600899454, -9.117616601269459053, -8.780289088706128453, -8.445887015288109367, -8.114782774046028990, -7.787209585599999428, -7.548674336869999557 ),
 .UNSPECIFIED. ) ;
#11972 = EDGE_CURVE ( 'NONE', #17632, #29227, #107089, .T. ) ;
#11974 = CARTESIAN_POINT ( 'NONE',  ( 2.500000000000000000, 1419.383841502129826, 144.0536014349980007 ) ) ;
#11973 = CARTESIAN_POINT ( 'NONE',  ( -19.54838982620000110, 1444.804232268380019, 224.9727483068980121 ) ) ;
#11975 = CARTESIAN_POINT ( 'NONE',  ( 0.1695961737810000036, 1488.805759878529898, 187.7260248280979908 ) ) ;
#11976 = CARTESIAN_POINT ( 'NONE',  ( -105.8736429085269890, 1378.613677389549821, 306.5408079283200209 ) ) ;
#11977 = ORIENTED_EDGE ( 'NONE', *, *, #50862, .T. ) ;
#11978 = CARTESIAN_POINT ( 'NONE',  ( 3.254401403604999743, 1516.919782530640077, 205.0791161293069820 ) ) ;
#11979 = CARTESIAN_POINT ( 'NONE',  ( 1.777827934399999865, 1405.774244366030189, 267.5358630757979768 ) ) ;
#11980 = CARTESIAN_POINT ( 'NONE',  ( 1.485593186740000071, 1515.527915486090023, 213.1675302385690145 ) ) ;
#11981 = EDGE_CURVE ( 'NONE', #39456, #97183, #14200, .T. ) ;
#11982 = CARTESIAN_POINT ( 'NONE',  ( 40.88432421962840380, 1450.842314229549856, 269.8587844018130681 ) ) ;
#11983 = CARTESIAN_POINT ( 'NONE',  ( -27.01382282590000017, 1451.969727051930022, 134.9184453750980026 ) ) ;
#11984 = CARTESIAN_POINT ( 'NONE',  ( -29.40443212115374649, 1512.187213306747481, 222.0897836382247306 ) ) ;
#11985 = CARTESIAN_POINT ( 'NONE',  ( -45.44691271756050099, 1440.913060394409968, 265.9511583644469965 ) ) ;
#11986 = CARTESIAN_POINT ( 'NONE',  ( -6.126746181595000174, 1514.923664147150021, 217.2480802176870043 ) ) ;
#11987 = CARTESIAN_POINT ( 'NONE',  ( -107.2374608147510031, 1384.994991009320074, 298.2563606770149818 ) ) ;
#11988 = DIRECTION ( 'NONE',  ( -0.2113515706023144647, -1.466546124833779360E-15, 0.9774101051267757301 ) ) ;
#11989 = B_SPLINE_CURVE_WITH_KNOTS ( 'NONE', 5,
 ( #54804, #27935, #61014, #79449, #2761, #20074, #88935, #88394, #3312 ),
 .UNSPECIFIED., .F., .F.,
 ( 6, 3, 6 ),
 ( -26.06148575846079751, -22.14719212230000167, -12.02292824550000105 ),
 .UNSPECIFIED. ) ;
#11990 = CARTESIAN_POINT ( 'NONE',  ( -1.653204953259999943, 1507.621692541890070, 221.1218351714989865 ) ) ;
#11991 = PLANE ( 'NONE',  #64049 ) ;
#11992 = ORIENTED_EDGE ( 'NONE', *, *, #9132, .T. ) ;
#11993 = CARTESIAN_POINT ( 'NONE',  ( -31.32742177469999945, 1440.913060387330006, 255.3819207742980097 ) ) ;
#11994 = CARTESIAN_POINT ( 'NONE',  ( 9.104904664964859506, 1467.958063039340004, 204.8661130570050091 ) ) ;
#11995 = CARTESIAN_POINT ( 'NONE',  ( -0.1067711740600000014, 1475.319450600529990, 269.4986873274979757 ) ) ;
#11996 = CARTESIAN_POINT ( 'NONE',  ( -4.259705254135069730, 1446.578490207630011, 159.5784562383719845 ) ) ;
#11998 = B_SPLINE_CURVE_WITH_KNOTS ( 'NONE', 3,
 ( #105087, #76701, #54160, #79894 ),
 .UNSPECIFIED., .F., .F.,
 ( 4, 4 ),
 ( 0.000000000000000000, 1.000000000000000000 ),
 .UNSPECIFIED. ) ;
#11997 = CARTESIAN_POINT ( 'NONE',  ( -28.22027524449999802, 1509.158030585729875, 210.3012591173880139 ) ) ;
#11999 = EDGE_CURVE ( 'NONE', #29284, #68807, #105960, .T. ) ;
#12000 = CARTESIAN_POINT ( 'NONE',  ( -4.122335531849919299, 1448.298783337578470, 185.1042314757649194 ) ) ;
#12001 = CARTESIAN_POINT ( 'NONE',  ( -37.33982031581620475, 1384.799273965830025, 237.6968796437000151 ) ) ;
#12002 = AXIS2_PLACEMENT_3D ( 'NONE', #42026, #83456, #100274 ) ;
#12003 = CARTESIAN_POINT ( 'NONE',  ( -17.58950218620000072, 1415.041103189330215, 207.8054830739180261 ) ) ;
#12004 = CARTESIAN_POINT ( 'NONE',  ( 11.87252949456130047, 1432.818935466539870, 149.9811197374779965 ) ) ;
#12005 = CARTESIAN_POINT ( 'NONE',  ( 26.79700173971789923, 1435.433286571610097, 135.3787855487989873 ) ) ;
#12007 = EDGE_CURVE ( 'NONE', #105161, #35207, #25372, .T. ) ;
#12006 = CARTESIAN_POINT ( 'NONE',  ( -8.229377170839249800, 1396.200436570979946, 216.4989716017560113 ) ) ;
#12008 = CARTESIAN_POINT ( 'NONE',  ( -14.77963593200000147, 1422.241748322230023, 229.4612819423979886 ) ) ;
#12009 = CARTESIAN_POINT ( 'NONE',  ( 31.32995031131189378, 1523.678648413191695, 196.3423562208913324 ) ) ;
#12010 = ORIENTED_EDGE ( 'NONE', *, *, #31489, .F. ) ;
#12011 = CARTESIAN_POINT ( 'NONE',  ( -11.33033813286753677, 1502.925034412118521, 207.0842279942457083 ) ) ;
#12012 = CARTESIAN_POINT ( 'NONE',  ( 1.802301219090000073, 1409.910657985330090, 232.1755723407979985 ) ) ;
#12013 = CARTESIAN_POINT ( 'NONE',  ( -20.87069991009999725, 1506.658021081189872, 214.5368842940590071 ) ) ;
#12015 = CARTESIAN_POINT ( 'NONE',  ( -14.10835369926500071, 1513.596256836700150, 192.4716710403669993 ) ) ;
#12014 = CARTESIAN_POINT ( 'NONE',  ( 11.56973989449999962, 1426.806448162329843, 132.2115754456980028 ) ) ;
#12016 = CARTESIAN_POINT ( 'NONE',  ( -3.558358604862239982, 1455.955982659530036, 200.3550966546550001 ) ) ;
#12017 = CARTESIAN_POINT ( 'NONE',  ( -12.32664273690000023, 1378.996295195989887, 209.7960013046609902 ) ) ;
#12018 = CARTESIAN_POINT ( 'NONE',  ( -2.291047527245000381, 1516.524310051880093, 201.4130759250869858 ) ) ;
#12019 = CARTESIAN_POINT ( 'NONE',  ( 7.783524595000000268, 1424.818165691749982, 211.8233307128890033 ) ) ;
#12021 = CARTESIAN_POINT ( 'NONE',  ( 2.470168521978396203, 1512.187213306747481, 242.8787258963054683 ) ) ;
#12020 = AXIS2_PLACEMENT_3D ( 'NONE', #47074, #3429, #81198 ) ;
#12022 = CARTESIAN_POINT ( 'NONE',  ( 4.416389894569999086, 1509.047812932029956, 180.2178558522979870 ) ) ;
#12023 = CARTESIAN_POINT ( 'NONE',  ( -11.16717556649999921, 1414.661898229710005, 212.7267128011690147 ) ) ;
#12024 = CARTESIAN_POINT ( 'NONE',  ( -47.74616927649559983, 1377.617239580540172, 243.6775589761319907 ) ) ;
#12025 = CARTESIAN_POINT ( 'NONE',  ( 4.239534266359169301, 1367.783695315041314, 210.6218459617142003 ) ) ;
#12027 = ORIENTED_EDGE ( 'NONE', *, *, #88452, .F. ) ;
#12026 = DIRECTION ( 'NONE',  ( 0.02091224828123190022, 0.9990482215818557998, 0.03827961371219716635 ) ) ;
#12028 = VERTEX_POINT ( 'NONE', #33477 ) ;
#12029 = DIRECTION ( 'NONE',  ( 0.9455185755993178454, 0.000000000000000000, -0.3255681544571537578 ) ) ;
#12030 = DIRECTION ( 'NONE',  ( 0.000000000000000000, 1.000000000000000000, 0.000000000000000000 ) ) ;
#12031 = CARTESIAN_POINT ( 'NONE',  ( -18.57722710470001815, 1435.146103754618707, 144.7442513582978449 ) ) ;
#12032 = LINE ( 'NONE', #70324, #69572 ) ;
#12034 = CARTESIAN_POINT ( 'NONE',  ( -1.358753378944950185, 1412.017682228260128, 185.5325774167320105 ) ) ;
#12033 = CARTESIAN_POINT ( 'NONE',  ( -7.777873728749999493, 1384.438531822959931, 218.8954641931690333 ) ) ;
#12035 = CARTESIAN_POINT ( 'NONE',  ( -31.32995031131211761, 1523.678648413191695, 196.3423562208917588 ) ) ;
#12036 = DIRECTION ( 'NONE',  ( -1.755985294532469921E-16, 1.000000000000000000, -1.338183447452831989E-16 ) ) ;
#12037 = CARTESIAN_POINT ( 'NONE',  ( -41.45619614403190667, 1444.641645903369863, 136.4680537501220101 ) ) ;
#12038 = SHAPE_REPRESENTATION_RELATIONSHIP ( 'NONE' , 'NONE' ,  #110199, #100095 ) ;
#12039 = CARTESIAN_POINT ( 'NONE',  ( -2.500000000000000000, 1448.231807117899962, 166.4374264918500046 ) ) ;
#12040 = LINE ( 'NONE', #46222, #88414 ) ;
#12041 = FACE_OUTER_BOUND ( 'NONE', #109948, .T. ) ;
#12042 = CARTESIAN_POINT ( 'NONE',  ( -2.286937354066500117, 1406.300447436870172, 269.2931096073519939 ) ) ;
#12043 = CARTESIAN_POINT ( 'NONE',  ( 41.48252513910000516, 1444.135613576870128, 136.5500652558980050 ) ) ;
#12044 = EDGE_LOOP ( 'NONE', ( #94679, #3550, #38083, #12324 ) ) ;
#12045 = CARTESIAN_POINT ( 'NONE',  ( 0.4151546846821903003, 1522.382868172863937, 175.3106345060153046 ) ) ;
#12046 = CARTESIAN_POINT ( 'NONE',  ( 21.39312961732869312, 1524.775785348137333, 233.9875869515353202 ) ) ;
#12047 = ORIENTED_EDGE ( 'NONE', *, *, #34185, .T. ) ;
#12048 = VERTEX_POINT ( 'NONE', #101786 ) ;
#12049 = CARTESIAN_POINT ( 'NONE',  ( -15.62861149524349891, 1418.244676918490086, 203.0179538217920197 ) ) ;
#12050 = CARTESIAN_POINT ( 'NONE',  ( 20.87949000879999772, 1495.383548355589937, 212.2163053943189936 ) ) ;
#12051 = AXIS2_PLACEMENT_3D ( 'NONE', #6592, #93340, #84933 ) ;
#12052 = CARTESIAN_POINT ( 'NONE',  ( 3.456007385174999946, 1516.647534046129977, 215.6697273451470096 ) ) ;
#12053 = CARTESIAN_POINT ( 'NONE',  ( 3.367054129315000033, 1511.558654537720031, 216.9757299529570105 ) ) ;
#12054 = ORIENTED_EDGE ( 'NONE', *, *, #51184, .F. ) ;
#12055 = CARTESIAN_POINT ( 'NONE',  ( -14.44412179201740010, 1509.548839732050055, 182.8006781750410141 ) ) ;
#12056 = CARTESIAN_POINT ( 'NONE',  ( -94.91986059570000123, 1375.460834337080087, 300.7314404810590531 ) ) ;
#12057 = CARTESIAN_POINT ( 'NONE',  ( 18.00081235489999898, 1415.932617989529945, 212.9990166833879925 ) ) ;
#12058 = CARTESIAN_POINT ( 'NONE',  ( 3.255340926295000159, 1516.962555622980062, 204.4977466407669908 ) ) ;
#12059 = DIRECTION ( 'NONE',  ( 0.000000000000000000, 0.000000000000000000, 1.000000000000000000 ) ) ;
#12060 = CYLINDRICAL_SURFACE ( 'NONE', #105685, 1.000000000000003775 ) ;
#12061 = CARTESIAN_POINT ( 'NONE',  ( -4.219013252539999925, 1410.436621388929780, 232.1416577203980012 ) ) ;
#12063 = ORIENTED_EDGE ( 'NONE', *, *, #69514, .F. ) ;
#12062 = CARTESIAN_POINT ( 'NONE',  ( -15.28420222189999933, 1497.713060387329961, 192.4536333146980098 ) ) ;
#12064 = CARTESIAN_POINT ( 'NONE',  ( 1.705087066220000169, 1507.082462650630077, 236.5153987699980007 ) ) ;
#12066 = CARTESIAN_POINT ( 'NONE',  ( -19.23736494940000341, 1383.854422637459948, 220.3626903602589948 ) ) ;
#12065 = VECTOR ( 'NONE', #91135, 1000.000000000000114 ) ;
#12067 = CARTESIAN_POINT ( 'NONE',  ( -8.301987938657498844, 1512.913060387330006, 185.0111222839169898 ) ) ;
#12068 = CARTESIAN_POINT ( 'NONE',  ( 28.88161794570000040, 1415.817973096529840, 270.2667682292980089 ) ) ;
#12069 = CARTESIAN_POINT ( 'NONE',  ( -2.284526496774999860, 1516.956048353049937, 212.5847947667770086 ) ) ;
#12070 = CARTESIAN_POINT ( 'NONE',  ( -66.42105914469999561, 1379.741982406930219, 275.2841866764590009 ) ) ;
#12071 = AXIS2_PLACEMENT_3D ( 'NONE', #58698, #92281, #32918 ) ;
#12072 = CARTESIAN_POINT ( 'NONE',  ( 0.02043389301803385377, 1507.170882767263492, 237.3556640025030049 ) ) ;
#12073 = CARTESIAN_POINT ( 'NONE',  ( -31.00914578553006962, 1524.547395018738371, 221.8103655202198468 ) ) ;
#12074 = CARTESIAN_POINT ( 'NONE',  ( 9.992021184015209556, 1491.422374287340062, 188.4943422680200058 ) ) ;
#12075 = CARTESIAN_POINT ( 'NONE',  ( 1.715109447055000125, 1516.963431999339946, 209.8570730874349977 ) ) ;
#12076 = EDGE_LOOP ( 'NONE', ( #7714, #56960, #63977, #55408 ) ) ;
#12077 = CARTESIAN_POINT ( 'NONE',  ( 4.352598717569040154, 1420.338240732929989, 185.6900682800660149 ) ) ;
#12078 = CARTESIAN_POINT ( 'NONE',  ( -4.415413580500000101, 1415.372779959029913, 232.3000245577979967 ) ) ;
#12079 = CARTESIAN_POINT ( 'NONE',  ( -109.9987472809999929, 1384.581606379090090, 311.2589846932590376 ) ) ;
#12080 = ORIENTED_EDGE ( 'NONE', *, *, #77220, .F. ) ;
#12081 = CARTESIAN_POINT ( 'NONE',  ( -25.36236875327359996, 1385.254273797359929, 223.9400902521850014 ) ) ;
#12082 = CARTESIAN_POINT ( 'NONE',  ( -2.532956463620000154, 1430.062184787290107, 201.0558268371090094 ) ) ;
#12083 = ADVANCED_FACE ( 'NONE', ( #56651 ), #61165, .T. ) ;
#12084 = CARTESIAN_POINT ( 'NONE',  ( -20.84038636311550263, 1509.309337355510024, 228.9357793634370069 ) ) ;
#12085 = DIRECTION ( 'NONE',  ( 0.4794255386041977873, -8.806904269216896357E-17, -0.8775825618903755343 ) ) ;
#12086 = CARTESIAN_POINT ( 'NONE',  ( 0.1069017372639999991, 1409.419549215130019, 233.0164748551979983 ) ) ;
#12087 = CARTESIAN_POINT ( 'NONE',  ( -0.06409245479768720111, 1420.448119606670161, 182.6888690408050024 ) ) ;
#12089 = CARTESIAN_POINT ( 'NONE',  ( 21.84020450222038079, 1523.382868172864164, 183.2638850454218016 ) ) ;
#12088 = CARTESIAN_POINT ( 'NONE',  ( 6.556022194504999234, 1516.833525648419936, 216.0623193043769845 ) ) ;
#12090 = CARTESIAN_POINT ( 'NONE',  ( -3.467940602053699806, 1495.562067921990092, 197.2905559617530002 ) ) ;
#12091 = CARTESIAN_POINT ( 'NONE',  ( 10.75551144678770044, 1470.210679328900142, 207.2751881891400103 ) ) ;
#12092 = VECTOR ( 'NONE', #102025, 1000.000000000000000 ) ;
#12093 = ORIENTED_EDGE ( 'NONE', *, *, #34433, .T. ) ;
#12094 = CARTESIAN_POINT ( 'NONE',  ( 1.708747624254999931, 1517.213554313520035, 202.1696795498070003 ) ) ;
#12095 = CARTESIAN_POINT ( 'NONE',  ( -15.08013804596499874, 1512.195694528090144, 221.7327207927669974 ) ) ;
#12096 = ORIENTED_EDGE ( 'NONE', *, *, #19891, .T. ) ;
#12097 = CARTESIAN_POINT ( 'NONE',  ( 7.499999999999999112, 1392.213060387289943, 209.1218459616989946 ) ) ;
#12098 = EDGE_CURVE ( 'NONE', #3729, #107968, #43018, .T. ) ;
#12099 =( BOUNDED_CURVE ( )  B_SPLINE_CURVE ( 3, ( #65073, #32560, #91367, #22469 ),
 .UNSPECIFIED., .F., .F. ) 
 B_SPLINE_CURVE_WITH_KNOTS ( ( 4, 4 ),
 ( 1.535862050798705081, 1.553281469862595188 ),
 .UNSPECIFIED. ) 
 CURVE ( )  GEOMETRIC_REPRESENTATION_ITEM ( )  RATIONAL_B_SPLINE_CURVE ( ( 1.000000000000000000, 0.9999747138131391822, 0.9999747138131391822, 1.000000000000000000 ) ) 
 REPRESENTATION_ITEM ( '' )  );
#12100 = CARTESIAN_POINT ( 'NONE',  ( 3.750000000000000000, 1516.051704408390151, 209.1218459616989946 ) ) ;
#12101 = CARTESIAN_POINT ( 'NONE',  ( 8.297057133861780898, 1511.753217516670247, 203.0771327291550108 ) ) ;
#12102 = PRODUCT_DEFINITION_CONTEXT ( 'detailed design', #9133, 'design' ) ;
#12103 = CARTESIAN_POINT ( 'NONE',  ( 1.542378980109999853, 1442.042834985789796, 218.9497927206290058 ) ) ;
#12104 = CARTESIAN_POINT ( 'NONE',  ( 15.66605189140578247, 1421.055886089876594, 227.6080301534365731 ) ) ;
#12105 = CARTESIAN_POINT ( 'NONE',  ( 5.557914828519999517, 1420.826195899929871, 186.0956685246979987 ) ) ;
#12106 = CARTESIAN_POINT ( 'NONE',  ( -18.18255051909999764, 1424.952931054730016, 227.0171290564980211 ) ) ;
#12107 = CARTESIAN_POINT ( 'NONE',  ( -17.78508617079999610, 1435.118679338369930, 145.5186544196980094 ) ) ;
#12108 = CARTESIAN_POINT ( 'NONE',  ( -105.5826323030000111, 1391.887506638209970, 304.2218459572590064 ) ) ;
#12109 = DIRECTION ( 'NONE',  ( -9.341989762165448955E-47, 1.000000000000000000, -1.836970198721029688E-16 ) ) ;
#12111 = DIRECTION ( 'NONE',  ( 0.9900965937346509760, 0.1403878024439500216, 3.790652827686680047E-16 ) ) ;
#12110 = CARTESIAN_POINT ( 'NONE',  ( 0.8764178805871419842, 1410.319213181679970, 233.0346325316370155 ) ) ;
#12112 = CARTESIAN_POINT ( 'NONE',  ( -1.748905610829809998, 1488.269106374019884, 219.8524659745219765 ) ) ;
#12113 = ORIENTED_EDGE ( 'NONE', *, *, #32367, .T. ) ;
#12114 = DIRECTION ( 'NONE',  ( -1.000000000000000000, 0.000000000000000000, 0.000000000000000000 ) ) ;
#12115 = CARTESIAN_POINT ( 'NONE',  ( -15.40297484210000079, 1508.551704408389924, 214.7119267552490101 ) ) ;
#12116 = DIRECTION ( 'NONE',  ( -1.000000000000000000, 0.000000000000000000, 0.000000000000000000 ) ) ;
#12117 = AXIS2_PLACEMENT_3D ( 'NONE', #109765, #33045, #24619 ) ;
#12118 = CARTESIAN_POINT ( 'NONE',  ( -11.92436196651230240, 1433.423664094866126, 149.9160749996637492 ) ) ;
#12119 = CARTESIAN_POINT ( 'NONE',  ( 14.38014760757802968, 1517.151704408390060, 208.3596762285818045 ) ) ;
#12120 = CARTESIAN_POINT ( 'NONE',  ( -16.24600786016249643, 1417.782917922866091, 204.8292002259562707 ) ) ;
#12121 = CARTESIAN_POINT ( 'NONE',  ( -3.350338079455601026, 1523.604703353109699, 242.0808062845893289 ) ) ;
#12122 = CARTESIAN_POINT ( 'NONE',  ( 14.59882275880000080, 1475.513060387329915, 223.7206687199980308 ) ) ;
#12123 = FACE_OUTER_BOUND ( 'NONE', #109175, .T. ) ;
#12124 = CARTESIAN_POINT ( 'NONE',  ( -7.338592697498807382, 1507.281022697548451, 235.5381695832356854 ) ) ;
#12125 = CARTESIAN_POINT ( 'NONE',  ( -6.435172845517500129, 1488.130694331340237, 218.4885078549579873 ) ) ;
#12126 = CARTESIAN_POINT ( 'NONE',  ( -4.354856984870000502, 1481.954696296189923, 231.1149923864989830 ) ) ;
#12127 = CARTESIAN_POINT ( 'NONE',  ( -81.60401292589429545, 1383.775847213790030, 304.6599215716950084 ) ) ;
#12128 = DIRECTION ( 'NONE',  ( -1.000000000000000000, 0.000000000000000000, 0.000000000000000000 ) ) ;
#12130 = EDGE_CURVE ( 'NONE', #29403, #16786, #60291, .T. ) ;
#12129 = CARTESIAN_POINT ( 'NONE',  ( -0.5179933185710690058, 1516.784603496090085, 201.4062599077630011 ) ) ;
#12132 = ORIENTED_EDGE ( 'NONE', *, *, #72671, .F. ) ;
#12131 = CARTESIAN_POINT ( 'NONE',  ( 21.18965232119999698, 1508.901491395929952, 190.3943043406979996 ) ) ;
#12133 = CARTESIAN_POINT ( 'NONE',  ( 13.77266209894789917, 1517.151704408390060, 201.2043266506040027 ) ) ;
#12134 = CARTESIAN_POINT ( 'NONE',  ( 14.69525441947700095, 1513.799047785610128, 224.1094165707140178 ) ) ;
#12135 = VERTEX_POINT ( 'NONE', #26185 ) ;
#12136 = EDGE_LOOP ( 'NONE', ( #25568, #49174, #91473 ) ) ;
#12137 = CARTESIAN_POINT ( 'NONE',  ( -7.762930123710000352, 1492.073939571090023, 209.9113589376980258 ) ) ;
#12138 = CARTESIAN_POINT ( 'NONE',  ( -109.7187112120000023, 1384.936990306269763, 297.0861906625590336 ) ) ;
#12139 = CARTESIAN_POINT ( 'NONE',  ( 13.17455542446274741, 1443.091355729311545, 169.3947984149703814 ) ) ;
#12141 = CARTESIAN_POINT ( 'NONE',  ( -13.69364984400000118, 1462.915759927429917, 238.2645906006979999 ) ) ;
#12140 = CARTESIAN_POINT ( 'NONE',  ( 40.92779976970093259, 1433.910425749881142, 269.6272358578021340 ) ) ;
#12142 = CARTESIAN_POINT ( 'NONE',  ( 76.99707197885322785, 1526.382868172863937, 398.8876973329328735 ) ) ;
#12143 = CONICAL_SURFACE ( 'NONE', #15702, 1.499999999999955369, 0.3430239404209998177 ) ;
#12144 = CARTESIAN_POINT ( 'NONE',  ( -11.93818826309999892, 1433.480069981700126, 149.8971985194979766 ) ) ;
#12145 = CARTESIAN_POINT ( 'NONE',  ( 26.88784107860000105, 1509.181461243030071, 204.0448338698880093 ) ) ;
#12146 = CARTESIAN_POINT ( 'NONE',  ( -19.56601163170000390, 1485.666649664629858, 190.1001640202979956 ) ) ;
#12147 = CARTESIAN_POINT ( 'NONE',  ( 5.996724739790000314, 1409.122470629630016, 188.2987590254980148 ) ) ;
#12148 = CARTESIAN_POINT ( 'NONE',  ( 4.876253047089999626, 1422.291999688530041, 184.8458127703979983 ) ) ;
#12149 = FACE_OUTER_BOUND ( 'NONE', #15169, .T. ) ;
#12150 = DIRECTION ( 'NONE',  ( 1.755985294532464991E-16, -1.000000000000000000, 1.338183447452830017E-16 ) ) ;
#12151 = DIRECTION ( 'NONE',  ( 0.03489949406805378795, 0.9993908271110926167, 3.148602398629828534E-12 ) ) ;
#12152 = AXIS2_PLACEMENT_3D ( 'NONE', #59672, #27712, #78669 ) ;
#12153 = CARTESIAN_POINT ( 'NONE',  ( -33.36586802512183425, 1523.382868172864164, 201.9069332299493169 ) ) ;
#12155 = VERTEX_POINT ( 'NONE', #68788 ) ;
#12154 = CARTESIAN_POINT ( 'NONE',  ( -16.19493240869999795, 1409.478599888930148, 193.4350318414979881 ) ) ;
#12156 = VERTEX_POINT ( 'NONE', #82399 ) ;
#12157 = CARTESIAN_POINT ( 'NONE',  ( -11.85768019138030027, 1431.748854777190218, 149.9507373201959979 ) ) ;
#12158 =( GEOMETRIC_REPRESENTATION_CONTEXT ( 3 ) GLOBAL_UNCERTAINTY_ASSIGNED_CONTEXT ( ( #92795 ) ) GLOBAL_UNIT_ASSIGNED_CONTEXT ( ( #4196, #29376, #13113 ) ) REPRESENTATION_CONTEXT ( 'NONE', 'WORKASPACE' ) );
#12159 = CARTESIAN_POINT ( 'NONE',  ( -11.67226624329999929, 1483.956261651290106, 228.3627183349989878 ) ) ;
#12160 = CARTESIAN_POINT ( 'NONE',  ( -10.68754386630000042, 1471.687871048830175, 270.3681166667980165 ) ) ;
#12161 = CARTESIAN_POINT ( 'NONE',  ( 21.62164173114529930, 1517.051704408389924, 208.0273405545509888 ) ) ;
#12162 = CARTESIAN_POINT ( 'NONE',  ( 6.464994551020000202, 1433.443311356699951, 154.6859263780980029 ) ) ;
#12163 = CARTESIAN_POINT ( 'NONE',  ( -15.61596525200000229, 1495.917977012930123, 224.3506286668980181 ) ) ;
#12164 = CARTESIAN_POINT ( 'NONE',  ( 0.2052324461623580010, 1452.314876516149980, 183.1678648498289874 ) ) ;
#12165 = CARTESIAN_POINT ( 'NONE',  ( -14.19989568679999969, 1422.015600902929918, 228.9627754381980083 ) ) ;
#12166 = CARTESIAN_POINT ( 'NONE',  ( -8.776085081250000641, 1460.194150302089838, 214.2375442011990003 ) ) ;
#12167 = CARTESIAN_POINT ( 'NONE',  ( 8.796059898601679805, 1362.759824263854171, 210.6218459616991936 ) ) ;
#12168 = CARTESIAN_POINT ( 'NONE',  ( -45.88106474657430311, 1437.104218600800095, 268.2135919139319640 ) ) ;
#12169 = EDGE_LOOP ( 'NONE', ( #99562, #27080, #8060, #51909 ) ) ;
#12170 = CARTESIAN_POINT ( 'NONE',  ( -3.541468562257029884, 1499.388879724870094, 181.3066299419379845 ) ) ;
#12171 = ORIENTED_EDGE ( 'NONE', *, *, #51072, .F. ) ;
#12172 = ORIENTED_EDGE ( 'NONE', *, *, #30380, .F. ) ;
#12173 = CARTESIAN_POINT ( 'NONE',  ( -7.710967015764999211, 1516.608208975040043, 210.2506035313070072 ) ) ;
#12174 = CARTESIAN_POINT ( 'NONE',  ( -5.062212390315069754, 1474.342205398819942, 198.8731691453010058 ) ) ;
#12175 = AXIS2_PLACEMENT_3D ( 'NONE', #81669, #99575, #97928 ) ;
#12176 = DIRECTION ( 'NONE',  ( 0.02091224828123159837, -0.9990482215818557998, 0.03827961371219689574 ) ) ;
#12177 = CARTESIAN_POINT ( 'NONE',  ( -13.31934106549999974, 1410.400658079930054, 189.8751199163980061 ) ) ;
#12178 = CARTESIAN_POINT ( 'NONE',  ( -27.01940583621439984, 1450.860076101910181, 136.4173285475219757 ) ) ;
#12179 = ORIENTED_EDGE ( 'NONE', *, *, #1011, .F. ) ;
#12180 = CARTESIAN_POINT ( 'NONE',  ( 3.838475640130000421, 1505.530984303090008, 221.3004008607989874 ) ) ;
#12181 = CARTESIAN_POINT ( 'NONE',  ( -1.708721022705000037, 1516.531533746980131, 201.8006767011069940 ) ) ;
#12182 = CARTESIAN_POINT ( 'NONE',  ( 7.567873768730000172, 1473.049319849490075, 217.1534710516689870 ) ) ;
#12183 = B_SPLINE_CURVE_WITH_KNOTS ( 'NONE', 5,
 ( #58373, #15234, #108207, #30397, #65126, #64588, #98707, #31495, #39909 ),
 .UNSPECIFIED., .F., .F.,
 ( 6, 3, 6 ),
 ( 0.000000000000000000, 0.2682459062916608961, 1.000000000000000000 ),
 .UNSPECIFIED. ) ;
#12184 = CARTESIAN_POINT ( 'NONE',  ( -8.106549357737529604, 1438.741334074130009, 205.9368686404189930 ) ) ;
#12185 = ORIENTED_EDGE ( 'NONE', *, *, #43802, .T. ) ;
#12186 = CARTESIAN_POINT ( 'NONE',  ( -19.24938132970260085, 1411.370636520449807, 270.3367931074290027 ) ) ;
#12187 = CARTESIAN_POINT ( 'NONE',  ( 3.463848119014229621, 1417.013915635440071, 232.0800632347320231 ) ) ;
#12188 = CARTESIAN_POINT ( 'NONE',  ( 0.02816689439180000351, 1396.454734805430007, 196.6641013465980166 ) ) ;
#12190 = VERTEX_POINT ( 'NONE', #99168 ) ;
#12189 = CARTESIAN_POINT ( 'NONE',  ( -8.706062076307372166, 1365.718773072405384, 207.6218459616988241 ) ) ;
#12191 = ORIENTED_EDGE ( 'NONE', *, *, #43900, .F. ) ;
#12192 = CARTESIAN_POINT ( 'NONE',  ( 44.85566571832070082, 1447.217473659629604, 268.9966131275909902 ) ) ;
#12193 = CARTESIAN_POINT ( 'NONE',  ( -2.029307951927409981, 1467.934477929960167, 220.0622926176330054 ) ) ;
#12194 = CARTESIAN_POINT ( 'NONE',  ( -13.65886266334669941, 1436.196144125749925, 150.4235525661960082 ) ) ;
#12195 = VECTOR ( 'NONE', #87784, 1000.000000000000000 ) ;
#12196 = CARTESIAN_POINT ( 'NONE',  ( -0.008200652638768689967, 1408.924627079619995, 186.2841847630899963 ) ) ;
#12197 = DIRECTION ( 'NONE',  ( 7.303600220002790452E-17, 1.000000000000000000, -3.615388577796539518E-17 ) ) ;
#12198 = DIRECTION ( 'NONE',  ( -0.03489950311976935254, 0.9993908267949999091, 1.331239895961819999E-11 ) ) ;
#12199 = CARTESIAN_POINT ( 'NONE',  ( -0.0001210645912511750048, 1475.561026843769923, 269.2948676583999941 ) ) ;
#12200 = CARTESIAN_POINT ( 'NONE',  ( 11.50684714920000040, 1415.041103189330215, 222.4903113597979996 ) ) ;
#12201 = CARTESIAN_POINT ( 'NONE',  ( 3.981544315609999884, 1446.451571810050154, 183.2730513936979833 ) ) ;
#12202 = CARTESIAN_POINT ( 'NONE',  ( -4.624736897314999595, 1516.994127245590107, 206.2540423059970180 ) ) ;
#12203 = VERTEX_POINT ( 'NONE', #59279 ) ;
#12204 = CYLINDRICAL_SURFACE ( 'NONE', #81280, 2.000000000000003553 ) ;
#12205 = CARTESIAN_POINT ( 'NONE',  ( -23.52416583785102944, 1448.205401278070667, 215.6064549854269785 ) ) ;
#12206 = ORIENTED_EDGE ( 'NONE', *, *, #98933, .T. ) ;
#12207 = CARTESIAN_POINT ( 'NONE',  ( 11.47315440600428715, 1454.673345936858368, 225.8564051334478506 ) ) ;
#12208 = CARTESIAN_POINT ( 'NONE',  ( 18.86688640473582268, 1511.187213306747708, 180.7825021045438518 ) ) ;
#12209 = DIRECTION ( 'NONE',  ( 1.755985294532464991E-16, -1.000000000000000000, 1.338183447452830017E-16 ) ) ;
#12210 = FACE_OUTER_BOUND ( 'NONE', #93558, .T. ) ;
#12211 = CARTESIAN_POINT ( 'NONE',  ( 19.58436876019999673, 1409.761450691529944, 197.7698869336979897 ) ) ;
#12212 = CARTESIAN_POINT ( 'NONE',  ( 21.81076600339999771, 1409.674709119329918, 208.0390244633379950 ) ) ;
#12213 = CARTESIAN_POINT ( 'NONE',  ( 17.00542863269999927, 1410.873424589829938, 226.2926139095980034 ) ) ;
#12214 = CARTESIAN_POINT ( 'NONE',  ( -14.06995080394465525, 1379.599519235348453, 211.7445496221188819 ) ) ;
#12215 = CIRCLE ( 'NONE', #74823, 17.26401014167801762 ) ;
#12216 = CARTESIAN_POINT ( 'NONE',  ( 8.775825618903722258, 1374.031200045389824, 213.9161013477410336 ) ) ;
#12217 = CARTESIAN_POINT ( 'NONE',  ( 2.500000000000000000, 1439.419208462029928, 162.1010771267879704 ) ) ;
#12218 = CIRCLE ( 'NONE', #19325, 2.500000000000002220 ) ;
#12219 = CARTESIAN_POINT ( 'NONE',  ( 4.038637462725000127, 1516.734985836460055, 214.8955147850770118 ) ) ;
#12220 = CARTESIAN_POINT ( 'NONE',  ( -32.85805783624297760, 1523.678648413191695, 217.1983043299907763 ) ) ;
#12221 = ORIENTED_EDGE ( 'NONE', *, *, #110594, .T. ) ;
#12222 = DIRECTION ( 'NONE',  ( 0.01393861123991820168, -0.01013782210637889994, 0.9998514588075779752 ) ) ;
#12223 = CARTESIAN_POINT ( 'NONE',  ( 21.71247731329056307, 1523.982201850120191, 234.6948375436859635 ) ) ;
#12224 = AXIS2_PLACEMENT_3D ( 'NONE', #19257, #11988, #55120 ) ;
#12225 = CARTESIAN_POINT ( 'NONE',  ( -18.05542497264810109, 1416.825784014559986, 209.4840452940109969 ) ) ;
#12226 = ADVANCED_FACE ( 'NONE', ( #90784 ), #16413, .T. ) ;
#12227 = VECTOR ( 'NONE', #100363, 1000.000000000000000 ) ;
#12228 = CARTESIAN_POINT ( 'NONE',  ( 3.669386717837979983, 1517.051704638620095, 202.5807756278150009 ) ) ;
#12229 = CARTESIAN_POINT ( 'NONE',  ( -38.47491875445290077, 1448.367029702490072, 136.4422118765199912 ) ) ;
#12230 = CIRCLE ( 'NONE', #94466, 1.999999999999999556 ) ;
#12231 = CARTESIAN_POINT ( 'NONE',  ( 11.60004869885203682, 1425.261174633484188, 138.0376396451788139 ) ) ;
#12232 = CARTESIAN_POINT ( 'NONE',  ( 11.73700276280139931, 1426.696010850159837, 144.1682878426319974 ) ) ;
#12233 = CARTESIAN_POINT ( 'NONE',  ( -2.902293737380750027, 1471.341547563029962, 183.8916672433869905 ) ) ;
#12234 = CARTESIAN_POINT ( 'NONE',  ( 11.06271855039999963, 1433.091631396069943, 151.7087564066980008 ) ) ;
#12235 = EDGE_CURVE ( 'NONE', #43726, #39623, #39840, .T. ) ;
#12236 = CARTESIAN_POINT ( 'NONE',  ( -19.58397906120409715, 1471.164316944340044, 270.0578164987000491 ) ) ;
#12237 = CARTESIAN_POINT ( 'NONE',  ( -32.86802468386297704, 1512.187213306747481, 201.0396662540046577 ) ) ;
#12238 = CARTESIAN_POINT ( 'NONE',  ( -109.1685115749999966, 1385.071170989440134, 297.1353643137590552 ) ) ;
#12239 = CARTESIAN_POINT ( 'NONE',  ( 11.78397860869369929, 1499.475900767659823, 204.3830586676889993 ) ) ;
#12240 = ORIENTED_EDGE ( 'NONE', *, *, #104640, .F. ) ;
#12241 = FACE_OUTER_BOUND ( 'NONE', #56637, .T. ) ;
#12242 = CARTESIAN_POINT ( 'NONE',  ( 12.37499353609999986, 1445.063428794549964, 150.7815459944920065 ) ) ;
#12243 = DIRECTION ( 'NONE',  ( 5.980589973904019347E-17, -1.000000000000000000, 1.736889445713099699E-16 ) ) ;
#12244 = CARTESIAN_POINT ( 'NONE',  ( 8.006052564334819266, 1398.150843778026456, 198.8796111588884230 ) ) ;
#12245 = CARTESIAN_POINT ( 'NONE',  ( 1.907725587109999843, 1490.900299108929858, 235.6062317305980116 ) ) ;
#12246 = AXIS2_PLACEMENT_3D ( 'NONE', #89299, #56253, #28850 ) ;
#12247 = B_SPLINE_CURVE_WITH_KNOTS ( 'NONE', 5,
 ( #69512, #60556, #94677, #96338, #17390, #70072 ),
 .UNSPECIFIED., .F., .F.,
 ( 6, 6 ),
 ( 0.000000000000000000, 11.48858425020000240 ),
 .UNSPECIFIED. ) ;
#12248 = CARTESIAN_POINT ( 'NONE',  ( -10.58047146200000022, 1509.111071725129932, 235.4109798456979945 ) ) ;
#12249 = CARTESIAN_POINT ( 'NONE',  ( -24.45121130426860034, 1383.848703213860063, 223.1218506052400130 ) ) ;
#12250 = CARTESIAN_POINT ( 'NONE',  ( 20.34262379729999992, 1485.757879992529979, 225.3684058912980106 ) ) ;
#12251 = CARTESIAN_POINT ( 'NONE',  ( 5.390423872767819979, 1422.474059485570024, 133.9852895348969923 ) ) ;
#12252 = CARTESIAN_POINT ( 'NONE',  ( -2.038646110889675178, 1525.960063244516959, 177.0579350083066004 ) ) ;
#12253 = CARTESIAN_POINT ( 'NONE',  ( 2.379842363999999932, 1464.647331468930133, 236.2541381392979929 ) ) ;
#12255 = EDGE_LOOP ( 'NONE', ( #5840, #72953, #99202, #55030 ) ) ;
#12254 = CARTESIAN_POINT ( 'NONE',  ( -41.66021910349999757, 1443.875694946319754, 135.6929188412979954 ) ) ;
#12256 = CARTESIAN_POINT ( 'NONE',  ( -1.271037680349999865, 1450.748653814689987, 181.7779247749980129 ) ) ;
#12257 = CARTESIAN_POINT ( 'NONE',  ( -45.10563462580000049, 1381.548674952109877, 219.7946006703589887 ) ) ;
#12258 = CARTESIAN_POINT ( 'NONE',  ( -3.444563290230000074, 1476.680507959189981, 199.3428731527990010 ) ) ;
#12260 = VERTEX_POINT ( 'NONE', #74003 ) ;
#12259 = DIRECTION ( 'NONE',  ( -0.8742006210163753011, -0.3833097456314917273, -0.2980719931803466616 ) ) ;
#12261 = CARTESIAN_POINT ( 'NONE',  ( 10.59810956035219753, 1477.523927547069889, 229.9254287524879885 ) ) ;
#12262 = VERTEX_POINT ( 'NONE', #93397 ) ;
#12263 = CARTESIAN_POINT ( 'NONE',  ( -11.37061168853300153, 1391.632271866039900, 214.0126550961279861 ) ) ;
#12264 = CARTESIAN_POINT ( 'NONE',  ( -10.66875363927314169, 1391.196586595016470, 215.3138778947951550 ) ) ;
#12265 = CARTESIAN_POINT ( 'NONE',  ( 32.02808312589916540, 1511.187213306747708, 198.2787714533495489 ) ) ;
#12266 = CARTESIAN_POINT ( 'NONE',  ( -1.189318188510000152, 1432.130355740389859, 218.1858096881190079 ) ) ;
#12267 = CARTESIAN_POINT ( 'NONE',  ( 20.65879167559999985, 1494.308160183190012, 205.1000562319489973 ) ) ;
#12268 = CARTESIAN_POINT ( 'NONE',  ( 14.34763326340369893, 1409.414090780570177, 213.2724514398500162 ) ) ;
#12269 = CARTESIAN_POINT ( 'NONE',  ( 12.55979069370000012, 1458.679714032590027, 224.9161459441990019 ) ) ;
#12270 = CARTESIAN_POINT ( 'NONE',  ( -87.21881660688978855, 1385.183764852800095, 290.6465622116569989 ) ) ;
#12271 = CARTESIAN_POINT ( 'NONE',  ( -18.87572180689999968, 1452.014070220629947, 191.8431515786979844 ) ) ;
#12272 = CARTESIAN_POINT ( 'NONE',  ( -68.77626911307648072, 1379.747998350314901, 280.2622293725648888 ) ) ;
#12273 = CARTESIAN_POINT ( 'NONE',  ( 13.35741048202589809, 1443.913060387329324, 164.9741927960640453 ) ) ;
#12274 = EDGE_LOOP ( 'NONE', ( #36625, #101627, #12888, #6946 ) ) ;
#12275 = ORIENTED_EDGE ( 'NONE', *, *, #94125, .T. ) ;
#12276 = CARTESIAN_POINT ( 'NONE',  ( -3.330134203884999700, 1515.051704408389924, 204.7920544413669859 ) ) ;
#12277 = CARTESIAN_POINT ( 'NONE',  ( 18.22279825098010164, 1457.639640533290049, 229.9734878635680104 ) ) ;
#12278 = CARTESIAN_POINT ( 'NONE',  ( 1.049829441584229750, 1496.809906337439998, 196.7866365865189948 ) ) ;
#12279 = CARTESIAN_POINT ( 'NONE',  ( 29.83693158363007569, 1462.368600761292100, 269.4690755030636637 ) ) ;
#12280 = CARTESIAN_POINT ( 'NONE',  ( -20.51885332321579725, 1505.236437000949991, 190.4655934336639689 ) ) ;
#12281 = CARTESIAN_POINT ( 'NONE',  ( 2.551411588599999725, 1397.989669479629811, 221.9716508525979748 ) ) ;
#12282 = CARTESIAN_POINT ( 'NONE',  ( 32.18357971099926118, 1524.059663615499630, 201.4963562058872526 ) ) ;
#12283 = CARTESIAN_POINT ( 'NONE',  ( -1.459671184189999860, 1476.698137529930136, 182.8094855557980054 ) ) ;
#12284 = CARTESIAN_POINT ( 'NONE',  ( -11.95743746174541933, 1364.171459020583370, 209.6218459617033432 ) ) ;
#12285 = CARTESIAN_POINT ( 'NONE',  ( -25.00976051679999657, 1436.598010167069788, 137.9330532114979917 ) ) ;
#12286 = DIRECTION ( 'NONE',  ( 8.727810504445229884E-47, -1.000000000000000000, 1.836970198721029688E-16 ) ) ;
#12287 = CARTESIAN_POINT ( 'NONE',  ( -5.789394700334999477, 1517.164987839469859, 207.4150481461570052 ) ) ;
#12288 = AXIS2_PLACEMENT_3D ( 'NONE', #43017, #59278, #76060 ) ;
#12289 = CARTESIAN_POINT ( 'NONE',  ( -12.84236090119540030, 1435.935773415550102, 150.8115148268369978 ) ) ;
#12290 = CARTESIAN_POINT ( 'NONE',  ( 30.95751052620453692, 1525.821544997590536, 201.4531494772885196 ) ) ;
#12291 = FACE_OUTER_BOUND ( 'NONE', #36705, .T. ) ;
#12292 = CARTESIAN_POINT ( 'NONE',  ( -0.3621993323151809774, 1416.825784014559986, 191.0664209890499876 ) ) ;
#12294 = CARTESIAN_POINT ( 'NONE',  ( 18.64588652299999794, 1416.828040475229955, 209.6843149956849857 ) ) ;
#12293 = VECTOR ( 'NONE', #37518, 1000.000000000000000 ) ;
#12295 = CARTESIAN_POINT ( 'NONE',  ( -107.5634112720000104, 1382.701802836779962, 297.7923862875589975 ) ) ;
#12296 = ORIENTED_EDGE ( 'NONE', *, *, #2389, .T. ) ;
#12297 = AXIS2_PLACEMENT_3D ( 'NONE', #11283, #18539, #104776 ) ;
#12298 = CARTESIAN_POINT ( 'NONE',  ( 16.98088721830000125, 1414.156372837330082, 255.1565004954979941 ) ) ;
#12299 = CARTESIAN_POINT ( 'NONE',  ( -25.61862525230000287, 1449.804154372189942, 208.1054677997580029 ) ) ;
#12301 = CARTESIAN_POINT ( 'NONE',  ( -16.60786730719999937, 1409.493019893330029, 195.7756164720979939 ) ) ;
#12300 = CARTESIAN_POINT ( 'NONE',  ( -10.88730305954610067, 1426.101976979720121, 91.15062580800939429 ) ) ;
#12302 = EDGE_CURVE ( 'NONE', #8198, #76159, #47014, .T. ) ;
#12303 = DIRECTION ( 'NONE',  ( -1.000000000000000000, -2.657783323254384930E-32, -1.224646799147351975E-16 ) ) ;
#12304 = CARTESIAN_POINT ( 'NONE',  ( -1.011872109909999887E-09, 1411.425361493330001, 255.2684082166979920 ) ) ;
#12305 = CARTESIAN_POINT ( 'NONE',  ( 3.305605061710000125, 1485.263013822589983, 219.7395602488990107 ) ) ;
#12306 = EDGE_CURVE ( 'NONE', #46444, #36359, #16663, .T. ) ;
#12307 = EDGE_CURVE ( 'NONE', #33249, #65829, #98685, .T. ) ;
#12308 = CARTESIAN_POINT ( 'NONE',  ( 2.935146075021433543, 1447.712003106908014, 154.8057247725446643 ) ) ;
#12309 = CARTESIAN_POINT ( 'NONE',  ( -23.01872370112488753, 1409.746765365450756, 208.8717086315775759 ) ) ;
#12310 = ORIENTED_EDGE ( 'NONE', *, *, #67340, .T. ) ;
#12311 = CARTESIAN_POINT ( 'NONE',  ( 173.8335085727383955, 1526.382868172863937, 100.8557906292069930 ) ) ;
#12312 = CARTESIAN_POINT ( 'NONE',  ( 11.80657790919278582, 1512.979858876890376, 225.6266235005796830 ) ) ;
#12313 = CARTESIAN_POINT ( 'NONE',  ( 38.59236949370160374, 1443.548215515760148, 137.1678974980540033 ) ) ;
#12314 = EDGE_LOOP ( 'NONE', ( #106570, #29558, #27303, #64706, #10983 ) ) ;
#12315 = ORIENTED_EDGE ( 'NONE', *, *, #104866, .T. ) ;
#12316 = CARTESIAN_POINT ( 'NONE',  ( -10.85852385830536448, 1424.794007418652882, 138.1924915167475660 ) ) ;
#12317 = CARTESIAN_POINT ( 'NONE',  ( -23.01870917701389985, 1409.746761054060244, 208.8717042921039990 ) ) ;
#12318 = ORIENTED_EDGE ( 'NONE', *, *, #7705, .F. ) ;
#12319 = CARTESIAN_POINT ( 'NONE',  ( -0.3052841619420000319, 1412.052214267130012, 184.9138573875980285 ) ) ;
#12320 = AXIS2_PLACEMENT_3D ( 'NONE', #93297, #94388, #33944 ) ;
#12321 = CARTESIAN_POINT ( 'NONE',  ( 10.27910644096741422, 1446.578925969647344, 153.2874156164771193 ) ) ;
#12322 = CARTESIAN_POINT ( 'NONE',  ( -3.369831055830000199, 1489.060830314729856, 235.9240531713980147 ) ) ;
#12323 = CARTESIAN_POINT ( 'NONE',  ( 16.64885258017236680, 1526.344110814218311, 234.9109520333671810 ) ) ;
#12324 = ORIENTED_EDGE ( 'NONE', *, *, #66245, .F. ) ;
#12325 = CARTESIAN_POINT ( 'NONE',  ( -11.61527099314350053, 1414.971349104630008, 221.0857754848229888 ) ) ;
#12326 = CARTESIAN_POINT ( 'NONE',  ( 15.25222867979999819, 1496.677411259530118, 225.2158252260980191 ) ) ;
#12327 = ORIENTED_EDGE ( 'NONE', *, *, #2746, .T. ) ;
#12328 = CARTESIAN_POINT ( 'NONE',  ( 1.704794803334999997, 1517.096587378560116, 204.4952540647470016 ) ) ;
#12329 = ORIENTED_EDGE ( 'NONE', *, *, #103785, .F. ) ;
#12330 = CARTESIAN_POINT ( 'NONE',  ( 11.86031229030020029, 1431.931911824779945, 149.9673457447429996 ) ) ;
#12331 = CARTESIAN_POINT ( 'NONE',  ( 5.513435553965000402, 1508.551704408389924, 202.1089243864769855 ) ) ;
#12332 = ORIENTED_EDGE ( 'NONE', *, *, #81136, .F. ) ;
#12333 = VERTEX_POINT ( 'NONE', #84989 ) ;
#12334 = CARTESIAN_POINT ( 'NONE',  ( -10.51558556386050114, 1480.736735032730166, 208.3484430820659838 ) ) ;
#12335 = CARTESIAN_POINT ( 'NONE',  ( 16.81497685297909683, 1526.382868172864164, 234.5399785031295892 ) ) ;
#12336 = CARTESIAN_POINT ( 'NONE',  ( 5.024924619706210294, 1497.858354990089992, 198.0416419176340241 ) ) ;
#12337 = EDGE_CURVE ( 'NONE', #26502, #73768, #403, .T. ) ;
#12338 = CARTESIAN_POINT ( 'NONE',  ( -2.779626312165170088, 1468.659898279970093, 219.1847641695690072 ) ) ;
#12339 = CARTESIAN_POINT ( 'NONE',  ( 18.16558062136190088, 1452.278704333800079, 145.2414311030810268 ) ) ;
#12340 = CARTESIAN_POINT ( 'NONE',  ( 9.213396914969999685, 1420.767274165939853, 196.7655569023989983 ) ) ;
#12341 = LINE ( 'NONE', #46532, #101366 ) ;
#12342 = CARTESIAN_POINT ( 'NONE',  ( -5.693783788968350912, 1494.776061667409977, 198.1946402388329886 ) ) ;
#12343 = CARTESIAN_POINT ( 'NONE',  ( -10.96966273854589957, 1432.359729197300112, 151.7701366752919796 ) ) ;
#12344 = CARTESIAN_POINT ( 'NONE',  ( 0.03526024722610697493, 1409.948177333189051, 233.1655130677910108 ) ) ;
#12346 = CARTESIAN_POINT ( 'NONE',  ( -106.2561851244600035, 1391.913059884029963, 305.4819836422510093 ) ) ;
#12345 = CARTESIAN_POINT ( 'NONE',  ( -19.19558940460000329, 1505.173093966990109, 209.0368464700519837 ) ) ;
#12347 = CARTESIAN_POINT ( 'NONE',  ( -67.99816612433596674, 1379.747625308294573, 279.4122903084538052 ) ) ;
#12348 = B_SPLINE_CURVE_WITH_KNOTS ( 'NONE', 3,
 ( #110559, #58516, #101036, #41701, #56861, #84250, #41150, #66382, #76404, #100501, #8089, #24336, #49569, #40045, #74227, #83697, #6993, #92646, #15920, #50122, #24870, #82609 ),
 .UNSPECIFIED., .F., .F.,
 ( 4, 2, 1, 1, 2, 2, 2, 2, 1, 1, 2, 2, 4 ),
 ( 0.000000000000000000, 0.1250000000000019151, 0.1874999999999887867, 0.2187499999999827360, 0.2343749999999658884, 0.2499999999999490685, 0.4999999999998919198, 0.6249999999998638867, 0.6874999999998662181, 0.7187499999998674394, 0.7343749999998693268, 0.7499999999998712141, 1.000000000000000000 ),
 .UNSPECIFIED. ) ;
#12349 = CARTESIAN_POINT ( 'NONE',  ( -24.51492576923349986, 1509.184387879659880, 222.5504090698890138 ) ) ;
#12350 = CARTESIAN_POINT ( 'NONE',  ( -6.867779409725000228, 1512.132770473870096, 201.9588434351270223 ) ) ;
#12351 = ORIENTED_EDGE ( 'NONE', *, *, #79504, .F. ) ;
#12352 = CARTESIAN_POINT ( 'NONE',  ( 28.02005514660000074, 1440.913060387330006, 248.0989693021979861 ) ) ;
#12353 = CIRCLE ( 'NONE', #74969, 1.000000000000007994 ) ;
#12354 = DIRECTION ( 'NONE',  ( 6.123233995736769734E-17, 1.000000000000000000, 1.124819836996399911E-32 ) ) ;
#12355 = CARTESIAN_POINT ( 'NONE',  ( -80.80534708309519942, 1384.991848082589968, 304.3854582852239901 ) ) ;
#12356 = B_SPLINE_SURFACE_WITH_KNOTS ( 'NONE', 5, 1, ( 
 ( #68568, #59059 ),
 ( #76392, #102130 ),
 ( #51761, #103226 ),
 ( #19220, #20338 ),
 ( #96514, #36603 ),
 ( #63498, #105470 ),
 ( #38247, #70249 ),
 ( #62390, #46684 ),
 ( #89757, #19793 ) ),
 .UNSPECIFIED., .F., .F., .F.,
 ( 6, 3, 6 ),
 ( 2, 2 ),
 ( 0.000000000000000000, 3.688278477100000341, 7.358176137350000090 ),
 ( 0.000000000000000000, 14.00000000000000000 ),
 .UNSPECIFIED. ) ;
#12357 = CARTESIAN_POINT ( 'NONE',  ( -1.676215897828090107, 1450.511945644329899, 182.4451613505460159 ) ) ;
#12358 = CARTESIAN_POINT ( 'NONE',  ( 4.507890822339999382, 1506.158184558590165, 220.0129750286989747 ) ) ;
#12359 = DIRECTION ( 'NONE',  ( 0.000000000000000000, 0.000000000000000000, 1.000000000000000000 ) ) ;
#12361 = ORIENTED_EDGE ( 'NONE', *, *, #74879, .F. ) ;
#12360 = CARTESIAN_POINT ( 'NONE',  ( -17.78871670860239718, 1419.650462417609788, 206.8064655431160190 ) ) ;
#12362 = CARTESIAN_POINT ( 'NONE',  ( 10.11781796957937551, 1428.435797280887527, 137.0999999980966777 ) ) ;
#12363 = CARTESIAN_POINT ( 'NONE',  ( -2.689480282155449764, 1439.963151421470002, 157.5730576003849990 ) ) ;
#12364 = CIRCLE ( 'NONE', #67776, 0.4999999999999980016 ) ;
#12365 = CARTESIAN_POINT ( 'NONE',  ( -1.013621472345935359, 1450.828806111348285, 154.2477477248477555 ) ) ;
#12366 = CARTESIAN_POINT ( 'NONE',  ( 0.1351882977586719992, 1430.428589182629821, 199.6983684263929888 ) ) ;
#12367 = ADVANCED_FACE ( 'NONE', ( #93944 ), #33805, .T. ) ;
#12368 = CARTESIAN_POINT ( 'NONE',  ( 13.51662153773500030, 1512.620989416249813, 225.5656590752669786 ) ) ;
#12369 = CARTESIAN_POINT ( 'NONE',  ( 4.459680871607520913, 1370.469415166398903, 208.9741522785391510 ) ) ;
#12370 = CARTESIAN_POINT ( 'NONE',  ( 27.74304799147289913, 1509.894878401100186, 194.6056596535900098 ) ) ;
#12371 = CARTESIAN_POINT ( 'NONE',  ( 8.340772919400350816, 1460.715584676179787, 204.0670572953980013 ) ) ;
#12372 = CARTESIAN_POINT ( 'NONE',  ( -4.762729318109999888, 1475.513060387329915, 229.9230423263979901 ) ) ;
#12373 = CARTESIAN_POINT ( 'NONE',  ( 17.00050166700000176, 1419.772799493030107, 226.7240349780979898 ) ) ;
#12374 = B_SPLINE_CURVE_WITH_KNOTS ( 'NONE', 5,
 ( #91410, #14687, #48876, #55076, #38240, #72422, #106553, #83538, #110403, #33682, #101423, #59473 ),
 .UNSPECIFIED., .F., .F.,
 ( 6, 3, 3, 6 ),
 ( 5.812632519320040103, 6.561021380799999747, 7.569428689259999565, 8.073627588195819271 ),
 .UNSPECIFIED. ) ;
#12375 = CARTESIAN_POINT ( 'NONE',  ( 10.00676819928309946, 1469.384229055800233, 210.0288051735269903 ) ) ;
#12376 = CARTESIAN_POINT ( 'NONE',  ( -21.30823923614777371, 1524.382868172804365, 233.7929508216643342 ) ) ;
#12377 = CARTESIAN_POINT ( 'NONE',  ( 2.476170596904999854, 1516.819260244609950, 207.4047612206870213 ) ) ;
#12378 = CARTESIAN_POINT ( 'NONE',  ( 45.67177355289999241, 1440.913081031829961, 266.1885934315979512 ) ) ;
#12379 = CARTESIAN_POINT ( 'NONE',  ( -17.84543917770000121, 1409.701167236529727, 223.9496858625980167 ) ) ;
#12380 = CARTESIAN_POINT ( 'NONE',  ( 16.10667296019999739, 1435.057002741109955, 146.9490725771979953 ) ) ;
#12381 = AXIS2_PLACEMENT_3D ( 'NONE', #108747, #32039, #7388 ) ;
#12382 = CARTESIAN_POINT ( 'NONE',  ( 21.81574974289999957, 1508.011787535030180, 191.7684141494979997 ) ) ;
#12383 = CARTESIAN_POINT ( 'NONE',  ( -16.34132978743479825, 1409.483684619830001, 192.7109133032730028 ) ) ;
#12384 = AXIS2_PLACEMENT_3D ( 'NONE', #94202, #42719, #34305 ) ;
#12385 = CARTESIAN_POINT ( 'NONE',  ( -6.179141267909999513, 1475.525926640629905, 266.9460417852980072 ) ) ;
#12386 = CARTESIAN_POINT ( 'NONE',  ( -14.22077585328280058, 1416.525864124620057, 203.1782020047139952 ) ) ;
#12387 = CARTESIAN_POINT ( 'NONE',  ( -36.93201630645109645, 1436.283700798310065, 135.4717700503809965 ) ) ;
#12388 = CARTESIAN_POINT ( 'NONE',  ( 0.2109277773507400033, 1456.827200395890031, 183.0892095144770053 ) ) ;
#12389 = CARTESIAN_POINT ( 'NONE',  ( -9.197920992606320567, 1408.707683617470138, 199.0017040286450083 ) ) ;
#12390 = CARTESIAN_POINT ( 'NONE',  ( 9.402787699681429245, 1428.181318586850011, 212.5511139594050007 ) ) ;
#12391 = CARTESIAN_POINT ( 'NONE',  ( 19.39983987835400114, 1522.382868172864164, 178.9515629539735642 ) ) ;
#12392 = CARTESIAN_POINT ( 'NONE',  ( 22.03465957474570658, 1522.382868172863937, 235.4136513321629991 ) ) ;
#12393 = CARTESIAN_POINT ( 'NONE',  ( 13.80599399779999992, 1434.979619872729927, 146.4346930199980079 ) ) ;
#12394 = CARTESIAN_POINT ( 'NONE',  ( -28.14962045949999592, 1435.955305551769925, 136.4811531283980059 ) ) ;
#12395 = CARTESIAN_POINT ( 'NONE',  ( 10.45867790589999835, 1442.264568908580031, 186.5135257037979670 ) ) ;
#12396 = ORIENTED_EDGE ( 'NONE', *, *, #43476, .T. ) ;
#12397 = CARTESIAN_POINT ( 'NONE',  ( 6.178095833435953033, 1510.835436364192674, 216.5837886796534804 ) ) ;
#12398 = CARTESIAN_POINT ( 'NONE',  ( -10.59587896540769947, 1409.283076634259942, 219.6744605712179919 ) ) ;
#12399 = CARTESIAN_POINT ( 'NONE',  ( 32.74318896774778409, 1524.667648926106949, 196.1902622063073807 ) ) ;
#12400 = ADVANCED_FACE ( 'NONE', ( #52527 ), #58830, .F. ) ;
#12401 = CARTESIAN_POINT ( 'NONE',  ( -13.58042247833220095, 1508.551704408300111, 210.3416305655150040 ) ) ;
#12402 = CARTESIAN_POINT ( 'NONE',  ( 15.96280133942260271, 1508.735390535940041, 232.0448960862960064 ) ) ;
#12403 = CARTESIAN_POINT ( 'NONE',  ( -37.88641905019999712, 1461.898525134130068, 267.8844275163979773 ) ) ;
#12404 = CARTESIAN_POINT ( 'NONE',  ( -15.52964687406499955, 1451.324136384999974, 222.4830579234560162 ) ) ;
#12405 = CARTESIAN_POINT ( 'NONE',  ( 18.95884613770000016, 1416.837177098729853, 210.4637958795879911 ) ) ;
#12406 = ADVANCED_FACE ( 'NONE', ( #80482 ), #13243, .T. ) ;
#12407 = CARTESIAN_POINT ( 'NONE',  ( 2.652938167623881238, 1396.005703029557708, 216.7884906539198369 ) ) ;
#12408 = CARTESIAN_POINT ( 'NONE',  ( -96.47684263679849437, 1384.607351846010033, 310.3230601989450292 ) ) ;
#12409 = CARTESIAN_POINT ( 'NONE',  ( -39.25154068821980502, 1384.988109809909929, 212.1860968133940162 ) ) ;
#12410 = CARTESIAN_POINT ( 'NONE',  ( -12.20257788280040145, 1490.746699033079949, 207.9129267422960083 ) ) ;
#12411 = CARTESIAN_POINT ( 'NONE',  ( -3.490046645198510156, 1508.551704408389924, 204.3447946308859855 ) ) ;
#12412 = CARTESIAN_POINT ( 'NONE',  ( -28.97445500416739961, 1509.604966152339784, 208.6943162784619972 ) ) ;
#12413 = CARTESIAN_POINT ( 'NONE',  ( 1.775988990184984795, 1526.208281990536761, 177.6737791622277882 ) ) ;
#12415 = EDGE_LOOP ( 'NONE', ( #21183, #8888, #105550, #2388, #110528 ) ) ;
#12414 = CARTESIAN_POINT ( 'NONE',  ( 7.878537825433329367, 1517.151704408390060, 200.0586249522280013 ) ) ;
#12416 = CARTESIAN_POINT ( 'NONE',  ( -109.9853374259999867, 1384.903358540060026, 311.4562094292589904 ) ) ;
#12417 = CARTESIAN_POINT ( 'NONE',  ( 0.000000000000000000, 1412.913060387329779, 209.1218459616989946 ) ) ;
#12418 = CARTESIAN_POINT ( 'NONE',  ( -112.3594079535740207, 1391.913060387289988, 305.9298179104569613 ) ) ;
#12419 = CARTESIAN_POINT ( 'NONE',  ( 2.372478608332516892, 1512.187213306747481, 174.8996806668726549 ) ) ;
#12420 = CARTESIAN_POINT ( 'NONE',  ( -17.54273015099310129, 1417.931783278020021, 206.8684746656099946 ) ) ;
#12421 = VECTOR ( 'NONE', #77683, 1000.000000000000114 ) ;
#12422 = CARTESIAN_POINT ( 'NONE',  ( 22.82660133449999762, 1409.710182870830067, 210.6508517238679872 ) ) ;
#12423 = CARTESIAN_POINT ( 'NONE',  ( 2.632747685671116056, 1389.413060387289988, 210.5601225775116063 ) ) ;
#12424 = CARTESIAN_POINT ( 'NONE',  ( -18.64099322077279908, 1468.021338938559893, 201.0622087414649855 ) ) ;
#12425 = CYLINDRICAL_SURFACE ( 'NONE', #3536, 2.000000000000002220 ) ;
#12427 = CARTESIAN_POINT ( 'NONE',  ( 19.37374569213924502, 1526.382868172863937, 183.8768763279539655 ) ) ;
#12426 = CARTESIAN_POINT ( 'NONE',  ( -11.31243770530000070, 1433.012837821759831, 151.5204583838979886 ) ) ;
#12428 = CARTESIAN_POINT ( 'NONE',  ( 27.95579582530499962, 1508.164266001930173, 207.9317693576919908 ) ) ;
#12429 = CARTESIAN_POINT ( 'NONE',  ( -101.1419410403000541, 1375.179104070690755, 291.9637869975591684 ) ) ;
#12430 = DIRECTION ( 'NONE',  ( 0.8090169943749551118, -0.000000000000000000, 0.5877852522924625900 ) ) ;
#12431 = CARTESIAN_POINT ( 'NONE',  ( -22.65374348950000183, 1411.052683204430195, 211.5465440029780098 ) ) ;
#12432 = CARTESIAN_POINT ( 'NONE',  ( 9.258247136800001442, 1363.198586359130104, 210.6218459616991936 ) ) ;
#12433 = CARTESIAN_POINT ( 'NONE',  ( 2.479246847704999812, 1516.983612918759945, 205.0778556245070092 ) ) ;
#12434 = CARTESIAN_POINT ( 'NONE',  ( 13.41316562022890047, 1508.156439062169966, 233.1856428097420064 ) ) ;
#12435 = ADVANCED_FACE ( 'NONE', ( #81556 ), #108429, .T. ) ;
#12436 = CARTESIAN_POINT ( 'NONE',  ( -14.64177459002939941, 1485.585968447049936, 186.6436936439779686 ) ) ;
#12437 = ORIENTED_EDGE ( 'NONE', *, *, #102136, .T. ) ;
#12438 = CARTESIAN_POINT ( 'NONE',  ( 7.947250527635000950, 1514.433282224309778, 206.1243428727769924 ) ) ;
#12439 = AXIS2_PLACEMENT_3D ( 'NONE', #12899, #48177, #99095 ) ;
#12440 = CARTESIAN_POINT ( 'NONE',  ( -10.67342804297004655, 1422.346099354243051, 210.6393889615464730 ) ) ;
#12442 = ORIENTED_EDGE ( 'NONE', *, *, #13778, .T. ) ;
#12441 = CARTESIAN_POINT ( 'NONE',  ( -67.81516288620989030, 1379.745697675489964, 279.2085842206279835 ) ) ;
#12443 = ORIENTED_EDGE ( 'NONE', *, *, #40559, .F. ) ;
#12444 = CARTESIAN_POINT ( 'NONE',  ( 27.93978865640000109, 1508.083000434530049, 211.1815961025180286 ) ) ;
#12445 = ORIENTED_EDGE ( 'NONE', *, *, #43609, .T. ) ;
#12446 = CARTESIAN_POINT ( 'NONE',  ( -105.0581302270000066, 1379.236400489019843, 304.0328620110590236 ) ) ;
#12447 = EDGE_CURVE ( 'NONE', #89941, #24269, #102268, .T. ) ;
#12448 = CARTESIAN_POINT ( 'NONE',  ( 1.527505831956530002, 1414.913527275050001, 192.0113405201620083 ) ) ;
#12450 = CARTESIAN_POINT ( 'NONE',  ( 1.005224880929999953, 1508.991333441630104, 179.4394713248979940 ) ) ;
#12449 = CARTESIAN_POINT ( 'NONE',  ( 15.95479805056280043, 1420.121857128410056, 191.2307307053519878 ) ) ;
#12451 = CARTESIAN_POINT ( 'NONE',  ( 10.92766316885620093, 1501.618323021010156, 205.6861136770480130 ) ) ;
#12452 =( BOUNDED_CURVE ( )  B_SPLINE_CURVE ( 3, ( #97901, #55380, #62712, #3886 ),
 .UNSPECIFIED., .F., .T. ) 
 B_SPLINE_CURVE_WITH_KNOTS ( ( 4, 4 ),
 ( 4.173463862610059749, 5.251314181851939544 ),
 .UNSPECIFIED. ) 
 CURVE ( )  GEOMETRIC_REPRESENTATION_ITEM ( )  RATIONAL_B_SPLINE_CURVE ( ( 1.000000000000000000, 0.9055071999559949347, 0.9055071999559949347, 1.000000000000000000 ) ) 
 REPRESENTATION_ITEM ( '' )  );
#12453 = ADVANCED_FACE ( 'NONE', ( #3799 ), #84376, .T. ) ;
#12454 = AXIS2_PLACEMENT_3D ( 'NONE', #1251, #44361, #1816 ) ;
#12455 = CARTESIAN_POINT ( 'NONE',  ( -25.08193098539699761, 1451.798897095909979, 136.5882795326729990 ) ) ;
#12456 = CARTESIAN_POINT ( 'NONE',  ( -1.335546054589999976, 1468.359610537590015, 219.4358368445990095 ) ) ;
#12457 = CARTESIAN_POINT ( 'NONE',  ( 12.14295705810000037, 1409.337101792229987, 227.8566549244980024 ) ) ;
#12458 = CARTESIAN_POINT ( 'NONE',  ( 7.311558199926071033, 1484.801511308949785, 217.1227323129160141 ) ) ;
#12459 = ADVANCED_FACE ( 'NONE', ( #31711 ), #24972, .T. ) ;
#12460 = CARTESIAN_POINT ( 'NONE',  ( 40.85417709044089918, 1440.196123996860024, 134.0999999980799657 ) ) ;
#12461 = DIRECTION ( 'NONE',  ( 1.836970198721029688E-16, 1.000000000000000000, -2.953460612019999929E-19 ) ) ;
#12462 = VERTEX_POINT ( 'NONE', #36687 ) ;
#12463 = CARTESIAN_POINT ( 'NONE',  ( 0.9103496401472069843, 1462.760058940530143, 230.5111392918950060 ) ) ;
#12464 = AXIS2_PLACEMENT_3D ( 'NONE', #82281, #23997, #82823 ) ;
#12465 = CARTESIAN_POINT ( 'NONE',  ( -17.29674189031538489, 1410.881757619984910, 225.9250326850611827 ) ) ;
#12466 = ORIENTED_EDGE ( 'NONE', *, *, #70639, .F. ) ;
#12467 = ORIENTED_EDGE ( 'NONE', *, *, #72735, .T. ) ;
#12468 = ORIENTED_EDGE ( 'NONE', *, *, #91161, .T. ) ;
#12469 = EDGE_CURVE ( 'NONE', #33967, #61502, #79808, .T. ) ;
#12470 = CARTESIAN_POINT ( 'NONE',  ( -5.919280326385000457, 1513.965983108850196, 216.7636238285669776 ) ) ;
#12471 = CARTESIAN_POINT ( 'NONE',  ( 16.78598026525966702, 1513.543684533296073, 195.9142244523475824 ) ) ;
#12472 = CARTESIAN_POINT ( 'NONE',  ( 7.871325772944452126, 1451.393740844790500, 152.9831421267123517 ) ) ;
#12473 = FACE_OUTER_BOUND ( 'NONE', #61275, .T. ) ;
#12474 = AXIS2_PLACEMENT_3D ( 'NONE', #8099, #49033, #92657 ) ;
#12475 = EDGE_CURVE ( 'NONE', #22102, #57273, #5547, .T. ) ;
#12476 = CARTESIAN_POINT ( 'NONE',  ( -18.04424466527178694, 1447.053540243377711, 216.4274986648658796 ) ) ;
#12477 = CARTESIAN_POINT ( 'NONE',  ( -68.14071486192135296, 1379.746697161519705, 278.7208864299544189 ) ) ;
#12478 = CARTESIAN_POINT ( 'NONE',  ( -4.805077596034999843, 1510.399296111369949, 201.5734650597370035 ) ) ;
#12479 = CARTESIAN_POINT ( 'NONE',  ( 8.506179033730001393, 1416.518532928429977, 193.0747662988979982 ) ) ;
#12480 = EDGE_CURVE ( 'NONE', #86431, #59011, #28998, .T. ) ;
#12481 = CARTESIAN_POINT ( 'NONE',  ( -61.39005965052979974, 1384.681648932039934, 247.0307441228220000 ) ) ;
#12482 = ORIENTED_EDGE ( 'NONE', *, *, #93254, .F. ) ;
#12483 = CARTESIAN_POINT ( 'NONE',  ( -3.463767296015000330, 1517.014196759610059, 207.4190915607570105 ) ) ;
#12484 = ORIENTED_EDGE ( 'NONE', *, *, #28927, .F. ) ;
#12485 = CARTESIAN_POINT ( 'NONE',  ( 29.57591471954300033, 1440.913060387330006, 251.2017233884100165 ) ) ;
#12486 = CARTESIAN_POINT ( 'NONE',  ( -19.00191528430000076, 1508.825455351729943, 187.6945225472979928 ) ) ;
#12487 = ORIENTED_EDGE ( 'NONE', *, *, #109837, .T. ) ;
#12488 = CARTESIAN_POINT ( 'NONE',  ( -0.1871068506425229983, 1450.906526472119822, 181.2442446829110168 ) ) ;
#12489 = CARTESIAN_POINT ( 'NONE',  ( -15.12918126009999931, 1409.441383038730010, 192.4788841068979934 ) ) ;
#12490 = DIRECTION ( 'NONE',  ( 0.000000000000000000, 0.000000000000000000, -1.000000000000000000 ) ) ;
#12491 = ADVANCED_FACE ( 'NONE', ( #60241 ), #24834, .T. ) ;
#12493 = DIRECTION ( 'NONE',  ( 1.755985294532469921E-16, -1.000000000000000000, 1.338183447452831989E-16 ) ) ;
#12492 = CARTESIAN_POINT ( 'NONE',  ( -24.36542518180000272, 1440.980548595849996, 211.6891219858079864 ) ) ;
#12494 = CARTESIAN_POINT ( 'NONE',  ( -6.625178543776530482, 1435.234561983659887, 216.2082763422070286 ) ) ;
#12495 = CARTESIAN_POINT ( 'NONE',  ( -5.822794808474560213, 1511.432897564909808, 201.1850910160889896 ) ) ;
#12496 = CARTESIAN_POINT ( 'NONE',  ( 26.93223535810000158, 1412.607180478629971, 266.6753325838979549 ) ) ;
#12497 = EDGE_CURVE ( 'NONE', #3072, #35478, #25640, .T. ) ;
#12498 = DIRECTION ( 'NONE',  ( -1.000000000000000000, 6.123233995736769734E-17, 0.000000000000000000 ) ) ;
#12499 = CARTESIAN_POINT ( 'NONE',  ( -13.41957906060000028, 1453.146242305830128, 193.5352814221980111 ) ) ;
#12501 = CARTESIAN_POINT ( 'NONE',  ( -23.76744983355909824, 1425.881514248650092, 210.9077260303419905 ) ) ;
#12500 = CARTESIAN_POINT ( 'NONE',  ( 15.73570983720359884, 1409.462563483369877, 192.9527024472970140 ) ) ;
#12502 = AXIS2_PLACEMENT_3D ( 'NONE', #69862, #18853, #11038 ) ;
#12503 = B_SPLINE_SURFACE_WITH_KNOTS ( 'NONE', 5, 5, ( 
 ( #63286, #3922, #70581, #55964, #15024, #99586 ),
 ( #73310, #22313, #39702, #38586, #73868, #109127 ),
 ( #21763, #90087, #74430, #107446, #66032, #47559 ),
 ( #32408, #81681, #14483, #31293, #4987, #57078 ),
 ( #30180, #56516, #90643, #22869, #48676, #72765 ),
 ( #49222, #100155, #4458, #64372, #39131, #12838 ) ),
 .UNSPECIFIED., .F., .F., .F.,
 ( 6, 6 ),
 ( 6, 6 ),
 ( 4.019724148039999889, 13.77031185580000106 ),
 ( 0.000000000000000000, 0.5000000000000000000 ),
 .UNSPECIFIED. ) ;
#12504 = CARTESIAN_POINT ( 'NONE',  ( 4.036119644515000715, 1516.647924054489977, 216.4458205765370167 ) ) ;
#12505 = EDGE_CURVE ( 'NONE', #11318, #57273, #71030, .T. ) ;
#12506 = CARTESIAN_POINT ( 'NONE',  ( 4.329448781177520189, 1515.064792686469900, 207.2788827064790098 ) ) ;
#12507 = CARTESIAN_POINT ( 'NONE',  ( 5.382074236615409291, 1511.451532973539770, 217.6102468295670178 ) ) ;
#12508 = CARTESIAN_POINT ( 'NONE',  ( 18.26221324211669739, 1446.581092866262679, 215.9872273256496840 ) ) ;
#12509 = CARTESIAN_POINT ( 'NONE',  ( 0.01327253640020150012, 1516.940252185109784, 211.9957649727570015 ) ) ;
#12510 = CARTESIAN_POINT ( 'NONE',  ( 2.127049456099050051, 1416.948096802419968, 220.8082361830769855 ) ) ;
#12511 = CARTESIAN_POINT ( 'NONE',  ( -8.970355387749442855, 1421.589330327102971, 137.0999999980979851 ) ) ;
#12513 = ORIENTED_EDGE ( 'NONE', *, *, #88460, .T. ) ;
#12512 = CARTESIAN_POINT ( 'NONE',  ( -106.4826975579999981, 1389.246194448199958, 308.7719952443590046 ) ) ;
#12514 = CARTESIAN_POINT ( 'NONE',  ( -17.05907944273172561, 1524.678541297861102, 237.1959721738423070 ) ) ;
#12515 = CIRCLE ( 'NONE', #51916, 0.5000000000000004441 ) ;
#12516 = CARTESIAN_POINT ( 'NONE',  ( 9.545816653570000199, 1464.920850548930048, 240.4008508649979774 ) ) ;
#12517 = CARTESIAN_POINT ( 'NONE',  ( 29.33952678943222736, 1526.382868172864164, 217.1408869592839324 ) ) ;
#12518 = CARTESIAN_POINT ( 'NONE',  ( -14.48634919999999937, 1416.023439645540066, 203.8591738074189834 ) ) ;
#12519 = DIRECTION ( 'NONE',  ( -0.000000000000000000, -1.000000000000000000, -0.000000000000000000 ) ) ;
#12520 = B_SPLINE_CURVE_WITH_KNOTS ( 'NONE', 3,
 ( #21328, #56626, #64494, #90199, #30853, #65028, #49329, #81253, #107566, #100273, #14601, #57194, #14041, #15139, #4568, #99146, #38702, #66150, #6205, #56072, #107014, #6750, #30302, #22424, #31404, #23553, #40356, #13483, #98610, #83455, #65585, #57745, #73979, #75088, #82913, #21873, #74537, #55534, #82373, #109238, #47673, #90762, #98056, #91319, #89659, #32522, #48232, #5672, #99698, #81802, #5102, #22989, #39257, #73432, #48791, #52090 ),
 .UNSPECIFIED., .F., .F.,
 ( 4, 2, 2, 2, 2, 2, 1, 1, 1, 1, 1, 1, 1, 1, 2, 2, 2, 2, 2, 2, 2, 2, 2, 1, 1, 2, 2, 1, 1, 2, 2, 2, 2, 4 ),
 ( 0.000000000000000000, 0.1249999999950490714, 0.2499999999900982539, 0.3749999999851474364, 0.4374999999826721386, 0.4687499999814371265, 0.4843749999808195095, 0.4921874999805105344, 0.4960937499803561579, 0.4980468749802758888, 0.4990234374802387518, 0.4995117187302201556, 0.4997558593552078876, 0.4998779296677017259, 0.4999389648239485617, 0.4999999999801953421, 0.5312499999787845262, 0.5624999999773735437, 0.5937499999759626723, 0.6249999999745516899, 0.6562499999731408185, 0.6874999999717298360, 0.6953124999714096477, 0.6992187499712494425, 0.6997070312212948506, 0.6999511718463149457, 0.7001953124713350407, 0.7011718749714233034, 0.7031249999716070453, 0.7187499999730988520, 0.7499999999760904590, 0.8124999999820647911, 0.8749999999880391233, 1.000000000000000000 ),
 .UNSPECIFIED. ) ;
#12521 = CARTESIAN_POINT ( 'NONE',  ( -3.968827103576990201, 1522.051704408389924, 229.5396913781519856 ) ) ;
#12523 = DIRECTION ( 'NONE',  ( 0.8090169943749551118, -0.000000000000000000, 0.5877852522924624790 ) ) ;
#12522 = CARTESIAN_POINT ( 'NONE',  ( -20.09300522639999897, 1457.445247091630108, 225.1158171901979870 ) ) ;
#12524 = CARTESIAN_POINT ( 'NONE',  ( -1.639329852409999955, 1484.768299803630043, 182.6367947853979956 ) ) ;
#12525 = CARTESIAN_POINT ( 'NONE',  ( -105.2403994794200059, 1380.288835873570179, 307.4042895074139778 ) ) ;
#12526 = EDGE_LOOP ( 'NONE', ( #41663, #19881, #26058, #74795 ) ) ;
#12527 = CARTESIAN_POINT ( 'NONE',  ( 3.447264348965000558, 1516.858765657450249, 205.6607986404769974 ) ) ;
#12528 = CARTESIAN_POINT ( 'NONE',  ( 0.7655880511680001055, 1406.782360832429958, 269.6498828098979743 ) ) ;
#12529 = CARTESIAN_POINT ( 'NONE',  ( -1.842962231260000028, 1515.372048949689997, 213.3835825136090136 ) ) ;
#12530 = EDGE_CURVE ( 'NONE', #17686, #41312, #4194, .T. ) ;
#12531 = CARTESIAN_POINT ( 'NONE',  ( 18.87687341284280151, 1468.931718062809978, 269.6477239524390370 ) ) ;
#12532 = EDGE_CURVE ( 'NONE', #27116, #21797, #30929, .T. ) ;
#12533 = CARTESIAN_POINT ( 'NONE',  ( 2.064218541529331929, 1464.188986783531618, 199.5203533287811126 ) ) ;
#12534 = CARTESIAN_POINT ( 'NONE',  ( 0.000000000000000000, 1413.913060387330006, 209.1218459616979999 ) ) ;
#12535 = CARTESIAN_POINT ( 'NONE',  ( -6.347844883064759358, 1440.117647072198906, 203.0612122617101818 ) ) ;
#12536 = AXIS2_PLACEMENT_3D ( 'NONE', #57396, #109980, #14802 ) ;
#12537 = CARTESIAN_POINT ( 'NONE',  ( -3.957900269260000048, 1458.284989000489986, 219.0746905126889885 ) ) ;
#12538 = CARTESIAN_POINT ( 'NONE',  ( -4.989533930479999491, 1429.437332217889889, 202.3857892670889953 ) ) ;
#12539 = CARTESIAN_POINT ( 'NONE',  ( 2.493007212856739763, 1449.246563104740062, 154.5202210656170223 ) ) ;
#12540 = CARTESIAN_POINT ( 'NONE',  ( -13.73229811677040146, 1415.184612916749984, 220.6533628109979759 ) ) ;
#12541 = DIRECTION ( 'NONE',  ( 0.000000000000000000, 1.000000000000000000, 0.000000000000000000 ) ) ;
#12542 = ORIENTED_EDGE ( 'NONE', *, *, #1619, .T. ) ;
#12543 = CARTESIAN_POINT ( 'NONE',  ( -12.15345565450000009, 1413.272114130229966, 265.6112251771979800 ) ) ;
#12544 = ADVANCED_FACE ( 'NONE', ( #65211 ), #101723, .F. ) ;
#12545 = CARTESIAN_POINT ( 'NONE',  ( 7.001391005937890100, 1467.620735506979827, 200.2764061176360144 ) ) ;
#12546 = CARTESIAN_POINT ( 'NONE',  ( -0.2163474815539999929, 1476.109084357029815, 267.8540247851980212 ) ) ;
#12547 = CARTESIAN_POINT ( 'NONE',  ( 17.07372443010000040, 1494.814959774189902, 195.5520917663990019 ) ) ;
#12548 = CARTESIAN_POINT ( 'NONE',  ( -10.81507089441019964, 1424.921187596680056, 144.1620444830689962 ) ) ;
#12549 = CARTESIAN_POINT ( 'NONE',  ( -3.344594669770147188, 1448.284147565596413, 184.7768058458345308 ) ) ;
#12550 = CARTESIAN_POINT ( 'NONE',  ( -36.08493826582400033, 1384.804586415280028, 235.7710440410830017 ) ) ;
#12551 = AXIS2_PLACEMENT_3D ( 'NONE', #95636, #53667, #53102 ) ;
#12552 = CARTESIAN_POINT ( 'NONE',  ( -105.9089176949999995, 1378.913060387289988, 303.0252558878589753 ) ) ;
#12553 = CARTESIAN_POINT ( 'NONE',  ( -9.542479485949998619, 1481.357605531989975, 204.5426345580789871 ) ) ;
#12554 = CARTESIAN_POINT ( 'NONE',  ( 8.071166603322222244, 1511.586661999316902, 205.5159583346354282 ) ) ;
#12555 = CARTESIAN_POINT ( 'NONE',  ( -10.58554379023919978, 1396.282715721989916, 212.3608612925139880 ) ) ;
#12556 = B_SPLINE_CURVE_WITH_KNOTS ( 'NONE', 3,
 ( #75044, #92362, #76678, #101295, #101856, #83417, #34122, #102420, #85064, #66104, #67195, #40868 ),
 .UNSPECIFIED., .F., .F.,
 ( 4, 2, 2, 2, 2, 4 ),
 ( 0.000000000000000000, 0.0007194225121803802993, 0.001079133768270255488, 0.001438845024360130894, 0.002158267536539314451, 0.002877690048718498008 ),
 .UNSPECIFIED. ) ;
#12557 = CARTESIAN_POINT ( 'NONE',  ( -14.61089922049999856, 1422.243781465129814, 228.7538395214980085 ) ) ;
#12558 = EDGE_CURVE ( 'NONE', #2857, #32152, #104036, .T. ) ;
#12559 = CARTESIAN_POINT ( 'NONE',  ( 19.57204117397504817, 1455.492560539847773, 225.8522660090905561 ) ) ;
#12560 = EDGE_LOOP ( 'NONE', ( #98522, #37950, #13338, #27893 ) ) ;
#12561 = CARTESIAN_POINT ( 'NONE',  ( -11.32803462625343194, 1502.699820297845008, 207.1273456882843789 ) ) ;
#12562 = CARTESIAN_POINT ( 'NONE',  ( 1.443308927659999963, 1409.130619246129982, 231.7887507488979963 ) ) ;
#12563 = CARTESIAN_POINT ( 'NONE',  ( -11.76598820887720009, 1428.979787295000051, 145.3127948738930115 ) ) ;
#12565 = CARTESIAN_POINT ( 'NONE',  ( -11.25155674426499885, 1512.842772631639946, 192.9205417576670243 ) ) ;
#12564 = CARTESIAN_POINT ( 'NONE',  ( 11.26090570969999938, 1425.591115143630077, 132.2030400731979967 ) ) ;
#12566 = DIRECTION ( 'NONE',  ( -1.000000000000000000, -4.614530979569559207E-09, -3.922279168137524319E-10 ) ) ;
#12567 = EDGE_CURVE ( 'NONE', #10827, #104308, #94988, .T. ) ;
#12568 = CARTESIAN_POINT ( 'NONE',  ( -12.37499353609999986, 1445.063428794549964, 205.2217743980949933 ) ) ;
#12569 = CIRCLE ( 'NONE', #76932, 4079.102027089948479 ) ;
#12570 = CARTESIAN_POINT ( 'NONE',  ( 6.941727252324999320, 1516.882217593000178, 201.7906628411569727 ) ) ;
#12571 = CARTESIAN_POINT ( 'NONE',  ( 8.075468704329999525, 1426.465554857850066, 211.6438910379590084 ) ) ;
#12572 = CARTESIAN_POINT ( 'NONE',  ( -7.298550013359999866, 1430.724169039930075, 149.5003602673979799 ) ) ;
#12573 = CARTESIAN_POINT ( 'NONE',  ( 7.288579114480000065, 1509.158655100730130, 180.9739811970979702 ) ) ;
#12574 = CARTESIAN_POINT ( 'NONE',  ( 6.252266454184999489, 1511.741868877540128, 217.9101624594169948 ) ) ;
#12575 = CARTESIAN_POINT ( 'NONE',  ( -86.23580615497749591, 1378.226136009930087, 302.2523813644399979 ) ) ;
#12576 = CARTESIAN_POINT ( 'NONE',  ( 8.100491796851672532, 1366.331969060035135, 207.6218459616988241 ) ) ;
#12578 = EDGE_LOOP ( 'NONE', ( #1097, #84747, #108743, #71678 ) ) ;
#12577 = CARTESIAN_POINT ( 'NONE',  ( 8.978224261840001219, 1452.688325861789963, 212.1105519951989891 ) ) ;
#12579 = ORIENTED_EDGE ( 'NONE', *, *, #76649, .T. ) ;
#12580 = CARTESIAN_POINT ( 'NONE',  ( -6.016809048099999835, 1396.654460031930057, 198.2004533729979983 ) ) ;
#12581 = CARTESIAN_POINT ( 'NONE',  ( 1.165162292670530064, 1482.877340327559978, 235.9985051030799923 ) ) ;
#12582 = EDGE_CURVE ( 'NONE', #85936, #8701, #30738, .T. ) ;
#12583 = CARTESIAN_POINT ( 'NONE',  ( 13.22806383159999832, 1431.113060387329824, 223.7296695649979767 ) ) ;
#12584 = CARTESIAN_POINT ( 'NONE',  ( 0.1955981723673640149, 1414.913060387329779, 225.1861338915940109 ) ) ;
#12586 = CARTESIAN_POINT ( 'NONE',  ( -1.363590407445679942, 1415.730364842510198, 185.3753152215819853 ) ) ;
#12585 = CARTESIAN_POINT ( 'NONE',  ( -7.683071123930000468, 1383.591828314379882, 218.9382038826490202 ) ) ;
#12587 = AXIS2_PLACEMENT_3D ( 'NONE', #53165, #88407, #97350 ) ;
#12588 = CARTESIAN_POINT ( 'NONE',  ( 0.5133699756429999095, 1410.311097179130002, 185.0719926106980040 ) ) ;
#12589 = ADVANCED_FACE ( 'NONE', ( #51157 ), #39989, .F. ) ;
#12590 = CARTESIAN_POINT ( 'NONE',  ( -2.031867801918239902, 1464.998398352370032, 198.3053289726209982 ) ) ;
#12591 = DIRECTION ( 'NONE',  ( -1.407418274235000032E-17, -1.000000000000000000, 2.576261870300899651E-17 ) ) ;
#12592 = FILL_AREA_STYLE_COLOUR ( '', #71822 ) ;
#12593 = CARTESIAN_POINT ( 'NONE',  ( 41.18767709054869641, 1440.809226716479998, 135.8247641852480001 ) ) ;
#12594 = CARTESIAN_POINT ( 'NONE',  ( 7.862841600128040120, 1396.187636867450010, 216.8852634763560161 ) ) ;
#12595 = CARTESIAN_POINT ( 'NONE',  ( -1.836970198721029983E-15, 1374.913060387289988, 209.1218459572589836 ) ) ;
#12596 = CARTESIAN_POINT ( 'NONE',  ( 11.70410276859999854, 1427.698297935130086, 149.0273710990979907 ) ) ;
#12597 = CARTESIAN_POINT ( 'NONE',  ( -18.89905695062199698, 1416.828039266840278, 207.5749027128360069 ) ) ;
#12598 = ORIENTED_EDGE ( 'NONE', *, *, #92867, .F. ) ;
#12599 = CARTESIAN_POINT ( 'NONE',  ( 4.098422289620000214, 1424.674502485429912, 185.1777122999980065 ) ) ;
#12600 = CARTESIAN_POINT ( 'NONE',  ( 21.14962954806519591, 1525.231909165050638, 233.8093717500290154 ) ) ;
#12601 = ORIENTED_EDGE ( 'NONE', *, *, #34273, .F. ) ;
#12602 = ORIENTED_EDGE ( 'NONE', *, *, #68472, .F. ) ;
#12603 = EDGE_CURVE ( 'NONE', #74077, #8151, #5723, .T. ) ;
#12604 = CARTESIAN_POINT ( 'NONE',  ( -17.36423504460000089, 1468.191340553330065, 228.4970079188980208 ) ) ;
#12605 = CARTESIAN_POINT ( 'NONE',  ( -12.83453119069999993, 1463.115711949329807, 230.6691871800979925 ) ) ;
#12606 = CARTESIAN_POINT ( 'NONE',  ( -2.482067898354999969, 1517.099836525840146, 214.9099431973869798 ) ) ;
#12607 = CARTESIAN_POINT ( 'NONE',  ( -13.18481025451849931, 1379.800827107049827, 208.6184356723600217 ) ) ;
#12608 = EDGE_CURVE ( 'NONE', #103878, #45131, #60122, .T. ) ;
#12609 = ORIENTED_EDGE ( 'NONE', *, *, #76897, .T. ) ;
#12610 = CARTESIAN_POINT ( 'NONE',  ( -12.51045652733512625, 1415.677402202029953, 206.7437175916260230 ) ) ;
#12611 = CARTESIAN_POINT ( 'NONE',  ( -28.76039927569999932, 1380.228231664269970, 215.0392276715589901 ) ) ;
#12612 = CARTESIAN_POINT ( 'NONE',  ( 2.576993404970000512, 1414.913060387329779, 225.2932022862979977 ) ) ;
#12613 = CARTESIAN_POINT ( 'NONE',  ( -0.7564342523539989704, 1516.783665406140017, 204.5091745923169810 ) ) ;
#12614 = VECTOR ( 'NONE', #81199, 1000.000000000000114 ) ;
#12615 = CARTESIAN_POINT ( 'NONE',  ( -11.88881437795680007, 1489.631889030339835, 211.9231216160999907 ) ) ;
#12616 = B_SPLINE_SURFACE_WITH_KNOTS ( 'NONE', 5, 5, ( 
 ( #52956, #87090, #78697, #70330, #27734, #96041 ),
 ( #19312, #36691, #10945, #70885, #93001, #58322 ),
 ( #48836, #16277, #57787, #58871, #97696, #57239 ),
 ( #82958, #6252, #6793, #71987, #20968, #50479 ),
 ( #40954, #55171, #74578, #33099, #84603, #75131 ),
 ( #15182, #29378, #63579, #46771, #24132, #109281 ),
 ( #7894, #84056, #89297, #91370, #67289, #80902 ),
 ( #106101, #12593, #4198, #72510, #49370, #7355 ),
 ( #40401, #23598, #66739, #41517, #32563, #101380 ),
 ( #108714, #32005, #24673, #91907, #38330, #99747 ),
 ( #83498, #49921, #66193, #100842, #100313, #92445 ),
 ( #15720, #106638, #29929, #64120, #75676, #109820 ) ),
 .UNSPECIFIED., .F., .F., .F.,
 ( 6, 3, 3, 6 ),
 ( 6, 6 ),
 ( -8.488962093846350222E-06, 6.410372910170000438, 10.64487668199999959, 14.62797318289999993 ),
 ( -8.488962093846350222E-06, 1.479090568609999989 ),
 .UNSPECIFIED. ) ;
#12617 = CARTESIAN_POINT ( 'NONE',  ( -42.06231988464593741, 1439.942263177195628, 269.6487542301402414 ) ) ;
#12618 = CARTESIAN_POINT ( 'NONE',  ( -3.191350148519999763, 1410.401812535530098, 232.4693402741980037 ) ) ;
#12620 = ORIENTED_EDGE ( 'NONE', *, *, #67215, .F. ) ;
#12619 = FACE_OUTER_BOUND ( 'NONE', #96138, .T. ) ;
#12621 = EDGE_CURVE ( 'NONE', #68839, #53112, #109661, .T. ) ;
#12622 = CYLINDRICAL_SURFACE ( 'NONE', #81519, 3.750000000000000000 ) ;
#12623 = CARTESIAN_POINT ( 'NONE',  ( 28.27621775960000150, 1508.136061369130175, 209.2246319227680260 ) ) ;
#12624 = CARTESIAN_POINT ( 'NONE',  ( -5.960032396909999974, 1384.206784872530079, 218.4667819198089944 ) ) ;
#12625 = PLANE ( 'NONE',  #7005 ) ;
#12626 = CARTESIAN_POINT ( 'NONE',  ( 44.13009079475659746, 1436.416161715979797, 270.2165924888440145 ) ) ;
#12627 = ADVANCED_FACE ( 'NONE', ( #94240 ), #84757, .F. ) ;
#12629 = CARTESIAN_POINT ( 'NONE',  ( -2.477986770365000257, 1516.922519270759949, 212.3907053662870226 ) ) ;
#12628 = VECTOR ( 'NONE', #24763, 999.9999999999998863 ) ;
#12630 = CARTESIAN_POINT ( 'NONE',  ( -66.55629426049999608, 1379.749035308849898, 275.7365325667589673 ) ) ;
#12631 = CARTESIAN_POINT ( 'NONE',  ( 22.60265952820000024, 1409.702346025430188, 208.8284293190110077 ) ) ;
#12632 = CARTESIAN_POINT ( 'NONE',  ( 0.004059509192577217401, 1508.830451557245169, 238.4590521952922018 ) ) ;
#12633 = CARTESIAN_POINT ( 'NONE',  ( 7.253078750751489778, 1425.167378741770108, 192.6391490917010287 ) ) ;
#12634 = CARTESIAN_POINT ( 'NONE',  ( -7.718230792536809659, 1516.885624574970052, 209.2907034861239879 ) ) ;
#12635 = CARTESIAN_POINT ( 'NONE',  ( -6.550870182235000172, 1516.727502608469877, 209.8762341530540141 ) ) ;
#12636 = CARTESIAN_POINT ( 'NONE',  ( 27.01367402797299277, 1509.856398671217903, 221.2719421893247898 ) ) ;
#12637 = CARTESIAN_POINT ( 'NONE',  ( -11.61299349109999923, 1417.902132930430071, 229.0839532085980181 ) ) ;
#12638 = CARTESIAN_POINT ( 'NONE',  ( -5.513435911474870110, 1508.551704408389924, 202.1089243664339961 ) ) ;
#12639 = VERTEX_POINT ( 'NONE', #78006 ) ;
#12640 = CARTESIAN_POINT ( 'NONE',  ( -22.89778237906369895, 1385.264640953090066, 222.3446852156519924 ) ) ;
#12641 = DIRECTION ( 'NONE',  ( -1.000000000000000000, 0.000000000000000000, 0.000000000000000000 ) ) ;
#12642 = TOROIDAL_SURFACE ( 'NONE', #84164, 7.500000000000000000, 0.2999999999999999889 ) ;
#12643 = CARTESIAN_POINT ( 'NONE',  ( -20.97376010811069946, 1508.893464270799996, 228.1411980946349729 ) ) ;
#12644 = CARTESIAN_POINT ( 'NONE',  ( -31.12456774391156600, 1525.960063244517187, 217.0912716842400698 ) ) ;
#12645 = CARTESIAN_POINT ( 'NONE',  ( 11.66936717579999971, 1421.865521096479824, 204.5896370874590104 ) ) ;
#12646 = CARTESIAN_POINT ( 'NONE',  ( 0.6489903397072023239, 1498.624614946328165, 197.8160440545376275 ) ) ;
#12647 = CIRCLE ( 'NONE', #34064, 0.9999999999999100719 ) ;
#12649 = CARTESIAN_POINT ( 'NONE',  ( -8.537822636805000087, 1517.051704408389924, 205.6971256312070011 ) ) ;
#12648 = CARTESIAN_POINT ( 'NONE',  ( 0.01073129396420149928, 1516.939491476980038, 216.4539099096770087 ) ) ;
#12650 = CARTESIAN_POINT ( 'NONE',  ( 19.06981280680000168, 1509.578992924630029, 186.6663347137979940 ) ) ;
#12651 = DIRECTION ( 'NONE',  ( 0.000000000000000000, 1.000000000000000000, -2.081668171172166620E-14 ) ) ;
#12652 = ORIENTED_EDGE ( 'NONE', *, *, #67363, .F. ) ;
#12653 = CARTESIAN_POINT ( 'NONE',  ( -7.330554171554999776, 1516.857992118400034, 201.7925428541169879 ) ) ;
#12654 = CARTESIAN_POINT ( 'NONE',  ( 10.49535538868399875, 1481.102825724099830, 207.9455356762770180 ) ) ;
#12655 = ORIENTED_EDGE ( 'NONE', *, *, #46120, .F. ) ;
#12656 = CARTESIAN_POINT ( 'NONE',  ( 11.60004869885204748, 1426.730434226297575, 134.4361623791434397 ) ) ;
#12657 = CARTESIAN_POINT ( 'NONE',  ( 9.930928656378739561, 1435.775907024141588, 152.5385279279675785 ) ) ;
#12658 = CARTESIAN_POINT ( 'NONE',  ( 8.842581916386802021, 1424.898463456729814, 195.7260410483776809 ) ) ;
#12659 = CARTESIAN_POINT ( 'NONE',  ( 2.634457758659999538, 1441.548974666690128, 218.6895019696289921 ) ) ;
#12660 = CARTESIAN_POINT ( 'NONE',  ( -26.36538957056309940, 1508.144877758350049, 201.5400870493360230 ) ) ;
#12661 = AXIS2_PLACEMENT_3D ( 'NONE', #10741, #36480, #87447 ) ;
#12662 = CARTESIAN_POINT ( 'NONE',  ( -2.704954423899999849, 1447.065239520570003, 170.5387359060979975 ) ) ;
#12663 = CARTESIAN_POINT ( 'NONE',  ( -19.15459394270000004, 1425.147755204630130, 223.9734305455980063 ) ) ;
#12664 = CARTESIAN_POINT ( 'NONE',  ( 17.30126322281369866, 1523.382868172864164, 180.8506073313484990 ) ) ;
#12665 = DIRECTION ( 'NONE',  ( -0.9455185755993177343, 0.000000000000000000, 0.3255681544571540909 ) ) ;
#12666 = CARTESIAN_POINT ( 'NONE',  ( 17.95536526520000109, 1461.940388925729849, 190.0337052255979984 ) ) ;
#12668 = DIRECTION ( 'NONE',  ( -0.1403878024439498828, 0.9900965937346509760, 0.000000000000000000 ) ) ;
#12667 = CARTESIAN_POINT ( 'NONE',  ( 5.547280765580000050, 1487.873461314389942, 198.4571336758990014 ) ) ;
#12669 = FACE_OUTER_BOUND ( 'NONE', #14083, .T. ) ;
#12670 = ORIENTED_EDGE ( 'NONE', *, *, #21286, .T. ) ;
#12671 = CARTESIAN_POINT ( 'NONE',  ( -105.5847408669999936, 1378.244047627129930, 303.6830150497589784 ) ) ;
#12672 = CARTESIAN_POINT ( 'NONE',  ( -13.32757262590000025, 1508.445659285190004, 217.0210970315689849 ) ) ;
#12673 = DIRECTION ( 'NONE',  ( 1.755985294532464991E-16, -1.000000000000000000, 1.338183447452830017E-16 ) ) ;
#12674 = CARTESIAN_POINT ( 'NONE',  ( 11.15470940107600128, 1470.295755632079818, 206.9817199298160233 ) ) ;
#12675 = CARTESIAN_POINT ( 'NONE',  ( -2.576618889659999745, 1485.526343952190246, 197.4968898064989844 ) ) ;
#12676 = CARTESIAN_POINT ( 'NONE',  ( 2.385019621457262762, 1526.073429442291626, 240.5311921326816673 ) ) ;
#12677 = CARTESIAN_POINT ( 'NONE',  ( -2.410642264446942296, 1525.163527997520532, 242.1266861310988645 ) ) ;
#12678 = CARTESIAN_POINT ( 'NONE',  ( -13.24668964730320297, 1444.655481269342545, 186.6492647222285370 ) ) ;
#12679 = CARTESIAN_POINT ( 'NONE',  ( -16.81223226430000039, 1414.913060387329779, 207.5743821216680089 ) ) ;
#12680 = CARTESIAN_POINT ( 'NONE',  ( 3.427496190376880136, 1494.480924628220009, 219.9046048467500043 ) ) ;
#12681 = CARTESIAN_POINT ( 'NONE',  ( 0.5708535463504419427, 1460.784162354619866, 230.4191111958880072 ) ) ;
#12682 = CARTESIAN_POINT ( 'NONE',  ( -107.5775718089879973, 1383.759024782929828, 311.0686465984289839 ) ) ;
#12683 = CARTESIAN_POINT ( 'NONE',  ( -109.9562721537739947, 1384.319945152750051, 311.4255092121239841 ) ) ;
#12684 = CARTESIAN_POINT ( 'NONE',  ( 0.1086926021523879904, 1516.965532036659852, 201.4015232171759919 ) ) ;
#12686 = ORIENTED_EDGE ( 'NONE', *, *, #46138, .F. ) ;
#12685 = CARTESIAN_POINT ( 'NONE',  ( 21.90604547420000259, 1509.617455791430075, 189.8984835829979829 ) ) ;
#12687 = CARTESIAN_POINT ( 'NONE',  ( 33.93019615848946557, 1522.382868172863937, 197.6607374645996060 ) ) ;
#12688 = CARTESIAN_POINT ( 'NONE',  ( 13.23930717780280020, 1512.526687531779999, 224.3998820107140091 ) ) ;
#12689 = ORIENTED_EDGE ( 'NONE', *, *, #101059, .F. ) ;
#12690 = ORIENTED_EDGE ( 'NONE', *, *, #9225, .T. ) ;
#12691 = CARTESIAN_POINT ( 'NONE',  ( -20.11385680769999951, 1487.601373209189887, 204.1067431612489997 ) ) ;
#12692 = CARTESIAN_POINT ( 'NONE',  ( -109.8952007060000113, 1384.926598849860056, 297.0284133136589730 ) ) ;
#12693 = CARTESIAN_POINT ( 'NONE',  ( 13.38997184703062260, 1443.386902099714234, 169.3691664011028593 ) ) ;
#12695 = CARTESIAN_POINT ( 'NONE',  ( -33.60183516099999679, 1440.913060390449800, 248.0844435644980024 ) ) ;
#12694 = CARTESIAN_POINT ( 'NONE',  ( 16.15334260449234449, 1412.751362655629691, 269.3697234748176470 ) ) ;
#12696 = CARTESIAN_POINT ( 'NONE',  ( -20.18772548640000153, 1494.510936209429929, 190.7767133961980051 ) ) ;
#12697 = CARTESIAN_POINT ( 'NONE',  ( -11.93562850120000007, 1433.536276356740018, 150.1881428924980071 ) ) ;
#12698 = CARTESIAN_POINT ( 'NONE',  ( 26.15185231619999939, 1509.826303196630079, 197.3935024311979873 ) ) ;
#12699 = CARTESIAN_POINT ( 'NONE',  ( 11.60004869885203682, 1426.786827912535728, 134.3786173235958472 ) ) ;
#12700 = CARTESIAN_POINT ( 'NONE',  ( 4.994880155184180381, 1467.527977092940091, 217.7500441216180036 ) ) ;
#12701 = CARTESIAN_POINT ( 'NONE',  ( -2.038847259689227531, 1522.382868172863937, 244.9330574173806667 ) ) ;
#12702 = CARTESIAN_POINT ( 'NONE',  ( -0.01406703361950679965, 1515.158574431529814, 213.4488389814559923 ) ) ;
#12703 = CARTESIAN_POINT ( 'NONE',  ( 5.268693351980000550, 1440.707873525929926, 154.8524945618979700 ) ) ;
#12704 = CARTESIAN_POINT ( 'NONE',  ( -10.67455619629699903, 1480.094165611569906, 214.0407775190860207 ) ) ;
#12705 = VECTOR ( 'NONE', #49096, 999.9999999999998863 ) ;
#12706 = CARTESIAN_POINT ( 'NONE',  ( -4.466366219213330879, 1362.092831090860955, 210.6218459617142003 ) ) ;
#12707 = CARTESIAN_POINT ( 'NONE',  ( 33.28034951413762599, 1522.644714754858114, 200.8029765415147097 ) ) ;
#12709 = ORIENTED_EDGE ( 'NONE', *, *, #12603, .T. ) ;
#12708 = CARTESIAN_POINT ( 'NONE',  ( 1.396945595908719806, 1473.097535771269804, 219.2356281669150064 ) ) ;
#12710 = ORIENTED_EDGE ( 'NONE', *, *, #76076, .F. ) ;
#12711 = CARTESIAN_POINT ( 'NONE',  ( -11.86563452110919847, 1432.303449558290140, 149.9823120433860026 ) ) ;
#12712 = CARTESIAN_POINT ( 'NONE',  ( -17.98650874570000013, 1489.991360812790163, 195.2845414362990084 ) ) ;
#12713 = CARTESIAN_POINT ( 'NONE',  ( -20.06107000609999957, 1468.329342173230089, 269.8982276395979625 ) ) ;
#12714 = CARTESIAN_POINT ( 'NONE',  ( 7.782527000790000038, 1421.790398246840141, 195.8641137985989928 ) ) ;
#12716 = CIRCLE ( 'NONE', #14449, 1.999999999999998890 ) ;
#12715 = CARTESIAN_POINT ( 'NONE',  ( -125.2268008667000743, 1376.302340817389677, 301.2019679020577883 ) ) ;
#12717 = DIRECTION ( 'NONE',  ( 0.4090087482554383702, -0.000000000000000000, 0.9125304618753937724 ) ) ;
#12718 = ADVANCED_FACE ( 'NONE', ( #61789 ), #50795, .T. ) ;
#12719 = CARTESIAN_POINT ( 'NONE',  ( 4.327305182180260168, 1515.146653429429989, 209.5728053323190068 ) ) ;
#12720 = EDGE_CURVE ( 'NONE', #25318, #19628, #54948, .T. ) ;
#12721 = CARTESIAN_POINT ( 'NONE',  ( -0.4151546846821903003, 1512.187213306747481, 243.9330574173806951 ) ) ;
#12722 = CARTESIAN_POINT ( 'NONE',  ( -10.26338073471560008, 1517.551704408389924, 184.6900425920350131 ) ) ;
#12723 = TOROIDAL_SURFACE ( 'NONE', #27037, 20.98341875039999849, 2.000000000000000000 ) ;
#12724 = CARTESIAN_POINT ( 'NONE',  ( -15.68560381520000035, 1410.853898380629971, 226.7268320020979786 ) ) ;
#12725 = CARTESIAN_POINT ( 'NONE',  ( 11.03759844033949911, 1362.198095653763176, 209.6218459617033432 ) ) ;
#12726 = CARTESIAN_POINT ( 'NONE',  ( -45.52611345104049434, 1436.768312834970175, 268.7663215527609850 ) ) ;
#12727 = EDGE_LOOP ( 'NONE', ( #34556, #10701, #5146, #46401 ) ) ;
#12728 = CARTESIAN_POINT ( 'NONE',  ( -3.542930565813509958, 1500.789291168119917, 181.2469841982909884 ) ) ;
#12729 = ORIENTED_EDGE ( 'NONE', *, *, #97538, .T. ) ;
#12730 = ORIENTED_EDGE ( 'NONE', *, *, #98607, .F. ) ;
#12731 = CARTESIAN_POINT ( 'NONE',  ( 5.788436334164999586, 1517.116049120239950, 211.4102033778369787 ) ) ;
#12732 = AXIS2_PLACEMENT_3D ( 'NONE', #98584, #21850, #82345 ) ;
#12733 = CARTESIAN_POINT ( 'NONE',  ( -9.138800708037619458, 1447.299821738310129, 212.1281046494140128 ) ) ;
#12734 = CARTESIAN_POINT ( 'NONE',  ( 16.37831395161595793, 1409.485003713481547, 224.8086535334813334 ) ) ;
#12735 = CARTESIAN_POINT ( 'NONE',  ( -16.01768569949999943, 1425.422481232729979, 190.6310110230979831 ) ) ;
#12736 = ADVANCED_FACE ( 'NONE', ( #64537 ), #22470, .T. ) ;
#12737 = CARTESIAN_POINT ( 'NONE',  ( -16.20519014447769734, 1470.472166712469971, 228.6977888834950079 ) ) ;
#12738 = EDGE_LOOP ( 'NONE', ( #84591, #90261, #101434, #21258 ) ) ;
#12739 = CARTESIAN_POINT ( 'NONE',  ( -0.7533001734329990429, 1516.714320817460020, 201.7957737879569891 ) ) ;
#12740 = CIRCLE ( 'NONE', #107443, 12.49965726619999984 ) ;
#12741 = CARTESIAN_POINT ( 'NONE',  ( 9.058637367070000224, 1472.814398557089817, 216.2138489941889929 ) ) ;
#12742 = CARTESIAN_POINT ( 'NONE',  ( -17.59599179729789853, 1384.528033373270091, 201.1169542061229834 ) ) ;
#12743 = VERTEX_POINT ( 'NONE', #107611 ) ;
#12744 = VECTOR ( 'NONE', #107545, 1000.000000000000000 ) ;
#12745 = CARTESIAN_POINT ( 'NONE',  ( -16.36542536654240010, 1412.568371408070107, 269.6441855290919989 ) ) ;
#12746 = CARTESIAN_POINT ( 'NONE',  ( -32.74366472130000716, 1435.640891862840135, 135.1028903260980201 ) ) ;
#12747 = DIRECTION ( 'NONE',  ( -0.9455185755993178454, 0.000000000000000000, 0.3255681544571537578 ) ) ;
#12749 = ORIENTED_EDGE ( 'NONE', *, *, #86288, .T. ) ;
#12748 = CARTESIAN_POINT ( 'NONE',  ( -7.895487264294541063, 1365.128408244944467, 209.6218459617148824 ) ) ;
#12750 = ORIENTED_EDGE ( 'NONE', *, *, #11107, .F. ) ;
#12751 = CARTESIAN_POINT ( 'NONE',  ( 42.04271831246587254, 1454.216331209674536, 269.0746633548914133 ) ) ;
#12752 = CARTESIAN_POINT ( 'NONE',  ( -0.1650793151492190025, 1467.512301221159987, 220.2121120126230096 ) ) ;
#12753 = CARTESIAN_POINT ( 'NONE',  ( -2.500000000000000000, 1419.498728202598613, 138.4985336053808282 ) ) ;
#12754 = CARTESIAN_POINT ( 'NONE',  ( -0.03619593704711999982, 1409.492594519410204, 185.3096333675919993 ) ) ;
#12755 = EDGE_CURVE ( 'NONE', #50508, #89888, #37658, .T. ) ;
#12756 = CARTESIAN_POINT ( 'NONE',  ( 1.137296650804999976, 1516.908147884120126, 210.8236964273370120 ) ) ;
#12757 = VECTOR ( 'NONE', #41283, 1000.000000000000000 ) ;
#12758 = CARTESIAN_POINT ( 'NONE',  ( -21.97938480444670262, 1506.433683733529961, 209.5040264213440082 ) ) ;
#12759 = CARTESIAN_POINT ( 'NONE',  ( -20.96644920750000196, 1435.767435547340028, 221.3947938468980112 ) ) ;
#12760 = CARTESIAN_POINT ( 'NONE',  ( 10.49648151684939990, 1474.485926324769935, 269.6275812235440412 ) ) ;
#12761 = CARTESIAN_POINT ( 'NONE',  ( 12.62835224979999893, 1416.067629290630066, 222.6573521500980064 ) ) ;
#12762 = CARTESIAN_POINT ( 'NONE',  ( 8.463742304414999751, 1511.382391139620040, 204.2973509411470161 ) ) ;
#12763 =( BOUNDED_CURVE ( )  B_SPLINE_CURVE ( 3, ( #39585, #82125, #5428, #81566 ),
 .UNSPECIFIED., .F., .F. ) 
 B_SPLINE_CURVE_WITH_KNOTS ( ( 4, 4 ),
 ( 4.245297863855720166, 5.179473289257879642 ),
 .UNSPECIFIED. ) 
 CURVE ( )  GEOMETRIC_REPRESENTATION_ITEM ( )  RATIONAL_B_SPLINE_CURVE ( ( 1.000000000000000000, 0.9285889602860022407, 0.9285889602860022407, 1.000000000000000000 ) ) 
 REPRESENTATION_ITEM ( '' )  );
#12764 = CARTESIAN_POINT ( 'NONE',  ( -5.012938901904998801, 1517.051603658920158, 206.6410320471169939 ) ) ;
#12765 = EDGE_CURVE ( 'NONE', #41410, #60554, #57630, .T. ) ;
#12766 = ORIENTED_EDGE ( 'NONE', *, *, #72866, .F. ) ;
#12767 = CARTESIAN_POINT ( 'NONE',  ( -42.60628464670860183, 1443.705283352449896, 135.6928033759050152 ) ) ;
#12768 = CARTESIAN_POINT ( 'NONE',  ( -22.53754828600002469, 1451.487084850873543, 219.3519410532077529 ) ) ;
#12769 = ORIENTED_EDGE ( 'NONE', *, *, #12755, .F. ) ;
#12771 = B_SPLINE_CURVE_WITH_KNOTS ( 'NONE', 3,
 ( #12220, #79446, #46414, #1648 ),
 .UNSPECIFIED., .F., .F.,
 ( 4, 4 ),
 ( 0.000000000000000000, 0.0002960034161023851105 ),
 .UNSPECIFIED. ) ;
#12770 = CARTESIAN_POINT ( 'NONE',  ( 2.483946272145344913, 1457.674397455789176, 228.7507860573133485 ) ) ;
#12772 = CARTESIAN_POINT ( 'NONE',  ( 24.19930084177359930, 1452.068017472880001, 136.4480432603959912 ) ) ;
#12773 = CARTESIAN_POINT ( 'NONE',  ( 13.72467564589999967, 1416.021639796329964, 196.5129936595979814 ) ) ;
#12774 = CARTESIAN_POINT ( 'NONE',  ( -13.96688741319999849, 1417.698261240689817, 203.4998333049589974 ) ) ;
#12775 = CARTESIAN_POINT ( 'NONE',  ( 20.06637829199999956, 1410.535413374630252, 197.5507824890980260 ) ) ;
#12776 = CARTESIAN_POINT ( 'NONE',  ( 13.26516604059999693, 1444.994950788470987, 176.9857848810979704 ) ) ;
#12777 = CARTESIAN_POINT ( 'NONE',  ( 16.10810117269999964, 1409.475567675330012, 225.1222583912979758 ) ) ;
#12778 = FACE_OUTER_BOUND ( 'NONE', #102231, .T. ) ;
#12779 = DIRECTION ( 'NONE',  ( -1.156023075842281927E-31, 1.000000000000000000, -1.698192320643030073E-16 ) ) ;
#12780 = CARTESIAN_POINT ( 'NONE',  ( 2.500000000000000000, 1439.435444791209875, 162.3942721139659682 ) ) ;
#12781 = CARTESIAN_POINT ( 'NONE',  ( 0.01244693565920149993, 1516.939646076049939, 214.9034317483770167 ) ) ;
#12782 = ORIENTED_EDGE ( 'NONE', *, *, #72558, .T. ) ;
#12783 = CARTESIAN_POINT ( 'NONE',  ( 7.709236068321770219, 1516.542108215149938, 207.3618294337510122 ) ) ;
#12784 = CARTESIAN_POINT ( 'NONE',  ( -4.161170142469999611, 1448.299083525829928, 185.1109003835979934 ) ) ;
#12785 = CARTESIAN_POINT ( 'NONE',  ( -16.65376764594610037, 1508.454796205149933, 213.7212175226700026 ) ) ;
#12786 = CARTESIAN_POINT ( 'NONE',  ( -40.17892786689739637, 1444.958062479619912, 136.9709319305609938 ) ) ;
#12787 = CIRCLE ( 'NONE', #48542, 2.000000000000001776 ) ;
#12788 = CARTESIAN_POINT ( 'NONE',  ( 11.60004869885213097, 1425.419067644911820, 138.1638145324133689 ) ) ;
#12789 = CARTESIAN_POINT ( 'NONE',  ( 30.25425994617003767, 1526.382868172863937, 199.2916410102368729 ) ) ;
#12790 = CARTESIAN_POINT ( 'NONE',  ( 17.91230580668798211, 1423.874090688956358, 225.7940723398736793 ) ) ;
#12791 = CARTESIAN_POINT ( 'NONE',  ( -12.31627863005989987, 1378.354374910739807, 209.6655814783919709 ) ) ;
#12792 = CARTESIAN_POINT ( 'NONE',  ( -41.54777830462669641, 1453.906998726859911, 269.7546269283009792 ) ) ;
#12793 = CARTESIAN_POINT ( 'NONE',  ( 29.00640787322850045, 1440.913060387239966, 234.9866596484439754 ) ) ;
#12794 = CARTESIAN_POINT ( 'NONE',  ( -20.79315288949999996, 1508.014485607329789, 228.0232908942979861 ) ) ;
#12795 = CARTESIAN_POINT ( 'NONE',  ( 10.21056514295750084, 1500.159686141239945, 203.5544954536850071 ) ) ;
#12796 = ORIENTED_EDGE ( 'NONE', *, *, #93847, .F. ) ;
#12797 = CARTESIAN_POINT ( 'NONE',  ( -2.041421749081904657, 1485.165825109578918, 182.8125668038368303 ) ) ;
#12798 = CARTESIAN_POINT ( 'NONE',  ( -4.360190560360000411, 1441.644575985890015, 201.4346498888789938 ) ) ;
#12799 = CARTESIAN_POINT ( 'NONE',  ( 1.719367447270000016, 1490.891747643629969, 235.7942165053979977 ) ) ;
#12800 = CARTESIAN_POINT ( 'NONE',  ( -10.99853003760000014, 1492.080317501190166, 210.0618239403530083 ) ) ;
#12801 = CARTESIAN_POINT ( 'NONE',  ( -16.45186348020000011, 1509.487572119630158, 233.0276686348979922 ) ) ;
#12802 = CARTESIAN_POINT ( 'NONE',  ( -31.40241232791079895, 1383.840297973970110, 229.3250844799549952 ) ) ;
#12803 = CARTESIAN_POINT ( 'NONE',  ( -3.117394057747560066, 1508.880977799760103, 204.6292041399409811 ) ) ;
#12804 = CARTESIAN_POINT ( 'NONE',  ( 7.121584085660000341, 1409.161751583630121, 222.2855843900980233 ) ) ;
#12805 = FACE_OUTER_BOUND ( 'NONE', #10347, .T. ) ;
#12806 = CARTESIAN_POINT ( 'NONE',  ( 2.033228060669999948, 1464.794380306530002, 236.1307052698979874 ) ) ;
#12808 = ORIENTED_EDGE ( 'NONE', *, *, #30380, .T. ) ;
#12807 = DIRECTION ( 'NONE',  ( 0.000000000000000000, 1.000000000000000000, -0.000000000000000000 ) ) ;
#12809 = CARTESIAN_POINT ( 'NONE',  ( -1.298785104950000102, 1450.901045541719895, 182.8763096061979923 ) ) ;
#12810 = VECTOR ( 'NONE', #34252, 1000.000000000000000 ) ;
#12811 = CARTESIAN_POINT ( 'NONE',  ( -22.93874217539999805, 1382.980169263400057, 202.5862763507190323 ) ) ;
#12812 = CARTESIAN_POINT ( 'NONE',  ( -3.326917603050000061, 1476.247319049890166, 199.3214893299089852 ) ) ;
#12814 = ORIENTED_EDGE ( 'NONE', *, *, #36890, .F. ) ;
#12813 = CARTESIAN_POINT ( 'NONE',  ( -18.07834331186310095, 1415.943166310999914, 208.8325883090850255 ) ) ;
#12815 = CARTESIAN_POINT ( 'NONE',  ( -2.515575408287869852, 1448.349567905599997, 188.5842445502629801 ) ) ;
#12816 = ORIENTED_EDGE ( 'NONE', *, *, #85138, .T. ) ;
#12817 = CARTESIAN_POINT ( 'NONE',  ( -10.24701828192700148, 1387.563789009890115, 217.6416621783679943 ) ) ;
#12818 = CARTESIAN_POINT ( 'NONE',  ( 1.720211288050000009, 1484.988610551289867, 201.3271807748389790 ) ) ;
#12819 = DIRECTION ( 'NONE',  ( -0.05488031785798359874, -0.01377321100617858243, -0.9983979413892970500 ) ) ;
#12820 = CARTESIAN_POINT ( 'NONE',  ( 10.97527900237937715, 1503.727326051738601, 212.8216792447624357 ) ) ;
#12821 = LINE ( 'NONE', #30166, #8836 ) ;
#12822 = CARTESIAN_POINT ( 'NONE',  ( -10.12425452533820014, 1472.594269829849964, 207.2375451810740117 ) ) ;
#12823 = CARTESIAN_POINT ( 'NONE',  ( 2.300012252027449744, 1408.993378584980064, 194.3064046096619961 ) ) ;
#12824 = CARTESIAN_POINT ( 'NONE',  ( 1.249000902699999922E-15, 1417.199650551829791, 167.6845966677979902 ) ) ;
#12825 = CARTESIAN_POINT ( 'NONE',  ( -94.74755207959219661, 1385.206845740749714, 294.8604545563650277 ) ) ;
#12826 = CARTESIAN_POINT ( 'NONE',  ( -17.84189080239999825, 1437.050698146910008, 191.2181082141979971 ) ) ;
#12827 = CARTESIAN_POINT ( 'NONE',  ( 20.71343476517534299, 1522.382868172863937, 238.3377464195763764 ) ) ;
#12828 = AXIS2_PLACEMENT_3D ( 'NONE', #107679, #83026, #58386 ) ;
#12829 = CARTESIAN_POINT ( 'NONE',  ( -0.2129864720161060154, 1450.905624701759962, 126.7681033905349892 ) ) ;
#12830 = EDGE_LOOP ( 'NONE', ( #90851, #83797 ) ) ;
#12831 = ORIENTED_EDGE ( 'NONE', *, *, #48155, .F. ) ;
#12832 = CARTESIAN_POINT ( 'NONE',  ( -7.012466319506879486, 1508.551704615640119, 214.6351047238229910 ) ) ;
#12833 = CARTESIAN_POINT ( 'NONE',  ( 17.92115727113900192, 1457.712037597299968, 229.4665076238089796 ) ) ;
#12834 = AXIS2_PLACEMENT_3D ( 'NONE', #54347, #88478, #97956 ) ;
#12835 = CARTESIAN_POINT ( 'NONE',  ( -11.25904675279999978, 1434.364368409959980, 151.5755386760980059 ) ) ;
#12836 = CARTESIAN_POINT ( 'NONE',  ( -3.883342170835969822E-10, 1466.795683113560017, 244.3026181627860183 ) ) ;
#12837 = CARTESIAN_POINT ( 'NONE',  ( -20.57999989205229951, 1507.217024252700185, 190.4080422748829733 ) ) ;
#12838 = CARTESIAN_POINT ( 'NONE',  ( -15.84432986099999852, 1419.853212303100008, 210.7451137706489703 ) ) ;
#12839 = CARTESIAN_POINT ( 'NONE',  ( -109.5275565480000068, 1385.603864912959807, 311.2689355842589976 ) ) ;
#12840 = CARTESIAN_POINT ( 'NONE',  ( 0.2010921131289999941, 1462.358627342330010, 182.8518807857980164 ) ) ;
#12841 = CARTESIAN_POINT ( 'NONE',  ( -11.67741975794039178, 1363.266342174300917, 209.6218459617033432 ) ) ;
#12842 = CARTESIAN_POINT ( 'NONE',  ( -25.16089740380983386, 1436.602010722529030, 137.5955485560597253 ) ) ;
#12843 = CARTESIAN_POINT ( 'NONE',  ( 3.071538966616301103, 1374.913060387290216, 210.7998353468136941 ) ) ;
#12844 = CARTESIAN_POINT ( 'NONE',  ( -1.135898823814999847, 1516.958737650239982, 208.0022537503870126 ) ) ;
#12845 = CARTESIAN_POINT ( 'NONE',  ( 11.23207286718879949, 1433.984507984109769, 151.5867044815779821 ) ) ;
#12846 = CARTESIAN_POINT ( 'NONE',  ( -13.57458050278340167, 1434.962060795229945, 148.8580072349309944 ) ) ;
#12847 = CARTESIAN_POINT ( 'NONE',  ( -8.030929497949999885, 1385.277656519309858, 218.7696094612490185 ) ) ;
#12848 = DIRECTION ( 'NONE',  ( 0.000000000000000000, 0.000000000000000000, 1.000000000000000000 ) ) ;
#12849 = FACE_OUTER_BOUND ( 'NONE', #49693, .T. ) ;
#12850 = CYLINDRICAL_SURFACE ( 'NONE', #8599, 4.999999999999997335 ) ;
#12851 = ORIENTED_EDGE ( 'NONE', *, *, #100073, .T. ) ;
#12852 = ADVANCED_FACE ( 'NONE', ( #81297 ), #77652, .F. ) ;
#12853 = CARTESIAN_POINT ( 'NONE',  ( -4.322907466360000002E-09, 1413.741945241729809, 248.5896189551980058 ) ) ;
#12854 = CARTESIAN_POINT ( 'NONE',  ( -1.603373619530000127, 1416.384743139180046, 204.3300628165089847 ) ) ;
#12856 = CARTESIAN_POINT ( 'NONE',  ( 2.447291524873689738E-14, 1423.636407223090146, 230.6287594130560024 ) ) ;
#12855 = CARTESIAN_POINT ( 'NONE',  ( -11.02848032900000064, 1426.931206522629736, 92.75091704169790319 ) ) ;
#12857 = LINE ( 'NONE', #3942, #60616 ) ;
#12858 = CARTESIAN_POINT ( 'NONE',  ( -25.00557959500000038, 1439.269656963860143, 216.3898167378279993 ) ) ;
#12859 = CARTESIAN_POINT ( 'NONE',  ( -0.4963980325270009319, 1487.926393457290033, 219.9945907317990077 ) ) ;
#12860 = EDGE_CURVE ( 'NONE', #57270, #38397, #9499, .T. ) ;
#12861 = CARTESIAN_POINT ( 'NONE',  ( 0.7590917812330791881, 1415.513639922078028, 233.2736437612532825 ) ) ;
#12862 = CARTESIAN_POINT ( 'NONE',  ( 27.01382310970000233, 1451.969724731730139, 134.9184576876980088 ) ) ;
#12863 = ORIENTED_EDGE ( 'NONE', *, *, #18575, .T. ) ;
#12864 = DIRECTION ( 'NONE',  ( 0.7636030818040332457, 6.919574257186762174E-11, 0.6456859402676993209 ) ) ;
#12865 = CARTESIAN_POINT ( 'NONE',  ( 12.73370630486426869, 1513.317537406170231, 225.8919084108109701 ) ) ;
#12866 = B_SPLINE_CURVE_WITH_KNOTS ( 'NONE', 3,
 ( #86796, #62179, #63287, #97401, #106354, #20670, #35854, #29640, #97939, #52659 ),
 .UNSPECIFIED., .F., .F.,
 ( 4, 3, 3, 4 ),
 ( -157.4421957110000108, -134.5125350903350068, -78.90080931318131263, -29.52656374274130258 ),
 .UNSPECIFIED. ) ;
#12867 = CARTESIAN_POINT ( 'NONE',  ( 32.02808312589922224, 1512.187213306747481, 219.9649204700462235 ) ) ;
#12868 = ORIENTED_EDGE ( 'NONE', *, *, #33938, .T. ) ;
#12869 = ORIENTED_EDGE ( 'NONE', *, *, #77699, .F. ) ;
#12870 = CARTESIAN_POINT ( 'NONE',  ( 10.56408392316350131, 1452.658046758459932, 209.7429679461859848 ) ) ;
#12871 = CARTESIAN_POINT ( 'NONE',  ( -22.70505693412289716, 1409.705930895240272, 208.9454396691020008 ) ) ;
#12872 = ORIENTED_EDGE ( 'NONE', *, *, #61336, .T. ) ;
#12873 = AXIS2_PLACEMENT_3D ( 'NONE', #3924, #10655, #88995 ) ;
#12874 = CARTESIAN_POINT ( 'NONE',  ( -15.17703146246870105, 1445.095302021130010, 196.7536351334289861 ) ) ;
#12875 = CARTESIAN_POINT ( 'NONE',  ( 4.291176059336820003, 1446.971469614359876, 154.7965853925720126 ) ) ;
#12876 = CARTESIAN_POINT ( 'NONE',  ( -0.6623973197610000252, 1470.488054031330194, 235.6950254979980173 ) ) ;
#12877 = DIRECTION ( 'NONE',  ( 0.9455185755993178454, 0.000000000000000000, -0.3255681544571539243 ) ) ;
#12878 = ORIENTED_EDGE ( 'NONE', *, *, #68151, .T. ) ;
#12879 =( NAMED_UNIT ( * ) SI_UNIT ( $, .STERADIAN. ) SOLID_ANGLE_UNIT ( ) );
#12880 = CARTESIAN_POINT ( 'NONE',  ( -3.487587049061890099, 1508.884219112060009, 204.6305577843690173 ) ) ;
#12881 = CARTESIAN_POINT ( 'NONE',  ( 2.330134126767420266, 1515.064792882699976, 204.7923971855439902 ) ) ;
#12882 = CARTESIAN_POINT ( 'NONE',  ( -1.132949114555000136, 1516.693851263360102, 204.1241276937270186 ) ) ;
#12883 = ORIENTED_EDGE ( 'NONE', *, *, #69252, .F. ) ;
#12884 = CARTESIAN_POINT ( 'NONE',  ( 5.697020712293880962, 1483.840076960939996, 219.4998280688900252 ) ) ;
#12885 = AXIS2_PLACEMENT_3D ( 'NONE', #6184, #77810, #102438 ) ;
#12886 = CARTESIAN_POINT ( 'NONE',  ( 12.80669964242905223, 1442.848007414932908, 186.8680711929162328 ) ) ;
#12887 = ORIENTED_EDGE ( 'NONE', *, *, #21584, .F. ) ;
#12888 = ORIENTED_EDGE ( 'NONE', *, *, #85913, .T. ) ;
#12889 = CARTESIAN_POINT ( 'NONE',  ( 2.582675909239575240, 1526.178928173327677, 175.9008252398585626 ) ) ;
#12890 = CARTESIAN_POINT ( 'NONE',  ( -3.672693132570179930, 1508.551704069029938, 220.1143460865109773 ) ) ;
#12891 = CARTESIAN_POINT ( 'NONE',  ( 13.43167347780000043, 1509.382104760729817, 235.1752220498979966 ) ) ;
#12892 =( BOUNDED_CURVE ( )  B_SPLINE_CURVE ( 3, ( #45209, #17180, #1543, #51373 ),
 .UNSPECIFIED., .F., .T. ) 
 B_SPLINE_CURVE_WITH_KNOTS ( ( 4, 4 ),
 ( 1.861138363454700073, 2.499452639686874811 ),
 .UNSPECIFIED. ) 
 CURVE ( )  GEOMETRIC_REPRESENTATION_ITEM ( )  RATIONAL_B_SPLINE_CURVE ( ( 1.000000000000000000, 0.9663334780259177359, 0.9663334780259177359, 1.000000000000000000 ) ) 
 REPRESENTATION_ITEM ( '' )  );
#12893 = CARTESIAN_POINT ( 'NONE',  ( -9.531705855666331217, 1470.352007687029982, 213.6243478951139991 ) ) ;
#12894 = CARTESIAN_POINT ( 'NONE',  ( 13.66841340714169917, 1452.435748873430157, 148.7307978952950123 ) ) ;
#12895 = CARTESIAN_POINT ( 'NONE',  ( 9.558212104659999042, 1420.850661932230196, 197.1275686703990004 ) ) ;
#12896 = CARTESIAN_POINT ( 'NONE',  ( -1.509201711952470104, 1475.790545536990066, 220.4654702390089938 ) ) ;
#12897 = CARTESIAN_POINT ( 'NONE',  ( -7.344663150544599617, 1494.134771815259910, 199.2391034037320026 ) ) ;
#12898 = CARTESIAN_POINT ( 'NONE',  ( -10.97167842400910054, 1432.478566107110055, 151.7700680134270215 ) ) ;
#12899 = CARTESIAN_POINT ( 'NONE',  ( 0.000000000000000000, 1508.913060387330006, 224.7618459619980058 ) ) ;
#12900 = CARTESIAN_POINT ( 'NONE',  ( -1.600048698852036821, 1411.254281879943164, 137.0999999980979851 ) ) ;
#12901 = CARTESIAN_POINT ( 'NONE',  ( -16.71457808692061420, 1379.711298523256573, 211.9342710108481072 ) ) ;
#12902 = CARTESIAN_POINT ( 'NONE',  ( -24.12862833684370045, 1508.487934531239944, 222.3657772772859857 ) ) ;
#12903 = CARTESIAN_POINT ( 'NONE',  ( -6.098897551624999913, 1511.444830760690138, 201.4618419945269920 ) ) ;
#12904 = ORIENTED_EDGE ( 'NONE', *, *, #84370, .T. ) ;
#12905 = CARTESIAN_POINT ( 'NONE',  ( 19.55988977460000200, 1474.636381753090063, 214.0184790771390055 ) ) ;
#12906 = FACE_OUTER_BOUND ( 'NONE', #49382, .T. ) ;
#12907 = CARTESIAN_POINT ( 'NONE',  ( -96.47393723009329847, 1384.954577916420021, 310.3344438142669901 ) ) ;
#12908 = CARTESIAN_POINT ( 'NONE',  ( -9.493009264660001278, 1386.944172907939901, 200.5464424274789792 ) ) ;
#12909 = CARTESIAN_POINT ( 'NONE',  ( -15.22934408750000124, 1415.677402202029953, 210.1988070706289875 ) ) ;
#12911 = ORIENTED_EDGE ( 'NONE', *, *, #7650, .F. ) ;
#12910 = CARTESIAN_POINT ( 'NONE',  ( -4.146782895030730387, 1426.018316030089863, 186.1121555109529879 ) ) ;
#12912 = CARTESIAN_POINT ( 'NONE',  ( -2.746125756363450243, 1440.068789215269817, 157.5210582709530058 ) ) ;
#12913 = CARTESIAN_POINT ( 'NONE',  ( -8.092117112805246038, 1477.146199184617444, 215.6332617364606392 ) ) ;
#12914 = CARTESIAN_POINT ( 'NONE',  ( 9.377597136699939995, 1436.953564941884679, 212.2519927847499162 ) ) ;
#12915 = CARTESIAN_POINT ( 'NONE',  ( 12.15948096493499975, 1512.592133792520144, 225.7486201106670194 ) ) ;
#12916 = CARTESIAN_POINT ( 'NONE',  ( 12.93742170084699872, 1415.431750870129918, 196.9031077866209785 ) ) ;
#12917 = CARTESIAN_POINT ( 'NONE',  ( 29.36867415615326493, 1526.382868172863937, 217.2593511714356396 ) ) ;
#12918 = B_SPLINE_CURVE_WITH_KNOTS ( 'NONE', 5,
 ( #9384, #110736, #43547, #35132, #69314, #103421, #60918, #18315, #52506, #86635, #28395, #62595, #11596, #89403, #63142 ),
 .UNSPECIFIED., .F., .F.,
 ( 6, 3, 3, 3, 6 ),
 ( 0.000000000000000000, 0.2487888922080676302, 0.5151303747020953283, 0.7162082858933614959, 1.000000000000000000 ),
 .UNSPECIFIED. ) ;
#12919 = FACE_OUTER_BOUND ( 'NONE', #103210, .T. ) ;
#12920 = CARTESIAN_POINT ( 'NONE',  ( 14.98057229850000027, 1422.105921276430081, 228.0570637948979993 ) ) ;
#12921 = CARTESIAN_POINT ( 'NONE',  ( -21.92916355573673570, 1523.390106123591067, 235.1782814742750816 ) ) ;
#12922 = CARTESIAN_POINT ( 'NONE',  ( -2.882326017515000061, 1516.969638403840008, 207.4201161117570109 ) ) ;
#12923 = CARTESIAN_POINT ( 'NONE',  ( 43.99407931230000202, 1429.912879050529909, 268.5626800188979928 ) ) ;
#12924 = CARTESIAN_POINT ( 'NONE',  ( -18.23736806889999684, 1410.046425294630126, 223.9609750991980093 ) ) ;
#12925 = CARTESIAN_POINT ( 'NONE',  ( 16.20369265950000326, 1435.886343892520017, 148.6899262114979763 ) ) ;
#12926 = CARTESIAN_POINT ( 'NONE',  ( -1.341411944869999928, 1418.672989064230023, 228.1617829935980239 ) ) ;
#12927 = CARTESIAN_POINT ( 'NONE',  ( 20.22895499020875576, 1427.701001985137054, 222.9553950507804814 ) ) ;
#12928 = CARTESIAN_POINT ( 'NONE',  ( -17.73407118999999810, 1423.343216095430080, 226.1884512641980223 ) ) ;
#12929 = CARTESIAN_POINT ( 'NONE',  ( 12.50106635730310067, 1427.054470077530141, 206.4470538787940086 ) ) ;
#12930 = CARTESIAN_POINT ( 'NONE',  ( -34.93809870825160147, 1435.719286479559969, 135.4750084030100084 ) ) ;
#12931 = CARTESIAN_POINT ( 'NONE',  ( 0.2168213374743849786, 1453.534145733320202, 183.2304789241289882 ) ) ;
#12932 = CARTESIAN_POINT ( 'NONE',  ( -8.967593744529999356, 1409.166218292129997, 220.9728305157979946 ) ) ;
#12933 = CARTESIAN_POINT ( 'NONE',  ( -0.1387231356229999824, 1418.535612649829773, 184.6749245791980059 ) ) ;
#12934 = CARTESIAN_POINT ( 'NONE',  ( -4.201139955930000447, 1515.456931311890003, 208.0107056655590156 ) ) ;
#12935 = CARTESIAN_POINT ( 'NONE',  ( -28.64126805841279833, 1509.753974595000273, 211.2596818611239939 ) ) ;
#12936 = CARTESIAN_POINT ( 'NONE',  ( 12.91324334049999933, 1434.774337969269936, 147.6246349161979765 ) ) ;
#12937 = CARTESIAN_POINT ( 'NONE',  ( 12.53380499169999851, 1445.052233488290085, 169.4755105685979970 ) ) ;
#12938 = CARTESIAN_POINT ( 'NONE',  ( 7.146336540040000074, 1441.350815057550108, 185.4538290344979714 ) ) ;
#12939 = ORIENTED_EDGE ( 'NONE', *, *, #46392, .T. ) ;
#12940 = CARTESIAN_POINT ( 'NONE',  ( 6.343099782127201713, 1511.025938525906668, 216.5295357475528704 ) ) ;
#12941 = CARTESIAN_POINT ( 'NONE',  ( 39.43202460889999372, 1438.613999458619901, 136.5563049865980076 ) ) ;
#12942 = CARTESIAN_POINT ( 'NONE',  ( -11.79257188989999960, 1490.424927487490095, 209.6468054275469797 ) ) ;
#12943 = CARTESIAN_POINT ( 'NONE',  ( -2.705738833059999848, 1468.840749178389842, 189.3603025906990069 ) ) ;
#12944 = CARTESIAN_POINT ( 'NONE',  ( 10.02421119480000122, 1480.534221758890226, 205.8829018067289951 ) ) ;
#12945 = CARTESIAN_POINT ( 'NONE',  ( -46.27884720130000318, 1440.913036523590108, 267.5894368609980347 ) ) ;
#12946 = CARTESIAN_POINT ( 'NONE',  ( -11.76640019110000068, 1437.123680669209989, 147.7210023317979903 ) ) ;
#12947 = CARTESIAN_POINT ( 'NONE',  ( 19.76088122879999887, 1434.994518313850222, 210.4584719956679919 ) ) ;
#12948 = CARTESIAN_POINT ( 'NONE',  ( -24.93044165159999892, 1508.532778223230025, 220.3720830472979912 ) ) ;
#12949 = CARTESIAN_POINT ( 'NONE',  ( -87.22487244391929551, 1384.624363658659831, 307.6774912203520671 ) ) ;
#12950 = CARTESIAN_POINT ( 'NONE',  ( -41.91864753602830262, 1384.994678410510005, 214.8065739413959818 ) ) ;
#12951 = CARTESIAN_POINT ( 'NONE',  ( -18.02257621027557377, 1526.382868172863937, 235.3484976865589147 ) ) ;
#12952 = CARTESIAN_POINT ( 'NONE',  ( -4.821236195118149936, 1508.551704408389924, 205.7350742881380086 ) ) ;
#12953 = CARTESIAN_POINT ( 'NONE',  ( -27.77560365120000085, 1451.943158935029942, 134.8960326030979786 ) ) ;
#12954 = CARTESIAN_POINT ( 'NONE',  ( -2.622430729442961184, 1523.621879633028811, 176.0901726876731459 ) ) ;
#12956 = VERTEX_POINT ( 'NONE', #104716 ) ;
#12955 = CARTESIAN_POINT ( 'NONE',  ( -2.098112454099999802, 1502.392812899289993, 230.4314219549989957 ) ) ;
#12957 = CARTESIAN_POINT ( 'NONE',  ( -9.592658376373048412, 1460.893772936906089, 207.6096792123005343 ) ) ;
#12958 = LINE ( 'NONE', #45509, #69049 ) ;
#12959 = CARTESIAN_POINT ( 'NONE',  ( -5.079869688909999681, 1496.157899184890084, 219.1414376983989882 ) ) ;
#12960 = CARTESIAN_POINT ( 'NONE',  ( 3.487592429471666033, 1508.909942010301620, 204.6312267328975452 ) ) ;
#12961 = CARTESIAN_POINT ( 'NONE',  ( 0.003812576784339999879, 1466.393772618229832, 235.6965108690979775 ) ) ;
#12962 = CARTESIAN_POINT ( 'NONE',  ( 22.52035456810000014, 1409.863932199730016, 213.1945697568480114 ) ) ;
#12963 = CARTESIAN_POINT ( 'NONE',  ( 3.229842584605000066, 1517.051704408389924, 200.7619551613470037 ) ) ;
#12964 = CARTESIAN_POINT ( 'NONE',  ( -9.701071637315321183, 1463.456538005379798, 228.1046814505860141 ) ) ;
#12965 = LINE ( 'NONE', #71840, #98289 ) ;
#12967 = CARTESIAN_POINT ( 'NONE',  ( -13.46522613409999991, 1379.673148676610026, 207.0022512300789685 ) ) ;
#12966 = CARTESIAN_POINT ( 'NONE',  ( -11.77090792110000095, 1432.440105173310030, 150.8116828678980141 ) ) ;
#12968 = CARTESIAN_POINT ( 'NONE',  ( 28.15873685633160051, 1508.155813927709914, 208.2598873620850100 ) ) ;
#12969 = CARTESIAN_POINT ( 'NONE',  ( -102.2221789262000016, 1377.418846546389659, 307.0760123268498205 ) ) ;
#12970 = CARTESIAN_POINT ( 'NONE',  ( -113.4000000000000057, 1378.913060387289988, 304.2218459572590064 ) ) ;
#12971 = FACE_OUTER_BOUND ( 'NONE', #74099, .T. ) ;
#12972 = CARTESIAN_POINT ( 'NONE',  ( -7.592149787969999508, 1361.964468435470053, 210.6218459616991936 ) ) ;
#12973 = CARTESIAN_POINT ( 'NONE',  ( 7.323034273964999841, 1516.609912606490070, 205.6670971239069843 ) ) ;
#12974 = CARTESIAN_POINT ( 'NONE',  ( -8.348176302887580391, 1484.298473836920039, 184.3911193790379741 ) ) ;
#12975 = EDGE_LOOP ( 'NONE', ( #31553, #92556, #58473, #34003, #52841 ) ) ;
#12976 = CARTESIAN_POINT ( 'NONE',  ( 11.85236273005710039, 1501.984533761569764, 213.9659136087529987 ) ) ;
#12977 = CARTESIAN_POINT ( 'NONE',  ( 18.83207817909999804, 1416.311719782429918, 210.6697760117079952 ) ) ;
#12979 = VERTEX_POINT ( 'NONE', #45932 ) ;
#12978 = CARTESIAN_POINT ( 'NONE',  ( -68.31931742147419584, 1379.746951998870145, 279.9044409820210149 ) ) ;
#12980 = ORIENTED_EDGE ( 'NONE', *, *, #97538, .F. ) ;
#12981 = CARTESIAN_POINT ( 'NONE',  ( 28.09217170250000351, 1508.632189945129994, 210.4865295626480020 ) ) ;
#12982 = EDGE_LOOP ( 'NONE', ( #103564, #28910, #892, #89721 ) ) ;
#12983 = CARTESIAN_POINT ( 'NONE',  ( 3.128860413254639816, 1484.852474905719873, 220.5520654540769954 ) ) ;
#12984 = CARTESIAN_POINT ( 'NONE',  ( 10.93419921699999975, 1501.146262457190005, 205.7756198371390042 ) ) ;
#12986 = DIRECTION ( 'NONE',  ( 1.755985294532469921E-16, -1.000000000000000000, 1.338183447452831989E-16 ) ) ;
#12985 = CARTESIAN_POINT ( 'NONE',  ( 0.7625704858929999164, 1427.674934138829940, 112.4493539157979995 ) ) ;
#12987 = CARTESIAN_POINT ( 'NONE',  ( 3.269025135755000200, 1517.026534522949987, 210.2412850599169758 ) ) ;
#12988 = CARTESIAN_POINT ( 'NONE',  ( -24.43329073687169739, 1451.996401077730070, 136.8824426089099973 ) ) ;
#12989 = CARTESIAN_POINT ( 'NONE',  ( -10.81509838440000060, 1424.921163249430037, 144.1641696258980119 ) ) ;
#12990 = CARTESIAN_POINT ( 'NONE',  ( 14.33852263799999882, 1409.413772630230142, 226.7380482434979854 ) ) ;
#12991 = CARTESIAN_POINT ( 'NONE',  ( 9.239580200065189430, 1483.101234906810078, 214.6484747421150132 ) ) ;
#12992 = CARTESIAN_POINT ( 'NONE',  ( 0.000000000000000000, 0.000000000000000000, 0.000000000000000000 ) ) ;
#12993 = CARTESIAN_POINT ( 'NONE',  ( 39.63067020500510296, 1438.364472239110000, 134.0999999979140114 ) ) ;
#12994 = DIRECTION ( 'NONE',  ( -5.980589973904019347E-17, 1.000000000000000000, -1.736889445713099699E-16 ) ) ;
#12995 = CARTESIAN_POINT ( 'NONE',  ( -17.65533327544169850, 1419.497269525679940, 207.2321674072659903 ) ) ;
#12996 = CARTESIAN_POINT ( 'NONE',  ( -16.80365118935687363, 1410.870881529783446, 226.3880813221334449 ) ) ;
#12997 = ORIENTED_EDGE ( 'NONE', *, *, #102214, .F. ) ;
#12998 = ORIENTED_EDGE ( 'NONE', *, *, #57592, .T. ) ;
#12999 = ORIENTED_EDGE ( 'NONE', *, *, #68110, .T. ) ;
#13000 = CARTESIAN_POINT ( 'NONE',  ( 10.01592177394908134, 1410.637502406660360, 229.8105954444164354 ) ) ;
#13001 = CARTESIAN_POINT ( 'NONE',  ( 32.10255801038882595, 1525.211477436245787, 217.0238529843554716 ) ) ;
#13002 = CARTESIAN_POINT ( 'NONE',  ( -14.10694522062919987, 1379.843704623709982, 211.3636899608110014 ) ) ;
#13003 = CARTESIAN_POINT ( 'NONE',  ( -3.092456351079999610, 1485.137949221930057, 183.1787329613979978 ) ) ;
#13004 = CARTESIAN_POINT ( 'NONE',  ( -17.59211063817642895, 1448.069329004949168, 217.8528919356413667 ) ) ;
#13005 = CARTESIAN_POINT ( 'NONE',  ( -64.34879093311614895, 1379.737658639894562, 270.9436941998574184 ) ) ;
#13006 = CARTESIAN_POINT ( 'NONE',  ( -1.935234340010000054, 1464.825742489889763, 198.7112508957989974 ) ) ;
#13007 = CARTESIAN_POINT ( 'NONE',  ( -1.115466430919999974, 1497.688001115629959, 231.6381069598980105 ) ) ;
#13008 = CARTESIAN_POINT ( 'NONE',  ( 7.803088030789999685, 1414.971262582530017, 194.2636415098980081 ) ) ;
#13009 = CARTESIAN_POINT ( 'NONE',  ( -57.51057651963380124, 1384.658127080889926, 238.7961619097730193 ) ) ;
#13010 = ORIENTED_EDGE ( 'NONE', *, *, #90350, .T. ) ;
#13011 = CARTESIAN_POINT ( 'NONE',  ( 4.608021669135000664, 1516.660388280709867, 207.4085285224269910 ) ) ;
#13012 = ORIENTED_EDGE ( 'NONE', *, *, #36587, .F. ) ;
#13013 = CARTESIAN_POINT ( 'NONE',  ( 11.33192160910000013, 1414.988015876829877, 222.3303154034980196 ) ) ;
#13014 = CARTESIAN_POINT ( 'NONE',  ( 18.79931365210000038, 1467.189280536129900, 227.8818516051979941 ) ) ;
#13015 = EDGE_LOOP ( 'NONE', ( #81408, #16714, #27284 ) ) ;
#13016 = CARTESIAN_POINT ( 'NONE',  ( -0.2055871306533119947, 1452.986193894690132, 183.2455700887460068 ) ) ;
#13017 = CARTESIAN_POINT ( 'NONE',  ( -8.588755447433969792, 1437.818850531529961, 207.9413692731380081 ) ) ;
#13018 = CARTESIAN_POINT ( 'NONE',  ( -17.52838533095563989, 1508.456237627404562, 212.5777381106094879 ) ) ;
#13019 = CARTESIAN_POINT ( 'NONE',  ( -24.34734233041475093, 1439.542451668733065, 212.0350045365903497 ) ) ;
#13020 = CARTESIAN_POINT ( 'NONE',  ( -8.546921754562520235, 1436.723958230239987, 213.9303451536549971 ) ) ;
#13021 = CARTESIAN_POINT ( 'NONE',  ( -5.554947045494709634, 1511.433089852210060, 200.9123561315769848 ) ) ;
#13022 = CARTESIAN_POINT ( 'NONE',  ( 2.764799436670000166, 1406.050782495030035, 266.9581426506979938 ) ) ;
#13023 = CARTESIAN_POINT ( 'NONE',  ( -5.551188713984379852, 1510.480349263560129, 201.5713426139130320 ) ) ;
#13025 = EDGE_CURVE ( 'NONE', #102287, #55469, #29534, .T. ) ;
#13024 = CARTESIAN_POINT ( 'NONE',  ( 25.50965763837719891, 1477.613428519450053, 206.2229539054640099 ) ) ;
#13026 = CARTESIAN_POINT ( 'NONE',  ( 15.73405928501899886, 1409.498448401794349, 192.5840719006893949 ) ) ;
#13027 = CARTESIAN_POINT ( 'NONE',  ( 2.292940169014999974, 1516.565291103010168, 215.6678853655270132 ) ) ;
#13028 = DIRECTION ( 'NONE',  ( 0.3363363969979660806, 0.9417419115949053898, 0.000000000000000000 ) ) ;
#13029 = CARTESIAN_POINT ( 'NONE',  ( -10.46978020201859039, 1480.344165297236941, 208.0133452714284772 ) ) ;
#13030 = CARTESIAN_POINT ( 'NONE',  ( 3.235048515759559873, 1466.472015849239824, 219.6884157167970102 ) ) ;
#13031 = CARTESIAN_POINT ( 'NONE',  ( -4.997573825325000385, 1516.742629295279812, 212.5803724681170195 ) ) ;
#13032 = CARTESIAN_POINT ( 'NONE',  ( -20.46400528210000047, 1470.815019615029996, 209.2097780812300130 ) ) ;
#13033 = CARTESIAN_POINT ( 'NONE',  ( 18.42577555256999844, 1424.509265906519886, 223.4215472205989954 ) ) ;
#13035 = ORIENTED_EDGE ( 'NONE', *, *, #31050, .F. ) ;
#13034 = CARTESIAN_POINT ( 'NONE',  ( -6.785810196629999957, 1424.002256156930116, 192.0785610996990158 ) ) ;
#13036 = CARTESIAN_POINT ( 'NONE',  ( -17.72020223055791632, 1524.201670966335769, 237.7556192861110560 ) ) ;
#13037 = CARTESIAN_POINT ( 'NONE',  ( 10.82580776920000076, 1458.182933819829941, 213.1729752121979971 ) ) ;
#13038 = CARTESIAN_POINT ( 'NONE',  ( -11.84746402709999913, 1431.045614906520086, 149.8348319904980031 ) ) ;
#13039 = CARTESIAN_POINT ( 'NONE',  ( -15.22114443889999968, 1415.799205417750045, 206.7037562793690029 ) ) ;
#13040 = CARTESIAN_POINT ( 'NONE',  ( -31.34137657934027388, 1523.382868172864164, 196.3411265156551906 ) ) ;
#13041 = CARTESIAN_POINT ( 'NONE',  ( 7.398264911990000137, 1422.106259636749883, 195.6015909957990289 ) ) ;
#13042 = CARTESIAN_POINT ( 'NONE',  ( -5.080191068885199890, 1480.093223193510084, 228.8813504292600101 ) ) ;
#13044 = FACE_OUTER_BOUND ( 'NONE', #27093, .T. ) ;
#13043 = CARTESIAN_POINT ( 'NONE',  ( -20.99010852809999861, 1470.085365941430155, 224.6554786799979979 ) ) ;
#13045 = CARTESIAN_POINT ( 'NONE',  ( -12.28855869350000063, 1378.253616442990051, 210.0769077263690008 ) ) ;
#13046 = VERTEX_POINT ( 'NONE', #47037 ) ;
#13047 = CARTESIAN_POINT ( 'NONE',  ( 7.323034273964999841, 1516.609912606490070, 205.6670971239069843 ) ) ;
#13048 = CARTESIAN_POINT ( 'NONE',  ( 3.443661293909999976, 1405.813131581129937, 267.8489083852979888 ) ) ;
#13049 = CARTESIAN_POINT ( 'NONE',  ( -4.653281936863520762, 1425.827070423550140, 186.2156739099499987 ) ) ;
#13050 = EDGE_CURVE ( 'NONE', #7383, #102192, #44225, .T. ) ;
#13051 = ADVANCED_FACE ( 'NONE', ( #36955 ), #23628, .T. ) ;
#13052 = CARTESIAN_POINT ( 'NONE',  ( 23.23643549727285063, 1432.926938218388614, 215.5924835263426758 ) ) ;
#13053 = EDGE_CURVE ( 'NONE', #42334, #96903, #20691, .T. ) ;
#13054 = CARTESIAN_POINT ( 'NONE',  ( -0.4102078045352910429, 1463.514555870267714, 199.3390046908783404 ) ) ;
#13055 = CARTESIAN_POINT ( 'NONE',  ( 11.60004869885203682, 1424.919899798115239, 136.4495436088716360 ) ) ;
#13056 = ADVANCED_FACE ( 'NONE', ( #105838 ), #85664, .F. ) ;
#13057 = CARTESIAN_POINT ( 'NONE',  ( -9.828024340748898524, 1446.801136768030119, 212.2328356403849909 ) ) ;
#13058 = CARTESIAN_POINT ( 'NONE',  ( -0.8745088286755380302, 1450.882521866100205, 155.0624047495070101 ) ) ;
#13059 = CARTESIAN_POINT ( 'NONE',  ( -1.554659401664016727, 1451.069394390376146, 183.6377582331552674 ) ) ;
#13060 = EDGE_CURVE ( 'NONE', #95045, #31004, #47900, .T. ) ;
#13061 = CARTESIAN_POINT ( 'NONE',  ( -19.65651483509421382, 1486.193852463049325, 190.0039420846813982 ) ) ;
#13062 = ADVANCED_FACE ( 'NONE', ( #6109 ), #90662, .T. ) ;
#13063 = CARTESIAN_POINT ( 'NONE',  ( -13.54623986534339863, 1415.059973079209840, 220.4667060011670117 ) ) ;
#13064 = DIRECTION ( 'NONE',  ( 0.000000000000000000, 0.000000000000000000, -1.000000000000000000 ) ) ;
#13065 = CARTESIAN_POINT ( 'NONE',  ( -10.05164999069999965, 1426.487183120430245, 224.8635561966979708 ) ) ;
#13066 = CARTESIAN_POINT ( 'NONE',  ( -26.90036304580700133, 1508.005472205750038, 211.7893878585630034 ) ) ;
#13067 = DIRECTION ( 'NONE',  ( 5.980589973904019347E-17, -1.000000000000000000, 1.736889445713099699E-16 ) ) ;
#13068 = CARTESIAN_POINT ( 'NONE',  ( -0.8789521870270000647, 1475.313312798630022, 269.4984183591980127 ) ) ;
#13069 = CARTESIAN_POINT ( 'NONE',  ( -11.78824854703250047, 1517.151704408390060, 206.8304425649369875 ) ) ;
#13070 = CARTESIAN_POINT ( 'NONE',  ( -18.17365796220000007, 1441.208305948289762, 213.5442559039389891 ) ) ;
#13071 = CARTESIAN_POINT ( 'NONE',  ( 7.196800634449999734, 1423.618640619720054, 213.1214840613790216 ) ) ;
#13072 = CARTESIAN_POINT ( 'NONE',  ( -39.86052437841249940, 1384.788194491199874, 241.8866321169209925 ) ) ;
#13073 = CARTESIAN_POINT ( 'NONE',  ( -16.81223434880759982, 1414.913060387349788, 207.5743820648510223 ) ) ;
#13074 = B_SPLINE_CURVE_WITH_KNOTS ( 'NONE', 5,
 ( #40500, #99286, #22013, #74678, #22562, #15280 ),
 .UNSPECIFIED., .F., .F.,
 ( 6, 6 ),
 ( 496.9399198659999684, 502.1482307969999965 ),
 .UNSPECIFIED. ) ;
#13075 = CARTESIAN_POINT ( 'NONE',  ( 12.17122754174319788, 1491.569219868120172, 207.3549893034999911 ) ) ;
#13076 = CARTESIAN_POINT ( 'NONE',  ( -20.28160989820316473, 1526.000688113805609, 184.8337570730359118 ) ) ;
#13077 = CARTESIAN_POINT ( 'NONE',  ( 8.353190717051095504, 1511.405768592756431, 204.6347806277314305 ) ) ;
#13078 = CARTESIAN_POINT ( 'NONE',  ( -11.06418126257080026, 1396.299430110810135, 209.4736323295360023 ) ) ;
#13079 = EDGE_CURVE ( 'NONE', #87972, #65907, #2167, .T. ) ;
#13080 =( BOUNDED_CURVE ( )  B_SPLINE_CURVE ( 3, ( #101436, #17990, #8491, #67889 ),
 .UNSPECIFIED., .F., .T. ) 
 B_SPLINE_CURVE_WITH_KNOTS ( ( 4, 4 ),
 ( 4.286339028762302661, 4.712350959126750283 ),
 .UNSPECIFIED. ) 
 CURVE ( )  GEOMETRIC_REPRESENTATION_ITEM ( )  RATIONAL_B_SPLINE_CURVE ( ( 1.000000000000000000, 0.9849332492076060541, 0.9849332492076060541, 1.000000000000000000 ) ) 
 REPRESENTATION_ITEM ( '' )  );
#13081 = CARTESIAN_POINT ( 'NONE',  ( -14.46398808510000045, 1422.169897544629976, 229.1124523973979876 ) ) ;
#13082 = CARTESIAN_POINT ( 'NONE',  ( 19.61749532786501504, 1455.455351503277598, 225.9183519794877384 ) ) ;
#13083 = ORIENTED_EDGE ( 'NONE', *, *, #30416, .T. ) ;
#13084 = CARTESIAN_POINT ( 'NONE',  ( -2.355634153848364942, 1410.373534213158564, 232.7087846842507588 ) ) ;
#13086 = EDGE_CURVE ( 'NONE', #8406, #90277, #30253, .T. ) ;
#13085 = CARTESIAN_POINT ( 'NONE',  ( 2.671304308019999851, 1410.383647588429994, 231.6679768729979969 ) ) ;
#13087 = DIRECTION ( 'NONE',  ( 1.000000000000000000, -3.196303315166338322E-31, 4.657260248767550292E-10 ) ) ;
#13089 = CARTESIAN_POINT ( 'NONE',  ( -12.18971938666500066, 1512.123542805230272, 194.3960765485670095 ) ) ;
#13088 = CARTESIAN_POINT ( 'NONE',  ( 11.15439083589999925, 1426.467706535029947, 101.9064184266980106 ) ) ;
#13090 = CARTESIAN_POINT ( 'NONE',  ( 11.74015320060000001, 1428.979986575930070, 144.1938086916980239 ) ) ;
#13091 = EDGE_CURVE ( 'NONE', #35126, #33349, #26654, .T. ) ;
#13092 = CARTESIAN_POINT ( 'NONE',  ( -5.192525392799999473, 1454.457094112089862, 201.2666327733590208 ) ) ;
#13093 = CARTESIAN_POINT ( 'NONE',  ( -6.556022232634999725, 1516.833525648419936, 202.1813725979570222 ) ) ;
#13094 = CARTESIAN_POINT ( 'NONE',  ( 7.156887453669999566, 1427.109879847909951, 213.1306117699590175 ) ) ;
#13095 = CARTESIAN_POINT ( 'NONE',  ( -9.609284535499998725, 1429.602790706330097, 148.1400166355980161 ) ) ;
#13096 = CARTESIAN_POINT ( 'NONE',  ( 3.450834020359999865, 1508.929450314329870, 180.3008642914979873 ) ) ;
#13097 = CARTESIAN_POINT ( 'NONE',  ( -22.99236997363790280, 1417.360559190849926, 209.8837839782780179 ) ) ;
#13098 = CARTESIAN_POINT ( 'NONE',  ( -67.06482036316408823, 1379.301523365260209, 281.5316999258700434 ) ) ;
#13099 = EDGE_CURVE ( 'NONE', #24662, #8790, #108574, .T. ) ;
#13100 = CARTESIAN_POINT ( 'NONE',  ( 7.503748088656135629, 1365.688229612017949, 208.3718459617061285 ) ) ;
#13102 = ORIENTED_EDGE ( 'NONE', *, *, #102697, .T. ) ;
#13101 = CARTESIAN_POINT ( 'NONE',  ( 8.171450972760000653, 1453.343394502490128, 214.0171812195989673 ) ) ;
#13103 = ORIENTED_EDGE ( 'NONE', *, *, #53572, .T. ) ;
#13104 = CARTESIAN_POINT ( 'NONE',  ( -10.56206167739999913, 1397.610775313830118, 200.9354534292479855 ) ) ;
#13105 = CARTESIAN_POINT ( 'NONE',  ( 2.777171832513400052, 1409.013373976660205, 230.3099596325619984 ) ) ;
#13106 = CARTESIAN_POINT ( 'NONE',  ( -1.326919707039999841, 1414.988017870030035, 226.4745228631980183 ) ) ;
#13107 = CARTESIAN_POINT ( 'NONE',  ( -13.15002888018213056, 1444.757386539127083, 169.3984147371142512 ) ) ;
#13108 = CARTESIAN_POINT ( 'NONE',  ( -33.42844755917204225, 1501.977400791986611, 196.1165140606796058 ) ) ;
#13109 = DIRECTION ( 'NONE',  ( -2.664535259100375697E-15, 0.000000000000000000, 1.000000000000000000 ) ) ;
#13111 = CARTESIAN_POINT ( 'NONE',  ( -21.50400446119279962, 1505.467562055609960, 209.6175409707290100 ) ) ;
#13110 = CARTESIAN_POINT ( 'NONE',  ( -7.768842288840000165, 1384.896297089400150, 218.9179251193590119 ) ) ;
#13112 = CARTESIAN_POINT ( 'NONE',  ( 12.12259107610000086, 1429.760645300329998, 188.8483479879979825 ) ) ;
#13113 =( NAMED_UNIT ( * ) SI_UNIT ( $, .STERADIAN. ) SOLID_ANGLE_UNIT ( ) );
#13114 = CARTESIAN_POINT ( 'NONE',  ( -40.40395559827349814, 1447.793233377660044, 135.9869587023879944 ) ) ;
#13115 = CARTESIAN_POINT ( 'NONE',  ( 11.01686548338170013, 1396.297777807429839, 210.2008554867939836 ) ) ;
#13116 = DIRECTION ( 'NONE',  ( -1.836970198721029688E-16, -1.000000000000000000, 0.000000000000000000 ) ) ;
#13117 = CARTESIAN_POINT ( 'NONE',  ( 11.84480386869999968, 1430.772386585429786, 150.1926085328979923 ) ) ;
#13118 = CARTESIAN_POINT ( 'NONE',  ( 40.26734871130000215, 1444.073094270329875, 137.1207092272979935 ) ) ;
#13119 = VERTEX_POINT ( 'NONE', #108014 ) ;
#13120 = CARTESIAN_POINT ( 'NONE',  ( 3.923287301289999807, 1424.011886354829812, 184.0527492022980027 ) ) ;
#13121 = CARTESIAN_POINT ( 'NONE',  ( 21.66438254905593652, 1525.042337199239455, 233.5340853539618138 ) ) ;
#13122 = ORIENTED_EDGE ( 'NONE', *, *, #90559, .F. ) ;
#13123 = ORIENTED_EDGE ( 'NONE', *, *, #42629, .F. ) ;
#13124 = CARTESIAN_POINT ( 'NONE',  ( -18.50511553393410225, 1458.242655195800126, 227.6372299999850100 ) ) ;
#13125 = CARTESIAN_POINT ( 'NONE',  ( -15.56902241549999921, 1459.426448572030040, 230.4822614389979947 ) ) ;
#13126 = CARTESIAN_POINT ( 'NONE',  ( 3.663607833879999998, 1422.147183830330050, 212.8701394151179898 ) ) ;
#13127 = CARTESIAN_POINT ( 'NONE',  ( 12.51099981750000012, 1416.825784017130218, 196.0986189373979869 ) ) ;
#13128 = CARTESIAN_POINT ( 'NONE',  ( -4.032397940005000514, 1516.981965530290154, 214.9074288837770155 ) ) ;
#13129 = CARTESIAN_POINT ( 'NONE',  ( -14.31913387383960057, 1380.323794892000024, 209.9058665205810144 ) ) ;
#13130 = ORIENTED_EDGE ( 'NONE', *, *, #32223, .F. ) ;
#13131 = CARTESIAN_POINT ( 'NONE',  ( -18.87812302109619722, 1508.542151561040100, 209.8906029150280119 ) ) ;
#13132 = CARTESIAN_POINT ( 'NONE',  ( -2.970203372320949775, 1509.150402853229934, 179.1115872997399947 ) ) ;
#13133 = CARTESIAN_POINT ( 'NONE',  ( -52.67346242910000598, 1377.510081756269983, 241.2642412513589818 ) ) ;
#13134 = CARTESIAN_POINT ( 'NONE',  ( 5.314269450500000325, 1416.216252248530054, 226.4136833372980107 ) ) ;
#13135 = CARTESIAN_POINT ( 'NONE',  ( -3.265407155974999753, 1516.754149861460064, 204.5121726906670006 ) ) ;
#13136 = ORIENTED_EDGE ( 'NONE', *, *, #95366, .T. ) ;
#13137 = CARTESIAN_POINT ( 'NONE',  ( -20.67635594879999772, 1509.397142808630178, 229.5476599413979670 ) ) ;
#13138 = CARTESIAN_POINT ( 'NONE',  ( -34.37676906152069023, 1423.369835011513487, 269.5228724793240076 ) ) ;
#13139 = CARTESIAN_POINT ( 'NONE',  ( -0.7965761836729999823, 1409.108857835930166, 232.5344281013979924 ) ) ;
#13141 = ORIENTED_EDGE ( 'NONE', *, *, #41774, .F. ) ;
#13140 = CARTESIAN_POINT ( 'NONE',  ( -30.98807061075481428, 1524.600389084707103, 196.4398012796251010 ) ) ;
#13142 = CARTESIAN_POINT ( 'NONE',  ( 2.500000000000000000, 1419.365944793089966, 145.1180007323769985 ) ) ;
#13143 = CARTESIAN_POINT ( 'NONE',  ( -29.89626096159269864, 1440.913060386809775, 238.0180708521619977 ) ) ;
#13144 = CARTESIAN_POINT ( 'NONE',  ( -76.21403627649999635, 1383.779720587099746, 301.0850818666589817 ) ) ;
#13146 = EDGE_CURVE ( 'NONE', #81968, #33889, #64269, .T. ) ;
#13145 = CARTESIAN_POINT ( 'NONE',  ( -14.12816946494867132, 1415.677402202033818, 214.2877445135121661 ) ) ;
#13147 = CARTESIAN_POINT ( 'NONE',  ( 35.87497415728719830, 1421.176152893739982, 270.2893687456389671 ) ) ;
#13148 = CARTESIAN_POINT ( 'NONE',  ( 2.298048923505000118, 1516.764084769670262, 212.5672535042169784 ) ) ;
#13149 = CARTESIAN_POINT ( 'NONE',  ( -50.64061620630000249, 1379.717051619300037, 241.3114574392589873 ) ) ;
#13150 = CARTESIAN_POINT ( 'NONE',  ( 22.75767681520000352, 1409.716280410829995, 208.6970310087830001 ) ) ;
#13151 = CARTESIAN_POINT ( 'NONE',  ( 28.44964981546457850, 1526.382868172864164, 198.3640452512597108 ) ) ;
#13152 = CARTESIAN_POINT ( 'NONE',  ( -30.60461244942465342, 1523.621879633029039, 221.8232741897822677 ) ) ;
#13153 = CARTESIAN_POINT ( 'NONE',  ( -7.719573677055920236, 1516.936920898230028, 209.1135880942899803 ) ) ;
#13154 = CARTESIAN_POINT ( 'NONE',  ( -2.476170635034999901, 1516.819260244609950, 210.8389306816469855 ) ) ;
#13155 = CARTESIAN_POINT ( 'NONE',  ( -106.9828373484442494, 1391.808999926056458, 300.6260578302935187 ) ) ;
#13156 = CARTESIAN_POINT ( 'NONE',  ( -2.333469697930000031, 1420.450119961529936, 233.1581355964979707 ) ) ;
#13157 = DIRECTION ( 'NONE',  ( -0.9455185755993178454, 0.000000000000000000, 0.3255681544571537578 ) ) ;
#13158 = ORIENTED_EDGE ( 'NONE', *, *, #46603, .F. ) ;
#13159 = CARTESIAN_POINT ( 'NONE',  ( -23.62280757684879973, 1385.261635569479949, 222.7744051212729914 ) ) ;
#13160 = ADVANCED_FACE ( 'NONE', ( #95091 ), #85562, .T. ) ;
#13161 = CARTESIAN_POINT ( 'NONE',  ( 18.89905520810000183, 1416.828042640230024, 210.6687957187479867 ) ) ;
#13162 = CARTESIAN_POINT ( 'NONE',  ( 0.6621667027629999369, 1417.277712856329799, 235.8679543975979982 ) ) ;
#13163 = CARTESIAN_POINT ( 'NONE',  ( -21.45144533046939728, 1509.599841436300039, 228.9220801472459925 ) ) ;
#13164 = DIRECTION ( 'NONE',  ( 0.7087494536659948441, -1.509903313468208275E-11, 0.7054602837354869704 ) ) ;
#13165 = CARTESIAN_POINT ( 'NONE',  ( 10.54588268310000032, 1424.218227896809822, 206.2742958475490127 ) ) ;
#13166 = DIRECTION ( 'NONE',  ( -0.001259577792888569910, -0.9990026034370939056, 0.04463419977654350251 ) ) ;
#13167 = CIRCLE ( 'NONE', #54476, 1.000000000000000888 ) ;
#13169 = CARTESIAN_POINT ( 'NONE',  ( 18.24633262864339756, 1416.842625005220043, 209.2839319684169936 ) ) ;
#13168 = CARTESIAN_POINT ( 'NONE',  ( 2.486474742745000022, 1516.560253536979872, 216.0557253731069807 ) ) ;
#13170 = DIRECTION ( 'NONE',  ( 0.03489949670246857150, -0.9993908270190969834, 0.000000000000000000 ) ) ;
#13171 = CARTESIAN_POINT ( 'NONE',  ( 10.77874527468759958, 1470.254009331350062, 207.3979366881200121 ) ) ;
#13172 = ORIENTED_EDGE ( 'NONE', *, *, #15183, .T. ) ;
#13173 = CARTESIAN_POINT ( 'NONE',  ( 2.872208710164999790, 1517.145312756229941, 201.7840522196070197 ) ) ;
#13174 = CARTESIAN_POINT ( 'NONE',  ( -15.47073874116500036, 1511.939906524110256, 221.6147769341669971 ) ) ;
#13175 = ORIENTED_EDGE ( 'NONE', *, *, #261, .T. ) ;
#13176 = CARTESIAN_POINT ( 'NONE',  ( 9.538745118365339337, 1491.433376268790198, 189.9872206277390205 ) ) ;
#13177 = AXIS2_PLACEMENT_3D ( 'NONE', #10247, #18627, #55035 ) ;
#13178 = ADVANCED_FACE ( 'NONE', ( #110225 ), #94621, .F. ) ;
#13179 = DIRECTION ( 'NONE',  ( -9.714451465470110893E-14, 0.000000000000000000, 1.000000000000000000 ) ) ;
#13180 = CARTESIAN_POINT ( 'NONE',  ( 10.95536116137719951, 1461.143322918870126, 209.2158675909050203 ) ) ;
#13181 = CARTESIAN_POINT ( 'NONE',  ( 9.302468707345267873, 1425.246985399160394, 195.5946313398209213 ) ) ;
#13182 = CARTESIAN_POINT ( 'NONE',  ( 2.545036209910000125, 1441.771739723390056, 218.3207620803289899 ) ) ;
#13183 = CARTESIAN_POINT ( 'NONE',  ( -27.95267126734610130, 1509.877447535139936, 200.9175030071420167 ) ) ;
#13184 = CARTESIAN_POINT ( 'NONE',  ( -2.500000000000000000, 1448.191388957439813, 168.9995349906980096 ) ) ;
#13186 = ADVANCED_FACE ( 'NONE', ( #90393 ), #4745, .F. ) ;
#13185 = CARTESIAN_POINT ( 'NONE',  ( -18.96805899230000136, 1425.896737524130003, 225.7257654465979897 ) ) ;
#13187 = CARTESIAN_POINT ( 'NONE',  ( -5.319029970947924291, 1474.880592167660325, 269.6432403010445569 ) ) ;
#13188 = CARTESIAN_POINT ( 'NONE',  ( -105.3802333100000084, 1391.003270672820008, 303.1242145234589884 ) ) ;
#13189 = CARTESIAN_POINT ( 'NONE',  ( 16.49310356919999876, 1438.571641227850023, 190.6611314653979719 ) ) ;
#13191 = CARTESIAN_POINT ( 'NONE',  ( 28.82461957139999953, 1509.587741799730111, 209.3236985425249941 ) ) ;
#13190 = CARTESIAN_POINT ( 'NONE',  ( 20.53760542139758627, 1525.821544997590763, 184.7213720461153912 ) ) ;
#13192 = CYLINDRICAL_SURFACE ( 'NONE', #33121, 4.000000000000002665 ) ;
#13193 = ORIENTED_EDGE ( 'NONE', *, *, #32333, .T. ) ;
#13194 = CONICAL_SURFACE ( 'NONE', #27528, 6.911399307709998219, 0.04363323129990067523 ) ;
#13195 = CARTESIAN_POINT ( 'NONE',  ( -1.804213505890000180, 1410.351307731129964, 186.0507930254979954 ) ) ;
#13196 = CARTESIAN_POINT ( 'NONE',  ( -8.839654036029999773, 1508.551704422490047, 218.8221981809089982 ) ) ;
#13197 = DIRECTION ( 'NONE',  ( -1.000000000000000000, 0.000000000000000000, 0.000000000000000000 ) ) ;
#13198 = ADVANCED_FACE ( 'NONE', ( #36282 ), #55310, .T. ) ;
#13199 = CARTESIAN_POINT ( 'NONE',  ( 11.36218398372849947, 1470.732519598219824, 208.3241800981469964 ) ) ;
#13200 = CARTESIAN_POINT ( 'NONE',  ( -0.9746356023110001043, 1408.913060387329779, 227.8345159065979715 ) ) ;
#13201 = CARTESIAN_POINT ( 'NONE',  ( -18.66848659289999901, 1509.564978303230191, 231.0930269267980179 ) ) ;
#13202 = CARTESIAN_POINT ( 'NONE',  ( -2.500000000000000000, 1425.944554418600092, 184.4763172118897785 ) ) ;
#13203 = CARTESIAN_POINT ( 'NONE',  ( -13.38590766640819929, 1443.378323276218453, 187.0149398295905883 ) ) ;
#13204 = CARTESIAN_POINT ( 'NONE',  ( -24.74784509953980205, 1438.337673821209819, 210.4711784212679788 ) ) ;
#13205 = CARTESIAN_POINT ( 'NONE',  ( -4.802241272635000335, 1508.551704408389924, 213.5515886218640276 ) ) ;
#13206 = ADVANCED_BREP_SHAPE_REPRESENTATION ( '', ( #8479, #21632 ), #95028 ) ;
#13207 = ADVANCED_FACE ( 'NONE', ( #19472 ), #82226, .F. ) ;
#13208 = CARTESIAN_POINT ( 'NONE',  ( 9.992011831555620560, 1491.422447192649770, 188.4943338504039900 ) ) ;
#13209 = CARTESIAN_POINT ( 'NONE',  ( -14.65515196210479942, 1415.677402204470127, 206.0377850102939874 ) ) ;
#13210 = CARTESIAN_POINT ( 'NONE',  ( -9.652435728993630448, 1460.634894123000095, 208.5891384216040194 ) ) ;
#13211 = CARTESIAN_POINT ( 'NONE',  ( 4.760952894889999065, 1429.902475422190037, 216.8416751273590251 ) ) ;
#13213 = ORIENTED_EDGE ( 'NONE', *, *, #89073, .T. ) ;
#13212 = CARTESIAN_POINT ( 'NONE',  ( 5.909797370239999736, 1492.458403186890109, 214.9549538718289909 ) ) ;
#13214 = CARTESIAN_POINT ( 'NONE',  ( -90.27695662370000207, 1381.024254781289983, 306.9587642179589579 ) ) ;
#13215 = CARTESIAN_POINT ( 'NONE',  ( 12.29919902959760059, 1512.135905030570029, 223.9492063288249994 ) ) ;
#13216 = ORIENTED_EDGE ( 'NONE', *, *, #66097, .T. ) ;
#13217 = ORIENTED_EDGE ( 'NONE', *, *, #58216, .F. ) ;
#13218 = CARTESIAN_POINT ( 'NONE',  ( 18.20034151899999841, 1415.948532224930204, 209.5286862425880088 ) ) ;
#13219 = CARTESIAN_POINT ( 'NONE',  ( -109.7182334529999963, 1384.930883209879994, 297.0861787735589701 ) ) ;
#13220 = CARTESIAN_POINT ( 'NONE',  ( -7.989567385690000023, 1384.306347471770096, 199.5291465469090042 ) ) ;
#13222 = CARTESIAN_POINT ( 'NONE',  ( -29.66529950549999839, 1450.991311267029914, 244.2516413496979908 ) ) ;
#13221 = CARTESIAN_POINT ( 'NONE',  ( 16.03281798909471334, 1412.714820832511350, 269.3691768658688375 ) ) ;
#13223 = CARTESIAN_POINT ( 'NONE',  ( -20.47206495659999703, 1503.720923633429948, 190.5096218837979904 ) ) ;
#13224 = EDGE_CURVE ( 'NONE', #84614, #80633, #51701, .T. ) ;
#13225 = CARTESIAN_POINT ( 'NONE',  ( -109.2578989990000053, 1384.875540820709830, 297.1358323108589730 ) ) ;
#13226 = CARTESIAN_POINT ( 'NONE',  ( -12.28855869350000063, 1378.253616442990051, 210.0769077263690008 ) ) ;
#13227 = CARTESIAN_POINT ( 'NONE',  ( 11.68729876646599841, 1426.728740079569889, 140.6125123695689751 ) ) ;
#13228 = CARTESIAN_POINT ( 'NONE',  ( -7.861206937845000020, 1512.631076693560090, 196.3108915640669920 ) ) ;
#13229 = CARTESIAN_POINT ( 'NONE',  ( -25.98834112620000170, 1441.634093611399976, 138.4860864867980297 ) ) ;
#13231 = EDGE_CURVE ( 'NONE', #100346, #21912, #23053, .T. ) ;
#13230 = CARTESIAN_POINT ( 'NONE',  ( -24.39234959440000239, 1440.942615255600003, 211.3352088233380073 ) ) ;
#13232 = CARTESIAN_POINT ( 'NONE',  ( 32.85805783624308418, 1523.678648413191695, 217.1983043299902931 ) ) ;
#13233 = CARTESIAN_POINT ( 'NONE',  ( -9.486023288045011270, 1479.268917112100098, 215.9504765402980127 ) ) ;
#13234 = CARTESIAN_POINT ( 'NONE',  ( -2.166229343104828509, 1362.494928687810898, 209.6218459617148824 ) ) ;
#13235 = CARTESIAN_POINT ( 'NONE',  ( 31.50799703744284130, 1526.382868172863937, 201.8203724569130202 ) ) ;
#13237 = ORIENTED_EDGE ( 'NONE', *, *, #1601, .F. ) ;
#13236 = CARTESIAN_POINT ( 'NONE',  ( 1.330142072575580153E-08, 1408.768101624430074, 261.3699198151659857 ) ) ;
#13238 = EDGE_LOOP ( 'NONE', ( #70890, #32784, #29631, #97582 ) ) ;
#13239 = CARTESIAN_POINT ( 'NONE',  ( -11.86071752599299955, 1431.960136582280029, 149.9694963188620136 ) ) ;
#13240 = CARTESIAN_POINT ( 'NONE',  ( -11.72566050890000078, 1483.562230513489794, 228.3064628327989851 ) ) ;
#13241 = CARTESIAN_POINT ( 'NONE',  ( -25.90444642199999947, 1468.044424510629824, 270.1671806390979782 ) ) ;
#13242 = CARTESIAN_POINT ( 'NONE',  ( -1.556886619979999997, 1415.063410501429871, 226.7642036972980009 ) ) ;
#13243 = CYLINDRICAL_SURFACE ( 'NONE', #39698, 2.000000000000003553 ) ;
#13244 = CARTESIAN_POINT ( 'NONE',  ( 35.25104840220150493, 1451.457745839210020, 135.5593480995689788 ) ) ;
#13245 = CARTESIAN_POINT ( 'NONE',  ( 0.2091819028966719896, 1452.039107084460056, 183.0587606973180073 ) ) ;
#13246 = CARTESIAN_POINT ( 'NONE',  ( 4.642066325181019693, 1484.267353360819925, 220.0190218960080131 ) ) ;
#13247 = CARTESIAN_POINT ( 'NONE',  ( 2.500000005229999989, 1448.233542442588032, 182.8968085845170037 ) ) ;
#13248 = CARTESIAN_POINT ( 'NONE',  ( -3.957094129160000140, 1456.622155725689936, 217.7529547663189931 ) ) ;
#13249 = CARTESIAN_POINT ( 'NONE',  ( 7.877099145829919991, 1362.118768394185963, 210.6218459616991936 ) ) ;
#13250 = CARTESIAN_POINT ( 'NONE',  ( -27.47176941845090070, 1412.619294620689971, 267.2173682766330103 ) ) ;
#13251 = ORIENTED_EDGE ( 'NONE', *, *, #110557, .F. ) ;
#13252 = CARTESIAN_POINT ( 'NONE',  ( -3.527569048119670203, 1486.518325592330029, 181.8541486797999767 ) ) ;
#13253 = AXIS2_PLACEMENT_3D ( 'NONE', #98689, #47199, #83529 ) ;
#13254 = VERTEX_POINT ( 'NONE', #10534 ) ;
#13255 = ORIENTED_EDGE ( 'NONE', *, *, #18621, .T. ) ;
#13256 = CARTESIAN_POINT ( 'NONE',  ( 4.045182479925000685, 1517.057265928030120, 210.8256255754569963 ) ) ;
#13257 = CARTESIAN_POINT ( 'NONE',  ( -8.949286084602180225, 1447.532838897989905, 212.1309938496879965 ) ) ;
#13259 = CARTESIAN_POINT ( 'NONE',  ( -3.307305241536517393, 1441.238720758000682, 170.5343657646909321 ) ) ;
#13258 = CARTESIAN_POINT ( 'NONE',  ( 2.880592928985000079, 1516.859514182039902, 211.9868180862470126 ) ) ;
#13260 = CARTESIAN_POINT ( 'NONE',  ( -17.30344447809999764, 1440.441197234099945, 190.6958610362979982 ) ) ;
#13261 = AXIS2_PLACEMENT_3D ( 'NONE', #77834, #25748, #1143 ) ;
#13262 = CARTESIAN_POINT ( 'NONE',  ( -2.166650729859409097, 1450.000234473310456, 182.9036927443551690 ) ) ;
#13263 = B_SPLINE_SURFACE_WITH_KNOTS ( 'NONE', 5, 1, ( 
 ( #91994, #49462 ),
 ( #108246, #84141 ),
 ( #108801, #93092 ),
 ( #15271, #16363 ),
 ( #110453, #50562 ),
 ( #82505, #42153 ) ),
 .UNSPECIFIED., .F., .F., .F.,
 ( 6, 6 ),
 ( 2, 2 ),
 ( 0.000000000000000000, 3.454439543779999955 ),
 ( 0.000000000000000000, 14.00000000000000000 ),
 .UNSPECIFIED. ) ;
#13264 = ORIENTED_EDGE ( 'NONE', *, *, #91628, .F. ) ;
#13265 = CARTESIAN_POINT ( 'NONE',  ( 1.600048698852036821, 1402.754281879943164, 137.0999999980979851 ) ) ;
#13266 = B_SPLINE_CURVE_WITH_KNOTS ( 'NONE', 5,
 ( #105299, #20175, #95792, #77895, #52706, #86841 ),
 .UNSPECIFIED., .F., .F.,
 ( 6, 6 ),
 ( 0.000000000000000000, 1.000000000000000000 ),
 .UNSPECIFIED. ) ;
#13267 = CARTESIAN_POINT ( 'NONE',  ( 6.941100277744999936, 1516.858069504249897, 202.1782432786469883 ) ) ;
#13268 = CARTESIAN_POINT ( 'NONE',  ( 10.51055417280000093, 1471.685891545489994, 212.2894659362390257 ) ) ;
#13269 = CARTESIAN_POINT ( 'NONE',  ( -17.14091472579860209, 1384.527013523339974, 201.0257602182319943 ) ) ;
#13270 = CARTESIAN_POINT ( 'NONE',  ( -42.11756425049719610, 1430.851161910550218, 270.3372090159310233 ) ) ;
#13271 = CARTESIAN_POINT ( 'NONE',  ( 2.854350849340439922, 1416.619839790820151, 231.9963541232479827 ) ) ;
#13272 = CARTESIAN_POINT ( 'NONE',  ( -2.546644429710000157, 1397.067797496830053, 196.4597125348979887 ) ) ;
#13274 = VERTEX_POINT ( 'NONE', #56819 ) ;
#13273 = CARTESIAN_POINT ( 'NONE',  ( -8.909267011570118910, 1365.369432761979624, 207.6218459616988241 ) ) ;
#13275 = ORIENTED_EDGE ( 'NONE', *, *, #499, .F. ) ;
#13276 = CARTESIAN_POINT ( 'NONE',  ( 45.63713076155215731, 1440.913099924324115, 268.9747509450593839 ) ) ;
#13277 = CARTESIAN_POINT ( 'NONE',  ( -2.080140501524690322, 1467.944488986910301, 220.0539240431270116 ) ) ;
#13278 = ADVANCED_FACE ( 'NONE', ( #106651 ), #82881, .T. ) ;
#13279 = CARTESIAN_POINT ( 'NONE',  ( 2.724500461545519059, 1367.224846223802842, 209.6218459617149108 ) ) ;
#13280 = DIRECTION ( 'NONE',  ( -1.755985294532469921E-16, 1.000000000000000000, -1.338183447452831989E-16 ) ) ;
#13281 = CARTESIAN_POINT ( 'NONE',  ( -7.326072182274999456, 1516.714320817460020, 209.8751461055349807 ) ) ;
#13282 = CARTESIAN_POINT ( 'NONE',  ( -68.77190080519999071, 1379.747925807450201, 280.3125203366930123 ) ) ;
#13283 = CARTESIAN_POINT ( 'NONE',  ( -20.19344737140000134, 1435.770039937179945, 222.9975873334980179 ) ) ;
#13284 = CARTESIAN_POINT ( 'NONE',  ( 5.178005602700659793, 1441.912561073429970, 216.3756019184010029 ) ) ;
#13285 = CARTESIAN_POINT ( 'NONE',  ( 12.77587743780000018, 1416.568813547830132, 222.7009457741980327 ) ) ;
#13286 = CARTESIAN_POINT ( 'NONE',  ( 7.803201805185000062, 1511.730395268069969, 206.0441542149769987 ) ) ;
#13287 = CARTESIAN_POINT ( 'NONE',  ( 0.7351097711180020200, 1516.977504706749869, 206.6301902066870184 ) ) ;
#13288 = VERTEX_POINT ( 'NONE', #46585 ) ;
#13289 = CARTESIAN_POINT ( 'NONE',  ( -36.37832868396120034, 1435.767865609909904, 135.3761632872109999 ) ) ;
#13290 = CARTESIAN_POINT ( 'NONE',  ( -22.20861559396504603, 1452.332390273548299, 220.3331572959684195 ) ) ;
#13291 = VERTEX_POINT ( 'NONE', #97517 ) ;
#13292 = CARTESIAN_POINT ( 'NONE',  ( 2.786005956417805685, 1457.636688197868125, 228.7054548384536190 ) ) ;
#13293 = EDGE_CURVE ( 'NONE', #38397, #3072, #38844, .T. ) ;
#13294 = CARTESIAN_POINT ( 'NONE',  ( 14.30561690719999923, 1416.274718424630009, 196.7258643987979951 ) ) ;
#13295 = DIRECTION ( 'NONE',  ( 0.004026485253168931785, 0.9999913661844075374, -0.001027118858027144602 ) ) ;
#13296 = CARTESIAN_POINT ( 'NONE',  ( 20.92457307240000119, 1409.643762580330076, 205.0061534547180031 ) ) ;
#13297 = DIRECTION ( 'NONE',  ( 0.1070030146457354309, 0.000000000000000000, 0.9942586961433751425 ) ) ;
#13298 = CARTESIAN_POINT ( 'NONE',  ( 10.56851139279999963, 1489.654861728290143, 206.0672006338689926 ) ) ;
#13299 = CARTESIAN_POINT ( 'NONE',  ( -3.494989020446679806, 1476.662911819639930, 199.3633622754599912 ) ) ;
#13300 = CARTESIAN_POINT ( 'NONE',  ( 24.58073941009117291, 1443.411714615211622, 213.1237255199102378 ) ) ;
#13301 = FACE_OUTER_BOUND ( 'NONE', #46050, .T. ) ;
#13302 = CARTESIAN_POINT ( 'NONE',  ( 4.620008207075000151, 1516.777260590120022, 214.8964555921769772 ) ) ;
#13303 = ORIENTED_EDGE ( 'NONE', *, *, #92101, .T. ) ;
#13304 = CARTESIAN_POINT ( 'NONE',  ( 7.713820733194500789, 1516.717189502959855, 208.3559500364069947 ) ) ;
#13305 = CARTESIAN_POINT ( 'NONE',  ( 4.613723315850000479E-06, 1474.175172091230024, 270.1377426632980132 ) ) ;
#13306 = CARTESIAN_POINT ( 'NONE',  ( -3.263114576272079827E-31, 1414.677402202029953, 209.1218459616989946 ) ) ;
#13307 = CARTESIAN_POINT ( 'NONE',  ( -16.10161876792589908, 1508.453223452970178, 214.3744947141610169 ) ) ;
#13308 = CARTESIAN_POINT ( 'NONE',  ( -37.65379800284389944, 1449.104226875719860, 136.3438977234109757 ) ) ;
#13309 = CARTESIAN_POINT ( 'NONE',  ( 19.37040130519999792, 1457.792564341990101, 211.0127811088189844 ) ) ;
#13310 = LINE ( 'NONE', #12789, #28175 ) ;
#13311 = CARTESIAN_POINT ( 'NONE',  ( 18.01996314195137927, 1424.295345311109713, 225.2602986464550838 ) ) ;
#13313 = ADVANCED_FACE ( 'NONE', ( #34439 ), #35611, .F. ) ;
#13312 = CARTESIAN_POINT ( 'NONE',  ( -107.4477384240240099, 1379.886883745280102, 299.0757736425410371 ) ) ;
#13314 = CARTESIAN_POINT ( 'NONE',  ( -3.602921956033400071E-07, 1407.180382923570050, 222.1388580509179747 ) ) ;
#13315 = CARTESIAN_POINT ( 'NONE',  ( 35.88934487943939899, 1440.913060387049882, 252.6421940191889632 ) ) ;
#13316 = CARTESIAN_POINT ( 'NONE',  ( -10.32197686275740089, 1470.787254133000033, 211.3220767278949950 ) ) ;
#13317 = CARTESIAN_POINT ( 'NONE',  ( 10.99775799211320049, 1499.987872926449882, 204.6284785093779988 ) ) ;
#13318 = ORIENTED_EDGE ( 'NONE', *, *, #60388, .F. ) ;
#13319 = EDGE_CURVE ( 'NONE', #110093, #53118, #24297, .T. ) ;
#13320 = ORIENTED_EDGE ( 'NONE', *, *, #56827, .F. ) ;
#13321 = VECTOR ( 'NONE', #20707, 1000.000000000000114 ) ;
#13322 = CARTESIAN_POINT ( 'NONE',  ( -7.012921583638330070, 1508.551704408389924, 203.6084103760139783 ) ) ;
#13323 = EDGE_CURVE ( 'NONE', #108385, #69912, #9621, .T. ) ;
#13324 = PLANE ( 'NONE',  #65795 ) ;
#13325 = CARTESIAN_POINT ( 'NONE',  ( -4.227553501430000082, 1441.218335795189887, 201.3833937247689789 ) ) ;
#13326 = DIRECTION ( 'NONE',  ( 0.9900965937346507539, -0.1403878024439509931, 3.790652827686679061E-16 ) ) ;
#13327 = VECTOR ( 'NONE', #96941, 1000.000000000000000 ) ;
#13328 = VECTOR ( 'NONE', #38434, 1000.000000000000000 ) ;
#13329 = ADVANCED_FACE ( 'NONE', ( #88578 ), #43404, .T. ) ;
#13330 = CARTESIAN_POINT ( 'NONE',  ( -11.00005007279999880, 1492.085135258889977, 210.0463809226660032 ) ) ;
#13331 = CARTESIAN_POINT ( 'NONE',  ( -1.657661096414910107, 1508.551704408389924, 220.0807554094629666 ) ) ;
#13332 = CARTESIAN_POINT ( 'NONE',  ( -49.65267816373729914, 1383.812483723600053, 260.6283176093329530 ) ) ;
#13333 = CARTESIAN_POINT ( 'NONE',  ( -4.059671833654999951, 1511.437978678640093, 200.9086510787369946 ) ) ;
#13334 = FACE_OUTER_BOUND ( 'NONE', #70550, .T. ) ;
#13335 = CARTESIAN_POINT ( 'NONE',  ( -11.81627054680200040, 1502.033420305900108, 208.8645209164289724 ) ) ;
#13336 = CARTESIAN_POINT ( 'NONE',  ( 2.318246505679999903, 1464.667746032229843, 236.3197918910979922 ) ) ;
#13338 = ORIENTED_EDGE ( 'NONE', *, *, #12532, .T. ) ;
#13337 = CARTESIAN_POINT ( 'NONE',  ( -0.8521672233359980364, 1489.820358975390036, 188.1651792795989877 ) ) ;
#13339 = CARTESIAN_POINT ( 'NONE',  ( -0.5354439702209998764, 1451.096935658430084, 182.2556569121979919 ) ) ;
#13340 = CARTESIAN_POINT ( 'NONE',  ( -23.75690532229999619, 1380.904381710259941, 220.2087197048589928 ) ) ;
#13341 = CARTESIAN_POINT ( 'NONE',  ( 4.391179462425729874, 1508.551704408389924, 205.0152113334139869 ) ) ;
#13343 = ORIENTED_EDGE ( 'NONE', *, *, #10614, .T. ) ;
#13342 = CARTESIAN_POINT ( 'NONE',  ( -17.65703761238349756, 1415.429375168339902, 208.7951508728979775 ) ) ;
#13344 = CARTESIAN_POINT ( 'NONE',  ( -16.53114207763760035, 1465.611540855740031, 220.7423250375829866 ) ) ;
#13345 = VERTEX_POINT ( 'NONE', #54986 ) ;
#13346 = B_SPLINE_CURVE_WITH_KNOTS ( 'NONE', 5,
 ( #40738, #66525, #92239, #49709, #83839, #110693, #33986, #7140, #102286, #25567, #75469, #109603 ),
 .UNSPECIFIED., .F., .F.,
 ( 6, 3, 3, 6 ),
 ( 0.000000000000000000, 0.3830643373806639218, 0.7943583785163387256, 1.000000000000000000 ),
 .UNSPECIFIED. ) ;
#13347 = CARTESIAN_POINT ( 'NONE',  ( -12.74756332158530014, 1389.858839731569788, 214.0101211577780020 ) ) ;
#13348 = CARTESIAN_POINT ( 'NONE',  ( 36.10037600688230697, 1437.471261748140023, 136.5386461258349868 ) ) ;
#13349 = DIRECTION ( 'NONE',  ( -1.000000000000000000, 0.000000000000000000, 0.000000000000000000 ) ) ;
#13350 = CARTESIAN_POINT ( 'NONE',  ( 8.847239431406803689, 1505.230286297941348, 216.6946609004857862 ) ) ;
#13351 = CARTESIAN_POINT ( 'NONE',  ( 3.829620113920000346, 1515.551704408389924, 211.4519800804890224 ) ) ;
#13352 = CARTESIAN_POINT ( 'NONE',  ( 19.21355886149643055, 1509.590266407224817, 186.7400054175685113 ) ) ;
#13353 = FACE_OUTER_BOUND ( 'NONE', #106258, .T. ) ;
#13354 = B_SPLINE_CURVE_WITH_KNOTS ( 'NONE', 5,
 ( #47127, #90200, #57196, #107016, #29756, #90763, #22991, #5673, #37616 ),
 .UNSPECIFIED., .F., .F.,
 ( 6, 3, 6 ),
 ( -3.000000000000000000, -1.500000000000000222, -5.116429209195416661E-07 ),
 .UNSPECIFIED. ) ;
#13355 = CARTESIAN_POINT ( 'NONE',  ( 18.80463711554499895, 1425.800691016006112, 225.6053601209239901 ) ) ;
#13356 = CARTESIAN_POINT ( 'NONE',  ( 13.25104486714040775, 1460.521307829560101, 224.0262041468786265 ) ) ;
#13357 = ADVANCED_FACE ( 'NONE', ( #46034 ), #8667, .F. ) ;
#13358 = CARTESIAN_POINT ( 'NONE',  ( -19.14657372330000129, 1478.162773027329877, 190.0467893125980083 ) ) ;
#13359 = CARTESIAN_POINT ( 'NONE',  ( 11.30106291239999905, 1432.291791669059876, 151.5220416249979962 ) ) ;
#13360 = CARTESIAN_POINT ( 'NONE',  ( -2.833916579333589869, 1449.814275768419975, 184.3649903733470126 ) ) ;
#13361 = ORIENTED_EDGE ( 'NONE', *, *, #976, .F. ) ;
#13362 = VERTEX_POINT ( 'NONE', #105933 ) ;
#13363 = VECTOR ( 'NONE', #51012, 1000.000000000000000 ) ;
#13364 = ADVANCED_FACE ( 'NONE', ( #29212 ), #68720, .T. ) ;
#13365 = CARTESIAN_POINT ( 'NONE',  ( 17.43739734485841808, 1526.178928173327449, 237.5162751070522518 ) ) ;
#13366 = CARTESIAN_POINT ( 'NONE',  ( -18.71884693102710173, 1442.006986966149952, 209.9877030880639950 ) ) ;
#13367 = CARTESIAN_POINT ( 'NONE',  ( -11.68969520689999797, 1434.472878431520030, 151.2717061033980031 ) ) ;
#13368 = CARTESIAN_POINT ( 'NONE',  ( 12.89505231660000106, 1420.989630775359956, 203.4267439564690108 ) ) ;
#13369 = CARTESIAN_POINT ( 'NONE',  ( -20.52883463880759862, 1505.559739956360090, 190.4562007501970129 ) ) ;
#13370 = CARTESIAN_POINT ( 'NONE',  ( -24.71655169530576401, 1435.786948140999357, 137.7886807324425149 ) ) ;
#13371 = CARTESIAN_POINT ( 'NONE',  ( -109.9979373700000025, 1385.333188379740022, 311.4502719372590036 ) ) ;
#13372 = CIRCLE ( 'NONE', #75981, 5.499916801759985319 ) ;
#13373 = CARTESIAN_POINT ( 'NONE',  ( -7.447811320689449843, 1511.198033794599951, 215.3870677586729983 ) ) ;
#13374 = CARTESIAN_POINT ( 'NONE',  ( -9.977700672470000143, 1365.292605733890014, 207.6218459616989946 ) ) ;
#13375 = CARTESIAN_POINT ( 'NONE',  ( -45.63478668459259779, 1440.473321573280145, 268.9749136988990017 ) ) ;
#13376 = CARTESIAN_POINT ( 'NONE',  ( 14.01395624050939936, 1452.538953007629743, 222.8951477747749834 ) ) ;
#13377 = CARTESIAN_POINT ( 'NONE',  ( -2.300729664794999962, 1516.923170579120097, 207.4211391557370234 ) ) ;
#13378 = CARTESIAN_POINT ( 'NONE',  ( -8.822183969887010591, 1447.794223493370055, 211.9042362736150267 ) ) ;
#13379 = CARTESIAN_POINT ( 'NONE',  ( 3.872712109488329890, 1407.067885255820102, 221.6343841272010025 ) ) ;
#13380 = CARTESIAN_POINT ( 'NONE',  ( -13.66429424859150110, 1434.998729100779883, 149.0303311387329757 ) ) ;
#13381 = CARTESIAN_POINT ( 'NONE',  ( -7.546363868560000299, 1385.222286201930046, 219.0767476026689735 ) ) ;
#13382 = B_SPLINE_SURFACE_WITH_KNOTS ( 'NONE', 5, 4, ( 
 ( #84587, #58304, #92426, #15701, #49904 ),
 ( #58854, #109262, #82938, #39843, #40937 ),
 ( #74006, #7878, #40384, #42047, #65613 ),
 ( #67270, #15162, #76198, #110344, #24112 ),
 ( #84039, #7337, #75660, #33617, #100296 ),
 ( #74561, #59419, #101362, #93531, #100825 ) ),
 .UNSPECIFIED., .F., .F., .F.,
 ( 6, 6 ),
 ( 5, 5 ),
 ( 0.000000000000000000, 111.1101480259999903 ),
 ( 25.81581217359999769, 39.03307591160000101 ),
 .UNSPECIFIED. ) ;
#13383 = CARTESIAN_POINT ( 'NONE',  ( 6.440382586182271218, 1425.293263514254704, 226.4189292768371047 ) ) ;
#13384 = CARTESIAN_POINT ( 'NONE',  ( 7.289056222716610023, 1425.011265941609963, 212.6780767636349765 ) ) ;
#13385 = ORIENTED_EDGE ( 'NONE', *, *, #67252, .T. ) ;
#13386 = CARTESIAN_POINT ( 'NONE',  ( 24.26836175920000116, 1418.067430823330142, 255.0044386299979919 ) ) ;
#13387 = CARTESIAN_POINT ( 'NONE',  ( -27.85639448530000095, 1508.131721226830223, 206.6638992223579976 ) ) ;
#13389 = CARTESIAN_POINT ( 'NONE',  ( -17.71298236049999986, 1410.454334518429960, 194.8352300936979873 ) ) ;
#13388 = CARTESIAN_POINT ( 'NONE',  ( -11.88865138995519999, 1491.218756537510217, 206.7026720337979953 ) ) ;
#13390 =( BOUNDED_CURVE ( )  B_SPLINE_CURVE ( 3, ( #40800, #13926, #89549, #48113 ),
 .UNSPECIFIED., .F., .F. ) 
 B_SPLINE_CURVE_WITH_KNOTS ( ( 4, 4 ),
 ( 4.801238875923769633, 5.185567269779980393 ),
 .UNSPECIFIED. ) 
 CURVE ( )  GEOMETRIC_REPRESENTATION_ITEM ( )  RATIONAL_B_SPLINE_CURVE ( ( 1.000000000000000000, 0.9877288052443483624, 0.9877288052443483624, 1.000000000000000000 ) ) 
 REPRESENTATION_ITEM ( '' )  );
#13391 = CARTESIAN_POINT ( 'NONE',  ( -8.718170062098048234, 1408.261133769854041, 270.1210666218138385 ) ) ;
#13392 = CARTESIAN_POINT ( 'NONE',  ( -29.87496801789999878, 1438.990456365560021, 238.0574310508980318 ) ) ;
#13393 = DIRECTION ( 'NONE',  ( -0.008080911954619110840, -0.2617474919842974757, -0.9651025589552190143 ) ) ;
#13394 = CARTESIAN_POINT ( 'NONE',  ( -7.916648676117490346, 1452.636604923769937, 151.3511352965829815 ) ) ;
#13395 = CARTESIAN_POINT ( 'NONE',  ( -18.89959501459999913, 1416.839692131129823, 207.5749782147480289 ) ) ;
#13396 = EDGE_LOOP ( 'NONE', ( #56907, #14508, #25513, #8047, #55753 ) ) ;
#13397 = CARTESIAN_POINT ( 'NONE',  ( 3.968827103902559550, 1522.051704408389924, 188.7040005461919918 ) ) ;
#13398 = CARTESIAN_POINT ( 'NONE',  ( 14.39977812427909853, 1514.266850649818707, 225.6063674502700565 ) ) ;
#13399 = CARTESIAN_POINT ( 'NONE',  ( -0.04627975075399999583, 1508.911444262829946, 238.5489451465980153 ) ) ;
#13400 = ORIENTED_EDGE ( 'NONE', *, *, #84946, .F. ) ;
#13401 = ORIENTED_EDGE ( 'NONE', *, *, #102475, .T. ) ;
#13402 = CARTESIAN_POINT ( 'NONE',  ( 9.181081645171898842, 1450.963532761650185, 210.1934668057190265 ) ) ;
#13403 = CARTESIAN_POINT ( 'NONE',  ( 6.345494395550000277, 1423.250787925290069, 195.0535775187989884 ) ) ;
#13404 = VERTEX_POINT ( 'NONE', #65025 ) ;
#13405 = CARTESIAN_POINT ( 'NONE',  ( 4.554954805175000843, 1508.731366866819826, 205.6342593439610198 ) ) ;
#13406 = CARTESIAN_POINT ( 'NONE',  ( -30.31940284292426924, 1523.382868172864164, 195.7503880523418616 ) ) ;
#13407 = B_SPLINE_CURVE_WITH_KNOTS ( 'NONE', 5,
 ( #103031, #53223, #21096, #87362, #47437, #81561 ),
 .UNSPECIFIED., .F., .F.,
 ( 6, 6 ),
 ( 0.000000000000000000, 1.000000000000000000 ),
 .UNSPECIFIED. ) ;
#13408 = CARTESIAN_POINT ( 'NONE',  ( -13.51912611120000030, 1489.054086407930072, 231.6518530692979994 ) ) ;
#13409 = CARTESIAN_POINT ( 'NONE',  ( 2.487921303217719871, 1508.551704408389924, 214.1089244078229967 ) ) ;
#13410 = ORIENTED_EDGE ( 'NONE', *, *, #11224, .T. ) ;
#13411 = CARTESIAN_POINT ( 'NONE',  ( 46.27887280396929981, 1441.860040026859906, 267.5894435840550045 ) ) ;
#13412 = CARTESIAN_POINT ( 'NONE',  ( -11.54244540313270129, 1414.913060387399810, 220.3473659478999878 ) ) ;
#13413 = CARTESIAN_POINT ( 'NONE',  ( -0.06054275102980000156, 1420.434684236430030, 183.3377748591979923 ) ) ;
#13414 = CARTESIAN_POINT ( 'NONE',  ( 6.937965660314999283, 1516.732530461250008, 204.1161457306970135 ) ) ;
#13415 = ORIENTED_EDGE ( 'NONE', *, *, #40017, .F. ) ;
#13416 = CARTESIAN_POINT ( 'NONE',  ( 11.55221588404359956, 1480.217597516799970, 211.4789165460060190 ) ) ;
#13417 = CARTESIAN_POINT ( 'NONE',  ( 13.45802170480480875, 1444.282616009370258, 187.8687362809869512 ) ) ;
#13418 = ORIENTED_EDGE ( 'NONE', *, *, #42680, .F. ) ;
#13419 = ORIENTED_EDGE ( 'NONE', *, *, #50033, .T. ) ;
#13420 = CARTESIAN_POINT ( 'NONE',  ( 0.7251570665222378809, 1526.278758871496620, 176.2636429491667514 ) ) ;
#13421 = CARTESIAN_POINT ( 'NONE',  ( -3.139802346294130242, 1508.551704408389924, 219.9904071531209979 ) ) ;
#13422 = CARTESIAN_POINT ( 'NONE',  ( 5.726337297911710422, 1499.318321574760148, 199.1886870359400064 ) ) ;
#13423 = CARTESIAN_POINT ( 'NONE',  ( -14.62991246550300062, 1513.722010160979835, 194.0917047335290135 ) ) ;
#13424 = CARTESIAN_POINT ( 'NONE',  ( 17.05418697632569902, 1452.317515055090098, 146.2608711844959828 ) ) ;
#13425 = CARTESIAN_POINT ( 'NONE',  ( 11.78997475979999976, 1420.248503611800061, 199.1713245500889968 ) ) ;
#13426 = CARTESIAN_POINT ( 'NONE',  ( 0.7985270487440959686, 1475.099758008560002, 220.5147217360619720 ) ) ;
#13427 = CARTESIAN_POINT ( 'NONE',  ( -108.9413858983323280, 1381.821374029668959, 297.6754583912645558 ) ) ;
#13428 = CARTESIAN_POINT ( 'NONE',  ( -10.98084453577630093, 1433.016921785290151, 151.7694248368179899 ) ) ;
#13429 = CARTESIAN_POINT ( 'NONE',  ( 0.03447861350279703141, 1409.362621839177336, 232.8245751882662660 ) ) ;
#13431 = CARTESIAN_POINT ( 'NONE',  ( -106.5049786777409935, 1391.913060387289988, 305.4200656224640511 ) ) ;
#13430 = CARTESIAN_POINT ( 'NONE',  ( 30.44069153016972251, 1525.425686270224332, 196.7701993420686506 ) ) ;
#13432 = CARTESIAN_POINT ( 'NONE',  ( 10.90038547020369997, 1425.457621502399888, 206.5065321829229958 ) ) ;
#13433 = CARTESIAN_POINT ( 'NONE',  ( -24.17892280350069711, 1508.624304443510027, 222.3905331272610226 ) ) ;
#13434 = CARTESIAN_POINT ( 'NONE',  ( 11.29523459009999975, 1425.738185348830029, 112.3426556953979940 ) ) ;
#13435 = ORIENTED_EDGE ( 'NONE', *, *, #35986, .F. ) ;
#13436 = CARTESIAN_POINT ( 'NONE',  ( 2.984513020910000147, 1427.913060387330006, 209.1218459616979999 ) ) ;
#13437 = CARTESIAN_POINT ( 'NONE',  ( -2.534203887357130203, 1421.318133204249989, 184.2270941939309807 ) ) ;
#13438 = CARTESIAN_POINT ( 'NONE',  ( -93.24395053702400560, 1384.962031755649832, 309.6487558849449897 ) ) ;
#13439 = AXIS2_PLACEMENT_3D ( 'NONE', #66230, #76804, #74614 ) ;
#13440 = CARTESIAN_POINT ( 'NONE',  ( -8.406173068439999341, 1386.862502020539978, 199.9329045535289993 ) ) ;
#13441 = CARTESIAN_POINT ( 'NONE',  ( 9.509695062716730263, 1426.375487959860038, 209.7904012934289995 ) ) ;
#13443 = ORIENTED_EDGE ( 'NONE', *, *, #3019, .T. ) ;
#13442 = CARTESIAN_POINT ( 'NONE',  ( -6.404454395499999286, 1464.203453065390022, 200.1263287045289871 ) ) ;
#13444 = CARTESIAN_POINT ( 'NONE',  ( 4.675254175260000089, 1430.199328422790131, 217.3863063698589997 ) ) ;
#13445 = CARTESIAN_POINT ( 'NONE',  ( -2.461716435160000049, 1435.943783413959864, 150.4083956814980070 ) ) ;
#13446 = CARTESIAN_POINT ( 'NONE',  ( -16.61413016530000064, 1416.994763352589871, 207.8498519981289974 ) ) ;
#13448 = EDGE_CURVE ( 'NONE', #71672, #54897, #58889, .T. ) ;
#13447 = CARTESIAN_POINT ( 'NONE',  ( -12.53380652166779896, 1445.052232296300190, 185.6742736269380032 ) ) ;
#13449 = CARTESIAN_POINT ( 'NONE',  ( 14.32022877053500132, 1513.136578080079744, 224.9650162968669918 ) ) ;
#13450 = CARTESIAN_POINT ( 'NONE',  ( 13.01538513870689862, 1416.535698381769862, 196.3451722032600060 ) ) ;
#13451 = AXIS2_PLACEMENT_3D ( 'NONE', #39023, #35043, #26069 ) ;
#13452 = CARTESIAN_POINT ( 'NONE',  ( 8.978117882695519469, 1435.738603067889699, 208.3990004362530044 ) ) ;
#13453 = CARTESIAN_POINT ( 'NONE',  ( -109.2523138997062802, 1387.517232177382994, 297.4607553404316604 ) ) ;
#13454 = CARTESIAN_POINT ( 'NONE',  ( 4.466626895270000119, 1422.096238294529940, 231.9296400908980047 ) ) ;
#13455 = CARTESIAN_POINT ( 'NONE',  ( 0.03226293719758020068, 1410.297897419189894, 233.2219341505459909 ) ) ;
#13456 = CARTESIAN_POINT ( 'NONE',  ( 3.745926128375240083, 1474.358832711759987, 219.9123296517309996 ) ) ;
#13457 = CARTESIAN_POINT ( 'NONE',  ( -18.56577482049999972, 1410.923936267830186, 223.7868423640980211 ) ) ;
#13458 = CARTESIAN_POINT ( 'NONE',  ( 31.44837959398582328, 1512.187213306747481, 197.3353852117981262 ) ) ;
#13459 = CARTESIAN_POINT ( 'NONE',  ( -1.121218465919999963, 1416.837080256330182, 228.0853546198979984 ) ) ;
#13460 = CARTESIAN_POINT ( 'NONE',  ( -4.219438644781110526, 1441.595895916910195, 183.5288106640859951 ) ) ;
#13461 = CARTESIAN_POINT ( 'NONE',  ( 24.26322120380000058, 1437.059134594650232, 214.0566016570280112 ) ) ;
#13462 = ADVANCED_FACE ( 'NONE', ( #74535 ), #108666, .F. ) ;
#13463 = CARTESIAN_POINT ( 'NONE',  ( 0.7576697579430009544, 1515.544658147190148, 204.9993528003190022 ) ) ;
#13464 = CARTESIAN_POINT ( 'NONE',  ( -0.6370436997427022519, 1522.051704408389924, 217.8527312947061603 ) ) ;
#13465 = CARTESIAN_POINT ( 'NONE',  ( -40.51263981762689781, 1439.427258870550077, 135.2566580804950149 ) ) ;
#13466 = CARTESIAN_POINT ( 'NONE',  ( -7.490735701819999370, 1414.913060387329779, 223.4518716291979956 ) ) ;
#13467 = DIRECTION ( 'NONE',  ( 0.000000000000000000, 0.000000000000000000, -1.000000000000000000 ) ) ;
#13468 = CARTESIAN_POINT ( 'NONE',  ( -6.425367583159999896, 1409.137439167629964, 223.2437179294980183 ) ) ;
#13469 = CARTESIAN_POINT ( 'NONE',  ( -15.10946924899999999, 1415.087745006229852, 201.1701658454080075 ) ) ;
#13470 = CARTESIAN_POINT ( 'NONE',  ( 13.16517659032116860, 1517.051704408389924, 194.0489770726361485 ) ) ;
#13471 = EDGE_CURVE ( 'NONE', #6947, #90388, #91004, .T. ) ;
#13472 = CARTESIAN_POINT ( 'NONE',  ( -1.210798686530613288, 1483.997144534682093, 198.5025898468677212 ) ) ;
#13473 = CARTESIAN_POINT ( 'NONE',  ( 12.06099931120000157, 1433.903617051039873, 149.0256926596979952 ) ) ;
#13474 = CARTESIAN_POINT ( 'NONE',  ( -27.26054292650000122, 1435.602462706470078, 136.1497272824979916 ) ) ;
#13475 = CARTESIAN_POINT ( 'NONE',  ( 9.098928921009999726, 1442.287229081999840, 185.1767890527980001 ) ) ;
#13476 = ORIENTED_EDGE ( 'NONE', *, *, #95878, .T. ) ;
#13477 = CARTESIAN_POINT ( 'NONE',  ( -17.03783583027061255, 1524.776010967693765, 181.0919469249481040 ) ) ;
#13478 = CARTESIAN_POINT ( 'NONE',  ( 8.001917699090000724, 1477.391948627790043, 200.4742795864889899 ) ) ;
#13479 = CARTESIAN_POINT ( 'NONE',  ( -11.93607054898440012, 1409.329877155629902, 218.1202972442949886 ) ) ;
#13480 = CARTESIAN_POINT ( 'NONE',  ( -11.12609304959999967, 1491.160356708789777, 209.7795734009459920 ) ) ;
#13481 = DIRECTION ( 'NONE',  ( 0.02616798426532259553, -0.9993150019883517698, 0.02616798426532229369 ) ) ;
#13482 = DIRECTION ( 'NONE',  ( -0.02617694830788819954, 0.9996573249755569268, 0.000000000000000000 ) ) ;
#13483 = CARTESIAN_POINT ( 'NONE',  ( 37.48449069387330468, 1421.396168078520759, 269.1919258218934488 ) ) ;
#13484 = CARTESIAN_POINT ( 'NONE',  ( -16.66936639845610202, 1523.382868172864164, 237.7608804993221838 ) ) ;
#13485 = CARTESIAN_POINT ( 'NONE',  ( -10.81518761075750135, 1424.921099531289883, 144.1705495212430037 ) ) ;
#13486 = CARTESIAN_POINT ( 'NONE',  ( -101.2260141739269983, 1384.598541685300006, 310.9427063241110432 ) ) ;
#13487 = CARTESIAN_POINT ( 'NONE',  ( -63.96209206476559217, 1385.081295340070028, 252.7243603260540112 ) ) ;
#13488 = CARTESIAN_POINT ( 'NONE',  ( -12.22594903035199998, 1490.655895506289880, 208.2081491493320016 ) ) ;
#13489 = CARTESIAN_POINT ( 'NONE',  ( -4.903489893049830961, 1508.551704408389924, 205.9871227246740091 ) ) ;
#13490 = CARTESIAN_POINT ( 'NONE',  ( -29.21489664634600203, 1509.775817166219895, 208.6508206576949931 ) ) ;
#13491 = CARTESIAN_POINT ( 'NONE',  ( 1.689251544526525040, 1526.344110814223313, 178.4720708657796422 ) ) ;
#13492 = CARTESIAN_POINT ( 'NONE',  ( -16.78911523114979687, 1410.870482649229871, 226.4125133055940182 ) ) ;
#13494 = ORIENTED_EDGE ( 'NONE', *, *, #35346, .F. ) ;
#13493 = CARTESIAN_POINT ( 'NONE',  ( -4.141727467620000880, 1502.720785751690073, 230.1321099188990047 ) ) ;
#13495 = CARTESIAN_POINT ( 'NONE',  ( -109.6584371800000071, 1384.889060004170005, 311.3230551812590079 ) ) ;
#13497 = CARTESIAN_POINT ( 'NONE',  ( 9.798888871456099992, 1470.345923341260004, 211.5472087270539987 ) ) ;
#13496 = CONICAL_SURFACE ( 'NONE', #83223, 0.9999999999999962252, 1.047197551199999799 ) ;
#13498 = EDGE_CURVE ( 'NONE', #11721, #42444, #95108, .T. ) ;
#13499 = CARTESIAN_POINT ( 'NONE',  ( -11.21575968800000034, 1500.080311486090068, 211.0958765857290018 ) ) ;
#13500 = DIRECTION ( 'NONE',  ( -0.2054769195713317398, -1.225281874271768203E-16, -0.9786619618251628516 ) ) ;
#13501 = CARTESIAN_POINT ( 'NONE',  ( -0.2485702761457760368, 1419.163708210889808, 184.5897658516240085 ) ) ;
#13502 = CARTESIAN_POINT ( 'NONE',  ( 0.002025548741049999855, 1465.101603547730065, 237.0127861282980177 ) ) ;
#13503 = CARTESIAN_POINT ( 'NONE',  ( 20.45064351119999912, 1410.549291213930019, 219.2538096947979795 ) ) ;
#13504 = B_SPLINE_SURFACE_WITH_KNOTS ( 'NONE', 5, 1, ( 
 ( #58705, #95472 ),
 ( #26597, #92837 ),
 ( #84445, #18738 ),
 ( #41349, #44525 ),
 ( #7731, #78671 ),
 ( #60794, #52390 ),
 ( #52933, #94920 ),
 ( #1989, #19288 ),
 ( #75517, #92287 ) ),
 .UNSPECIFIED., .F., .F., .F.,
 ( 6, 3, 6 ),
 ( 2, 2 ),
 ( 0.000000000000000000, 3.644587434069999965, 7.267547310080000322 ),
 ( 0.000000000000000000, 14.00000000000000000 ),
 .UNSPECIFIED. ) ;
#13505 = CARTESIAN_POINT ( 'NONE',  ( -1.795919047817160052, 1417.208812584569841, 185.7430934334929873 ) ) ;
#13506 = CARTESIAN_POINT ( 'NONE',  ( -9.563909551760000127, 1464.644246208489903, 228.2425506381989919 ) ) ;
#13507 = CARTESIAN_POINT ( 'NONE',  ( -17.86706492440000105, 1424.552609962230008, 227.1966067826979838 ) ) ;
#13509 = CARTESIAN_POINT ( 'NONE',  ( -11.61328182866063408, 1426.778534732830167, 135.3257729749631721 ) ) ;
#13508 = CARTESIAN_POINT ( 'NONE',  ( -3.294781662986297377, 1511.738149259171223, 201.1454951801678135 ) ) ;
#13510 = CARTESIAN_POINT ( 'NONE',  ( 27.45153079662120277, 1488.737808995739897, 208.6597228503549957 ) ) ;
#13511 = CARTESIAN_POINT ( 'NONE',  ( -102.6162175075999983, 1366.350733876289951, 304.2218459572590064 ) ) ;
#13512 = CARTESIAN_POINT ( 'NONE',  ( 16.73628186595838940, 1526.382868172863937, 234.1845039693043589 ) ) ;
#13513 = CARTESIAN_POINT ( 'NONE',  ( -24.02615488320000026, 1435.747509074109985, 211.0797796158580013 ) ) ;
#13514 = CARTESIAN_POINT ( 'NONE',  ( 4.262353028400000632, 1360.811275533930029, 210.6218459616991936 ) ) ;
#13515 = CARTESIAN_POINT ( 'NONE',  ( -6.948321743994999800, 1517.049325831759916, 205.0875650164470017 ) ) ;
#13516 = CARTESIAN_POINT ( 'NONE',  ( -11.27431701509130058, 1484.787218902319864, 185.3755693123800086 ) ) ;
#13517 = ORIENTED_EDGE ( 'NONE', *, *, #30305, .T. ) ;
#13518 = CARTESIAN_POINT ( 'NONE',  ( -7304.654438325449519, 5182.767774292097783, -10649.19336541359553 ) ) ;
#13519 = CARTESIAN_POINT ( 'NONE',  ( 14.20190145760000000, 1416.831305841230005, 196.5056575589980241 ) ) ;
#13521 = ORIENTED_EDGE ( 'NONE', *, *, #12505, .F. ) ;
#13520 = CARTESIAN_POINT ( 'NONE',  ( -67.84113287159999572, 1379.747601269260031, 279.1899061516589882 ) ) ;
#13522 = ORIENTED_EDGE ( 'NONE', *, *, #85721, .T. ) ;
#13523 = CARTESIAN_POINT ( 'NONE',  ( 4.326079331027290031, 1515.193466796180928, 207.2788825876957048 ) ) ;
#13524 = EDGE_LOOP ( 'NONE', ( #58197, #15211, #13172, #62338, #3812 ) ) ;
#13525 = CARTESIAN_POINT ( 'NONE',  ( 0.7917928493246050303, 1485.631538064390043, 220.9725313029949803 ) ) ;
#13526 = AXIS2_PLACEMENT_3D ( 'NONE', #105789, #48078, #29603 ) ;
#13527 = DIRECTION ( 'NONE',  ( -0.000000000000000000, -1.000000000000000000, -0.000000000000000000 ) ) ;
#13529 = CARTESIAN_POINT ( 'NONE',  ( 24.59498489902570029, 1440.913044926110160, 213.3385239659299941 ) ) ;
#13528 = CARTESIAN_POINT ( 'NONE',  ( -10.79135257254849911, 1424.935556423300113, 142.6770767068849750 ) ) ;
#13530 = CARTESIAN_POINT ( 'NONE',  ( -2.477975353594999763, 1516.839862955080207, 210.2583935552169976 ) ) ;
#13531 = B_SPLINE_CURVE_WITH_KNOTS ( 'NONE', 3,
 ( #6191, #49315, #40343, #15662, #7300, #31942, #66137, #83441, #6736, #109224 ),
 .UNSPECIFIED., .F., .F.,
 ( 4, 2, 2, 2, 4 ),
 ( 0.000000000000000000, 0.2500000000000000555, 0.5000000000000001110, 0.7500000000000000000, 1.000000000000000000 ),
 .UNSPECIFIED. ) ;
#13532 = CARTESIAN_POINT ( 'NONE',  ( -24.22051753955809872, 1452.051472547239882, 136.7607190383920113 ) ) ;
#13533 = CARTESIAN_POINT ( 'NONE',  ( -11.15489169059999952, 1425.160568487430055, 144.1681086605980227 ) ) ;
#13534 = CARTESIAN_POINT ( 'NONE',  ( 12.32229772640000043, 1409.510185481929966, 228.2568190012979983 ) ) ;
#13535 = CARTESIAN_POINT ( 'NONE',  ( 10.24469654192340151, 1481.487780100139844, 213.2148028526819985 ) ) ;
#13536 = SHAPE_DEFINITION_REPRESENTATION ( #2615, #49395 ) ;
#13538 = AXIS2_PLACEMENT_3D ( 'NONE', #100357, #98704, #23645 ) ;
#13537 = CARTESIAN_POINT ( 'NONE',  ( 41.34669637366360462, 1445.942886885989992, 134.0999999985539830 ) ) ;
#13539 =( BOUNDED_CURVE ( )  B_SPLINE_CURVE ( 3, ( #66848, #100423, #33757, #92562 ),
 .UNSPECIFIED., .F., .F. ) 
 B_SPLINE_CURVE_WITH_KNOTS ( ( 4, 4 ),
 ( 4.731011162954751548, 4.740923033578477330 ),
 .UNSPECIFIED. ) 
 CURVE ( )  GEOMETRIC_REPRESENTATION_ITEM ( )  RATIONAL_B_SPLINE_CURVE ( ( 1.000000000000000000, 0.9999918129184852678, 0.9999918129184852678, 1.000000000000000000 ) ) 
 REPRESENTATION_ITEM ( '' )  );
#13540 = CARTESIAN_POINT ( 'NONE',  ( -39.89415922108589996, 1441.413485003220103, 136.8703014936540114 ) ) ;
#13541 = CARTESIAN_POINT ( 'NONE',  ( -9.104803454449999833, 1421.479062531979935, 192.1853131694989827 ) ) ;
#13542 = CARTESIAN_POINT ( 'NONE',  ( 10.46269364489999987, 1491.122602117189899, 212.5073291737689942 ) ) ;
#13543 = ORIENTED_EDGE ( 'NONE', *, *, #100654, .F. ) ;
#13544 = ORIENTED_EDGE ( 'NONE', *, *, #64856, .T. ) ;
#13545 = CARTESIAN_POINT ( 'NONE',  ( 13.44542361074219272, 1410.755498752201902, 228.3208216478837755 ) ) ;
#13546 = CARTESIAN_POINT ( 'NONE',  ( 16.25736642822587541, 1514.559393048426728, 194.3359286633053955 ) ) ;
#13547 = CARTESIAN_POINT ( 'NONE',  ( 12.55779355105019945, 1500.097530588729796, 207.3428969177340093 ) ) ;
#13548 = CARTESIAN_POINT ( 'NONE',  ( -2.330134120368332784, 1515.551704408390151, 213.0801841075446248 ) ) ;
#13549 = CARTESIAN_POINT ( 'NONE',  ( -12.61160395369999954, 1379.083170920169778, 208.5076010308980017 ) ) ;
#13550 = CARTESIAN_POINT ( 'NONE',  ( -64.79513261177929451, 1379.738836812454565, 271.8835555406362801 ) ) ;
#13551 = CARTESIAN_POINT ( 'NONE',  ( 1.951019270089999980, 1465.893727891289927, 198.2556634289990143 ) ) ;
#13552 = DIRECTION ( 'NONE',  ( 1.755985294532464991E-16, -1.000000000000000000, 1.338183447452830017E-16 ) ) ;
#13553 = CARTESIAN_POINT ( 'NONE',  ( 8.513185067469999368, 1416.823418193329871, 193.0629307024979937 ) ) ;
#13554 = CARTESIAN_POINT ( 'NONE',  ( -86.70839285767250715, 1384.825211293280063, 290.2321663967470613 ) ) ;
#13555 = ORIENTED_EDGE ( 'NONE', *, *, #106659, .F. ) ;
#13556 = DIRECTION ( 'NONE',  ( -1.755985294532469921E-16, 1.000000000000000000, -1.338183447452831989E-16 ) ) ;
#13557 = CARTESIAN_POINT ( 'NONE',  ( 2.286472886424999906, 1516.883361325900069, 208.3638615500849767 ) ) ;
#13558 = VERTEX_POINT ( 'NONE', #59945 ) ;
#13559 = CARTESIAN_POINT ( 'NONE',  ( 39.12848466419210069, 1440.913060387330006, 266.3488084145499784 ) ) ;
#13560 = CARTESIAN_POINT ( 'NONE',  ( -0.001791162408697688979, 1451.698462366203557, 154.0731293207397812 ) ) ;
#13561 = EDGE_LOOP ( 'NONE', ( #41763, #77920, #33546, #44076 ) ) ;
#13562 = CARTESIAN_POINT ( 'NONE',  ( -17.61555691395482626, 1524.600389084707103, 180.6475253884790391 ) ) ;
#13563 = CARTESIAN_POINT ( 'NONE',  ( -16.05717579490000091, 1409.640429902829965, 192.0135573943979921 ) ) ;
#13564 = DIRECTION ( 'NONE',  ( 0.000000000000000000, 1.000000000000000000, 0.000000000000000000 ) ) ;
#13565 = B_SPLINE_CURVE_WITH_KNOTS ( 'NONE', 3,
 ( #81896, #5202, #39356, #73530, #56718, #90852, #82468, #5766, #83013, #6305, #108762, #32054, #66243, #33694, #76266, #7949, #75725, #67337, #102543, #136 ),
 .UNSPECIFIED., .F., .F.,
 ( 4, 2, 1, 2, 2, 2, 1, 1, 1, 2, 2, 4 ),
 ( 0.000000000000000000, 0.1249999999999671929, 0.1874999999999319433, 0.2187499999999147626, 0.2499999999998974987, 0.3749999999999085731, 0.4374999999999144018, 0.4687499999999174549, 0.4843749999999021894, 0.4921874999998945288, 0.4999999999998868683, 1.000000000000000000 ),
 .UNSPECIFIED. ) ;
#13566 = CARTESIAN_POINT ( 'NONE',  ( -9.614403431034910241, 1461.326383761360148, 207.8336058208969916 ) ) ;
#13567 = CARTESIAN_POINT ( 'NONE',  ( -9.473155674714520913, 1437.814104512410040, 211.9418041017489713 ) ) ;
#13568 = CARTESIAN_POINT ( 'NONE',  ( -5.586203269550379602, 1511.461696079649982, 200.4008954912939942 ) ) ;
#13569 = CARTESIAN_POINT ( 'NONE',  ( -2.853750452219999900, 1508.244831386429951, 180.6847236935980163 ) ) ;
#13570 = DIRECTION ( 'NONE',  ( -0.7882878497004317531, 0.000000000000000000, -0.6153066438895888890 ) ) ;
#13571 = CARTESIAN_POINT ( 'NONE',  ( -21.19880661589021642, 1526.382868172863937, 184.6948938244649696 ) ) ;
#13573 = CARTESIAN_POINT ( 'NONE',  ( -11.60004869885203505, 1422.719538780906987, 136.9994203799023751 ) ) ;
#13572 = CARTESIAN_POINT ( 'NONE',  ( 11.91931064610000135, 1462.777662358629868, 231.7750175801980106 ) ) ;
#13574 = CARTESIAN_POINT ( 'NONE',  ( 5.780861236055000241, 1516.783701990830195, 216.0610654530370027 ) ) ;
#13575 = CARTESIAN_POINT ( 'NONE',  ( -22.70509189929999749, 1409.705932116229860, 208.9454376012710100 ) ) ;
#13576 = CARTESIAN_POINT ( 'NONE',  ( -10.32752872691269985, 1480.656876279547532, 207.0167722732371942 ) ) ;
#13577 = AXIS2_PLACEMENT_3D ( 'NONE', #69519, #71170, #60003 ) ;
#13578 = CARTESIAN_POINT ( 'NONE',  ( 18.05155555704234160, 1447.068055369337799, 216.4740371628595028 ) ) ;
#13579 = CARTESIAN_POINT ( 'NONE',  ( 0.01322035751810150123, 1516.939819969850078, 213.1588969678170145 ) ) ;
#13580 = AXIS2_PLACEMENT_3D ( 'NONE', #79892, #88284, #70969 ) ;
#13581 = CARTESIAN_POINT ( 'NONE',  ( 3.272123973761280169, 1515.551704204689941, 212.7661975563979979 ) ) ;
#13582 = CARTESIAN_POINT ( 'NONE',  ( 29.41653834769454079, 1525.790287071785542, 221.5659752742948569 ) ) ;
#13584 = EDGE_LOOP ( 'NONE', ( #37137, #93284 ) ) ;
#13583 = CARTESIAN_POINT ( 'NONE',  ( -10.61669498371649922, 1508.551704408389924, 207.6874897006059939 ) ) ;
#13585 = CARTESIAN_POINT ( 'NONE',  ( -1.389373685237467404, 1526.382868173645647, 178.7050053866561541 ) ) ;
#13586 = CARTESIAN_POINT ( 'NONE',  ( 1.850459186030000239E-08, 1461.348673278630031, 221.5631610194979828 ) ) ;
#13587 = CARTESIAN_POINT ( 'NONE',  ( -10.95393205669999936, 1431.218946973030143, 151.6850706372979971 ) ) ;
#13588 = CARTESIAN_POINT ( 'NONE',  ( -7.527539147472119829, 1439.311770005190056, 204.6539930853050180 ) ) ;
#13589 = CARTESIAN_POINT ( 'NONE',  ( 2.188346568509999646, 1415.918919806530084, 232.1097023429979913 ) ) ;
#13590 = CARTESIAN_POINT ( 'NONE',  ( 17.04790460295257049, 1526.208281990536761, 182.6359253440253667 ) ) ;
#13591 = CARTESIAN_POINT ( 'NONE',  ( 12.09590827429999926, 1445.294669298059944, 186.8687448601980066 ) ) ;
#13593 = CARTESIAN_POINT ( 'NONE',  ( -2.461141685384151234, 1421.750035621559618, 139.1420193482996410 ) ) ;
#13592 = CARTESIAN_POINT ( 'NONE',  ( -24.98397261459999896, 1470.079709032829896, 213.5815951536679904 ) ) ;
#13594 = CARTESIAN_POINT ( 'NONE',  ( -2.296012628010000611, 1485.567333802330040, 182.6448570080980005 ) ) ;
#13595 = ORIENTED_EDGE ( 'NONE', *, *, #37154, .F. ) ;
#13596 = CARTESIAN_POINT ( 'NONE',  ( 4.028630584655000568, 1516.812923327049930, 205.6617440802170051 ) ) ;
#13597 = CARTESIAN_POINT ( 'NONE',  ( 3.386199433509999857, 1406.870005270030106, 269.6463559134979846 ) ) ;
#13598 = CARTESIAN_POINT ( 'NONE',  ( 0.7147294630619990263, 1515.255091259190067, 213.4463119403589815 ) ) ;
#13599 = CARTESIAN_POINT ( 'NONE',  ( 10.92694110706779931, 1489.979356094880131, 208.4358879340020110 ) ) ;
#13600 = CIRCLE ( 'NONE', #76208, 1.999999999999921618 ) ;
#13601 = EDGE_CURVE ( 'NONE', #93500, #19377, #44586, .T. ) ;
#13602 = CARTESIAN_POINT ( 'NONE',  ( 21.02260244975787629, 1428.161636300771761, 219.7400186835844522 ) ) ;
#13603 = CARTESIAN_POINT ( 'NONE',  ( 18.70459388984919968, 1509.566239199539950, 186.5372755781170042 ) ) ;
#13604 = CARTESIAN_POINT ( 'NONE',  ( 10.10004869885228196, 1422.222932908421399, 137.0999999980979567 ) ) ;
#13605 = CYLINDRICAL_SURFACE ( 'NONE', #71120, 7.500000000000000000 ) ;
#13606 = CARTESIAN_POINT ( 'NONE',  ( -2.499999999939920059, 1448.906648583599917, 155.3362572337090057 ) ) ;
#13607 = DIRECTION ( 'NONE',  ( 0.000000000000000000, 0.000000000000000000, -1.000000000000000000 ) ) ;
#13608 = CARTESIAN_POINT ( 'NONE',  ( 2.434526083211889791, 1449.527760230520016, 155.0642281637050246 ) ) ;
#13609 = LINE ( 'NONE', #81933, #51901 ) ;
#13610 = CARTESIAN_POINT ( 'NONE',  ( -11.25901873340000137, 1500.172003384790059, 210.8567363195689950 ) ) ;
#13611 = B_SPLINE_CURVE_WITH_KNOTS ( 'NONE', 3,
 ( #54951, #48194, #89077, #64456, #47092, #12363, #12912, #46551, #56589, #108633 ),
 .UNSPECIFIED., .F., .F.,
 ( 4, 2, 2, 2, 4 ),
 ( -0.1575290654450730021, -0.1192767518302590007, -0.08059141058286700687, -0.04144259288940019270, 0.000000000000000000 ),
 .UNSPECIFIED. ) ;
#13612 = CARTESIAN_POINT ( 'NONE',  ( -5.052203702459999946, 1416.825952163429974, 255.3819207742980097 ) ) ;
#13613 = CARTESIAN_POINT ( 'NONE',  ( -27.24294176985399929, 1507.989564505149929, 211.0449899648789938 ) ) ;
#13614 = CARTESIAN_POINT ( 'NONE',  ( 2.707874995500000104, 1440.598919863020001, 162.2212737941979981 ) ) ;
#13615 = CARTESIAN_POINT ( 'NONE',  ( -2.765183635730000145, 1475.775321107629907, 266.9581418145979796 ) ) ;
#13616 = CARTESIAN_POINT ( 'NONE',  ( -4.225123281554489907, 1446.251028937339925, 166.4050594329440003 ) ) ;
#13617 = CARTESIAN_POINT ( 'NONE',  ( -12.17813008270000097, 1438.571549855089870, 224.0393728361989929 ) ) ;
#13618 = CARTESIAN_POINT ( 'NONE',  ( 1.191524307911315805, 1526.382868172863937, 239.2353018730792087 ) ) ;
#13619 = CARTESIAN_POINT ( 'NONE',  ( -26.96405532890430123, 1384.839336572749971, 225.2101427744029820 ) ) ;
#13620 = LINE ( 'NONE', #79901, #14253 ) ;
#13621 = CARTESIAN_POINT ( 'NONE',  ( 4.487249773072029768, 1509.038615930399828, 211.6097810847319920 ) ) ;
#13622 = B_SPLINE_CURVE_WITH_KNOTS ( 'NONE', 3,
 ( #100036, #23327, #49112, #98934 ),
 .UNSPECIFIED., .F., .F.,
 ( 4, 4 ),
 ( 0.000000000000000000, 1.000000000000000000 ),
 .UNSPECIFIED. ) ;
#13623 = CARTESIAN_POINT ( 'NONE',  ( 12.11998591773940070, 1491.481808809230188, 207.0704772481079772 ) ) ;
#13624 = CARTESIAN_POINT ( 'NONE',  ( 31.14814740298836071, 1525.697946996672272, 216.7341141171428944 ) ) ;
#13625 = CARTESIAN_POINT ( 'NONE',  ( 7.167383184274696006, 1508.551704408383557, 203.6084103738921272 ) ) ;
#13626 = CARTESIAN_POINT ( 'NONE',  ( -18.88476838489999921, 1410.934753883030226, 196.4486472547980043 ) ) ;
#13627 = CARTESIAN_POINT ( 'NONE',  ( 12.62071130547100140, 1421.509729680500186, 206.8448693545120136 ) ) ;
#13628 = CARTESIAN_POINT ( 'NONE',  ( -45.45115383179999924, 1437.791621493419825, 268.9798130223979911 ) ) ;
#13629 = VERTEX_POINT ( 'NONE', #24626 ) ;
#13630 = CARTESIAN_POINT ( 'NONE',  ( -23.64337456402409998, 1435.765682558080016, 212.0350035351450231 ) ) ;
#13631 = CARTESIAN_POINT ( 'NONE',  ( -7.494335721685672524, 1510.727597956327827, 215.1764273590825098 ) ) ;
#13632 = CARTESIAN_POINT ( 'NONE',  ( -1.581688265954455330, 1426.946673137334528, 134.0999999980979851 ) ) ;
#13634 = CARTESIAN_POINT ( 'NONE',  ( -12.28497688116499909, 1512.406775501100128, 192.5826067984669976 ) ) ;
#13633 = CARTESIAN_POINT ( 'NONE',  ( 11.70398732309999978, 1426.301175225830093, 141.8453807417980101 ) ) ;
#13635 = CARTESIAN_POINT ( 'NONE',  ( -32.28466283162143213, 1522.382868172863937, 219.1752493337717738 ) ) ;
#13636 = CARTESIAN_POINT ( 'NONE',  ( 27.95267559299999860, 1445.173348664639889, 137.3670106792980050 ) ) ;
#13637 = CARTESIAN_POINT ( 'NONE',  ( -2.485846037024999955, 1516.545806094630279, 201.8003900583769905 ) ) ;
#13638 = CARTESIAN_POINT ( 'NONE',  ( 7.455956092950000169, 1426.129841999370001, 212.4361423238889870 ) ) ;
#13639 = CARTESIAN_POINT ( 'NONE',  ( 24.11200011979999758, 1496.633574749990203, 206.8275458132090137 ) ) ;
#13640 = CARTESIAN_POINT ( 'NONE',  ( 7.316304300719999709, 1507.280216345330018, 182.6970440027980089 ) ) ;
#13641 = CARTESIAN_POINT ( 'NONE',  ( -23.08547268613130043, 1417.322834144340050, 209.8740766914669962 ) ) ;
#13642 = CARTESIAN_POINT ( 'NONE',  ( -94.10761133452021454, 1379.531657316930023, 303.8031716826509978 ) ) ;
#13643 = CARTESIAN_POINT ( 'NONE',  ( 8.988338641415380081, 1366.896325247159893, 210.6218459616987957 ) ) ;
#13645 = ORIENTED_EDGE ( 'NONE', *, *, #100660, .T. ) ;
#13644 = CARTESIAN_POINT ( 'NONE',  ( -17.17760814124009983, 1517.051704413129983, 195.4929600000709797 ) ) ;
#13646 = ORIENTED_EDGE ( 'NONE', *, *, #52303, .F. ) ;
#13647 = FACE_OUTER_BOUND ( 'NONE', #31595, .T. ) ;
#13648 = CARTESIAN_POINT ( 'NONE',  ( -18.11398223329999979, 1409.545614585430030, 221.5743542847980052 ) ) ;
#13649 = CARTESIAN_POINT ( 'NONE',  ( 2.017315236659999567, 1508.958728568330116, 238.2933174268979997 ) ) ;
#13650 = CARTESIAN_POINT ( 'NONE',  ( -13.41779013147873556, 1444.382168163145707, 169.3666020351543580 ) ) ;
#13651 = CARTESIAN_POINT ( 'NONE',  ( -26.37063482739999998, 1509.833943247529987, 196.6232252598979926 ) ) ;
#13652 = CARTESIAN_POINT ( 'NONE',  ( -7.803201843315000552, 1511.730395268069969, 212.1995376873570081 ) ) ;
#13654 = CARTESIAN_POINT ( 'NONE',  ( 17.67011187210000145, 1416.263755027329807, 225.7720003271979863 ) ) ;
#13653 = CARTESIAN_POINT ( 'NONE',  ( -9.027091862569999847, 1384.059351705820063, 218.5832182276589890 ) ) ;
#13655 = CARTESIAN_POINT ( 'NONE',  ( 3.391241998599999974, 1410.302160405929953, 185.8412960619979799 ) ) ;
#13656 = CARTESIAN_POINT ( 'NONE',  ( 1.925297170580940076, 1519.551704408389924, 230.6853930747409720 ) ) ;
#13657 = CARTESIAN_POINT ( 'NONE',  ( -41.14067036663129784, 1444.183244330699836, 136.8991323217539957 ) ) ;
#13658 =( NAMED_UNIT ( * ) PLANE_ANGLE_UNIT ( ) SI_UNIT ( $, .RADIAN. ) );
#13659 = CARTESIAN_POINT ( 'NONE',  ( 11.05052638022029932, 1396.298953271829987, 208.4418276999739987 ) ) ;
#13660 = CARTESIAN_POINT ( 'NONE',  ( 0.7186627752419999515, 1416.547221146729953, 190.3376467024980059 ) ) ;
#13661 = CARTESIAN_POINT ( 'NONE',  ( 11.46948732749999955, 1425.744653023729825, 146.7325240263980106 ) ) ;
#13662 = CARTESIAN_POINT ( 'NONE',  ( 8.118253553867917915, 1509.196863918152303, 180.9331809445035901 ) ) ;
#13663 = ORIENTED_EDGE ( 'NONE', *, *, #52242, .F. ) ;
#13664 = CARTESIAN_POINT ( 'NONE',  ( -16.64885258016628100, 1526.344110814221949, 183.3327398900398748 ) ) ;
#13665 = CARTESIAN_POINT ( 'NONE',  ( 2.664535259099999805E-15, 1420.121162737279974, 209.1218459616989946 ) ) ;
#13666 = EDGE_LOOP ( 'NONE', ( #85739, #89540 ) ) ;
#13667 = ORIENTED_EDGE ( 'NONE', *, *, #108159, .T. ) ;
#13668 = DIRECTION ( 'NONE',  ( 0.03489949677361985775, 0.9993908270166123042, -2.608312631526985536E-10 ) ) ;
#13669 = CARTESIAN_POINT ( 'NONE',  ( -15.19063573600000083, 1460.421792992729934, 229.0783609468980160 ) ) ;
#13670 = CARTESIAN_POINT ( 'NONE',  ( -7.605711504302860249, 1407.218299713070110, 198.4634440487380118 ) ) ;
#13671 = CARTESIAN_POINT ( 'NONE',  ( -28.27139721233049485, 1526.382868172864164, 198.6830693683576499 ) ) ;
#13672 = CARTESIAN_POINT ( 'NONE',  ( 5.005700201405000271, 1516.732530461250008, 216.0598116305469887 ) ) ;
#13673 = CARTESIAN_POINT ( 'NONE',  ( 31.23437356469446868, 1512.187213306747481, 221.8968241038843701 ) ) ;
#13674 = VECTOR ( 'NONE', #88619, 1000.000000000000114 ) ;
#13675 = VERTEX_POINT ( 'NONE', #76720 ) ;
#13676 = CARTESIAN_POINT ( 'NONE',  ( -12.99430343120000053, 1503.123593417290067, 208.6821788852620045 ) ) ;
#13677 = FACE_OUTER_BOUND ( 'NONE', #79414, .T. ) ;
#13678 = CARTESIAN_POINT ( 'NONE',  ( -63.58938922729999632, 1374.821258372890043, 269.7443356278590159 ) ) ;
#13679 = ADVANCED_FACE ( 'NONE', ( #83453 ), #33053, .T. ) ;
#13680 = ADVANCED_FACE ( 'NONE', ( #93504 ), #109236, .F. ) ;
#13681 = LINE ( 'NONE', #54644, #64354 ) ;
#13682 = CARTESIAN_POINT ( 'NONE',  ( -3.267291643295000103, 1516.842852731759876, 205.6749038603869906 ) ) ;
#13683 = ORIENTED_EDGE ( 'NONE', *, *, #1786, .T. ) ;
#13684 = CARTESIAN_POINT ( 'NONE',  ( -1.704170752255000032, 1516.927039499179955, 209.8797722570040207 ) ) ;
#13685 = CARTESIAN_POINT ( 'NONE',  ( -20.65148373499999934, 1509.627424770630114, 230.2251059840980076 ) ) ;
#13686 = EDGE_CURVE ( 'NONE', #92019, #4978, #24800, .T. ) ;
#13688 = ADVANCED_FACE ( 'NONE', ( #58277 ), #85657, .T. ) ;
#13687 = CARTESIAN_POINT ( 'NONE',  ( -30.31662843376689764, 1419.814115720066638, 269.4742331920600691 ) ) ;
#13689 = CARTESIAN_POINT ( 'NONE',  ( 6.742834585605000264, 1512.383155430650049, 217.4973484156870143 ) ) ;
#13691 = EDGE_LOOP ( 'NONE', ( #98945, #53018, #85144, #100202, #109761, #76620 ) ) ;
#13690 = CARTESIAN_POINT ( 'NONE',  ( 2.485500793217951809, 1524.600389084707103, 175.7314721497423591 ) ) ;
#13692 = CARTESIAN_POINT ( 'NONE',  ( -0.006857176400948759853, 1451.190334390920043, 182.2890573962069993 ) ) ;
#13693 = CARTESIAN_POINT ( 'NONE',  ( -28.26405544321290009, 1440.913060387430050, 232.2089891578019945 ) ) ;
#13694 = CARTESIAN_POINT ( 'NONE',  ( -76.15242393239999785, 1384.064636357489917, 301.1578881669589691 ) ) ;
#13695 = CARTESIAN_POINT ( 'NONE',  ( 20.41258333560000082, 1494.156730172889866, 204.1224707391089908 ) ) ;
#13696 = CARTESIAN_POINT ( 'NONE',  ( 6.330344484264800009, 1409.538285424360083, 270.3701841699830197 ) ) ;
#13697 = CARTESIAN_POINT ( 'NONE',  ( 1.135185044044999980, 1516.778853242349896, 212.5689744308569971 ) ) ;
#13698 = CARTESIAN_POINT ( 'NONE',  ( -58.05210803569999456, 1379.715589859269812, 257.1931556633589935 ) ) ;
#13699 = CARTESIAN_POINT ( 'NONE',  ( 22.79202929419999890, 1409.708931967830040, 208.9783749518630032 ) ) ;
#13700 = CARTESIAN_POINT ( 'NONE',  ( -20.35720160430000192, 1509.285577334429945, 188.5733222705979983 ) ) ;
#13701 = CARTESIAN_POINT ( 'NONE',  ( -0.6587146994840009651, 1442.893519126590036, 219.0943606518089837 ) ) ;
#13702 = CARTESIAN_POINT ( 'NONE',  ( -7.709021946870369568, 1516.533929790709863, 211.5536301404889912 ) ) ;
#13703 =( BOUNDED_CURVE ( )  B_SPLINE_CURVE ( 3, ( #82197, #105776, #47516, #13322 ),
 .UNSPECIFIED., .F., .F. ) 
 B_SPLINE_CURVE_WITH_KNOTS ( ( 4, 4 ),
 ( 5.498203534171459239, 7.068313952310489867 ),
 .UNSPECIFIED. ) 
 CURVE ( )  GEOMETRIC_REPRESENTATION_ITEM ( )  RATIONAL_B_SPLINE_CURVE ( ( 1.000000000000000000, 0.8048994966190576861, 0.8048994966190576861, 1.000000000000000000 ) ) 
 REPRESENTATION_ITEM ( '' )  );
#13704 = CARTESIAN_POINT ( 'NONE',  ( 6.563915523884999992, 1517.184063036290127, 210.2461356256870033 ) ) ;
#13705 = CARTESIAN_POINT ( 'NONE',  ( 22.51756156282889876, 1509.699390964210124, 227.9212218486820234 ) ) ;
#13707 = EDGE_CURVE ( 'NONE', #8134, #102115, #80313, .T. ) ;
#13706 = DIRECTION ( 'NONE',  ( 0.000000000000000000, -1.000000000000000000, 1.836970198721029688E-16 ) ) ;
#13708 = CARTESIAN_POINT ( 'NONE',  ( 6.075340425011860113, 1422.570843986066166, 139.1419349980001812 ) ) ;
#13710 = ORIENTED_EDGE ( 'NONE', *, *, #57594, .F. ) ;
#13709 = CARTESIAN_POINT ( 'NONE',  ( -22.69270896030000273, 1385.265743060869909, 222.0224438233589979 ) ) ;
#13711 = CARTESIAN_POINT ( 'NONE',  ( -53.96171695904460108, 1385.098550058179853, 269.7692938834680376 ) ) ;
#13712 = CARTESIAN_POINT ( 'NONE',  ( 30.31940284289168375, 1523.456924617338018, 195.7503880522679651 ) ) ;
#13713 = CARTESIAN_POINT ( 'NONE',  ( 1.533058233270000015, 1417.373139556630122, 235.5867829536979912 ) ) ;
#13714 = ADVANCED_FACE ( 'NONE', ( #68350 ), #34719, .T. ) ;
#13715 = CARTESIAN_POINT ( 'NONE',  ( -20.38982155428609744, 1508.363530249980158, 228.6178044578140032 ) ) ;
#13716 = DIRECTION ( 'NONE',  ( -0.02616798426500960631, -0.9993150019883683122, 0.02616798426500965835 ) ) ;
#13717 = EDGE_CURVE ( 'NONE', #75960, #97242, #94317, .T. ) ;
#13718 = CARTESIAN_POINT ( 'NONE',  ( 11.44494620870000112, 1422.175562347540108, 206.4125902192689921 ) ) ;
#13719 = CARTESIAN_POINT ( 'NONE',  ( -31.23437356469455040, 1512.187213306747481, 197.3468678195118287 ) ) ;
#13721 = CARTESIAN_POINT ( 'NONE',  ( -16.32516330111020153, 1416.706030269645225, 208.2451548885862564 ) ) ;
#13720 = CARTESIAN_POINT ( 'NONE',  ( 1.129386202275000084, 1516.613712827999962, 216.4452363774470030 ) ) ;
#13722 = CARTESIAN_POINT ( 'NONE',  ( -22.53878221424140094, 1411.058442688259902, 212.0450776560099939 ) ) ;
#13723 = CARTESIAN_POINT ( 'NONE',  ( 33.82780500856144101, 1523.429859730330691, 220.5611772381395213 ) ) ;
#13724 = ORIENTED_EDGE ( 'NONE', *, *, #93831, .T. ) ;
#13725 = CARTESIAN_POINT ( 'NONE',  ( -4.035490750684999739, 1516.630499592039996, 201.4102952541169884 ) ) ;
#13726 = CARTESIAN_POINT ( 'NONE',  ( -15.91746622356499863, 1512.594959757389915, 220.0895646873669875 ) ) ;
#13727 = ORIENTED_EDGE ( 'NONE', *, *, #47344, .T. ) ;
#13728 = CARTESIAN_POINT ( 'NONE',  ( 21.83863730836035444, 1523.580203803270933, 234.9763103460704770 ) ) ;
#13729 = AXIS2_PLACEMENT_3D ( 'NONE', #39399, #74122, #4161 ) ;
#13730 = CARTESIAN_POINT ( 'NONE',  ( 23.99815499239999994, 1446.810867530319911, 216.6209177652979747 ) ) ;
#13731 = CARTESIAN_POINT ( 'NONE',  ( 6.562075743890480872, 1439.579727447380037, 154.3677175799390398 ) ) ;
#13732 = CARTESIAN_POINT ( 'NONE',  ( 8.961967794501056517, 1424.998307906903619, 195.6926762925650110 ) ) ;
#13733 =( BOUNDED_CURVE ( )  B_SPLINE_CURVE ( 3, ( #48850, #91383, #99759, #50494 ),
 .UNSPECIFIED., .F., .T. ) 
 B_SPLINE_CURVE_WITH_KNOTS ( ( 4, 4 ),
 ( 0.000000000000000000, 0.7048113239778029948 ),
 .UNSPECIFIED. ) 
 CURVE ( )  GEOMETRIC_REPRESENTATION_ITEM ( )  RATIONAL_B_SPLINE_CURVE ( ( 1.000000000000000000, 0.9590300661663095916, 0.9590300661663095916, 1.000000000000000000 ) ) 
 REPRESENTATION_ITEM ( '' )  );
#13734 = CARTESIAN_POINT ( 'NONE',  ( 2.353483798069999633, 1441.866266782089951, 218.3762686079190019 ) ) ;
#13735 = CARTESIAN_POINT ( 'NONE',  ( -27.75185986752750011, 1509.834791352900083, 200.9939385945500021 ) ) ;
#13736 = CARTESIAN_POINT ( 'NONE',  ( -4.225063841879999949, 1446.249083902760276, 165.9135368162980058 ) ) ;
#13737 = CARTESIAN_POINT ( 'NONE',  ( -19.90838456339999851, 1426.253534361829907, 222.6506651951980018 ) ) ;
#13738 = CARTESIAN_POINT ( 'NONE',  ( -19.09679337948567834, 1472.008470696052427, 269.5331241273682394 ) ) ;
#13739 = CARTESIAN_POINT ( 'NONE',  ( -105.6969335659999985, 1391.135062214819982, 302.0247559743589818 ) ) ;
#13740 = CARTESIAN_POINT ( 'NONE',  ( 16.69260089830000027, 1445.375861641200117, 190.4510651168980075 ) ) ;
#13742 = CARTESIAN_POINT ( 'NONE',  ( -18.44765774540020331, 1436.509381524827404, 212.9697281596460243 ) ) ;
#13741 = CARTESIAN_POINT ( 'NONE',  ( -106.2334119559999976, 1391.826625675339983, 302.0221818237590128 ) ) ;
#13743 = CARTESIAN_POINT ( 'NONE',  ( -34.90552475763031737, 1457.877490100739578, 269.5302477027990449 ) ) ;
#13744 = ORIENTED_EDGE ( 'NONE', *, *, #13498, .T. ) ;
#13745 = LINE ( 'NONE', #71524, #19489 ) ;
#13746 = CARTESIAN_POINT ( 'NONE',  ( -16.39029410570000067, 1508.551704408389924, 213.5052586272289830 ) ) ;
#13747 = CARTESIAN_POINT ( 'NONE',  ( -10.75110831211170925, 1424.962421341598429, 140.1405872077429535 ) ) ;
#13748 = FACE_OUTER_BOUND ( 'NONE', #69950, .T. ) ;
#13749 = CARTESIAN_POINT ( 'NONE',  ( -4.963802804109999300, 1497.713060387329961, 230.9126810519979927 ) ) ;
#13750 = CARTESIAN_POINT ( 'NONE',  ( 1.461527277530950020, 1494.461654286979865, 181.6651345972479703 ) ) ;
#13751 = CARTESIAN_POINT ( 'NONE',  ( -0.1669645939030000026, 1417.346234731630148, 235.5731359111979941 ) ) ;
#13752 = VECTOR ( 'NONE', #101987, 1000.000000000000000 ) ;
#13753 = CARTESIAN_POINT ( 'NONE',  ( -13.41712910526564428, 1444.385627665757056, 186.9257196579762592 ) ) ;
#13754 = CARTESIAN_POINT ( 'NONE',  ( -4.237827489471030242E-15, 1374.913060387289988, 209.1218459572589836 ) ) ;
#13755 = CARTESIAN_POINT ( 'NONE',  ( -16.68599179819999989, 1461.099982565929849, 230.2790296985980092 ) ) ;
#13756 = PRODUCT_RELATED_PRODUCT_CATEGORY ( 'part', '', ( #48283 ) ) ;
#13757 = DIRECTION ( 'NONE',  ( 0.000000000000000000, 1.000000000000000000, 0.000000000000000000 ) ) ;
#13758 = CARTESIAN_POINT ( 'NONE',  ( -15.27276080761430066, 1415.677402202069970, 208.6833046621170240 ) ) ;
#13759 = CARTESIAN_POINT ( 'NONE',  ( 24.18632888440000173, 1435.416476431710180, 137.3041773823979952 ) ) ;
#13760 = CARTESIAN_POINT ( 'NONE',  ( 6.634516952019999358, 1427.014769761329944, 214.0188387700289923 ) ) ;
#13762 = VERTEX_POINT ( 'NONE', #31 ) ;
#13761 = FACE_OUTER_BOUND ( 'NONE', #62968, .T. ) ;
#13763 = CARTESIAN_POINT ( 'NONE',  ( -103.5772069679999845, 1380.769252584959986, 299.2318157808589945 ) ) ;
#13764 = CARTESIAN_POINT ( 'NONE',  ( 14.49132057761110026, 1513.569700117019920, 224.2258521170180074 ) ) ;
#13765 = ORIENTED_EDGE ( 'NONE', *, *, #76451, .F. ) ;
#13766 = ORIENTED_EDGE ( 'NONE', *, *, #8063, .T. ) ;
#13767 = CARTESIAN_POINT ( 'NONE',  ( -12.30179092849999911, 1502.247259483089920, 210.0097377508620013 ) ) ;
#13768 = CARTESIAN_POINT ( 'NONE',  ( -19.02270174366725541, 1526.382868172864164, 232.8547275633879678 ) ) ;
#13770 = CARTESIAN_POINT ( 'NONE',  ( -30.53571888319999772, 1440.913060387119913, 240.1260121746980190 ) ) ;
#13769 = CARTESIAN_POINT ( 'NONE',  ( 34.62851765911016599, 1423.653131627848325, 269.5264373704582113 ) ) ;
#13771 = CARTESIAN_POINT ( 'NONE',  ( -20.32871120239999740, 1505.119216028529991, 189.5393039330980116 ) ) ;
#13772 = CARTESIAN_POINT ( 'NONE',  ( -11.67569575809999982, 1433.467371848380026, 150.9894905005979808 ) ) ;
#13773 = EDGE_CURVE ( 'NONE', #42556, #71088, #26302, .T. ) ;
#13774 = CARTESIAN_POINT ( 'NONE',  ( 22.52609270479999992, 1509.699688878229836, 209.5602205471840023 ) ) ;
#13775 = CARTESIAN_POINT ( 'NONE',  ( -19.21919559470000394, 1486.268158006530030, 189.5244098630979863 ) ) ;
#13776 = AXIS2_PLACEMENT_3D ( 'NONE', #50255, #100081, #110682 ) ;
#13777 = CARTESIAN_POINT ( 'NONE',  ( 26.41765092578760132, 1465.529458439430073, 209.4782902591080074 ) ) ;
#13778 = EDGE_CURVE ( 'NONE', #22756, #88339, #100798, .T. ) ;
#13779 = CARTESIAN_POINT ( 'NONE',  ( -14.94707557629999961, 1464.258769156330118, 228.3755978434980136 ) ) ;
#13780 = CARTESIAN_POINT ( 'NONE',  ( 0.1141777316373559920, 1515.158022524200078, 213.4488534336589964 ) ) ;
#13781 = LINE ( 'NONE', #98358, #26469 ) ;
#13782 = CARTESIAN_POINT ( 'NONE',  ( -6.593308786588120363, 1477.792378428569918, 218.6399986688279853 ) ) ;
#13783 = CARTESIAN_POINT ( 'NONE',  ( 4.058282819955586262, 1361.791725152615072, 207.6218459616988241 ) ) ;
#13784 = CARTESIAN_POINT ( 'NONE',  ( -11.05535904383813772, 1509.424240718018382, 237.0105353482844350 ) ) ;
#13786 = ORIENTED_EDGE ( 'NONE', *, *, #4667, .T. ) ;
#13785 = CARTESIAN_POINT ( 'NONE',  ( 1.580222541931140213E-08, 1407.992705438240137, 263.0165072346359807 ) ) ;
#13787 = ORIENTED_EDGE ( 'NONE', *, *, #54464, .T. ) ;
#13788 = CARTESIAN_POINT ( 'NONE',  ( -11.86521650604180067, 1432.274229656389934, 149.9820447970350017 ) ) ;
#13789 = CARTESIAN_POINT ( 'NONE',  ( 19.28284482985129955, 1498.021048960190001, 221.9090220746840316 ) ) ;
#13790 = CARTESIAN_POINT ( 'NONE',  ( -25.76377174219999944, 1467.778888206429883, 270.2932678896979724 ) ) ;
#13791 = CARTESIAN_POINT ( 'NONE',  ( 12.76760079159999961, 1508.356069781229962, 233.5455612081979950 ) ) ;
#13792 = CARTESIAN_POINT ( 'NONE',  ( -123.2094608542982570, 1377.418846546388068, 298.8629130685321229 ) ) ;
#13793 = CARTESIAN_POINT ( 'NONE',  ( 35.95601944595329513, 1451.436210798189904, 134.6957181338510168 ) ) ;
#13794 = EDGE_CURVE ( 'NONE', #82045, #108700, #12353, .T. ) ;
#13795 = CARTESIAN_POINT ( 'NONE',  ( 4.327096512618459734, 1515.154622198469951, 209.3777992006019701 ) ) ;
#13796 = CARTESIAN_POINT ( 'NONE',  ( -8.369546976630001467, 1384.842463915960025, 199.7754933009489946 ) ) ;
#13797 = CARTESIAN_POINT ( 'NONE',  ( 12.59722465782060929, 1416.835288274323830, 223.3994078652815745 ) ) ;
#13798 = CARTESIAN_POINT ( 'NONE',  ( -3.776193667280000277, 1457.838857791890177, 218.3090359982990094 ) ) ;
#13799 = CARTESIAN_POINT ( 'NONE',  ( 11.91688765630230762, 1364.847998537791682, 208.3718459617010978 ) ) ;
#13800 = CARTESIAN_POINT ( 'NONE',  ( -33.58184217919399828, 1416.684724268960053, 268.5991851112240170 ) ) ;
#13801 = ORIENTED_EDGE ( 'NONE', *, *, #106154, .T. ) ;
#13802 = DIRECTION ( 'NONE',  ( -0.000000000000000000, -1.000000000000000000, -0.000000000000000000 ) ) ;
#13803 = ORIENTED_EDGE ( 'NONE', *, *, #53675, .T. ) ;
#13804 = ORIENTED_EDGE ( 'NONE', *, *, #17385, .T. ) ;
#13805 = CARTESIAN_POINT ( 'NONE',  ( 2.494020282435000180, 1516.876240617270014, 211.4047611534970201 ) ) ;
#13806 = CARTESIAN_POINT ( 'NONE',  ( 4.881181484400870296, 1423.435338320519350, 184.1811047220472517 ) ) ;
#13807 = EDGE_CURVE ( 'NONE', #46504, #104636, #82961, .T. ) ;
#13809 = CARTESIAN_POINT ( 'NONE',  ( -2.959283871624123652, 1440.912977528160809, 170.5323342040075545 ) ) ;
#13808 = CARTESIAN_POINT ( 'NONE',  ( 6.948321705865000197, 1517.049325831759916, 213.1561268858870051 ) ) ;
#13810 = CARTESIAN_POINT ( 'NONE',  ( -16.90743626299999747, 1425.425775615030034, 191.1833389174979914 ) ) ;
#13811 = CIRCLE ( 'NONE', #47809, 0.5000000000000004441 ) ;
#13812 = CARTESIAN_POINT ( 'NONE',  ( -2.338681342886227643, 1449.681344963495803, 182.9863964398574865 ) ) ;
#13813 = ORIENTED_EDGE ( 'NONE', *, *, #20296, .T. ) ;
#13814 = CARTESIAN_POINT ( 'NONE',  ( -26.33338208449999840, 1436.244409726509957, 136.6927053810979942 ) ) ;
#13815 = EDGE_CURVE ( 'NONE', #38555, #69834, #64344, .T. ) ;
#13816 = ADVANCED_FACE ( 'NONE', ( #28879 ), #71475, .F. ) ;
#13817 = CARTESIAN_POINT ( 'NONE',  ( 7.716878902974999122, 1516.833976295079992, 201.7919207096969672 ) ) ;
#13818 = CARTESIAN_POINT ( 'NONE',  ( -35.15123146724445746, 1451.685553865498377, 134.6826639932257024 ) ) ;
#13819 = CARTESIAN_POINT ( 'NONE',  ( -11.64339741151500007, 1384.514520786359981, 200.1925094546899970 ) ) ;
#13820 = CARTESIAN_POINT ( 'NONE',  ( 1.332267629549999902E-15, 1391.913060387289988, 209.1218459616989946 ) ) ;
#13821 = CARTESIAN_POINT ( 'NONE',  ( -17.29882006758230162, 1523.542365884046376, 180.8528181918347570 ) ) ;
#13822 = CARTESIAN_POINT ( 'NONE',  ( -2.494988787169999611, 1396.538086358129931, 196.8133008506979991 ) ) ;
#13824 = VERTEX_POINT ( 'NONE', #10974 ) ;
#13823 = CARTESIAN_POINT ( 'NONE',  ( -8.774526971944801801, 1365.153596817209063, 210.6218459617142003 ) ) ;
#13825 = ORIENTED_EDGE ( 'NONE', *, *, #92728, .F. ) ;
#13826 = DIRECTION ( 'NONE',  ( 0.000000000000000000, -1.000000000000000000, 6.123233995736769734E-17 ) ) ;
#13827 = EDGE_CURVE ( 'NONE', #44756, #30516, #2598, .T. ) ;
#13828 = DIRECTION ( 'NONE',  ( -0.9980967576068039415, 0.06164622171533089973, -0.001614249983439999900 ) ) ;
#13829 = CARTESIAN_POINT ( 'NONE',  ( -13.31006320136440024, 1436.110929636480023, 150.6000258946120312 ) ) ;
#13830 = CARTESIAN_POINT ( 'NONE',  ( -0.03701251498699020120, 1409.597194001649996, 185.2367800943269742 ) ) ;
#13831 = AXIS2_PLACEMENT_3D ( 'NONE', #42530, #91825, #43094 ) ;
#13832 = CARTESIAN_POINT ( 'NONE',  ( -4.031168805994999715, 1516.805675336850072, 209.8787446699039947 ) ) ;
#13833 = B_SPLINE_CURVE_WITH_KNOTS ( 'NONE', 3,
 ( #87361, #10657, #11216, #46479, #45380, #80611, #63830 ),
 .UNSPECIFIED., .F., .F.,
 ( 4, 3, 4 ),
 ( -157.6565403109999863, -100.4035695696150015, -30.32814665380000463 ),
 .UNSPECIFIED. ) ;
#13834 = EDGE_CURVE ( 'NONE', #84259, #16269, #86685, .T. ) ;
#13835 = CARTESIAN_POINT ( 'NONE',  ( -68.74858467349999103, 1379.747915711970109, 280.1349441135590155 ) ) ;
#13836 = CARTESIAN_POINT ( 'NONE',  ( -19.49135957599999713, 1435.772693388610151, 224.3034628955980168 ) ) ;
#13837 = CARTESIAN_POINT ( 'NONE',  ( 8.311313017077319287, 1438.191820040039829, 214.6582622035640213 ) ) ;
#13838 = DIRECTION ( 'NONE',  ( -9.120877578445558697E-47, 1.000000000000000000, -1.836970198721029688E-16 ) ) ;
#13839 = CARTESIAN_POINT ( 'NONE',  ( 11.87714094419999888, 1445.674110516890096, 187.3195964094980184 ) ) ;
#13840 = CARTESIAN_POINT ( 'NONE',  ( -5.789394700334999477, 1517.164987839469859, 207.4150481461570052 ) ) ;
#13841 = EDGE_LOOP ( 'NONE', ( #107525, #1979, #32965, #84928 ) ) ;
#13842 = DIRECTION ( 'NONE',  ( 0.02616795315377970499, -0.9993150033772691954, 0.02616796233622665710 ) ) ;
#13843 = CARTESIAN_POINT ( 'NONE',  ( -12.81185530964340025, 1416.835419214280137, 196.2456592538570135 ) ) ;
#13844 = ORIENTED_EDGE ( 'NONE', *, *, #82806, .T. ) ;
#13845 = CARTESIAN_POINT ( 'NONE',  ( 7.392443486661196772, 1456.543737492606169, 227.5801189955647885 ) ) ;
#13846 = CARTESIAN_POINT ( 'NONE',  ( 24.11264749536519858, 1452.065943334660005, 136.7679447854590080 ) ) ;
#13847 = CARTESIAN_POINT ( 'NONE',  ( 13.25967437329999932, 1414.983773852829927, 197.8194332346980104 ) ) ;
#13848 = EDGE_CURVE ( 'NONE', #44161, #2901, #96376, .T. ) ;
#13849 = LINE ( 'NONE', #48033, #61073 ) ;
#13850 = CARTESIAN_POINT ( 'NONE',  ( 18.78254047960000150, 1409.568961153929877, 198.1179043739980159 ) ) ;
#13851 = CARTESIAN_POINT ( 'NONE',  ( 29.99620953741488449, 1524.382868172863937, 198.4974435154498735 ) ) ;
#13852 = CARTESIAN_POINT ( 'NONE',  ( 32.85805783624306287, 1523.678648413191695, 201.0453875934054224 ) ) ;
#13853 = ADVANCED_FACE ( 'NONE', ( #70917 ), #70360, .F. ) ;
#13854 = CARTESIAN_POINT ( 'NONE',  ( -0.07181796816713301168, 1506.512156835258793, 187.0734039034420562 ) ) ;
#13855 = CARTESIAN_POINT ( 'NONE',  ( 24.59034321158132030, 1443.280774260655335, 213.0723101612708206 ) ) ;
#13856 = AXIS2_PLACEMENT_3D ( 'NONE', #75878, #8105, #59092 ) ;
#13857 = CARTESIAN_POINT ( 'NONE',  ( 2.500000000000000000, 1439.559074696859852, 165.1937459529769967 ) ) ;
#13858 = CARTESIAN_POINT ( 'NONE',  ( 2.291676273424999799, 1516.534976163889951, 216.4430396779769978 ) ) ;
#13859 = ORIENTED_EDGE ( 'NONE', *, *, #107025, .T. ) ;
#13860 = CARTESIAN_POINT ( 'NONE',  ( 7.709114176761669768, 1516.537453364269822, 207.2981373406960017 ) ) ;
#13861 = DIRECTION ( 'NONE',  ( 0.000000000000000000, 1.000000000000000000, 0.000000000000000000 ) ) ;
#13862 = EDGE_CURVE ( 'NONE', #53297, #36343, #46901, .T. ) ;
#13863 = CARTESIAN_POINT ( 'NONE',  ( -2.500000000000000000, 1448.552414648389913, 183.1264116536979998 ) ) ;
#13864 = CARTESIAN_POINT ( 'NONE',  ( 0.2699275208915274948, 1452.980711559484462, 183.2606270490059615 ) ) ;
#13865 = CARTESIAN_POINT ( 'NONE',  ( 0.9117115396459989363, 1473.693686166890075, 219.3348546764989919 ) ) ;
#13866 = CARTESIAN_POINT ( 'NONE',  ( 11.31084951485244439, 1425.493973826349475, 138.7225535732650883 ) ) ;
#13867 = FACE_OUTER_BOUND ( 'NONE', #26592, .T. ) ;
#13868 = CARTESIAN_POINT ( 'NONE',  ( -2.500000000000000000, 1429.342233201230101, 157.2075084771979903 ) ) ;
#13869 = CARTESIAN_POINT ( 'NONE',  ( -109.1450416020000063, 1385.242479493820156, 297.1468691531589457 ) ) ;
#13870 = CARTESIAN_POINT ( 'NONE',  ( -4.329448781177520189, 1515.064792686469900, 210.9648092169189795 ) ) ;
#13871 = CARTESIAN_POINT ( 'NONE',  ( 30.29215768548720078, 1440.913060385460085, 239.2711865524379959 ) ) ;
#13872 = CARTESIAN_POINT ( 'NONE',  ( -10.26524962935310015, 1471.547416617549970, 209.8736591177010098 ) ) ;
#13873 = CARTESIAN_POINT ( 'NONE',  ( 20.71343476517513338, 1512.187213306747481, 179.9059455038194528 ) ) ;
#13874 = VERTEX_POINT ( 'NONE', #29410 ) ;
#13875 = ORIENTED_EDGE ( 'NONE', *, *, #29200, .F. ) ;
#13876 = B_SPLINE_CURVE_WITH_KNOTS ( 'NONE', 3,
 ( #71531, #83190, #92679, #75892, #99972, #109499, #82072 ),
 .UNSPECIFIED., .F., .F.,
 ( 4, 3, 4 ),
 ( 4.902660412303320943E-05, 0.0008424868313097026457, 0.002262927881332990609 ),
 .UNSPECIFIED. ) ;
#13877 = CARTESIAN_POINT ( 'NONE',  ( 11.23388613411650638, 1442.762691980111640, 207.0699376370758955 ) ) ;
#13878 = AXIS2_PLACEMENT_3D ( 'NONE', #77283, #75081, #92395 ) ;
#13879 = DIRECTION ( 'NONE',  ( -0.000000000000000000, -1.000000000000000000, -0.000000000000000000 ) ) ;
#13880 = CARTESIAN_POINT ( 'NONE',  ( -1.160688383098266607, 1409.478226354181515, 185.8299063934154276 ) ) ;
#13881 = CARTESIAN_POINT ( 'NONE',  ( 11.36218962193319904, 1502.758839311570000, 211.1250559367580024 ) ) ;
#13882 = PLANE ( 'NONE',  #12454 ) ;
#13883 = VECTOR ( 'NONE', #40248, 1000.000000000000114 ) ;
#13884 = CARTESIAN_POINT ( 'NONE',  ( -16.73628186595804834, 1526.382868172864164, 234.1845039693045862 ) ) ;
#13885 = EDGE_CURVE ( 'NONE', #84300, #9928, #40971, .T. ) ;
#13886 = CARTESIAN_POINT ( 'NONE',  ( -31.34137657934000387, 1523.382868172864164, 221.9025654077414345 ) ) ;
#13887 = CARTESIAN_POINT ( 'NONE',  ( -43.53822014877789570, 1383.822559367279837, 248.2938733222130168 ) ) ;
#13888 = CIRCLE ( 'NONE', #71175, 0.9999999999999309441 ) ;
#13889 = DIRECTION ( 'NONE',  ( 0.4090087482554486953, 0.000000000000000000, 0.9125304618753892205 ) ) ;
#13890 = DIRECTION ( 'NONE',  ( -0.9455185755993178454, 0.000000000000000000, 0.3255681544571539243 ) ) ;
#13891 = CARTESIAN_POINT ( 'NONE',  ( -12.18420476197879943, 1502.395317283280065, 208.9521721262090068 ) ) ;
#13892 = CARTESIAN_POINT ( 'NONE',  ( 1.594477961910000019, 1465.161208926829886, 235.7125682595980152 ) ) ;
#13894 = VERTEX_POINT ( 'NONE', #61958 ) ;
#13893 = CARTESIAN_POINT ( 'NONE',  ( -4.848919996459999382, 1489.192135936889827, 188.8958457811990002 ) ) ;
#13895 = CARTESIAN_POINT ( 'NONE',  ( -0.4378289194489999869, 1452.327479224130002, 183.2409674511980029 ) ) ;
#13896 = CARTESIAN_POINT ( 'NONE',  ( -24.91449396329999999, 1379.865431598030000, 218.2371346374789880 ) ) ;
#13897 = CARTESIAN_POINT ( 'NONE',  ( -4.124924170559999936, 1474.647204749290040, 198.4545245537989899 ) ) ;
#13899 = VERTEX_POINT ( 'NONE', #72016 ) ;
#13898 = CARTESIAN_POINT ( 'NONE',  ( -31.11295512654738715, 1525.790287071770535, 216.3449412819151689 ) ) ;
#13900 = CARTESIAN_POINT ( 'NONE',  ( 7.755350745836239845, 1459.738700650969804, 228.9106056711640065 ) ) ;
#13901 = ORIENTED_EDGE ( 'NONE', *, *, #59607, .T. ) ;
#13902 = CARTESIAN_POINT ( 'NONE',  ( -10.24752963132049999, 1388.126283780050017, 217.1897018944860349 ) ) ;
#13903 = CARTESIAN_POINT ( 'NONE',  ( 35.00372651682169334, 1437.143722424219959, 136.5385674641080129 ) ) ;
#13904 = CARTESIAN_POINT ( 'NONE',  ( -113.4000000000000057, 1390.913060387289988, 304.2218459572590064 ) ) ;
#13905 = CARTESIAN_POINT ( 'NONE',  ( -4.329791528864999961, 1515.051704408389924, 212.4519801359869859 ) ) ;
#13906 = CARTESIAN_POINT ( 'NONE',  ( -106.5596784199999973, 1379.201018628780048, 300.2813271376589910 ) ) ;
#13907 = ADVANCED_FACE ( 'NONE', ( #97727 ), #12625, .T. ) ;
#13908 = CARTESIAN_POINT ( 'NONE',  ( 9.549000552458089430, 1470.075890067440014, 212.3436661921319910 ) ) ;
#13909 = CARTESIAN_POINT ( 'NONE',  ( 7.731549308429999989, 1490.593532645290225, 209.4666211040999997 ) ) ;
#13910 = TOROIDAL_SURFACE ( 'NONE', #12175, 1.000000000000000000, 1.000000000000000000 ) ;
#13911 = DIRECTION ( 'NONE',  ( 0.000000000000000000, 1.000000000000000000, 0.000000000000000000 ) ) ;
#13912 = CARTESIAN_POINT ( 'NONE',  ( 18.28980197170000110, 1425.401422957629848, 225.1796033777980028 ) ) ;
#13913 = CARTESIAN_POINT ( 'NONE',  ( -2.170627987649289992, 1485.611815795640041, 197.4219879416550327 ) ) ;
#13914 = CARTESIAN_POINT ( 'NONE',  ( -18.58834951790000289, 1452.000874628230122, 191.0927309286979892 ) ) ;
#13915 = CYLINDRICAL_SURFACE ( 'NONE', #30510, 1.000000000000000888 ) ;
#13916 = LINE ( 'NONE', #74421, #46317 ) ;
#13917 = ORIENTED_EDGE ( 'NONE', *, *, #80887, .F. ) ;
#13918 = ORIENTED_EDGE ( 'NONE', *, *, #25586, .T. ) ;
#13919 = CARTESIAN_POINT ( 'NONE',  ( -109.1646150049198809, 1384.938164062486749, 297.1326220263049436 ) ) ;
#13920 = CARTESIAN_POINT ( 'NONE',  ( 18.98230138205870077, 1456.646672190919844, 228.3944069568109967 ) ) ;
#13921 = CARTESIAN_POINT ( 'NONE',  ( -13.07625826729999829, 1434.964688253329996, 150.0206613299980063 ) ) ;
#13922 = B_SPLINE_CURVE_WITH_KNOTS ( 'NONE', 5,
 ( #11265, #1211, #9581, #86297, #71186, #103080, #88515, #44315, #43210, #105308, #77359, #26381 ),
 .UNSPECIFIED., .F., .F.,
 ( 6, 3, 3, 6 ),
 ( 22.90453557749570024, 35.06371889219999360, 67.00219837880000284, 78.53166967965620415 ),
 .UNSPECIFIED. ) ;
#13923 = EDGE_CURVE ( 'NONE', #103948, #70633, #97645, .T. ) ;
#13924 = FACE_OUTER_BOUND ( 'NONE', #108589, .T. ) ;
#13925 = CARTESIAN_POINT ( 'NONE',  ( -20.29633810112639836, 1498.028987413850246, 190.6747321216680007 ) ) ;
#13926 = CARTESIAN_POINT ( 'NONE',  ( 6.447768684100981140, 1509.138221431309603, 237.9469272652861775 ) ) ;
#13927 = CARTESIAN_POINT ( 'NONE',  ( -109.3009594169999872, 1387.251231179749993, 311.0223495752589997 ) ) ;
#13928 = CARTESIAN_POINT ( 'NONE',  ( -7.946770108222969142, 1511.532743959790196, 215.0475857338450396 ) ) ;
#13929 = CARTESIAN_POINT ( 'NONE',  ( -9.328535443848540609, 1363.278783432131831, 210.6218459616991936 ) ) ;
#13930 = CARTESIAN_POINT ( 'NONE',  ( 19.35628570429999940, 1496.398810548190113, 218.7515486585290034 ) ) ;
#13931 = EDGE_CURVE ( 'NONE', #109119, #21788, #76219, .T. ) ;
#13932 = DIRECTION ( 'NONE',  ( 0.8672669759446689497, 0.000000000000000000, 0.4978433412588633700 ) ) ;
#13933 = CARTESIAN_POINT ( 'NONE',  ( -5.788691363644999477, 1517.157901477309906, 207.9987443536870160 ) ) ;
#13934 = CIRCLE ( 'NONE', #4996, 12.73448142120000171 ) ;
#13935 = CARTESIAN_POINT ( 'NONE',  ( -15.26161778761860077, 1417.220034897830146, 226.9233734088860217 ) ) ;
#13936 = CARTESIAN_POINT ( 'NONE',  ( 1.303375595325469982, 1408.418417958420150, 222.6667617130129884 ) ) ;
#13937 = CARTESIAN_POINT ( 'NONE',  ( -13.17087381283750069, 1434.856356709339934, 149.0413483970049811 ) ) ;
#13938 = CARTESIAN_POINT ( 'NONE',  ( -3.262203552877475765, 1455.259740959270175, 200.2677761270983297 ) ) ;
#13939 = CARTESIAN_POINT ( 'NONE',  ( -1.132427485120000064E-14, 1421.588970873729977, 90.97065375769790307 ) ) ;
#13940 = CARTESIAN_POINT ( 'NONE',  ( 7.231911623789289756, 1424.971209983940071, 212.7891681502780159 ) ) ;
#13941 = ORIENTED_EDGE ( 'NONE', *, *, #53555, .F. ) ;
#13942 = CARTESIAN_POINT ( 'NONE',  ( 36.81312681149999833, 1438.597774589839901, 254.5659337911980060 ) ) ;
#13943 = CARTESIAN_POINT ( 'NONE',  ( -26.66930585420000099, 1508.126733771030104, 202.3624711673980130 ) ) ;
#13945 = CARTESIAN_POINT ( 'NONE',  ( 28.15443155984639745, 1509.896245780209938, 217.4026704617729990 ) ) ;
#13944 = CARTESIAN_POINT ( 'NONE',  ( -2.534380535060000383, 1489.036591809629954, 181.6187424111979851 ) ) ;
#13946 = CARTESIAN_POINT ( 'NONE',  ( 1.454856650999370338, 1507.661996469931182, 181.0451578313067387 ) ) ;
#13947 = CARTESIAN_POINT ( 'NONE',  ( -2.499803828369999546E-09, 1418.297051470129873, 231.7760247027979972 ) ) ;
#13948 = CARTESIAN_POINT ( 'NONE',  ( -29.14950047876969563, 1509.937906416141459, 204.4881255053639109 ) ) ;
#13949 = ADVANCED_FACE ( 'NONE', ( #83676 ), #40577, .F. ) ;
#13950 = CARTESIAN_POINT ( 'NONE',  ( -15.09100122165660096, 1452.386071012250113, 147.7982250704480123 ) ) ;
#13951 = CARTESIAN_POINT ( 'NONE',  ( -18.64618908219999938, 1416.835809767629826, 208.5595418432099848 ) ) ;
#13952 = ORIENTED_EDGE ( 'NONE', *, *, #2554, .T. ) ;
#13953 = CARTESIAN_POINT ( 'NONE',  ( -107.8638321499309995, 1378.913060387349788, 300.1214876574690607 ) ) ;
#13954 = CARTESIAN_POINT ( 'NONE',  ( 16.66936639838844059, 1523.456924617337791, 237.7608804993615479 ) ) ;
#13955 = CARTESIAN_POINT ( 'NONE',  ( -0.04733364164779999689, 1508.924981715130116, 238.6962721304979880 ) ) ;
#13956 = CARTESIAN_POINT ( 'NONE',  ( 10.94703604719999923, 1501.632067650890122, 205.7462135331290085 ) ) ;
#13957 = EDGE_LOOP ( 'NONE', ( #67593, #35701, #36155, #30049 ) ) ;
#13958 = EDGE_LOOP ( 'NONE', ( #32359, #16684, #51628, #19888 ) ) ;
#13959 = AXIS2_PLACEMENT_3D ( 'NONE', #98850, #90996, #59082 ) ;
#13960 = CARTESIAN_POINT ( 'NONE',  ( 2.902343876856320115, 1466.632250330839952, 234.1422825383600070 ) ) ;
#13961 = CARTESIAN_POINT ( 'NONE',  ( -24.05637053410000092, 1410.857966063630101, 209.5800563058490127 ) ) ;
#13962 = EDGE_CURVE ( 'NONE', #31336, #714, #104390, .T. ) ;
#13963 = ORIENTED_EDGE ( 'NONE', *, *, #31840, .T. ) ;
#13964 = CARTESIAN_POINT ( 'NONE',  ( 3.487587063703020185, 1509.038630936360050, 204.6345965708119934 ) ) ;
#13965 = CARTESIAN_POINT ( 'NONE',  ( 7.557982130680000132, 1491.185578662290027, 210.9716881467189751 ) ) ;
#13966 = AXIS2_PLACEMENT_3D ( 'NONE', #29770, #45511, #96998 ) ;
#13967 = AXIS2_PLACEMENT_3D ( 'NONE', #31394, #65574, #82902 ) ;
#13968 = ADVANCED_FACE ( 'NONE', ( #40026 ), #51737, .F. ) ;
#13969 = CARTESIAN_POINT ( 'NONE',  ( -6.824245157110000015, 1498.345970854529924, 235.3115248808979914 ) ) ;
#13970 = CARTESIAN_POINT ( 'NONE',  ( 5.496544696010749576, 1440.579441483889923, 154.7743156854139954 ) ) ;
#13971 = AXIS2_PLACEMENT_3D ( 'NONE', #102400, #26242, #49822 ) ;
#13972 = CARTESIAN_POINT ( 'NONE',  ( 45.23156575188859563, 1448.572260723799900, 267.6264533449969463 ) ) ;
#13973 = CARTESIAN_POINT ( 'NONE',  ( -11.22084002886469989, 1414.913060387399810, 220.6193154192710040 ) ) ;
#13974 = CARTESIAN_POINT ( 'NONE',  ( 0.08742462538030000563, 1420.450111770730018, 182.6858894113979943 ) ) ;
#13975 = CARTESIAN_POINT ( 'NONE',  ( 7.323034273964999841, 1516.609912606490070, 205.6670971239069843 ) ) ;
#13976 = ORIENTED_EDGE ( 'NONE', *, *, #14442, .T. ) ;
#13977 = CARTESIAN_POINT ( 'NONE',  ( -12.01638156518240130, 1440.881463477919851, 187.8051726210379968 ) ) ;
#13978 = CARTESIAN_POINT ( 'NONE',  ( 13.24072114446620496, 1443.163570684924025, 187.6152391747091599 ) ) ;
#13979 = ORIENTED_EDGE ( 'NONE', *, *, #55066, .T. ) ;
#13980 = ORIENTED_EDGE ( 'NONE', *, *, #100225, .F. ) ;
#13981 = DIRECTION ( 'NONE',  ( 0.03489949670246857150, 0.9993908270190969834, 0.000000000000000000 ) ) ;
#13982 = FACE_OUTER_BOUND ( 'NONE', #43509, .T. ) ;
#13983 = CARTESIAN_POINT ( 'NONE',  ( -13.89676593410340111, 1513.004579589629884, 193.8317604122359796 ) ) ;
#13984 = CARTESIAN_POINT ( 'NONE',  ( 0.2432393513109950001, 1452.904566282009910, 152.5224177206319780 ) ) ;
#13985 = CARTESIAN_POINT ( 'NONE',  ( 0.4721006504984889829, 1410.034462268999960, 269.8654312524320176 ) ) ;
#13986 = ADVANCED_FACE ( 'NONE', ( #67461 ), #34389, .F. ) ;
#13987 = CARTESIAN_POINT ( 'NONE',  ( 19.33082836830000062, 1455.567049562989951, 210.0625852571630219 ) ) ;
#13988 = CARTESIAN_POINT ( 'NONE',  ( 19.03616775833818409, 1456.571930367182176, 225.7629732080275176 ) ) ;
#13989 = CARTESIAN_POINT ( 'NONE',  ( -9.783936618240000271, 1438.409968277489952, 210.7790527803989846 ) ) ;
#13990 = CARTESIAN_POINT ( 'NONE',  ( 0.03346608192457139336, 1410.062748283369501, 233.1925408425690875 ) ) ;
#13992 = FACE_OUTER_BOUND ( 'NONE', #98910, .T. ) ;
#13991 = CARTESIAN_POINT ( 'NONE',  ( -13.53570968906610084, 1434.951797543509883, 148.7640763676990048 ) ) ;
#13993 = CARTESIAN_POINT ( 'NONE',  ( 12.11307097544860056, 1426.902643091930031, 206.5905068478429882 ) ) ;
#13994 = AXIS2_PLACEMENT_3D ( 'NONE', #69347, #69908, #1584 ) ;
#13995 = CARTESIAN_POINT ( 'NONE',  ( -9.810612324704180764, 1440.011860597360055, 207.1182720801899961 ) ) ;
#13996 = EDGE_CURVE ( 'NONE', #36754, #29937, #105326, .T. ) ;
#13997 = CARTESIAN_POINT ( 'NONE',  ( 2.416798835000000256, 1426.601114010129777, 146.0361887655980127 ) ) ;
#13998 = ORIENTED_EDGE ( 'NONE', *, *, #86486, .T. ) ;
#13999 = CARTESIAN_POINT ( 'NONE',  ( 8.968032268709999144, 1477.614756788489785, 227.8520689727990032 ) ) ;
#14000 = CARTESIAN_POINT ( 'NONE',  ( 4.500000000000000000, 1439.615672362369878, 127.8666744532979891 ) ) ;
#14001 = CARTESIAN_POINT ( 'NONE',  ( -92.83937824579700759, 1384.962964213820214, 309.5464475911989553 ) ) ;
#14002 = CARTESIAN_POINT ( 'NONE',  ( -8.865249977160001293, 1387.451792102280024, 200.3692866900990168 ) ) ;
#14003 = CARTESIAN_POINT ( 'NONE',  ( 9.362196585121042247, 1423.087187200049812, 210.9628769778060189 ) ) ;
#14005 = ORIENTED_EDGE ( 'NONE', *, *, #3506, .F. ) ;
#14004 = CARTESIAN_POINT ( 'NONE',  ( 11.21861042134139907, 1425.044613964269956, 203.0203497653440081 ) ) ;
#14006 = CARTESIAN_POINT ( 'NONE',  ( 3.789103669029999732, 1428.956962167089841, 216.4960976464589919 ) ) ;
#14007 = CARTESIAN_POINT ( 'NONE',  ( 16.48231778833692118, 1525.661275128775515, 236.6690309048151732 ) ) ;
#14008 = CARTESIAN_POINT ( 'NONE',  ( -14.35483103309999819, 1416.837177090929799, 221.5788728750979999 ) ) ;
#14009 = LINE ( 'NONE', #56039, #25337 ) ;
#14010 = CARTESIAN_POINT ( 'NONE',  ( 9.327651199099038948, 1434.415569083649871, 206.2244204008570136 ) ) ;
#14011 = DIRECTION ( 'NONE',  ( -0.8672669759446595128, 0.000000000000000000, 0.4978433412588795237 ) ) ;
#14012 = CARTESIAN_POINT ( 'NONE',  ( 5.291552456182019526, 1457.527819738830203, 199.7187647539589932 ) ) ;
#14013 = CARTESIAN_POINT ( 'NONE',  ( -106.6863336295694040, 1390.802642226108446, 300.1531170756869074 ) ) ;
#14014 = CARTESIAN_POINT ( 'NONE',  ( 9.464617871280001538, 1422.096644224830015, 230.5969590778979921 ) ) ;
#14015 = CARTESIAN_POINT ( 'NONE',  ( -32.39800393421789693, 1524.816548299036867, 201.1912629570496733 ) ) ;
#14016 = FACE_OUTER_BOUND ( 'NONE', #57925, .T. ) ;
#14017 = CARTESIAN_POINT ( 'NONE',  ( 18.26532265589999682, 1415.628674266529742, 209.8910850646770143 ) ) ;
#14018 = CARTESIAN_POINT ( 'NONE',  ( -3.703568358935259930, 1497.311626042180023, 220.9591690318370070 ) ) ;
#14019 = CARTESIAN_POINT ( 'NONE',  ( -0.5647852981080000445, 1422.358767625429891, 228.0117178583979864 ) ) ;
#14020 = CARTESIAN_POINT ( 'NONE',  ( -25.74151704639999849, 1448.987115190519944, 137.5013012925980149 ) ) ;
#14021 = DIRECTION ( 'NONE',  ( -0.2054769195713179730, -0.000000000000000000, -0.9786619618251657382 ) ) ;
#14022 = CARTESIAN_POINT ( 'NONE',  ( 0.7322251555290010261, 1515.253704548189944, 204.7973436813889805 ) ) ;
#14023 = DIRECTION ( 'NONE',  ( 5.980589973904019347E-17, -1.000000000000000000, 1.736889445713099699E-16 ) ) ;
#14024 = DIRECTION ( 'NONE',  ( 0.1070030146457371656, 0.000000000000000000, 0.9942586961433751425 ) ) ;
#14025 = CARTESIAN_POINT ( 'NONE',  ( -1.523411567629999963, 1416.219761280829971, 227.9399405097980207 ) ) ;
#14026 = CARTESIAN_POINT ( 'NONE',  ( -113.4000000000000057, 1377.913060387289988, 304.2218459572590064 ) ) ;
#14027 = CARTESIAN_POINT ( 'NONE',  ( -13.49752382283059937, 1408.354313590640004, 207.9364978486700295 ) ) ;
#14028 = CARTESIAN_POINT ( 'NONE',  ( -14.59411311879999928, 1414.913060387329779, 201.4749348725179914 ) ) ;
#14029 = DIRECTION ( 'NONE',  ( 0.000000000000000000, 1.000000000000000000, 0.000000000000000000 ) ) ;
#14030 = CARTESIAN_POINT ( 'NONE',  ( 13.80526003289999970, 1434.979593547039940, 149.1900205729979803 ) ) ;
#14031 = CARTESIAN_POINT ( 'NONE',  ( -26.81574567050000013, 1435.910853872800089, 136.5210682332980241 ) ) ;
#14032 = CARTESIAN_POINT ( 'NONE',  ( -0.7433232216159980643, 1450.780014651390047, 189.8792753856990032 ) ) ;
#14033 = VERTEX_POINT ( 'NONE', #25962 ) ;
#14034 = CARTESIAN_POINT ( 'NONE',  ( -16.48400375142206897, 1525.790287071779403, 181.7637264533375685 ) ) ;
#14035 = B_SPLINE_CURVE_WITH_KNOTS ( 'NONE', 5,
 ( #36096, #80301, #70836, #104946, #88709, #44498 ),
 .UNSPECIFIED., .F., .F.,
 ( 6, 6 ),
 ( 0.000000000000000000, 1.000000000000000000 ),
 .UNSPECIFIED. ) ;
#14036 = CARTESIAN_POINT ( 'NONE',  ( 5.085252852200000007, 1478.772695843590100, 199.8786784519290052 ) ) ;
#14037 = CARTESIAN_POINT ( 'NONE',  ( -105.0307287566989061, 1380.923348513794508, 308.4048763095673280 ) ) ;
#14038 = CARTESIAN_POINT ( 'NONE',  ( -11.81643738809999888, 1490.595564134589722, 209.0680961509349913 ) ) ;
#14039 = DIRECTION ( 'NONE',  ( 0.9125304618754024322, 0.000000000000000000, -0.4090087482554191078 ) ) ;
#14040 = DIRECTION ( 'NONE',  ( 0.5877852522924807976, 0.000000000000000000, 0.8090169943749417891 ) ) ;
#14041 = CARTESIAN_POINT ( 'NONE',  ( 31.03490941718551710, 1415.854366402851610, 269.3355724915077190 ) ) ;
#14042 = AXIS2_PLACEMENT_3D ( 'NONE', #108566, #14493, #15034 ) ;
#14043 = CARTESIAN_POINT ( 'NONE',  ( -20.01067139950000140, 1507.877425041529932, 188.9709217985979706 ) ) ;
#14044 = CARTESIAN_POINT ( 'NONE',  ( 21.39771952614790251, 1509.704955107219803, 188.4542851670070149 ) ) ;
#14045 = CARTESIAN_POINT ( 'NONE',  ( 3.421433458210000111, 1428.746990730030120, 185.0224803175979957 ) ) ;
#14046 = CARTESIAN_POINT ( 'NONE',  ( -61.65894565632150659, 1385.069567178810075, 247.6034208562279844 ) ) ;
#14047 = CARTESIAN_POINT ( 'NONE',  ( -18.72690275718909092, 1526.278758871498894, 236.1309272327495421 ) ) ;
#14048 = CARTESIAN_POINT ( 'NONE',  ( -4.849688736979540060, 1508.551704408389924, 205.8172135933860147 ) ) ;
#14049 = AXIS2_PLACEMENT_3D ( 'NONE', #64050, #98168, #21440 ) ;
#14050 = CARTESIAN_POINT ( 'NONE',  ( -29.15335221010520073, 1509.735908701399921, 208.6618227458789931 ) ) ;
#14051 = CARTESIAN_POINT ( 'NONE',  ( -16.03581849651680002, 1409.473033727780148, 225.1836456777660089 ) ) ;
#14053 = ORIENTED_EDGE ( 'NONE', *, *, #38006, .F. ) ;
#14052 = CARTESIAN_POINT ( 'NONE',  ( 3.048018904480000124, 1501.579531795289995, 230.2806870085990170 ) ) ;
#14054 = CARTESIAN_POINT ( 'NONE',  ( -109.9849080340000000, 1384.910086089010065, 311.4561084402590154 ) ) ;
#14055 = CONICAL_SURFACE ( 'NONE', #12297, 1.000000000000005773, 0.7853981633970000820 ) ;
#14056 = CARTESIAN_POINT ( 'NONE',  ( 10.91646513216940129, 1471.120537862260107, 210.1608033267570192 ) ) ;
#14057 =( BOUNDED_CURVE ( )  B_SPLINE_CURVE ( 3, ( #40790, #110749, #25067, #101776 ),
 .UNSPECIFIED., .F., .F. ) 
 B_SPLINE_CURVE_WITH_KNOTS ( ( 4, 4 ),
 ( 4.424456909735084764, 5.579818660943519859 ),
 .UNSPECIFIED. ) 
 CURVE ( )  GEOMETRIC_REPRESENTATION_ITEM ( )  RATIONAL_B_SPLINE_CURVE ( ( 1.000000000000000000, 0.8918208900458772792, 0.8918208900458772792, 1.000000000000000000 ) ) 
 REPRESENTATION_ITEM ( '' )  );
#14058 = CARTESIAN_POINT ( 'NONE',  ( 2.446787376320000096, 1432.353341358199941, 150.2884730787980061 ) ) ;
#14059 = CARTESIAN_POINT ( 'NONE',  ( -109.9861441850000006, 1384.675965057090025, 311.4500065002590077 ) ) ;
#14060 = CARTESIAN_POINT ( 'NONE',  ( -0.07455736060109920127, 1420.122296152110039, 183.7971148460100039 ) ) ;
#14061 = CARTESIAN_POINT ( 'NONE',  ( 1.600823151459999982, 1464.924551132029819, 236.5189088668979878 ) ) ;
#14062 = CARTESIAN_POINT ( 'NONE',  ( 22.37934482829999894, 1410.615956673830169, 215.1176883408980132 ) ) ;
#14063 = CARTESIAN_POINT ( 'NONE',  ( -1.801360752315949831, 1412.633430038469896, 185.9483006541370003 ) ) ;
#14064 = CARTESIAN_POINT ( 'NONE',  ( -9.541049972259999734, 1464.842190924689930, 228.2655280639989996 ) ) ;
#14065 = CARTESIAN_POINT ( 'NONE',  ( -17.58613261789999882, 1424.135132543530062, 227.0015458978980121 ) ) ;
#14067 = CARTESIAN_POINT ( 'NONE',  ( 8.272555700608019129E-16, 1374.413060387289988, 209.1218459616989946 ) ) ;
#14066 = DIRECTION ( 'NONE',  ( -9.520246157234046601E-08, 3.411689477181459810E-09, 0.9999999999999954481 ) ) ;
#14068 = CARTESIAN_POINT ( 'NONE',  ( 25.80251995263579801, 1449.911705404210124, 208.7286070993190208 ) ) ;
#14069 = CARTESIAN_POINT ( 'NONE',  ( -113.4000000000000057, 1358.631207110790001, 297.2777708435189652 ) ) ;
#14070 = DIRECTION ( 'NONE',  ( -0.6736849260863841948, 0.000000000000000000, 0.7390186874254148774 ) ) ;
#14071 = CARTESIAN_POINT ( 'NONE',  ( 0.000000000000000000, 1512.187213306747481, 209.1218459616979999 ) ) ;
#14072 = CARTESIAN_POINT ( 'NONE',  ( -5.369546485720880113, 1374.928881103789990, 203.3687134724160046 ) ) ;
#14073 = CARTESIAN_POINT ( 'NONE',  ( 1.119717716265000051, 1517.038650117239968, 205.6590103047369951 ) ) ;
#14074 = AXIS2_PLACEMENT_3D ( 'NONE', #80508, #36840, #11640 ) ;
#14075 = CARTESIAN_POINT ( 'NONE',  ( -17.67465541829999864, 1423.538376080030048, 226.2965632852980207 ) ) ;
#14076 = ORIENTED_EDGE ( 'NONE', *, *, #96093, .F. ) ;
#14077 = CARTESIAN_POINT ( 'NONE',  ( 14.57021081669999951, 1474.586296236829867, 224.5225414627979887 ) ) ;
#14078 = CARTESIAN_POINT ( 'NONE',  ( -4.221396571449520074, 1441.605459665790022, 169.0259831405610100 ) ) ;
#14080 = EDGE_LOOP ( 'NONE', ( #57181, #8333, #72917, #4343, #107975 ) ) ;
#14079 = CARTESIAN_POINT ( 'NONE',  ( -67.82383404051370235, 1379.746049001880010, 279.2023482137329893 ) ) ;
#14081 = ORIENTED_EDGE ( 'NONE', *, *, #78951, .T. ) ;
#14082 = CARTESIAN_POINT ( 'NONE',  ( -9.881278461464678031, 1379.739605549548514, 216.5635243919133188 ) ) ;
#14083 = EDGE_LOOP ( 'NONE', ( #10847, #85734, #31084, #47666 ) ) ;
#14084 = CARTESIAN_POINT ( 'NONE',  ( 4.084250103052634806, 1507.178795293708163, 181.6747635981337510 ) ) ;
#14085 = CARTESIAN_POINT ( 'NONE',  ( 11.85459489379999987, 1500.917690086590255, 208.6046474440059910 ) ) ;
#14087 = CARTESIAN_POINT ( 'NONE',  ( 15.76856008000959974, 1410.855127137190038, 191.5168014226029811 ) ) ;
#14086 = CARTESIAN_POINT ( 'NONE',  ( -11.64111738558995235, 1425.862200434439728, 144.4792545450150385 ) ) ;
#14088 = CARTESIAN_POINT ( 'NONE',  ( -3.253301419385000504, 1516.790374942449944, 210.2573062871869922 ) ) ;
#14089 = EDGE_CURVE ( 'NONE', #89963, #1678, #57604, .T. ) ;
#14090 = CARTESIAN_POINT ( 'NONE',  ( -106.2140063875329901, 1378.913060387799987, 305.8740827694030031 ) ) ;
#14091 = DIRECTION ( 'NONE',  ( -0.000000000000000000, -1.000000000000000000, -0.000000000000000000 ) ) ;
#14093 = ADVANCED_FACE ( 'NONE', ( #76953 ), #51192, .T. ) ;
#14092 = CARTESIAN_POINT ( 'NONE',  ( 7.192202089616840155, 1484.368469734710061, 217.2056949635710055 ) ) ;
#14094 = APPLICATION_PROTOCOL_DEFINITION ( 'draft international standard', 'automotive_design', 1998, #57061 ) ;
#14095 = CARTESIAN_POINT ( 'NONE',  ( 35.14989576411770145, 1451.591923343930148, 134.0999999983660018 ) ) ;
#14096 = CARTESIAN_POINT ( 'NONE',  ( -40.23150629975690151, 1442.858491698010084, 137.0288987757270149 ) ) ;
#14097 = CARTESIAN_POINT ( 'NONE',  ( -22.15968245387939817, 1485.573395578509917, 217.2083751193320040 ) ) ;
#14098 = CARTESIAN_POINT ( 'NONE',  ( -1.150312585214009919, 1431.780365134439990, 200.7950712129770068 ) ) ;
#14099 = ORIENTED_EDGE ( 'NONE', *, *, #44566, .F. ) ;
#14100 = ORIENTED_EDGE ( 'NONE', *, *, #45484, .F. ) ;
#14101 = CARTESIAN_POINT ( 'NONE',  ( 15.03292567439081040, 1410.810032661595415, 227.4772455420474842 ) ) ;
#14102 = CARTESIAN_POINT ( 'NONE',  ( 31.12456774391177206, 1525.960063244516959, 217.0912716842394730 ) ) ;
#14103 = CARTESIAN_POINT ( 'NONE',  ( -0.01304308391829999900, 1452.999749671330164, 183.2385070535979708 ) ) ;
#14104 = CARTESIAN_POINT ( 'NONE',  ( -3.151745281339999760, 1484.261526075930078, 183.3481135453979789 ) ) ;
#14105 = CARTESIAN_POINT ( 'NONE',  ( -2.500000000000000000, 1439.579545607999989, 165.8618564662860138 ) ) ;
#14106 = VECTOR ( 'NONE', #52320, 1000.000000000000000 ) ;
#14107 = CARTESIAN_POINT ( 'NONE',  ( -41.48252422893380498, 1444.135613197089924, 136.5500652606600056 ) ) ;
#14108 = EDGE_CURVE ( 'NONE', #98226, #108494, #1667, .T. ) ;
#14109 = CARTESIAN_POINT ( 'NONE',  ( 12.63295115314390848, 1420.317390383416978, 200.3640917624317410 ) ) ;
#14110 = CARTESIAN_POINT ( 'NONE',  ( -9856.831406432045696, 2833.746317950422963, 1378.242121024269181 ) ) ;
#14111 = FACE_OUTER_BOUND ( 'NONE', #42625, .T. ) ;
#14112 = FACE_OUTER_BOUND ( 'NONE', #90102, .T. ) ;
#14113 = CARTESIAN_POINT ( 'NONE',  ( -76.07930854709739776, 1384.773566694879946, 277.2872448374639589 ) ) ;
#14114 = ORIENTED_EDGE ( 'NONE', *, *, #76651, .F. ) ;
#14115 = DIRECTION ( 'NONE',  ( 1.755985294532464991E-16, -1.000000000000000000, 1.338183447452830017E-16 ) ) ;
#14116 = CARTESIAN_POINT ( 'NONE',  ( -7.339749373344999661, 1517.224900789629828, 207.4124613591469881 ) ) ;
#14117 = ORIENTED_EDGE ( 'NONE', *, *, #4240, .F. ) ;
#14118 = CARTESIAN_POINT ( 'NONE',  ( 38.27236334520110006, 1440.913060387330006, 265.3011690063839865 ) ) ;
#14119 = AXIS2_PLACEMENT_3D ( 'NONE', #44820, #54328, #103595 ) ;
#14120 = CARTESIAN_POINT ( 'NONE',  ( -0.0002251272801281111791, 1452.162349662644374, 153.8758817369695464 ) ) ;
#14121 = ORIENTED_EDGE ( 'NONE', *, *, #103630, .T. ) ;
#14122 = AXIS2_PLACEMENT_3D ( 'NONE', #104679, #70013, #1138 ) ;
#14123 = CARTESIAN_POINT ( 'NONE',  ( -0.1792353353211550149, 1451.688816654250104, 183.0380716929619780 ) ) ;
#14124 = CARTESIAN_POINT ( 'NONE',  ( -16.66095200220000194, 1410.867389019930215, 191.7375190235979971 ) ) ;
#14125 = CARTESIAN_POINT ( 'NONE',  ( -17.71193101166619854, 1521.951704408389787, 221.5709757775249784 ) ) ;
#14126 = CARTESIAN_POINT ( 'NONE',  ( -10.52899351214830048, 1462.479394878560015, 207.9464375330440191 ) ) ;
#14127 = CARTESIAN_POINT ( 'NONE',  ( -13.11134949370000058, 1419.893956787529987, 222.0035429825979918 ) ) ;
#14128 = CARTESIAN_POINT ( 'NONE',  ( -20.17495577355367686, 1508.361608974187902, 228.9114165637121232 ) ) ;
#14129 = CARTESIAN_POINT ( 'NONE',  ( -1.469541472189999975, 1508.190586172730036, 180.6206999101979989 ) ) ;
#14130 = CARTESIAN_POINT ( 'NONE',  ( -6.372167638625000130, 1511.069621805459974, 201.7253008890070021 ) ) ;
#14131 = CARTESIAN_POINT ( 'NONE',  ( -21.86721050905450525, 1523.611961620354123, 183.2036325349451715 ) ) ;
#14133 = FACE_OUTER_BOUND ( 'NONE', #71585, .T. ) ;
#14132 = CARTESIAN_POINT ( 'NONE',  ( 15.64891445259999969, 1459.656115944430212, 231.4809545682979888 ) ) ;
#14134 = LINE ( 'NONE', #83008, #871 ) ;
#14135 = AXIS2_PLACEMENT_3D ( 'NONE', #100961, #67959, #68506 ) ;
#14136 = EDGE_CURVE ( 'NONE', #97990, #109192, #60157, .T. ) ;
#14137 = CARTESIAN_POINT ( 'NONE',  ( 1.708720984574999768, 1516.531533746980131, 216.4430152012269843 ) ) ;
#14138 = VERTEX_POINT ( 'NONE', #804 ) ;
#14139 = CIRCLE ( 'NONE', #76730, 26.43993992909998525 ) ;
#14140 = DIRECTION ( 'NONE',  ( -1.755985294532469921E-16, 1.000000000000000000, -1.338183447452831989E-16 ) ) ;
#14141 = CARTESIAN_POINT ( 'NONE',  ( -0.1362281291136649974, 1507.781361289090000, 180.7563895008119914 ) ) ;
#14142 = CIRCLE ( 'NONE', #69667, 2.000000000000003553 ) ;
#14143 = CARTESIAN_POINT ( 'NONE',  ( 31.32995031131198616, 1523.678648413191695, 221.9013357025044115 ) ) ;
#14144 = CARTESIAN_POINT ( 'NONE',  ( -0.7356989727169980231, 1517.020847257979995, 212.5827121409169820 ) ) ;
#14145 = CARTESIAN_POINT ( 'NONE',  ( 3.982959079218740595, 1515.551843419029865, 211.9714081247090292 ) ) ;
#14146 = EDGE_CURVE ( 'NONE', #64548, #98856, #1462, .T. ) ;
#14147 = CARTESIAN_POINT ( 'NONE',  ( 4.283856666023710069, 1440.956247486469920, 155.9231014612180104 ) ) ;
#14149 = ORIENTED_EDGE ( 'NONE', *, *, #108567, .F. ) ;
#14148 = CARTESIAN_POINT ( 'NONE',  ( 3.487584963647319736, 1508.551704408610021, 213.9544597577999809 ) ) ;
#14150 = CARTESIAN_POINT ( 'NONE',  ( -1.338895077078837259, 1526.382868172864164, 178.6697305272290635 ) ) ;
#14151 = B_SPLINE_CURVE_WITH_KNOTS ( 'NONE', 5,
 ( #51995, #86136, #104037, #93973, #1599, #35736 ),
 .UNSPECIFIED., .F., .F.,
 ( 6, 6 ),
 ( -14.36013212639999992, -6.500205904970000503 ),
 .UNSPECIFIED. ) ;
#14152 = CARTESIAN_POINT ( 'NONE',  ( 7.894399719279999950, 1460.747930716730025, 221.5712129898979867 ) ) ;
#14153 = CARTESIAN_POINT ( 'NONE',  ( -11.27444857399999911, 1430.307468795130035, 151.2292110278980033 ) ) ;
#14154 = CARTESIAN_POINT ( 'NONE',  ( -2.586254842240000240, 1431.686802674690171, 214.1917715254589893 ) ) ;
#14155 = CARTESIAN_POINT ( 'NONE',  ( -6.058566992285000730, 1440.303333100529926, 202.7033299732119929 ) ) ;
#14156 = CARTESIAN_POINT ( 'NONE',  ( 6.384249653904870314, 1425.832381260119973, 153.2928915029530117 ) ) ;
#14157 = CARTESIAN_POINT ( 'NONE',  ( -21.25167763996070036, 1489.809143648679992, 209.5009534265659852 ) ) ;
#14158 = CARTESIAN_POINT ( 'NONE',  ( 12.50628814030000058, 1446.659047563680133, 188.2618572318980057 ) ) ;
#14160 = CARTESIAN_POINT ( 'NONE',  ( -11.57364750537059805, 1482.638710595820157, 206.3005749242109914 ) ) ;
#14159 = CARTESIAN_POINT ( 'NONE',  ( -24.63752222140000114, 1457.439077831530085, 211.8173745106979879 ) ) ;
#14161 = CARTESIAN_POINT ( 'NONE',  ( -1.518145821790000127, 1484.332293859730044, 182.5346457296979850 ) ) ;
#14162 = AXIS2_PLACEMENT_3D ( 'NONE', #37837, #105040, #79846 ) ;
#14163 = ORIENTED_EDGE ( 'NONE', *, *, #103365, .T. ) ;
#14164 = CARTESIAN_POINT ( 'NONE',  ( 7.323974606304999746, 1516.647924054489977, 205.0857262875869935 ) ) ;
#14165 = CARTESIAN_POINT ( 'NONE',  ( 6.208817084409999687, 1406.025614260530119, 267.8376454021980066 ) ) ;
#14166 = CARTESIAN_POINT ( 'NONE',  ( 0.4274135159440000109, 1409.096031525230046, 185.6227926432979984 ) ) ;
#14167 = CARTESIAN_POINT ( 'NONE',  ( 18.09099147780000294, 1410.879528734529913, 193.6270419906979896 ) ) ;
#14168 = CARTESIAN_POINT ( 'NONE',  ( 22.92656223559736262, 1432.082429570070190, 216.2522404191055614 ) ) ;
#14169 = CARTESIAN_POINT ( 'NONE',  ( 2.983564572711930651, 1464.490552568307066, 199.7433000633449467 ) ) ;
#14170 = CARTESIAN_POINT ( 'NONE',  ( -1.466750842539999988, 1450.866641565780128, 183.4132864747979852 ) ) ;
#14171 = CARTESIAN_POINT ( 'NONE',  ( -10.15733737953619986, 1447.239609962909981, 211.0279899296229758 ) ) ;
#14172 = CARTESIAN_POINT ( 'NONE',  ( -2.500094832422949942, 1448.919094719029999, 155.0643300295350002 ) ) ;
#14173 = CARTESIAN_POINT ( 'NONE',  ( -1.635975655120868177, 1451.617099953195975, 184.0322519377451727 ) ) ;
#14174 = CARTESIAN_POINT ( 'NONE',  ( 0.5697989934050000649, 1450.893162568020216, 155.6080914337979948 ) ) ;
#14175 = CARTESIAN_POINT ( 'NONE',  ( -14.45145579027879990, 1416.702560754940123, 221.3854044765280094 ) ) ;
#14176 = CARTESIAN_POINT ( 'NONE',  ( -11.02815901449999991, 1500.365335154690001, 213.0134302711989847 ) ) ;
#14177 = CARTESIAN_POINT ( 'NONE',  ( -1.221245327089999926E-15, 1427.913060387330006, 209.1218459616979999 ) ) ;
#14178 = CARTESIAN_POINT ( 'NONE',  ( -27.01737277763200140, 1507.999902240279880, 211.4327103027169983 ) ) ;
#14179 = B_SPLINE_CURVE_WITH_KNOTS ( 'NONE', 3,
 ( #87742, #11020, #62566, #65297 ),
 .UNSPECIFIED., .F., .F.,
 ( 4, 4 ),
 ( 7.312299096839999457, 15.60583060000000089 ),
 .UNSPECIFIED. ) ;
#14180 = CARTESIAN_POINT ( 'NONE',  ( 3.137342596209999890, 1440.799554483159909, 158.1457359887980090 ) ) ;
#14181 = CARTESIAN_POINT ( 'NONE',  ( -4.953282586809999444, 1475.369567567530112, 269.2856847212980256 ) ) ;
#14182 = CARTESIAN_POINT ( 'NONE',  ( -10.86003582634030806, 1424.791813296290229, 138.1872773544496624 ) ) ;
#14183 = CARTESIAN_POINT ( 'NONE',  ( 15.90990255763500016, 1513.492015765619954, 198.1616908427670296 ) ) ;
#14184 = CARTESIAN_POINT ( 'NONE',  ( 17.71073067720600136, 1414.282064044829895, 224.0326197095010059 ) ) ;
#14185 = CARTESIAN_POINT ( 'NONE',  ( -57.94140768939789865, 1384.704083737000019, 277.3428793058350266 ) ) ;
#14186 = CARTESIAN_POINT ( 'NONE',  ( -12.39573405564622988, 1517.151704408390060, 199.6750929870061668 ) ) ;
#14187 = CARTESIAN_POINT ( 'NONE',  ( -3.793220392315020284, 1517.051709179979980, 215.8229393325320018 ) ) ;
#14188 = B_SPLINE_SURFACE_WITH_KNOTS ( 'NONE', 5, 5, ( 
 ( #105786, #38550, #38017, #106317, #78932, #21173 ),
 ( #11710, #104663, #89512, #71100, #12803, #37464 ),
 ( #46983, #105224, #62142, #96268, #45882, #20100 ),
 ( #81107, #72728, #106853, #30144, #27959, #11177 ),
 ( #19545, #53753, #3340, #87886, #79477, #80019 ),
 ( #74395, #82207, #66552, #109090, #90609, #5512 ) ),
 .UNSPECIFIED., .F., .F., .F.,
 ( 6, 6 ),
 ( 6, 6 ),
 ( 7.548574938123289613, 12.57628284734769863 ),
 ( 0.000000000000000000, 0.5000183579477079920 ),
 .UNSPECIFIED. ) ;
#14189 = CARTESIAN_POINT ( 'NONE',  ( -105.8044893139999942, 1378.913060387289988, 303.5347832593589601 ) ) ;
#14190 = CARTESIAN_POINT ( 'NONE',  ( 31.56778878607238781, 1525.408337840050308, 216.2063969590453496 ) ) ;
#14191 = CARTESIAN_POINT ( 'NONE',  ( 7.895892558453802224, 1512.040964529616303, 206.1210073478832783 ) ) ;
#14192 = CARTESIAN_POINT ( 'NONE',  ( -21.90047919039999869, 1409.842284365829983, 203.3532602289579927 ) ) ;
#14193 = CARTESIAN_POINT ( 'NONE',  ( 12.84018448277500113, 1421.301739308270044, 205.5319240985589886 ) ) ;
#14194 = CARTESIAN_POINT ( 'NONE',  ( -42.76956658369999786, 1430.336806088530011, 269.7319452664979735 ) ) ;
#14195 = VERTEX_POINT ( 'NONE', #60726 ) ;
#14196 = B_SPLINE_SURFACE_WITH_KNOTS ( 'NONE', 5, 5, ( 
 ( #10618, #17317, #10052, #11181, #51512, #9500 ),
 ( #44786, #87323, #26860, #85644, #62146, #17877 ),
 ( #52074, #78936, #36358, #2789, #95718, #86207 ),
 ( #52626, #95170, #71104, #18983, #8944, #61047 ),
 ( #43665, #77817, #61585, #18426, #45343, #79482 ),
 ( #53180, #86763, #43117, #44226, #77277, #70549 ) ),
 .UNSPECIFIED., .F., .F., .F.,
 ( 6, 6 ),
 ( 6, 6 ),
 ( 0.000000000000000000, 2.079987011550000098 ),
 ( 0.000000000000000000, 2.000000000000000000 ),
 .UNSPECIFIED. ) ;
#14197 = CARTESIAN_POINT ( 'NONE',  ( -4.294703086410359916, 1410.439188197537533, 232.1146548671422067 ) ) ;
#14198 = CARTESIAN_POINT ( 'NONE',  ( -7.541469379549965879, 1510.554407340499438, 214.8833459881294345 ) ) ;
#14199 = CARTESIAN_POINT ( 'NONE',  ( 2.740685684163910008, 1426.136188963130053, 188.7843764270949976 ) ) ;
#14200 =( BOUNDED_CURVE ( )  B_SPLINE_CURVE ( 3, ( #12427, #46617, #104844, #90224 ),
 .UNSPECIFIED., .F., .T. ) 
 B_SPLINE_CURVE_WITH_KNOTS ( ( 4, 4 ),
 ( 4.712388980384689674, 6.283185307179586232 ),
 .UNSPECIFIED. ) 
 CURVE ( )  GEOMETRIC_REPRESENTATION_ITEM ( )  RATIONAL_B_SPLINE_CURVE ( ( 1.000000000000000000, 0.8047378541243649375, 0.8047378541243649375, 1.000000000000000000 ) ) 
 REPRESENTATION_ITEM ( '' )  );
#14202 = CARTESIAN_POINT ( 'NONE',  ( -12.22392939165850123, 1377.774275016259935, 210.6554241722059828 ) ) ;
#14201 = CARTESIAN_POINT ( 'NONE',  ( 11.15477939360000015, 1425.160653555029967, 144.1599692641979971 ) ) ;
#14203 = CARTESIAN_POINT ( 'NONE',  ( -8.881784197000000993E-16, 1392.213060387289943, 209.1218459616989946 ) ) ;
#14204 = AXIS2_PLACEMENT_3D ( 'NONE', #39833, #73996, #6222 ) ;
#14205 = DIRECTION ( 'NONE',  ( 0.000000000000000000, 0.000000000000000000, 1.000000000000000000 ) ) ;
#14206 = CARTESIAN_POINT ( 'NONE',  ( 28.03239352649999816, 1444.711964598699979, 137.4439080250980112 ) ) ;
#14207 = CARTESIAN_POINT ( 'NONE',  ( -5.005700239535000762, 1516.732530461250008, 202.1838802717869896 ) ) ;
#14208 = CARTESIAN_POINT ( 'NONE',  ( 7.666825005110000646, 1426.360134655189995, 212.0592671631690109 ) ) ;
#14209 = DIRECTION ( 'NONE',  ( -1.000000000000000000, 0.000000000000000000, -1.989566177384290042E-13 ) ) ;
#14210 = CARTESIAN_POINT ( 'NONE',  ( 15.91746618543499814, 1512.594959757389915, 198.1541272149669908 ) ) ;
#14211 = FACE_BOUND ( 'NONE', #11189, .T. ) ;
#14212 = CARTESIAN_POINT ( 'NONE',  ( -3.771520276690010220, 1379.037774784969997, 211.6703177581799764 ) ) ;
#14213 = AXIS2_PLACEMENT_3D ( 'NONE', #72876, #56624, #30300 ) ;
#14214 = CARTESIAN_POINT ( 'NONE',  ( 20.46625007539810071, 1507.818601948450123, 228.4183590306939777 ) ) ;
#14216 = ORIENTED_EDGE ( 'NONE', *, *, #52118, .F. ) ;
#14215 = CARTESIAN_POINT ( 'NONE',  ( -21.75077721616250059, 1379.626252247850061, 213.4816723946260026 ) ) ;
#14217 = ORIENTED_EDGE ( 'NONE', *, *, #26901, .T. ) ;
#14218 = CARTESIAN_POINT ( 'NONE',  ( -11.92220220670000153, 1397.363550527129746, 203.3627882915380098 ) ) ;
#14219 = CARTESIAN_POINT ( 'NONE',  ( -20.26547961730000225, 1410.542145032029794, 220.2212046400979943 ) ) ;
#14220 = CARTESIAN_POINT ( 'NONE',  ( -3.260378293283676232, 1516.582197291435023, 201.4115601429068079 ) ) ;
#14221 = CARTESIAN_POINT ( 'NONE',  ( -12.70095137425357379, 1445.015557356070303, 169.4597653655617648 ) ) ;
#14222 = FACE_OUTER_BOUND ( 'NONE', #30815, .T. ) ;
#14223 = CARTESIAN_POINT ( 'NONE',  ( -15.92986207429999901, 1416.139014782290133, 209.7537124246929920 ) ) ;
#14225 = CARTESIAN_POINT ( 'NONE',  ( -1.362564840747860107, 1414.935332577269946, 185.4090015132200051 ) ) ;
#14224 = CARTESIAN_POINT ( 'NONE',  ( 2.618187928979999857, 1445.209012209990078, 200.3785934838089986 ) ) ;
#14226 = CARTESIAN_POINT ( 'NONE',  ( 3.798727053469999504, 1410.301227430230028, 185.9690677660979645 ) ) ;
#14227 = CARTESIAN_POINT ( 'NONE',  ( -7.752197826429999772, 1416.823872462129884, 192.4769319036979880 ) ) ;
#14228 = CARTESIAN_POINT ( 'NONE',  ( 2.132506400839999650, 1418.942295325089844, 204.3612836522989937 ) ) ;
#14229 = CARTESIAN_POINT ( 'NONE',  ( 10.95806849906840164, 1396.295724571469918, 207.5366794976360154 ) ) ;
#14230 = CARTESIAN_POINT ( 'NONE',  ( 1.555569193349999990, 1415.296882296330068, 191.0414296403980075 ) ) ;
#14231 = CARTESIAN_POINT ( 'NONE',  ( 10.93289368750000001, 1429.709397299530110, 151.3050649637980030 ) ) ;
#14232 = CARTESIAN_POINT ( 'NONE',  ( 8.375502445464999113, 1512.383155430630040, 202.3790113465069851 ) ) ;
#14233 = ORIENTED_EDGE ( 'NONE', *, *, #96652, .F. ) ;
#14234 = CARTESIAN_POINT ( 'NONE',  ( 13.34701713054489858, 1434.912624059160180, 148.9125970433090060 ) ) ;
#14235 = CARTESIAN_POINT ( 'NONE',  ( 22.08523692261549698, 1523.530935881284904, 184.4211863326289915 ) ) ;
#14236 = VERTEX_POINT ( 'NONE', #41686 ) ;
#14237 = ORIENTED_EDGE ( 'NONE', *, *, #105498, .F. ) ;
#14238 = DIRECTION ( 'NONE',  ( -0.7020890432300541661, 0.02451748950546728256, -0.7116669643060977712 ) ) ;
#14239 = CARTESIAN_POINT ( 'NONE',  ( -13.76044198839999844, 1462.505312967929967, 230.0314476057980073 ) ) ;
#14240 = AXIS2_PLACEMENT_3D ( 'NONE', #97532, #73991, #89129 ) ;
#14241 = CARTESIAN_POINT ( 'NONE',  ( -109.3216456436046968, 1387.209460202328955, 311.0349939649406110 ) ) ;
#14242 = CARTESIAN_POINT ( 'NONE',  ( 29.99620953741487384, 1526.382868172863937, 198.4974435154498735 ) ) ;
#14243 = CARTESIAN_POINT ( 'NONE',  ( -4.615644842514999624, 1517.009964551830080, 216.0692237534070159 ) ) ;
#14244 = CARTESIAN_POINT ( 'NONE',  ( -13.10979329346079858, 1380.091434411379851, 209.5250314328370109 ) ) ;
#14245 = ORIENTED_EDGE ( 'NONE', *, *, #67201, .T. ) ;
#14246 = CARTESIAN_POINT ( 'NONE',  ( -11.40405654770000154, 1501.068632103089840, 208.2804062866189838 ) ) ;
#14247 = CARTESIAN_POINT ( 'NONE',  ( -11.73541398288529969, 1509.403454113690032, 181.4876751329869933 ) ) ;
#14248 = CARTESIAN_POINT ( 'NONE',  ( -30.31557410699999977, 1377.728231664160148, 212.6771353113689713 ) ) ;
#14249 = EDGE_CURVE ( 'NONE', #7609, #74455, #62439, .T. ) ;
#14250 = CARTESIAN_POINT ( 'NONE',  ( -1.715704529104999931, 1516.757508073510053, 205.8704515699670026 ) ) ;
#14251 = ORIENTED_EDGE ( 'NONE', *, *, #17933, .T. ) ;
#14252 = CARTESIAN_POINT ( 'NONE',  ( 4.042388501175000037, 1517.045004075700035, 209.8579434088520088 ) ) ;
#14253 = VECTOR ( 'NONE', #98751, 1000.000000000000000 ) ;
#14254 = CARTESIAN_POINT ( 'NONE',  ( -20.28559706309999910, 1508.605287556030135, 228.9894631997980241 ) ) ;
#14255 = EDGE_CURVE ( 'NONE', #1934, #58146, #68018, .T. ) ;
#14256 = CARTESIAN_POINT ( 'NONE',  ( -5.503799114343967958, 1410.587718136319836, 269.3375590789236753 ) ) ;
#14257 = CARTESIAN_POINT ( 'NONE',  ( -0.5979851740210000433, 1408.933942489730043, 231.6757385099979842 ) ) ;
#14259 = ORIENTED_EDGE ( 'NONE', *, *, #100225, .T. ) ;
#14258 = CARTESIAN_POINT ( 'NONE',  ( -7.713339349770000020, 1475.513060387329915, 189.5179100386980053 ) ) ;
#14260 = CARTESIAN_POINT ( 'NONE',  ( 2.500000000000000000, 1432.255994091859975, 157.4927853088979930 ) ) ;
#14261 = CARTESIAN_POINT ( 'NONE',  ( -34.53043532563810203, 1440.913060389100110, 249.9798763198099891 ) ) ;
#14262 = CARTESIAN_POINT ( 'NONE',  ( -27.62594988560000075, 1384.837137189770147, 225.6315537474590371 ) ) ;
#14263 = CARTESIAN_POINT ( 'NONE',  ( -14.00462132320000030, 1415.677402202029953, 214.2425697179989754 ) ) ;
#14264 = CARTESIAN_POINT ( 'NONE',  ( 13.52613638629999926, 1409.420097905330067, 270.2585879650980019 ) ) ;
#14265 = CARTESIAN_POINT ( 'NONE',  ( 0.01322035751810150123, 1516.939819969850078, 213.1588969678170145 ) ) ;
#14266 = CARTESIAN_POINT ( 'NONE',  ( 22.70509154759999859, 1409.705932507530179, 209.2982499274170323 ) ) ;
#14267 = CARTESIAN_POINT ( 'NONE',  ( -20.27305603270000134, 1508.384852854430164, 189.2299609745979865 ) ) ;
#14268 = CARTESIAN_POINT ( 'NONE',  ( 0.02750565378459880056, 1442.646891867090062, 219.1054768861489777 ) ) ;
#14269 = CARTESIAN_POINT ( 'NONE',  ( -7.709377382076580076, 1516.547507499529956, 211.8130208532940060 ) ) ;
#14270 = CARTESIAN_POINT ( 'NONE',  ( -3.251394400264999707, 1516.757508073510053, 210.8375504612070017 ) ) ;
#14271 = CARTESIAN_POINT ( 'NONE',  ( 4.172462890132850433, 1421.447587853880123, 185.0121838783159944 ) ) ;
#14272 = CARTESIAN_POINT ( 'NONE',  ( 0.4435038406939999511, 1418.672163285830038, 184.7048927289980043 ) ) ;
#14273 = CARTESIAN_POINT ( 'NONE',  ( 10.98083629090000102, 1433.016921068679949, 151.7694307944979926 ) ) ;
#14275 = ORIENTED_EDGE ( 'NONE', *, *, #60980, .F. ) ;
#14274 = CARTESIAN_POINT ( 'NONE',  ( -39.28171750389999772, 1390.901355467679878, 224.3483216179589874 ) ) ;
#14276 = CARTESIAN_POINT ( 'NONE',  ( -44.66018671116690086, 1385.154557438659822, 250.8453420411730406 ) ) ;
#14277 = CARTESIAN_POINT ( 'NONE',  ( 18.95839814150000180, 1416.827520077830059, 210.4638737380680027 ) ) ;
#14278 = LINE ( 'NONE', #84248, #52163 ) ;
#14279 = PRODUCT ( 'Feed Screw', 'Feed Screw', '', ( #81854 ) ) ;
#14280 = CARTESIAN_POINT ( 'NONE',  ( -1.347852712580000167, 1417.336052002229962, 235.7060345899980121 ) ) ;
#14281 = CIRCLE ( 'NONE', #80406, 0.9999999999999974465 ) ;
#14282 = CARTESIAN_POINT ( 'NONE',  ( -5.386815040730001058, 1432.449270638659982, 154.6099187821979797 ) ) ;
#14283 = CARTESIAN_POINT ( 'NONE',  ( 11.19329478399999900, 1422.593227753940027, 205.2156856529389870 ) ) ;
#14284 = DIRECTION ( 'NONE',  ( 0.000000000000000000, 0.000000000000000000, 1.000000000000000000 ) ) ;
#14286 = DIRECTION ( 'NONE',  ( -0.000000000000000000, -1.000000000000000000, -0.000000000000000000 ) ) ;
#14285 = CARTESIAN_POINT ( 'NONE',  ( 3.454748808194999743, 1516.609912606490070, 216.4448802441970088 ) ) ;
#14287 = CARTESIAN_POINT ( 'NONE',  ( -25.76861165497327022, 1450.790415003483076, 136.9094829965818292 ) ) ;
#14288 = CARTESIAN_POINT ( 'NONE',  ( 32.09235212275375915, 1525.402221411349956, 221.9833860708131397 ) ) ;
#14289 = ORIENTED_EDGE ( 'NONE', *, *, #59852, .F. ) ;
#14290 = CARTESIAN_POINT ( 'NONE',  ( 5.778372563615000068, 1516.932669162149978, 202.1763558832970205 ) ) ;
#14291 = CARTESIAN_POINT ( 'NONE',  ( -13.58235846979999906, 1416.828040475229955, 221.9087530951979659 ) ) ;
#14292 = ORIENTED_EDGE ( 'NONE', *, *, #90099, .T. ) ;
#14293 = VECTOR ( 'NONE', #18209, 1000.000000000000000 ) ;
#14294 = CARTESIAN_POINT ( 'NONE',  ( 1.600048698852036821, 1401.254281879943164, 135.5999999980979851 ) ) ;
#14295 = CARTESIAN_POINT ( 'NONE',  ( 24.32016871089999910, 1444.936401044380091, 214.5085396922679877 ) ) ;
#14296 = CARTESIAN_POINT ( 'NONE',  ( 10.87641374706830177, 1461.647512902760127, 210.5511653657890179 ) ) ;
#14297 = CARTESIAN_POINT ( 'NONE',  ( 8.406304952171057110, 1424.431735268568445, 195.8247349441674032 ) ) ;
#14298 = CARTESIAN_POINT ( 'NONE',  ( 2.594761893819999887, 1441.567844146989955, 218.7008844616090073 ) ) ;
#14299 = CARTESIAN_POINT ( 'NONE',  ( 15.61977316628497015, 1421.021825222467442, 227.6337086628678037 ) ) ;
#14300 = LINE ( 'NONE', #82629, #5638 ) ;
#14301 = CARTESIAN_POINT ( 'NONE',  ( -19.72693241579999679, 1426.900081331430101, 224.3685230545979721 ) ) ;
#14302 = CARTESIAN_POINT ( 'NONE',  ( 7.432030730716068234, 1487.100624600356241, 201.2524259029208054 ) ) ;
#14303 = CARTESIAN_POINT ( 'NONE',  ( -106.9455967239999978, 1390.237690493389891, 299.5801972406590039 ) ) ;
#14304 = CARTESIAN_POINT ( 'NONE',  ( 17.19739463999625784, 1525.960063244516959, 181.9833109756548595 ) ) ;
#14305 = CARTESIAN_POINT ( 'NONE',  ( 0.2758982302775880302, 1410.303294781930163, 233.2202553833849663 ) ) ;
#14306 = CARTESIAN_POINT ( 'NONE',  ( -29.82212560978975802, 1462.379445244557701, 269.4689213073284577 ) ) ;
#14307 = ORIENTED_EDGE ( 'NONE', *, *, #60175, .T. ) ;
#14308 = CARTESIAN_POINT ( 'NONE',  ( -5.642160312090365615, 1406.970328519305667, 269.6422777563649333 ) ) ;
#14309 = CARTESIAN_POINT ( 'NONE',  ( 11.19358401111760060, 1470.358879059469928, 207.1653923726030087 ) ) ;
#14310 = DIRECTION ( 'NONE',  ( -1.000000000000000000, 0.000000000000000000, 0.000000000000000000 ) ) ;
#14311 = AXIS2_PLACEMENT_3D ( 'NONE', #40502, #99845, #29889 ) ;
#14312 = CARTESIAN_POINT ( 'NONE',  ( -0.2068382967480000001, 1416.433929650830123, 233.7159416108979997 ) ) ;
#14313 = CARTESIAN_POINT ( 'NONE',  ( -13.11599568954357942, 1444.787961940224932, 186.4523988439049731 ) ) ;
#14314 = B_SPLINE_SURFACE_WITH_KNOTS ( 'NONE', 5, 5, ( 
 ( #17336, #78387, #76176, #69460, #104133, #52093 ),
 ( #35836, #77293, #8964, #42574, #60499, #85663 ),
 ( #59398, #43135, #9515, #10635, #85114, #27419 ),
 ( #61602, #102461, #95735, #86780, #591, #110325 ),
 ( #18999, #67793, #1695, #34169, #10069, #93509 ),
 ( #61068, #34718, #70019, #53199, #86224, #25195 ),
 ( #51530, #68909, #103011, #8402, #87339, #26307 ),
 ( #33598, #44243, #43683, #16781, #50985, #76725 ),
 ( #94620, #38, #68355, #17896, #35275, #94067 ) ),
 .UNSPECIFIED., .F., .F., .F.,
 ( 6, 3, 6 ),
 ( 6, 6 ),
 ( 1.832321132619999986E-17, 6.516940428549999886, 11.47905148820000143 ),
 ( 0.000000000000000000, 1.000000000000000000 ),
 .UNSPECIFIED. ) ;
#14315 = CARTESIAN_POINT ( 'NONE',  ( 12.53380499169999851, 1442.773887286369927, 169.4755105685979970 ) ) ;
#14316 = DIRECTION ( 'NONE',  ( 0.000000000000000000, 0.000000000000000000, 1.000000000000000000 ) ) ;
#14317 = DIRECTION ( 'NONE',  ( 0.7071067811865475727, 1.631342908290929267E-16, -0.7071067811865475727 ) ) ;
#14318 = CARTESIAN_POINT ( 'NONE',  ( -14.01525996361490023, 1415.677402202029953, 204.0303134510289738 ) ) ;
#14319 = ADVANCED_FACE ( 'NONE', ( #66910 ), #86444, .T. ) ;
#14320 = CARTESIAN_POINT ( 'NONE',  ( 24.97897394130000137, 1436.441733159510022, 137.9167456186980019 ) ) ;
#14321 = CARTESIAN_POINT ( 'NONE',  ( -8.551515107930001136, 1437.707591943389843, 226.0657740139990040 ) ) ;
#14323 = ORIENTED_EDGE ( 'NONE', *, *, #72941, .F. ) ;
#14322 = DIRECTION ( 'NONE',  ( 0.000000000000000000, 0.000000000000000000, -1.000000000000000000 ) ) ;
#14324 = CARTESIAN_POINT ( 'NONE',  ( -113.4000000000000057, 1381.047475678389901, 309.3701288452589893 ) ) ;
#14325 = CARTESIAN_POINT ( 'NONE',  ( 14.08695216841010023, 1513.170547668200015, 224.3743395614490055 ) ) ;
#14326 = ORIENTED_EDGE ( 'NONE', *, *, #57405, .T. ) ;
#14327 = ORIENTED_EDGE ( 'NONE', *, *, #47380, .T. ) ;
#14328 = EDGE_CURVE ( 'NONE', #6825, #20574, #43899, .T. ) ;
#14329 = CARTESIAN_POINT ( 'NONE',  ( 18.16418870590809931, 1416.835419214280137, 209.1673351295509917 ) ) ;
#14330 = CARTESIAN_POINT ( 'NONE',  ( -8.862265221084019373, 1384.931617321382419, 218.6851228964859502 ) ) ;
#14332 = CARTESIAN_POINT ( 'NONE',  ( -9.325404508809999271, 1464.388849669230012, 238.2842606474980016 ) ) ;
#14331 = CARTESIAN_POINT ( 'NONE',  ( 41.80252838952070249, 1437.000150592197542, 269.6437000537932818 ) ) ;
#14333 = CARTESIAN_POINT ( 'NONE',  ( -19.81987573899999688, 1494.487655362629766, 189.5802261639979918 ) ) ;
#14334 = CARTESIAN_POINT ( 'NONE',  ( -11.74619720679999979, 1433.378107375729996, 150.8204405054979986 ) ) ;
#14335 = FACE_OUTER_BOUND ( 'NONE', #104524, .T. ) ;
#14336 = CARTESIAN_POINT ( 'NONE',  ( 9.708970498318210574, 1463.715168242549908, 210.4580945914069900 ) ) ;
#14337 = CARTESIAN_POINT ( 'NONE',  ( -27.30723893600000096, 1439.410402289340254, 137.0765984299980005 ) ) ;
#14338 = CARTESIAN_POINT ( 'NONE',  ( -12.78690713350000152, 1416.828040475229955, 195.5394874918979724 ) ) ;
#14339 = DIRECTION ( 'NONE',  ( 0.000000000000000000, 1.000000000000000000, 0.000000000000000000 ) ) ;
#14340 = CARTESIAN_POINT ( 'NONE',  ( -2.923263464371510079, 1409.521016840560151, 186.8216758237240072 ) ) ;
#14341 = CARTESIAN_POINT ( 'NONE',  ( 4.017468778259492446, 1361.987815076348852, 210.6218459617142003 ) ) ;
#14342 = CARTESIAN_POINT ( 'NONE',  ( -11.06185805447235104, 1509.424462684860146, 237.0079586032242389 ) ) ;
#14344 = ORIENTED_EDGE ( 'NONE', *, *, #96009, .F. ) ;
#14343 = CARTESIAN_POINT ( 'NONE',  ( 8.404157474328759975E-09, 1409.508817234440130, 259.7239082992959993 ) ) ;
#14345 = ORIENTED_EDGE ( 'NONE', *, *, #92728, .T. ) ;
#14346 = CARTESIAN_POINT ( 'NONE',  ( -11.85807509641779944, 1431.776270381120185, 149.9536850627220019 ) ) ;
#14347 = CARTESIAN_POINT ( 'NONE',  ( -13.56738355449999922, 1505.237168496690174, 227.8242396965990224 ) ) ;
#14348 = CARTESIAN_POINT ( 'NONE',  ( -7.287608047049999982, 1471.338968442629948, 269.8696687364979994 ) ) ;
#14349 = CARTESIAN_POINT ( 'NONE',  ( -1.924402692774775270, 1474.171439542113376, 219.1969456462446431 ) ) ;
#14350 = CARTESIAN_POINT ( 'NONE',  ( -1.110223024630000146E-16, 1433.447556881219953, 155.4376913957980264 ) ) ;
#14351 = CARTESIAN_POINT ( 'NONE',  ( 34.59019106360999984, 1451.551308700359868, 135.5662212263999891 ) ) ;
#14352 = AXIS2_PLACEMENT_3D ( 'NONE', #37003, #38106, #20734 ) ;
#14353 = CARTESIAN_POINT ( 'NONE',  ( 4.327986479516090057, 1515.120635733899917, 209.9709076042840081 ) ) ;
#14354 = CARTESIAN_POINT ( 'NONE',  ( -8.383874734839999121, 1384.494374329680113, 199.7996924129390095 ) ) ;
#14355 = CARTESIAN_POINT ( 'NONE',  ( 10.03380816088620087, 1469.200710370999786, 209.4646523673320075 ) ) ;
#14356 = CARTESIAN_POINT ( 'NONE',  ( -3.738989945110000157, 1456.530141059690095, 217.8454007011089857 ) ) ;
#14357 = CARTESIAN_POINT ( 'NONE',  ( 9.663424421699261302, 1363.752474719050042, 210.6218459616991936 ) ) ;
#14358 = CARTESIAN_POINT ( 'NONE',  ( -37.25277800141729756, 1420.473031640739919, 269.0086013173549873 ) ) ;
#14359 = CIRCLE ( 'NONE', #50123, 1.999999999999999556 ) ;
#14360 = ORIENTED_EDGE ( 'NONE', *, *, #32911, .T. ) ;
#14361 = ORIENTED_EDGE ( 'NONE', *, *, #40545, .T. ) ;
#14362 = EDGE_LOOP ( 'NONE', ( #92273, #72808 ) ) ;
#14363 = CARTESIAN_POINT ( 'NONE',  ( 2.299656316094999653, 1516.843453247299749, 211.5982966343670171 ) ) ;
#14364 = CARTESIAN_POINT ( 'NONE',  ( -2.500000000000000000, 1428.666845053830002, 184.0221679455979995 ) ) ;
#14366 = CARTESIAN_POINT ( 'NONE',  ( -17.64250891069632843, 1419.640929922183432, 207.0584130580827207 ) ) ;
#14365 = CARTESIAN_POINT ( 'NONE',  ( 5.010422963235000360, 1516.929569650079884, 213.1529883219070030 ) ) ;
#14367 = CARTESIAN_POINT ( 'NONE',  ( -14.25300571640000058, 1440.433557114710084, 188.8957244713979833 ) ) ;
#14368 = CIRCLE ( 'NONE', #85921, 1.999999999999999556 ) ;
#14369 = CARTESIAN_POINT ( 'NONE',  ( -2.310656430857296328, 1449.746119739275400, 182.9714966330411698 ) ) ;
#14370 = ORIENTED_EDGE ( 'NONE', *, *, #70946, .T. ) ;
#14371 = CARTESIAN_POINT ( 'NONE',  ( -26.37348269860000016, 1435.500559562420221, 135.8355299040979958 ) ) ;
#14372 = SHAPE_REPRESENTATION ( 'MAS-682', ( #74442, #52208, #3932, #95, #73635, #62700, #57330, #107571, #59323, #11032 ), #72680 ) ;
#14373 = CARTESIAN_POINT ( 'NONE',  ( 4.615644804385000022, 1517.009964551830080, 202.1744681489270192 ) ) ;
#14374 = EDGE_CURVE ( 'NONE', #64042, #50617, #51784, .T. ) ;
#14375 = DIRECTION ( 'NONE',  ( 0.000000000000000000, -1.000000000000000000, 0.000000000000000000 ) ) ;
#14376 = CARTESIAN_POINT ( 'NONE',  ( -22.89435465436789841, 1384.539855335990069, 202.5339165971940076 ) ) ;
#14377 = CARTESIAN_POINT ( 'NONE',  ( 0.02192820754129999605, 1407.539782043129890, 196.0601747759980071 ) ) ;
#14378 = CARTESIAN_POINT ( 'NONE',  ( -16.66936639839001444, 1523.456924617335972, 180.4828114240353329 ) ) ;
#14379 = DIRECTION ( 'NONE',  ( 0.4794255386041986200, 0.000000000000000000, 0.8775825618903752012 ) ) ;
#14381 = ORIENTED_EDGE ( 'NONE', *, *, #32, .T. ) ;
#14380 = CARTESIAN_POINT ( 'NONE',  ( -10.02185219043178144, 1364.916310432309956, 210.6218459616987957 ) ) ;
#14382 = ORIENTED_EDGE ( 'NONE', *, *, #25710, .T. ) ;
#14383 = CARTESIAN_POINT ( 'NONE',  ( 0.2568979742649999398, 1452.981230334829888, 183.2590030997980080 ) ) ;
#14384 = CARTESIAN_POINT ( 'NONE',  ( -28.27139721233027458, 1526.382868172864164, 219.5606225550389468 ) ) ;
#14385 = CARTESIAN_POINT ( 'NONE',  ( -14.59279134157089963, 1436.244781760590058, 149.8708244536879874 ) ) ;
#14386 = CIRCLE ( 'NONE', #7287, 8.432239102140000497 ) ;
#14387 = CARTESIAN_POINT ( 'NONE',  ( -0.8179048554660000026, 1485.520952860329999, 181.9073606171980089 ) ) ;
#14388 = CARTESIAN_POINT ( 'NONE',  ( 7.338411959395000572, 1517.170512887980067, 211.6064236274570192 ) ) ;
#14389 = CARTESIAN_POINT ( 'NONE',  ( 6.083541831545586476, 1460.052579242508727, 201.6434494505425334 ) ) ;
#14390 = CARTESIAN_POINT ( 'NONE',  ( 5.519893427111519202, 1440.499866072189889, 154.7645221071819890 ) ) ;
#14391 = CARTESIAN_POINT ( 'NONE',  ( 5.878018521898390247, 1440.945822282649942, 215.8104943704309733 ) ) ;
#14392 = CARTESIAN_POINT ( 'NONE',  ( -3.887243918150000104E-16, 1418.913060387330006, 172.2701767054979882 ) ) ;
#14393 = CARTESIAN_POINT ( 'NONE',  ( 7.890119370045001190, 1511.483345606789953, 205.5629819087669716 ) ) ;
#14394 = CARTESIAN_POINT ( 'NONE',  ( -6.951175166914999259, 1517.170721208160103, 206.8315896683770063 ) ) ;
#14395 = ORIENTED_EDGE ( 'NONE', *, *, #46699, .F. ) ;
#14396 = CARTESIAN_POINT ( 'NONE',  ( -33.91369114127179785, 1435.681798693280143, 134.7398496782940072 ) ) ;
#14397 = CARTESIAN_POINT ( 'NONE',  ( -10.93621683099999942, 1471.189486259790101, 208.1842957432819787 ) ) ;
#14398 = CARTESIAN_POINT ( 'NONE',  ( -24.02428866992241652, 1445.062781591384919, 212.2832923785209118 ) ) ;
#14399 = ORIENTED_EDGE ( 'NONE', *, *, #83173, .T. ) ;
#14401 = AXIS2_PLACEMENT_3D ( 'NONE', #37861, #72047, #73117 ) ;
#14400 = FACE_OUTER_BOUND ( 'NONE', #85668, .T. ) ;
#14402 = CARTESIAN_POINT ( 'NONE',  ( 12.83022075569469855, 1434.689919048429829, 149.3777740995939780 ) ) ;
#14403 = CARTESIAN_POINT ( 'NONE',  ( 13.40958059889999987, 1414.996444526030018, 197.9133051477979848 ) ) ;
#14404 = CARTESIAN_POINT ( 'NONE',  ( -11.40252061979999887, 1416.855034940659834, 204.2434678627789992 ) ) ;
#14405 = DIRECTION ( 'NONE',  ( -0.7067699325516847431, 0.03085807370037648573, 0.7067701477343176775 ) ) ;
#14406 = LINE ( 'NONE', #55902, #62519 ) ;
#14407 = CARTESIAN_POINT ( 'NONE',  ( 3.773762947180000271, 1486.021325443789920, 199.0256766443990273 ) ) ;
#14408 = CARTESIAN_POINT ( 'NONE',  ( 30.31940284292419108, 1523.382868172864164, 222.4933038710543372 ) ) ;
#14409 = CARTESIAN_POINT ( 'NONE',  ( 4.243484587782480055, 1441.412175538559950, 162.2162703121909999 ) ) ;
#14410 = EDGE_CURVE ( 'NONE', #23318, #22363, #46680, .T. ) ;
#14411 = CARTESIAN_POINT ( 'NONE',  ( -15.73573827020000060, 1409.462564476230000, 225.2909780739980192 ) ) ;
#14412 = CARTESIAN_POINT ( 'NONE',  ( 18.14949073579999705, 1432.344282874789997, 211.8258969992290019 ) ) ;
#14413 = CARTESIAN_POINT ( 'NONE',  ( -0.7396922758749979732, 1517.135701590510052, 216.4591432822169850 ) ) ;
#14414 = ORIENTED_EDGE ( 'NONE', *, *, #56853, .T. ) ;
#14415 = CARTESIAN_POINT ( 'NONE',  ( 7.716938320446660171, 1516.836245356829750, 208.7837035492700011 ) ) ;
#14416 = DIRECTION ( 'NONE',  ( 0.000000000000000000, 0.000000000000000000, 1.000000000000000000 ) ) ;
#14417 = CARTESIAN_POINT ( 'NONE',  ( -18.10358820054819873, 1416.830086716310007, 209.2067746984330086 ) ) ;
#14418 = CARTESIAN_POINT ( 'NONE',  ( -15.62742587511660020, 1508.451903174239987, 214.8815429522870204 ) ) ;
#14419 = CARTESIAN_POINT ( 'NONE',  ( 1.617204962490000009, 1473.963834395889990, 219.3699064269989947 ) ) ;
#14420 = CARTESIAN_POINT ( 'NONE',  ( -0.04582397527460040088, 1508.911460179130017, 179.8421084519130204 ) ) ;
#14421 = CARTESIAN_POINT ( 'NONE',  ( 11.60004869885203682, 1426.172749320205185, 138.0249698027471936 ) ) ;
#14422 = CARTESIAN_POINT ( 'NONE',  ( -2.500000000000000000, 1419.382898089430000, 144.1038810569979773 ) ) ;
#14423 = CARTESIAN_POINT ( 'NONE',  ( -2.933467300942110167, 1454.462654904609963, 199.0544936251469892 ) ) ;
#14424 = CARTESIAN_POINT ( 'NONE',  ( -3.527889728650740089E-07, 1407.083036151889928, 222.1289087389290273 ) ) ;
#14425 = B_SPLINE_SURFACE_WITH_KNOTS ( 'NONE', 5, 5, ( 
 ( #320, #69172, #50695, #67519, #34445, #86496 ),
 ( #8127, #68621, #102723, #26017, #60214, #24908 ),
 ( #9790, #17610, #94332, #42293, #85952, #94907 ),
 ( #9253, #18181, #77561, #866, #103278, #43957 ),
 ( #19839, #28809, #27701, #96567, #87052, #54044 ),
 ( #12553, #1976, #54586, #88722, #71954, #71405 ),
 ( #35542, #79776, #87621, #36111, #89258, #3083 ),
 ( #11462, #55138, #106065, #36654, #46731, #80865 ),
 ( #103855, #69737, #18722, #45082, #37210, #44512 ) ),
 .UNSPECIFIED., .F., .F., .F.,
 ( 6, 3, 6 ),
 ( 6, 6 ),
 ( 12.02292824550000105, 22.14719212230000167, 26.06149361980000023 ),
 ( 0.000000000000000000, 2.000000000000000000 ),
 .UNSPECIFIED. ) ;
#14426 = CARTESIAN_POINT ( 'NONE',  ( 28.28124823237279983, 1440.913060387279984, 232.2763879390959971 ) ) ;
#14428 = CARTESIAN_POINT ( 'NONE',  ( 10.00306449797230002, 1469.399223428769801, 210.0757042779839878 ) ) ;
#14427 = CARTESIAN_POINT ( 'NONE',  ( -9.915141243902969137, 1471.119519607170105, 211.8083852528800151 ) ) ;
#14429 = DIRECTION ( 'NONE',  ( 0.3090169943749446757, 0.000000000000000000, -0.9510565162951544194 ) ) ;
#14430 = ORIENTED_EDGE ( 'NONE', *, *, #3607, .T. ) ;
#14431 = ORIENTED_EDGE ( 'NONE', *, *, #82837, .T. ) ;
#14432 = CARTESIAN_POINT ( 'NONE',  ( 2.694739704345540332, 1517.151704408390060, 206.1657712119973382 ) ) ;
#14433 = CARTESIAN_POINT ( 'NONE',  ( -47.22427986889969276, 1578.884133025160281, 191.3316845414530007 ) ) ;
#14434 = CARTESIAN_POINT ( 'NONE',  ( -3.578533967270000282, 1442.500416740689843, 200.8327418449289894 ) ) ;
#14435 = CARTESIAN_POINT ( 'NONE',  ( 11.35344352881629959, 1502.969967087519990, 211.0626227285410152 ) ) ;
#14436 = CARTESIAN_POINT ( 'NONE',  ( 2.087781202739551034, 1508.813655593662361, 237.6275677725071773 ) ) ;
#14437 = VECTOR ( 'NONE', #76896, 1000.000000000000000 ) ;
#14438 = CARTESIAN_POINT ( 'NONE',  ( 10.80761588395260020, 1422.264295156030130, 211.0685490254289789 ) ) ;
#14439 = CARTESIAN_POINT ( 'NONE',  ( 0.000000000000000000, 1441.261220175949802, 126.8032249175980155 ) ) ;
#14440 = CARTESIAN_POINT ( 'NONE',  ( 1.108124621956710021, 1508.551704408389924, 219.8565429179099908 ) ) ;
#14441 = CARTESIAN_POINT ( 'NONE',  ( -43.78017172700090498, 1383.822166568830198, 248.7628566075970014 ) ) ;
#14442 = EDGE_CURVE ( 'NONE', #11383, #24304, #33558, .T. ) ;
#14444 = B_SPLINE_CURVE_WITH_KNOTS ( 'NONE', 5,
 ( #100965, #57360, #65744, #92032, #92570, #59000, #99307, #66856, #74149 ),
 .UNSPECIFIED., .F., .F.,
 ( 6, 3, 6 ),
 ( 0.000000000000000000, 0.5050532947838839437, 1.000000000000000000 ),
 .UNSPECIFIED. ) ;
#14443 = CARTESIAN_POINT ( 'NONE',  ( -4.036380785655000025, 1511.355055856609852, 201.1360035737969838 ) ) ;
#14445 = ADVANCED_FACE ( 'NONE', ( #37703 ), #17704, .T. ) ;
#14446 = CARTESIAN_POINT ( 'NONE',  ( -15.13403568919999920, 1507.625766668030110, 191.8456552481979998 ) ) ;
#14447 = CARTESIAN_POINT ( 'NONE',  ( -12.30475894872500042, 1502.479826408779900, 208.9714260491429911 ) ) ;
#14449 = AXIS2_PLACEMENT_3D ( 'NONE', #41685, #68562, #33271 ) ;
#14448 = DIRECTION ( 'NONE',  ( -1.076084536626781954E-17, -1.000000000000000000, -4.313860721084074369E-17 ) ) ;
#14450 = EDGE_CURVE ( 'NONE', #52333, #69312, #68198, .T. ) ;
#14452 = ORIENTED_EDGE ( 'NONE', *, *, #91698, .T. ) ;
#14451 = CARTESIAN_POINT ( 'NONE',  ( -115.9619579297967391, 1377.913060387289988, 305.7827340268977991 ) ) ;
#14453 = CARTESIAN_POINT ( 'NONE',  ( 33.23421991949457066, 1522.906363951597314, 217.4142352873253685 ) ) ;
#14454 = CARTESIAN_POINT ( 'NONE',  ( -13.38802240389999909, 1383.860181226410077, 218.7963554078490063 ) ) ;
#14455 = ADVANCED_FACE ( 'NONE', ( #18668 ), #2354, .T. ) ;
#14456 = CARTESIAN_POINT ( 'NONE',  ( 4.072632511270110278, 1508.551704408389924, 204.7001764067349825 ) ) ;
#14457 = ORIENTED_EDGE ( 'NONE', *, *, #76813, .F. ) ;
#14458 = EDGE_LOOP ( 'NONE', ( #57796, #95237, #45423, #19049 ) ) ;
#14459 = ADVANCED_FACE ( 'NONE', ( #82462 ), #74071, .F. ) ;
#14460 = CARTESIAN_POINT ( 'NONE',  ( -8.779303069688410233, 1386.002643005009986, 218.5317853082520116 ) ) ;
#14461 = CARTESIAN_POINT ( 'NONE',  ( -4.324121571198319636, 1515.222544082249897, 206.1650193910969904 ) ) ;
#14462 = CARTESIAN_POINT ( 'NONE',  ( -0.5623044073341159077, 1416.835806620478706, 227.7680351671496624 ) ) ;
#14464 = EDGE_CURVE ( 'NONE', #31461, #79161, #63821, .T. ) ;
#14463 = CARTESIAN_POINT ( 'NONE',  ( -5.142705184740000490, 1462.990135410090033, 200.8040030810390135 ) ) ;
#14465 = CARTESIAN_POINT ( 'NONE',  ( -105.8704711980000042, 1378.498029401629992, 301.8910949082590491 ) ) ;
#14466 = CARTESIAN_POINT ( 'NONE',  ( 4.326079330760677522, 1515.193466806362267, 211.4519800883807079 ) ) ;
#14467 = AXIS2_PLACEMENT_3D ( 'NONE', #62571, #54706, #44638 ) ;
#14468 = CARTESIAN_POINT ( 'NONE',  ( -22.52564151159999639, 1509.699673122230024, 190.3321270482979912 ) ) ;
#14469 = CARTESIAN_POINT ( 'NONE',  ( 0.6562332730204689657, 1408.935976558159837, 194.1358227214440149 ) ) ;
#14470 = CARTESIAN_POINT ( 'NONE',  ( 18.28844460585999698, 1425.323495367109899, 225.4768200461419951 ) ) ;
#14471 = PLANE ( 'NONE',  #105479 ) ;
#14472 = CARTESIAN_POINT ( 'NONE',  ( 7.647588771564749699, 1433.658576088640075, 203.7587819791999948 ) ) ;
#14473 = CARTESIAN_POINT ( 'NONE',  ( 11.86584296470000055, 1432.318021067500013, 149.9824182361979865 ) ) ;
#14474 = CARTESIAN_POINT ( 'NONE',  ( -4.162009348731279701, 1449.631390586350108, 185.0510865354499970 ) ) ;
#14475 = ORIENTED_EDGE ( 'NONE', *, *, #90855, .F. ) ;
#14477 = ADVANCED_FACE ( 'NONE', ( #56154 ), #47756, .T. ) ;
#14476 = CARTESIAN_POINT ( 'NONE',  ( -20.91563475928094462, 1525.795403383247276, 184.9927169682721910 ) ) ;
#14478 = CARTESIAN_POINT ( 'NONE',  ( 19.75053106571979811, 1455.500286668259832, 226.5546858144080318 ) ) ;
#14479 = CARTESIAN_POINT ( 'NONE',  ( 14.06572279189999897, 1410.763503171529919, 191.2785366137979963 ) ) ;
#14480 = VECTOR ( 'NONE', #44496, 1000.000000000000000 ) ;
#14481 = DIRECTION ( 'NONE',  ( -0.6709778558543730842, 0.000000000000000000, -0.7414773880254664773 ) ) ;
#14482 = CARTESIAN_POINT ( 'NONE',  ( -33.93019615848550785, 1522.906561336852519, 220.5829544588085014 ) ) ;
#14483 = CARTESIAN_POINT ( 'NONE',  ( -15.24773871110000023, 1420.384425983460005, 211.9003051376789983 ) ) ;
#14484 = CARTESIAN_POINT ( 'NONE',  ( -109.5956166280000019, 1386.715462780010057, 311.2107475812589996 ) ) ;
#14485 = EDGE_CURVE ( 'NONE', #79230, #18078, #14690, .T. ) ;
#14486 = CARTESIAN_POINT ( 'NONE',  ( -1.211166369079999861, 1482.210497797730113, 182.3203058735979880 ) ) ;
#14487 = CARTESIAN_POINT ( 'NONE',  ( -9.692061980449999226, 1363.802329763670059, 207.6218459616989946 ) ) ;
#14488 = CARTESIAN_POINT ( 'NONE',  ( -45.63009907890679528, 1440.261568459579848, 268.9750367124860304 ) ) ;
#14489 = CARTESIAN_POINT ( 'NONE',  ( -20.64235243649999774, 1507.778435260330070, 191.4718973457979985 ) ) ;
#14490 = EDGE_CURVE ( 'NONE', #87520, #16155, #52247, .T. ) ;
#14491 = CARTESIAN_POINT ( 'NONE',  ( -3.462835665494999660, 1517.038650117239968, 208.0021282158369900 ) ) ;
#14492 = CARTESIAN_POINT ( 'NONE',  ( 6.294750265487480512, 1408.079328831549901, 220.7028845641339672 ) ) ;
#14493 = DIRECTION ( 'NONE',  ( 0.000000000000000000, 1.000000000000000000, 0.000000000000000000 ) ) ;
#14494 = CARTESIAN_POINT ( 'NONE',  ( 2.958237723154419463, 1515.068899831249155, 204.7925047457962648 ) ) ;
#14495 = CARTESIAN_POINT ( 'NONE',  ( 7.439392163950960146, 1425.194634625760045, 212.3718729812599975 ) ) ;
#14497 = ADVANCED_FACE ( 'NONE', ( #85751 ), #787, .T. ) ;
#14496 = TOROIDAL_SURFACE ( 'NONE', #87913, 2.000000000000000000, 1.000000000000000000 ) ;
#14498 = EDGE_LOOP ( 'NONE', ( #14430, #92431, #53703, #36932 ) ) ;
#14499 = CARTESIAN_POINT ( 'NONE',  ( 22.11712025709999807, 1419.857860618529912, 248.4077083947979929 ) ) ;
#14500 = CARTESIAN_POINT ( 'NONE',  ( -28.00748489060000068, 1508.132844953629956, 207.4252966237179976 ) ) ;
#14502 = CARTESIAN_POINT ( 'NONE',  ( -15.26851443651900020, 1512.495155157800127, 222.3098048121690056 ) ) ;
#14501 = CARTESIAN_POINT ( 'NONE',  ( 0.4750796042289999743, 1494.209875447929790, 181.4895372315980069 ) ) ;
#14503 = LINE ( 'NONE', #31864, #53423 ) ;
#14504 = CARTESIAN_POINT ( 'NONE',  ( -25.73196798229999871, 1439.230040327810002, 220.8240077837979811 ) ) ;
#14505 = FACE_OUTER_BOUND ( 'NONE', #31759, .T. ) ;
#14506 = CARTESIAN_POINT ( 'NONE',  ( -19.88783023904650094, 1452.218562051830304, 143.3852592352909880 ) ) ;
#14507 = CARTESIAN_POINT ( 'NONE',  ( 29.25355977910000149, 1451.030362765829977, 136.3073753608980212 ) ) ;
#14508 = ORIENTED_EDGE ( 'NONE', *, *, #94757, .T. ) ;
#14509 = CARTESIAN_POINT ( 'NONE',  ( -3.030912759255987243, 1457.699420191448780, 218.6115341449503262 ) ) ;
#14510 = CARTESIAN_POINT ( 'NONE',  ( 17.29393938232482597, 1523.621879633028584, 237.3864571009499969 ) ) ;
#14511 = CARTESIAN_POINT ( 'NONE',  ( 15.74706555227250249, 1422.765470877109919, 229.4186969687229976 ) ) ;
#14512 = CARTESIAN_POINT ( 'NONE',  ( 10.41028103169999852, 1461.975860366590041, 210.7993106899690190 ) ) ;
#14513 = ORIENTED_EDGE ( 'NONE', *, *, #88115, .T. ) ;
#14514 = ORIENTED_EDGE ( 'NONE', *, *, #31026, .T. ) ;
#14515 = CARTESIAN_POINT ( 'NONE',  ( -64.53985313679999081, 1384.829190178189947, 254.0316580881589630 ) ) ;
#14516 = CARTESIAN_POINT ( 'NONE',  ( -24.11339479709999978, 1410.986675406829818, 209.4109128042719874 ) ) ;
#14517 = DIRECTION ( 'NONE',  ( 1.755985294532464991E-16, -1.000000000000000000, 1.338183447452830017E-16 ) ) ;
#14518 = CARTESIAN_POINT ( 'NONE',  ( 4.492644247030710858, 1508.880967439349888, 205.3188537370700146 ) ) ;
#14519 = CARTESIAN_POINT ( 'NONE',  ( -10.26338073471560008, 1517.551704408389924, 184.6900425920350131 ) ) ;
#14520 = PRESENTATION_LAYER_ASSIGNMENT (  '', '', ( #62877 ) ) ;
#14521 = CARTESIAN_POINT ( 'NONE',  ( -16.93884296450000093, 1507.634939588830093, 230.1482605005980133 ) ) ;
#14522 = ADVANCED_FACE ( 'NONE', ( #24719 ), #16864, .T. ) ;
#14523 = CARTESIAN_POINT ( 'NONE',  ( 4.058335268219130931, 1508.551704408389924, 213.8008226954089821 ) ) ;
#14524 = CARTESIAN_POINT ( 'NONE',  ( 43.30895383271469967, 1452.717412850039864, 266.4924207902549824 ) ) ;
#14525 = CARTESIAN_POINT ( 'NONE',  ( -0.9591896699583389863, 1424.151861139469929, 228.3373416235070010 ) ) ;
#14526 = ADVANCED_FACE ( 'NONE', ( #3431 ), #78469, .T. ) ;
#14527 = CARTESIAN_POINT ( 'NONE',  ( -6.465298943309999657, 1427.283379109839871, 203.6615921516590220 ) ) ;
#14528 = CARTESIAN_POINT ( 'NONE',  ( 2.284526458645000258, 1516.956048353049937, 205.6588971355569981 ) ) ;
#14529 = CIRCLE ( 'NONE', #100391, 1.000000000000002442 ) ;
#14530 = ORIENTED_EDGE ( 'NONE', *, *, #39541, .T. ) ;
#14531 = CARTESIAN_POINT ( 'NONE',  ( -7.228663065755877248, 1519.913060387329779, 183.1074954935087646 ) ) ;
#14532 = CARTESIAN_POINT ( 'NONE',  ( 6.822769659250000451, 1469.182992717989691, 208.8962877339269824 ) ) ;
#14533 = CARTESIAN_POINT ( 'NONE',  ( 12.92590733569883810, 1442.905621755283619, 187.0717105805051119 ) ) ;
#14534 = ORIENTED_EDGE ( 'NONE', *, *, #106284, .T. ) ;
#14535 = VERTEX_POINT ( 'NONE', #28611 ) ;
#14536 = CARTESIAN_POINT ( 'NONE',  ( -10.37614225292699999, 1479.403275255469907, 210.6296033183759846 ) ) ;
#14537 = CARTESIAN_POINT ( 'NONE',  ( -2.688576586735480056, 1508.385808335360025, 220.6470044136009960 ) ) ;
#14538 = CARTESIAN_POINT ( 'NONE',  ( -12.42116348050100072, 1512.160613316490071, 194.1975122379490131 ) ) ;
#14539 = CARTESIAN_POINT ( 'NONE',  ( 10.24150551940120124, 1502.975079637399858, 216.6982935228119800 ) ) ;
#14540 = CARTESIAN_POINT ( 'NONE',  ( 10.45480669290000009, 1420.576652099880221, 197.8458654235990082 ) ) ;
#14541 = CARTESIAN_POINT ( 'NONE',  ( 1.690297610143600027, 1474.866452951810061, 220.4152850073089667 ) ) ;
#14542 = CARTESIAN_POINT ( 'NONE',  ( -107.7075879675156358, 1380.190251876901129, 298.7630690546642427 ) ) ;
#14543 = CARTESIAN_POINT ( 'NONE',  ( -5.038226297060000469, 1495.449696765989984, 198.6986880815990162 ) ) ;
#14544 = CARTESIAN_POINT ( 'NONE',  ( 0.000000000000000000, 1440.913060387330006, 134.0999999980979851 ) ) ;
#14546 = DIRECTION ( 'NONE',  ( 0.03206686913393481247, -0.9990097415445143847, -0.03084237674223211378 ) ) ;
#14545 = CARTESIAN_POINT ( 'NONE',  ( -16.73048837315040061, 1413.002407920880160, 191.6778219149559845 ) ) ;
#14547 = CARTESIAN_POINT ( 'NONE',  ( 11.95048161449970081, 1426.790502429370008, 206.5664867952030193 ) ) ;
#14548 = EDGE_CURVE ( 'NONE', #72755, #24414, #54393, .T. ) ;
#14549 = CIRCLE ( 'NONE', #55759, 32.13701971169416538 ) ;
#14550 = CARTESIAN_POINT ( 'NONE',  ( -25.71573637233310095, 1509.811073689510067, 223.1001859706680079 ) ) ;
#14551 = CARTESIAN_POINT ( 'NONE',  ( 11.81707110430000007, 1430.266231075130008, 147.2485970657980090 ) ) ;
#14552 = ORIENTED_EDGE ( 'NONE', *, *, #4232, .F. ) ;
#14553 = CARTESIAN_POINT ( 'NONE',  ( -0.1681681984989999989, 1420.473120458229914, 179.3023655596979893 ) ) ;
#14554 = FACE_OUTER_BOUND ( 'NONE', #92326, .T. ) ;
#14555 = CARTESIAN_POINT ( 'NONE',  ( -97.11742683014449540, 1384.953084665809911, 310.4397664338810046 ) ) ;
#14556 = CARTESIAN_POINT ( 'NONE',  ( -9.634077209289999999, 1386.855370323769876, 200.5463740245589861 ) ) ;
#14557 = CARTESIAN_POINT ( 'NONE',  ( 2.382436964801011303, 1426.901689560120076, 137.0999999980980135 ) ) ;
#14559 = ORIENTED_EDGE ( 'NONE', *, *, #20753, .T. ) ;
#14558 = CARTESIAN_POINT ( 'NONE',  ( 11.14534346802929932, 1422.715803301600090, 203.3389832068340013 ) ) ;
#14560 = CARTESIAN_POINT ( 'NONE',  ( 1.839725546759999775, 1430.652037411689889, 217.6678242507890104 ) ) ;
#14561 = CARTESIAN_POINT ( 'NONE',  ( -1.657615632539999773, 1440.444625599219989, 150.6406752848980091 ) ) ;
#14562 = EDGE_CURVE ( 'NONE', #106368, #78107, #41520, .T. ) ;
#14563 = CARTESIAN_POINT ( 'NONE',  ( -14.00875083269999877, 1416.819760292330102, 221.8514977783980271 ) ) ;
#14564 = CARTESIAN_POINT ( 'NONE',  ( 11.53532962319999911, 1433.771858699349877, 151.2647645120979973 ) ) ;
#14565 = CARTESIAN_POINT ( 'NONE',  ( 3.967440335210983271, 1431.784492063039352, 200.3531908705770093 ) ) ;
#14566 = CARTESIAN_POINT ( 'NONE',  ( 0.6359931820546259607, 1450.890027228909958, 181.3124269289969845 ) ) ;
#14567 = CARTESIAN_POINT ( 'NONE',  ( -30.31118248177353536, 1526.186458717539381, 201.5497466985122799 ) ) ;
#14568 = ADVANCED_FACE ( 'NONE', ( #19647 ), #42823, .T. ) ;
#14569 = CARTESIAN_POINT ( 'NONE',  ( 11.76598840989999850, 1428.979790717830156, 145.3128034382980047 ) ) ;
#14570 = CARTESIAN_POINT ( 'NONE',  ( -109.9857364230449974, 1384.899971927750130, 311.4562996732899478 ) ) ;
#14571 = CARTESIAN_POINT ( 'NONE',  ( 12.64400598149999944, 1419.760550675029890, 229.1492764728980092 ) ) ;
#14572 = CARTESIAN_POINT ( 'NONE',  ( 3.968827104744170331, 1517.051704408389924, 188.7040005449509863 ) ) ;
#14573 = CARTESIAN_POINT ( 'NONE',  ( 8.623178418239669796, 1441.178012935769857, 153.8582158081470084 ) ) ;
#14574 = CARTESIAN_POINT ( 'NONE',  ( -17.56312616970000207, 1409.691384886529931, 224.4360229823980148 ) ) ;
#14575 = VECTOR ( 'NONE', #51913, 1000.000000000000000 ) ;
#14576 = CARTESIAN_POINT ( 'NONE',  ( -0.7149693253490000400, 1422.352078937030001, 228.1616098511979942 ) ) ;
#14577 = CARTESIAN_POINT ( 'NONE',  ( -25.87590796830000173, 1449.884901504650088, 136.9990172420979775 ) ) ;
#14578 = DIRECTION ( 'NONE',  ( -0.9391860388032872153, -1.840964726716158065E-08, 0.3434087717531252304 ) ) ;
#14579 = CARTESIAN_POINT ( 'NONE',  ( 12.78701137800000076, 1416.830001031129996, 222.9175051919979751 ) ) ;
#14580 = CARTESIAN_POINT ( 'NONE',  ( 12.67629937430701936, 1426.478869958664063, 202.7079000866955028 ) ) ;
#14581 = EDGE_CURVE ( 'NONE', #94751, #25667, #106950, .T. ) ;
#14582 = CARTESIAN_POINT ( 'NONE',  ( 20.33508568879010170, 1432.834458530000120, 214.7556887718170060 ) ) ;
#14583 = CARTESIAN_POINT ( 'NONE',  ( -3.346430209710000270, 1414.913060387329779, 225.7371794378979928 ) ) ;
#14584 = CARTESIAN_POINT ( 'NONE',  ( 0.2075961268654689940, 1458.701262879619890, 183.0088039633720030 ) ) ;
#14586 = EDGE_LOOP ( 'NONE', ( #51294, #61822, #95993, #26911 ) ) ;
#14585 = CARTESIAN_POINT ( 'NONE',  ( -5.629143959155359589, 1407.138657505239962, 221.3608015446720003 ) ) ;
#14587 = CARTESIAN_POINT ( 'NONE',  ( -0.3973340087122340103, 1418.672806152889962, 184.7148007238050127 ) ) ;
#14588 = ADVANCED_FACE ( 'NONE', ( #108056 ), #6150, .T. ) ;
#14589 = CARTESIAN_POINT ( 'NONE',  ( -27.78452750130110260, 1508.000976266860107, 210.4681927182890036 ) ) ;
#14590 = CARTESIAN_POINT ( 'NONE',  ( 11.87926624510000018, 1433.311557364369946, 149.0256386714980010 ) ) ;
#14591 = CARTESIAN_POINT ( 'NONE',  ( -11.18562212430000002, 1414.421228241719973, 212.6817167181389721 ) ) ;
#14592 = CARTESIAN_POINT ( 'NONE',  ( 2.175409717514719593E-31, 1397.551704408390151, 209.1218459616989946 ) ) ;
#14593 = ORIENTED_EDGE ( 'NONE', *, *, #23305, .T. ) ;
#14594 = CARTESIAN_POINT ( 'NONE',  ( -16.99775931995139189, 1524.964230758882877, 181.1932721696053079 ) ) ;
#14595 = CARTESIAN_POINT ( 'NONE',  ( 2.470168522033036496, 1523.481610118015169, 175.3649660273507607 ) ) ;
#14596 = CARTESIAN_POINT ( 'NONE',  ( 26.78807150899999812, 1436.761941354120154, 136.7824147662979897 ) ) ;
#14597 = CARTESIAN_POINT ( 'NONE',  ( -11.01499743910000007, 1491.713862414889718, 209.6260353422130152 ) ) ;
#14599 = ADVANCED_FACE ( 'NONE', ( #56573 ), #82315, .F. ) ;
#14598 = CARTESIAN_POINT ( 'NONE',  ( -0.3328314641405109575, 1452.976685807730291, 183.2631399573310205 ) ) ;
#14600 = CARTESIAN_POINT ( 'NONE',  ( 14.96949722733650034, 1508.714436942260136, 232.5787688410800058 ) ) ;
#14601 = CARTESIAN_POINT ( 'NONE',  ( 29.75796374405569367, 1414.999058895863755, 269.3609185650325912 ) ) ;
#14602 = CARTESIAN_POINT ( 'NONE',  ( 21.99073835760000151, 1489.474306034229812, 209.8571700393559922 ) ) ;
#14603 = CARTESIAN_POINT ( 'NONE',  ( 2.372478608332516892, 1522.862737210649811, 243.3440112565233449 ) ) ;
#14604 = CARTESIAN_POINT ( 'NONE',  ( 2.500000004270000353, 1431.428399487389925, 183.6496936308980139 ) ) ;
#14605 = CARTESIAN_POINT ( 'NONE',  ( -62.23936251973370304, 1385.072491325380042, 248.8854521166869915 ) ) ;
#14606 = MECHANICAL_DESIGN_GEOMETRIC_PRESENTATION_REPRESENTATION (  '', ( #39642 ), #34280 ) ;
#14607 = CARTESIAN_POINT ( 'NONE',  ( -12.24955825400350129, 1490.502947928989897, 208.7174997126320193 ) ) ;
#14608 = CARTESIAN_POINT ( 'NONE',  ( -4.751625979119149967, 1508.551704408389924, 205.5757039018049852 ) ) ;
#14609 = ORIENTED_EDGE ( 'NONE', *, *, #28120, .T. ) ;
#14610 = CARTESIAN_POINT ( 'NONE',  ( -27.26775544359999870, 1450.672803855060010, 136.4409915286979924 ) ) ;
#14611 = ADVANCED_FACE ( 'NONE', ( #39766 ), #73926, .F. ) ;
#14612 = EDGE_CURVE ( 'NONE', #55821, #101169, #98554, .T. ) ;
#14613 = CARTESIAN_POINT ( 'NONE',  ( -16.62210571749790233, 1410.725220498880162, 226.5039651633489939 ) ) ;
#14615 = ORIENTED_EDGE ( 'NONE', *, *, #7519, .F. ) ;
#14614 = CARTESIAN_POINT ( 'NONE',  ( -1.254332924399999882, 1509.200097453389844, 218.0171178735590161 ) ) ;
#14616 = CARTESIAN_POINT ( 'NONE',  ( -12.17829449539999942, 1509.277426923929852, 182.3210652022980014 ) ) ;
#14617 = CARTESIAN_POINT ( 'NONE',  ( 10.18337656697590177, 1470.443896296289950, 210.2471389431320006 ) ) ;
#14618 = CARTESIAN_POINT ( 'NONE',  ( 21.23228481039999949, 1508.977225803030024, 226.2585636259979935 ) ) ;
#14619 = CARTESIAN_POINT ( 'NONE',  ( -109.8144715679999877, 1384.521880215379952, 311.3640776482590127 ) ) ;
#14620 = CARTESIAN_POINT ( 'NONE',  ( -11.00301372470000061, 1492.094802143589959, 210.0154403701209844 ) ) ;
#14621 = CARTESIAN_POINT ( 'NONE',  ( 1.236506327399999883, 1466.454922307530069, 235.1997163242980093 ) ) ;
#14622 = CARTESIAN_POINT ( 'NONE',  ( 20.12362348629999786, 1409.615792804430157, 216.8331973927680281 ) ) ;
#14623 = CARTESIAN_POINT ( 'NONE',  ( -1.979485596885299792, 1414.929432389800013, 186.0262034026189895 ) ) ;
#14624 = CARTESIAN_POINT ( 'NONE',  ( -15.98001441509999943, 1422.636699047329785, 227.8263916563979876 ) ) ;
#14626 = CARTESIAN_POINT ( 'NONE',  ( -20.71343476517554905, 1501.977400791986611, 179.9059455038197086 ) ) ;
#14625 = LINE ( 'NONE', #98630, #38912 ) ;
#14627 = CARTESIAN_POINT ( 'NONE',  ( 27.33115299130880160, 1488.742645355629975, 208.2830191072760044 ) ) ;
#14628 = CARTESIAN_POINT ( 'NONE',  ( -98.25428012471454053, 1340.114449826970258, 312.4959906388990589 ) ) ;
#14629 = CARTESIAN_POINT ( 'NONE',  ( 22.81443202775711754, 1509.728776510858552, 190.2493757223895727 ) ) ;
#14630 = CARTESIAN_POINT ( 'NONE',  ( -0.9329003126829999992, 1416.492614553930025, 233.5735679209980162 ) ) ;
#14631 = CARTESIAN_POINT ( 'NONE',  ( -4.745098151930000618, 1360.923919868589792, 210.6218459616991936 ) ) ;
#14632 = AXIS2_PLACEMENT_3D ( 'NONE', #63408, #80726, #72343 ) ;
#14633 = CARTESIAN_POINT ( 'NONE',  ( -6.949265684145000677, 1517.089216728169959, 205.6689289091970068 ) ) ;
#14634 = CARTESIAN_POINT ( 'NONE',  ( -18.26675480510339966, 1424.840341062940070, 227.6848255537819909 ) ) ;
#14635 = ORIENTED_EDGE ( 'NONE', *, *, #90472, .T. ) ;
#14636 = ADVANCED_FACE ( 'NONE', ( #65536 ), #99642, .F. ) ;
#14637 = DIRECTION ( 'NONE',  ( 0.4882662618185301118, -0.4884709562387606896, -0.7231819843448463736 ) ) ;
#14638 = CARTESIAN_POINT ( 'NONE',  ( -4.248370253443329858, 1441.364699328089955, 161.3861545258119747 ) ) ;
#14640 = ORIENTED_EDGE ( 'NONE', *, *, #107504, .F. ) ;
#14639 = CARTESIAN_POINT ( 'NONE',  ( -68.45375916347519762, 1379.747171630710000, 280.0545672679439804 ) ) ;
#14641 = ORIENTED_EDGE ( 'NONE', *, *, #65688, .F. ) ;
#14642 = CARTESIAN_POINT ( 'NONE',  ( -8.226710716830746506, 1382.151431053786609, 218.4368142409218194 ) ) ;
#14643 = ORIENTED_EDGE ( 'NONE', *, *, #65595, .F. ) ;
#14644 = CARTESIAN_POINT ( 'NONE',  ( -2.298816259811510054, 1486.462377102800019, 220.8289805423670202 ) ) ;
#14645 = CARTESIAN_POINT ( 'NONE',  ( 11.29999465100000045, 1500.851204880689920, 206.6218521946089766 ) ) ;
#14647 = CARTESIAN_POINT ( 'NONE',  ( 15.78629296034880092, 1410.112424319529964, 191.7210461700169901 ) ) ;
#14646 = CARTESIAN_POINT ( 'NONE',  ( -11.16292084342922486, 1425.155877134990533, 144.6903838373057454 ) ) ;
#14648 = CARTESIAN_POINT ( 'NONE',  ( 6.952166382295000169, 1517.213554313520035, 210.8305935944869987 ) ) ;
#14649 = CARTESIAN_POINT ( 'NONE',  ( -17.83486663330526767, 1523.678648413191695, 180.3677388339002334 ) ) ;
#14650 = AXIS2_PLACEMENT_3D ( 'NONE', #43659, #85087, #8378 ) ;
#14651 = CARTESIAN_POINT ( 'NONE',  ( -107.7594617770490117, 1378.913060387289988, 308.1713896475600336 ) ) ;
#14652 = CARTESIAN_POINT ( 'NONE',  ( 32.02808312589922224, 1511.187213306747708, 219.9649204700462235 ) ) ;
#14653 = CARTESIAN_POINT ( 'NONE',  ( 12.69768439988109954, 1500.465451651789863, 208.8630517188479985 ) ) ;
#14654 =( LENGTH_UNIT ( ) NAMED_UNIT ( * ) SI_UNIT ( .MILLI., .METRE. ) );
#14655 = CARTESIAN_POINT ( 'NONE',  ( 38.02701353894249792, 1450.427746997079794, 134.0999999984749991 ) ) ;
#14656 = DIRECTION ( 'NONE',  ( 0.000000000000000000, 0.000000000000000000, -1.000000000000000000 ) ) ;
#14657 = CARTESIAN_POINT ( 'NONE',  ( -18.80013861839099931, 1505.319286544219949, 222.5373194665829999 ) ) ;
#14658 = CARTESIAN_POINT ( 'NONE',  ( -42.06231979437640689, 1440.913089571769888, 269.6487552725350270 ) ) ;
#14659 = ORIENTED_EDGE ( 'NONE', *, *, #37893, .T. ) ;
#14660 = ORIENTED_EDGE ( 'NONE', *, *, #6976, .F. ) ;
#14661 = CARTESIAN_POINT ( 'NONE',  ( -6.055196954515000840, 1514.134513140259969, 216.7673245375070223 ) ) ;
#14662 = CARTESIAN_POINT ( 'NONE',  ( 10.56204787542680101, 1452.677117374779982, 209.7945773243330052 ) ) ;
#14663 = CARTESIAN_POINT ( 'NONE',  ( 11.55221588404359956, 1480.217597516799970, 211.4789165460060190 ) ) ;
#14664 = CARTESIAN_POINT ( 'NONE',  ( -21.12755052628529739, 1507.992901756090077, 209.5250462511280034 ) ) ;
#14665 = CARTESIAN_POINT ( 'NONE',  ( -2.500000000000000000, 1439.588444403090080, 166.1975935960979882 ) ) ;
#14667 = DIRECTION ( 'NONE',  ( -0.000000000000000000, -1.000000000000000000, -0.000000000000000000 ) ) ;
#14666 = VECTOR ( 'NONE', #38001, 1000.000000000000000 ) ;
#14668 = CARTESIAN_POINT ( 'NONE',  ( 12.53380745427929988, 1442.773887455719887, 186.4115735415020083 ) ) ;
#14669 = CARTESIAN_POINT ( 'NONE',  ( 36.37832874669670247, 1451.642701154630004, 134.4205496038819945 ) ) ;
#14670 = CARTESIAN_POINT ( 'NONE',  ( -18.29243834081962206, 1484.963126390134676, 219.4937029363345573 ) ) ;
#14671 = CARTESIAN_POINT ( 'NONE',  ( 25.59635045179999580, 1439.616312306700138, 138.2644159780979862 ) ) ;
#14672 = CARTESIAN_POINT ( 'NONE',  ( 5.681577933589999851, 1414.971279908829956, 193.1266172032979966 ) ) ;
#14673 = CARTESIAN_POINT ( 'NONE',  ( -80.90462325147591116, 1384.798765408159852, 284.2668994243870202 ) ) ;
#14674 = ORIENTED_EDGE ( 'NONE', *, *, #78062, .T. ) ;
#14675 = VECTOR ( 'NONE', #55034, 1000.000000000000000 ) ;
#14676 = CARTESIAN_POINT ( 'NONE',  ( 5.778372563615000068, 1516.932669162149978, 202.1763558832970205 ) ) ;
#14677 = CARTESIAN_POINT ( 'NONE',  ( 3.449647440015000122, 1516.829948096479939, 208.3645479958780129 ) ) ;
#14678 = VERTEX_POINT ( 'NONE', #40306 ) ;
#14679 = CARTESIAN_POINT ( 'NONE',  ( 40.65972102606890104, 1440.913060387330006, 268.1254238195359676 ) ) ;
#14680 = CARTESIAN_POINT ( 'NONE',  ( -0.001314202166405476846, 1451.878195095055389, 154.0173218471571488 ) ) ;
#14681 = EDGE_LOOP ( 'NONE', ( #77189, #60144, #51166, #24450, #29333 ) ) ;
#14682 = CARTESIAN_POINT ( 'NONE',  ( -0.2068025458765339886, 1451.165312576740007, 182.5378010495940089 ) ) ;
#14683 = DIRECTION ( 'NONE',  ( 0.000000000000000000, 0.000000000000000000, 1.000000000000000000 ) ) ;
#14684 = CARTESIAN_POINT ( 'NONE',  ( -18.22821675530000007, 1443.229620277490085, 204.5519556382290034 ) ) ;
#14685 = FACE_OUTER_BOUND ( 'NONE', #26789, .T. ) ;
#14686 = CARTESIAN_POINT ( 'NONE',  ( -13.25650536310000049, 1429.127351718030013, 222.3136094715979993 ) ) ;
#14687 = CARTESIAN_POINT ( 'NONE',  ( 12.95816640841469969, 1435.988574857560025, 150.7628740217149925 ) ) ;
#14688 = CARTESIAN_POINT ( 'NONE',  ( -0.6813215632989999548, 1508.998955527629960, 179.3434203495980057 ) ) ;
#14689 = CARTESIAN_POINT ( 'NONE',  ( -13.50155420119999938, 1434.968988600790226, 146.4346116559979976 ) ) ;
#14690 = LINE ( 'NONE', #83004, #75042 ) ;
#14692 = CARTESIAN_POINT ( 'NONE',  ( -11.60004869885203682, 1422.222932908413441, 135.5999999980978714 ) ) ;
#14691 = CARTESIAN_POINT ( 'NONE',  ( 14.97860510539999979, 1460.097680310830128, 231.5368076450980084 ) ) ;
#14693 = CARTESIAN_POINT ( 'NONE',  ( 20.08195036849999937, 1474.154268156089984, 211.0972226708090034 ) ) ;
#14694 = CARTESIAN_POINT ( 'NONE',  ( 0.5133626083067620582, 1410.311097044259895, 185.0719925509139898 ) ) ;
#14695 = VERTEX_POINT ( 'NONE', #108616 ) ;
#14696 = CARTESIAN_POINT ( 'NONE',  ( -22.71973404851811651, 1409.706432500549909, 209.0865126238462892 ) ) ;
#14697 = CARTESIAN_POINT ( 'NONE',  ( -0.06152828947505290663, 1508.663433079589822, 180.0530326742579916 ) ) ;
#14698 = CARTESIAN_POINT ( 'NONE',  ( 0.8837376337392799375, 1516.687471173209360, 216.8348885015759038 ) ) ;
#14699 = CARTESIAN_POINT ( 'NONE',  ( 3.460101851884999746, 1516.812923327049930, 213.1504765548870068 ) ) ;
#14700 = CARTESIAN_POINT ( 'NONE',  ( 2.958097658348910031, 1515.068899390480283, 213.4512612428040086 ) ) ;
#14701 = CARTESIAN_POINT ( 'NONE',  ( -11.60004869885203682, 1425.267055893744555, 138.0405467508053050 ) ) ;
#14703 = ORIENTED_EDGE ( 'NONE', *, *, #9048, .T. ) ;
#14702 = CARTESIAN_POINT ( 'NONE',  ( -3.829620113550000315, 1515.551704408389924, 211.4519800877889963 ) ) ;
#14704 = FACE_OUTER_BOUND ( 'NONE', #34723, .T. ) ;
#14705 = CARTESIAN_POINT ( 'NONE',  ( 22.61371014190000039, 1448.753361709010051, 213.3230883210279956 ) ) ;
#14706 = EDGE_CURVE ( 'NONE', #67085, #103816, #42913, .T. ) ;
#14707 = CARTESIAN_POINT ( 'NONE',  ( -11.28722548159999839, 1431.252270778690217, 151.4401771847979887 ) ) ;
#14708 = CARTESIAN_POINT ( 'NONE',  ( 19.09768422228310314, 1456.930751240180143, 225.1426474012400263 ) ) ;
#14709 = CARTESIAN_POINT ( 'NONE',  ( -5.209734426898009474, 1441.765094112799943, 201.7747637104849900 ) ) ;
#14710 = CARTESIAN_POINT ( 'NONE',  ( 27.01916870379659841, 1450.861785352695961, 136.4169503727333392 ) ) ;
#14711 = CARTESIAN_POINT ( 'NONE',  ( 16.53175237172159839, 1526.069472839387117, 182.3016483747060761 ) ) ;
#14712 = CARTESIAN_POINT ( 'NONE',  ( -8.630935213989998189, 1438.255193345089992, 208.1083423884190040 ) ) ;
#14714 = CARTESIAN_POINT ( 'NONE',  ( 7.211935934568220574, 1517.151704408390060, 224.6757451961901495 ) ) ;
#14713 = CARTESIAN_POINT ( 'NONE',  ( -20.18632372599999769, 1482.730689116930080, 226.9986024029979887 ) ) ;
#14715 = CARTESIAN_POINT ( 'NONE',  ( -2.041421758439999845, 1485.165825108230138, 182.8125668122980017 ) ) ;
#14716 = VERTEX_POINT ( 'NONE', #77238 ) ;
#14717 = CARTESIAN_POINT ( 'NONE',  ( 3.446942071715000111, 1516.842852731759876, 205.8545543269370057 ) ) ;
#14718 = CARTESIAN_POINT ( 'NONE',  ( 12.63282632850000020, 1407.538329530530063, 269.2355767699979765 ) ) ;
#14719 = CARTESIAN_POINT ( 'NONE',  ( 38.62985698226480480, 1443.711942198199949, 137.1840658525169943 ) ) ;
#14720 = LINE ( 'NONE', #83038, #58552 ) ;
#14721 = DIRECTION ( 'NONE',  ( 1.000000000000000000, 0.000000000000000000, 0.000000000000000000 ) ) ;
#14722 = DIRECTION ( 'NONE',  ( 0.4794255386042028388, 0.000000000000000000, 0.8775825618903727587 ) ) ;
#14723 =( BOUNDED_CURVE ( )  B_SPLINE_CURVE ( 3, ( #84201, #56808, #100453, #99885 ),
 .UNSPECIFIED., .F., .F. ) 
 B_SPLINE_CURVE_WITH_KNOTS ( ( 4, 4 ),
 ( 1.168456980160074821, 1.504276012154933673 ),
 .UNSPECIFIED. ) 
 CURVE ( )  GEOMETRIC_REPRESENTATION_ITEM ( )  RATIONAL_B_SPLINE_CURVE ( ( 1.000000000000000000, 0.9906241907223192200, 0.9906241907223192200, 1.000000000000000000 ) ) 
 REPRESENTATION_ITEM ( '' )  );
#14724 = CARTESIAN_POINT ( 'NONE',  ( 11.86716023049999968, 1432.353341358199941, 147.6509521729980179 ) ) ;
#14725 = CARTESIAN_POINT ( 'NONE',  ( -9.954727031183750796, 1446.941805363540198, 211.8349694523599851 ) ) ;
#14726 = CARTESIAN_POINT ( 'NONE',  ( -2.431405112757329956, 1449.537433628249801, 154.7921730761810011 ) ) ;
#14727 = B_SPLINE_CURVE_WITH_KNOTS ( 'NONE', 3,
 ( #47906, #98298, #21574, #3726, #72567, #97196, #13721, #37856, #63635, #106159, #97749, #21020, #55224, #89354 ),
 .UNSPECIFIED., .F., .F.,
 ( 4, 2, 2, 2, 2, 2, 4 ),
 ( 0.000000000000000000, 0.2499999999999116262, 0.4999999999998232525, 0.6249999999997172262, 0.6874999999997223332, 0.7499999999997273292, 1.000000000000000000 ),
 .UNSPECIFIED. ) ;
#14728 = CARTESIAN_POINT ( 'NONE',  ( -1.620797157046767856, 1450.704051676946619, 183.2587108462243748 ) ) ;
#14729 = EDGE_CURVE ( 'NONE', #43735, #37608, #43630, .T. ) ;
#14730 = FACE_OUTER_BOUND ( 'NONE', #103844, .T. ) ;
#14731 = CARTESIAN_POINT ( 'NONE',  ( -14.45556168306239897, 1416.765224586759814, 221.3896323238510035 ) ) ;
#14732 = DIRECTION ( 'NONE',  ( 0.03489949670247471936, -0.9993908270190967613, 3.814740354449985581E-14 ) ) ;
#14733 = CARTESIAN_POINT ( 'NONE',  ( -3.268607721189999982, 1425.981674306129889, 219.6133833292979887 ) ) ;
#14735 = ADVANCED_FACE ( 'NONE', ( #87281 ), #95682, .F. ) ;
#14734 = DIRECTION ( 'NONE',  ( 0.9125304618753967700, 0.000000000000000000, -0.4090087482554317089 ) ) ;
#14736 = CARTESIAN_POINT ( 'NONE',  ( 2.704768305889999613, 1440.770142154440009, 166.9241121263980006 ) ) ;
#14737 = CARTESIAN_POINT ( 'NONE',  ( -1.778075049280000153, 1476.051869520629907, 267.5358627141980037 ) ) ;
#14738 = CARTESIAN_POINT ( 'NONE',  ( -11.28161544973855612, 1425.477714925698820, 138.6342417071923592 ) ) ;
#14739 = CARTESIAN_POINT ( 'NONE',  ( 9.699838620905369524, 1453.359120950689885, 212.1672243862410028 ) ) ;
#14740 = CARTESIAN_POINT ( 'NONE',  ( 18.05970663803819676, 1417.701653607439994, 223.4092527363580132 ) ) ;
#14741 = CARTESIAN_POINT ( 'NONE',  ( -43.87927512900789395, 1384.769549923549903, 249.3322899781709907 ) ) ;
#14742 = CARTESIAN_POINT ( 'NONE',  ( -107.0856175946619970, 1391.913060387289988, 301.5308894922570175 ) ) ;
#14743 = CIRCLE ( 'NONE', #57624, 2.000000000062579275 ) ;
#14744 = CARTESIAN_POINT ( 'NONE',  ( -4.380123784945419985, 1517.051697240460271, 216.5788674826960118 ) ) ;
#14745 = EDGE_CURVE ( 'NONE', #75409, #91917, #62992, .T. ) ;
#14746 = CARTESIAN_POINT ( 'NONE',  ( -105.5765342570000058, 1378.949837160079824, 302.9213429863589795 ) ) ;
#14747 = CARTESIAN_POINT ( 'NONE',  ( 31.54872587855177102, 1525.317359687841190, 216.6695404376949057 ) ) ;
#14748 = CARTESIAN_POINT ( 'NONE',  ( 8.115348803788476673, 1511.538158271185011, 205.3742513834712611 ) ) ;
#14749 = CARTESIAN_POINT ( 'NONE',  ( -0.4983014274912969666, 1395.930461456620151, 220.1163257280059895 ) ) ;
#14750 = CARTESIAN_POINT ( 'NONE',  ( 12.91792090909249779, 1421.070795045020077, 203.9889279772430086 ) ) ;
#14751 = CARTESIAN_POINT ( 'NONE',  ( -43.43972853289999847, 1430.028892233129909, 269.0356351862979523 ) ) ;
#14752 = ORIENTED_EDGE ( 'NONE', *, *, #40626, .T. ) ;
#14753 = CARTESIAN_POINT ( 'NONE',  ( -2.372478608332516892, 1501.977400791986611, 243.3440112565233449 ) ) ;
#14754 = CARTESIAN_POINT ( 'NONE',  ( -13.59241398700699932, 1508.144654051440057, 209.5353803071969878 ) ) ;
#14755 = CARTESIAN_POINT ( 'NONE',  ( -0.7913646410377903617, 1426.918876941764893, 134.0999999980979851 ) ) ;
#14757 = CARTESIAN_POINT ( 'NONE',  ( -14.87514316876499976, 1513.853571676670072, 194.0180321211670105 ) ) ;
#14756 = CARTESIAN_POINT ( 'NONE',  ( 11.57203810419999890, 1425.906236901130114, 139.6353521643979718 ) ) ;
#14758 = CARTESIAN_POINT ( 'NONE',  ( 17.24701803731020888, 1523.844789899202851, 237.3932575341077325 ) ) ;
#14759 = DIRECTION ( 'NONE',  ( 0.000000000000000000, 1.000000000000000000, 0.000000000000000000 ) ) ;
#14760 = CARTESIAN_POINT ( 'NONE',  ( 39.49614528243539979, 1448.959577479020027, 136.3036146745320139 ) ) ;
#14761 = CARTESIAN_POINT ( 'NONE',  ( 4.034280915654999689, 1517.049325831759916, 202.1735242262370207 ) ) ;
#14762 = CARTESIAN_POINT ( 'NONE',  ( 8.034189947220001571, 1427.422895264749968, 212.2991858979890196 ) ) ;
#14763 = CARTESIAN_POINT ( 'NONE',  ( -12.60062663947178407, 1398.286608578669757, 212.3194447688631499 ) ) ;
#14765 = CARTESIAN_POINT ( 'NONE',  ( 15.82925651883499896, 1512.053076656670100, 196.3893797332669919 ) ) ;
#14764 = B_SPLINE_CURVE_WITH_KNOTS ( 'NONE', 3,
 ( #89643, #72322, #47654, #107548, #46022, #81782, #12929, #37598, #5084, #22406, #90743, #11849, #71800, #63388, #75621, #92946, #67768, #50421, #25172, #85089, #7295, #91298, #33576, #6733, #100254, #99678, #66132, #14580 ),
 .UNSPECIFIED., .F., .F.,
 ( 4, 3, 3, 3, 3, 3, 3, 3, 3, 4 ),
 ( -25.30278714349060110, -25.16708866733689831, -24.99913445276009938, -24.69548176202949819, -24.08817638056840238, -23.17766623311220187, -22.54008017006870190, -21.79135080256759949, -20.68911956487800197, -19.77745725219000050 ),
 .UNSPECIFIED. ) ;
#14766 = CARTESIAN_POINT ( 'NONE',  ( -16.43468781389340094, 1420.643514338609975, 203.2794736519120136 ) ) ;
#14767 = CARTESIAN_POINT ( 'NONE',  ( -27.34872825612519875, 1378.876396125770043, 217.1833578772759950 ) ) ;
#14768 = ADVANCED_FACE ( 'NONE', ( #45300 ), #61386, .F. ) ;
#14769 = CARTESIAN_POINT ( 'NONE',  ( 21.02092206099549898, 1509.698195058749889, 230.2140218131270046 ) ) ;
#14771 = VERTEX_POINT ( 'NONE', #20596 ) ;
#14770 = CARTESIAN_POINT ( 'NONE',  ( -31.51240728630000376, 1379.723496875969886, 219.1466601182590068 ) ) ;
#14772 = EDGE_LOOP ( 'NONE', ( #82970, #26827, #50053, #49143 ) ) ;
#14773 = CARTESIAN_POINT ( 'NONE',  ( 12.04367873614740070, 1433.833094619370058, 150.1136006245660042 ) ) ;
#14774 = CARTESIAN_POINT ( 'NONE',  ( -12.05715834750000148, 1396.854116735730031, 212.7715747960579904 ) ) ;
#14775 = CARTESIAN_POINT ( 'NONE',  ( -19.57217229339999776, 1409.761027581930193, 220.5029208888979895 ) ) ;
#14776 = ORIENTED_EDGE ( 'NONE', *, *, #28893, .F. ) ;
#14777 = CARTESIAN_POINT ( 'NONE',  ( -12.53380499174499896, 1445.052233488290085, 169.4755105688890069 ) ) ;
#14778 = CARTESIAN_POINT ( 'NONE',  ( 20.81322922288373434, 1509.688917493156396, 230.4060755301925667 ) ) ;
#14779 = DIRECTION ( 'NONE',  ( -0.9455185755993178454, 0.000000000000000000, 0.3255681544571537578 ) ) ;
#14782 = EDGE_CURVE ( 'NONE', #24877, #79432, #101580, .T. ) ;
#14781 = CARTESIAN_POINT ( 'NONE',  ( -13.70767992804610103, 1507.681782264339972, 184.2567517037919913 ) ) ;
#14780 = DIRECTION ( 'NONE',  ( 0.03489949888733943212, -0.1170789740109212107, 0.9925092134695590040 ) ) ;
#14783 = CARTESIAN_POINT ( 'NONE',  ( 2.434134029640000030, 1449.238291734089898, 183.8493297274980023 ) ) ;
#14784 = CARTESIAN_POINT ( 'NONE',  ( -12.22918613309999891, 1416.219761279530076, 194.7382282326980203 ) ) ;
#14785 = CARTESIAN_POINT ( 'NONE',  ( 2.548339227810000107, 1419.358184697269962, 204.5809049373789890 ) ) ;
#14786 =( NAMED_UNIT ( * ) PLANE_ANGLE_UNIT ( ) SI_UNIT ( $, .RADIAN. ) );
#14787 = CARTESIAN_POINT ( 'NONE',  ( 10.81872853871839979, 1396.290858712909994, 206.7702252306009711 ) ) ;
#14788 = CARTESIAN_POINT ( 'NONE',  ( -1.458875156116091532, 1414.913372219064286, 226.1171707424567785 ) ) ;
#14789 = DIRECTION ( 'NONE',  ( -5.980589973904019347E-17, 1.000000000000000000, -1.736889445713099699E-16 ) ) ;
#14790 = CARTESIAN_POINT ( 'NONE',  ( 30.31940284292409515, 1523.382868172864164, 195.7503880523414352 ) ) ;
#14791 = ORIENTED_EDGE ( 'NONE', *, *, #57648, .F. ) ;
#14792 = CARTESIAN_POINT ( 'NONE',  ( 13.00929752435379960, 1434.785411124280017, 149.1497742818210099 ) ) ;
#14793 = ORIENTED_EDGE ( 'NONE', *, *, #106659, .T. ) ;
#14794 = EDGE_LOOP ( 'NONE', ( #23752, #91040, #51857, #109550 ) ) ;
#14795 = CARTESIAN_POINT ( 'NONE',  ( -12.99775963039999915, 1420.302662752830201, 196.1023006302990268 ) ) ;
#14796 = CARTESIAN_POINT ( 'NONE',  ( -6.816513146730000194, 1465.924515906329816, 233.8132117517980078 ) ) ;
#14797 = CARTESIAN_POINT ( 'NONE',  ( -107.4877904035150067, 1389.702161918033880, 309.4250478887230997 ) ) ;
#14798 = CARTESIAN_POINT ( 'NONE',  ( 4.618119666265000589, 1516.706638732659940, 216.0591847158069925 ) ) ;
#14799 = CARTESIAN_POINT ( 'NONE',  ( -12.63531666014029931, 1379.388864909599988, 208.8707713015120078 ) ) ;
#14800 = VERTEX_POINT ( 'NONE', #106819 ) ;
#14801 = CARTESIAN_POINT ( 'NONE',  ( -13.19474177440000062, 1503.345007237690197, 208.6791437603130248 ) ) ;
#14802 = DIRECTION ( 'NONE',  ( -0.8907681516580507886, 0.000000000000000000, 0.4544580288560209347 ) ) ;
#14803 = CARTESIAN_POINT ( 'NONE',  ( -36.43074434249999172, 1380.172836988449944, 219.9641098163590129 ) ) ;
#14804 = ORIENTED_EDGE ( 'NONE', *, *, #105498, .T. ) ;
#14805 = CARTESIAN_POINT ( 'NONE',  ( 2.865588684285000021, 1516.890356958860139, 205.8536102114670143 ) ) ;
#14806 = ORIENTED_EDGE ( 'NONE', *, *, #50033, .F. ) ;
#14807 = CARTESIAN_POINT ( 'NONE',  ( -7.719640941135000212, 1516.939452820819952, 209.1319487995289705 ) ) ;
#14808 = CARTESIAN_POINT ( 'NONE',  ( -7.587902012781059469, 1453.124660370870060, 203.6743039436619824 ) ) ;
#14809 = CARTESIAN_POINT ( 'NONE',  ( -29.83131695263168837, 1419.453406920455336, 269.4690164430861614 ) ) ;
#14810 = CARTESIAN_POINT ( 'NONE',  ( -2.286415621570000223, 1410.371193408130011, 232.7320840571979943 ) ) ;
#14812 = ORIENTED_EDGE ( 'NONE', *, *, #99379, .F. ) ;
#14811 = CARTESIAN_POINT ( 'NONE',  ( -0.8265315298756289453, 1415.089948427370018, 226.4875429796719857 ) ) ;
#14813 = CARTESIAN_POINT ( 'NONE',  ( 24.62909011900000067, 1439.532667989389893, 212.3621347402479955 ) ) ;
#14814 = CARTESIAN_POINT ( 'NONE',  ( -34.94693337376789799, 1440.913060388619897, 250.8280191517029891 ) ) ;
#14815 = CARTESIAN_POINT ( 'NONE',  ( -32.14702491180000266, 1384.162411493540048, 229.9166993473590139 ) ) ;
#14816 = CARTESIAN_POINT ( 'NONE',  ( -0.3779027989101099716, 1465.092193578540218, 236.9869935022780112 ) ) ;
#14817 = CARTESIAN_POINT ( 'NONE',  ( 10.49062974637460144, 1411.164843042819939, 269.6264656941679618 ) ) ;
#14818 = CARTESIAN_POINT ( 'NONE',  ( -4.611879723454999969, 1516.858533673840157, 213.7437437946470027 ) ) ;
#14819 = CARTESIAN_POINT ( 'NONE',  ( 23.51425668899999621, 1409.991808817929950, 208.7354357160110112 ) ) ;
#14820 = CARTESIAN_POINT ( 'NONE',  ( -21.25388494759999958, 1509.593767402129970, 188.9414823285979992 ) ) ;
#14821 = CARTESIAN_POINT ( 'NONE',  ( 2.792478474500000196, 1441.472946933690082, 218.6424847214589988 ) ) ;
#14822 = CARTESIAN_POINT ( 'NONE',  ( -11.60004869885203682, 1424.920234265779300, 136.4497806840202827 ) ) ;
#14823 = CARTESIAN_POINT ( 'NONE',  ( 6.952166382295000169, 1517.213554313520035, 210.8305935944869987 ) ) ;
#14824 = CARTESIAN_POINT ( 'NONE',  ( -3.099034158239330150, 1447.528034658634169, 154.8291887632518922 ) ) ;
#14825 = CARTESIAN_POINT ( 'NONE',  ( 0.1542088501289999858, 1419.787199956130053, 184.3756093272979797 ) ) ;
#14826 = CARTESIAN_POINT ( 'NONE',  ( -11.61583318246324126, 1486.022327833872623, 184.5199211660089134 ) ) ;
#14828 = ORIENTED_EDGE ( 'NONE', *, *, #10415, .T. ) ;
#14827 = CARTESIAN_POINT ( 'NONE',  ( -69.40052021539999316, 1389.408898824169910, 290.4326261031590093 ) ) ;
#14829 = CARTESIAN_POINT ( 'NONE',  ( -40.13732683962579983, 1385.181215360810029, 242.3489691607209977 ) ) ;
#14830 = CARTESIAN_POINT ( 'NONE',  ( 44.59191286470000648, 1449.238683939599923, 266.2373440796980049 ) ) ;
#14831 = DIRECTION ( 'NONE',  ( -0.8775825618903712044, 0.000000000000000000, -0.4794255386042061140 ) ) ;
#14832 = CARTESIAN_POINT ( 'NONE',  ( -5.334367723879999801, 1417.997726539230143, 234.5082296770980008 ) ) ;
#14833 = CARTESIAN_POINT ( 'NONE',  ( -5.455799340109999562, 1438.116814643030011, 154.7280984898980307 ) ) ;
#14834 = CARTESIAN_POINT ( 'NONE',  ( 11.55388455309999962, 1425.897125911080138, 204.0276920965590080 ) ) ;
#14835 = DIRECTION ( 'NONE',  ( -1.000000000000000000, 0.000000000000000000, -1.989566177384290042E-13 ) ) ;
#14836 = APPLICATION_CONTEXT ( 'automotive_design' ) ;
#14838 = FACE_OUTER_BOUND ( 'NONE', #98381, .T. ) ;
#14837 = CARTESIAN_POINT ( 'NONE',  ( -3.452917061035000401, 1517.089216728169959, 216.0711116162470091 ) ) ;
#14839 = CARTESIAN_POINT ( 'NONE',  ( -25.25200574389469921, 1450.804213008409988, 137.6134964715130025 ) ) ;
#14840 = CARTESIAN_POINT ( 'NONE',  ( 10.36471150681333775, 1423.168727259207344, 137.2130303604900803 ) ) ;
#14841 = ORIENTED_EDGE ( 'NONE', *, *, #2290, .T. ) ;
#14842 = CARTESIAN_POINT ( 'NONE',  ( -5.781490582474999584, 1516.807958722750072, 202.5702025453269925 ) ) ;
#14843 = CARTESIAN_POINT ( 'NONE',  ( -16.72999346986500058, 1513.736060322949925, 223.1141918444669727 ) ) ;
#14844 = CARTESIAN_POINT ( 'NONE',  ( 0.08825444290579999296, 1477.418261180029958, 229.8744888911979842 ) ) ;
#14845 = CARTESIAN_POINT ( 'NONE',  ( -1.491506560153235128, 1512.187213306747481, 175.5704429466618421 ) ) ;
#14846 = CARTESIAN_POINT ( 'NONE',  ( 5.519893427111519202, 1440.499866072189889, 154.7645221071819890 ) ) ;
#14847 = CARTESIAN_POINT ( 'NONE',  ( 8.377797352699728251, 1424.395980914158827, 195.8294568783052512 ) ) ;
#14848 = CARTESIAN_POINT ( 'NONE',  ( -0.5525556504920010603, 1444.336369769489920, 218.0684148105289921 ) ) ;
#14849 = CARTESIAN_POINT ( 'NONE',  ( 12.93497730519910149, 1419.267168090624182, 228.9863995134908521 ) ) ;
#14850 = CARTESIAN_POINT ( 'NONE',  ( 40.24868989356649962, 1444.402556327009961, 137.0644448199289798 ) ) ;
#14851 = CARTESIAN_POINT ( 'NONE',  ( -20.17314850740000409, 1426.673360916329784, 222.1514211777979995 ) ) ;
#14852 = DIRECTION ( 'NONE',  ( -6.123233995736769734E-17, -1.000000000000000000, -1.124819836996399911E-32 ) ) ;
#14853 = CARTESIAN_POINT ( 'NONE',  ( -107.4403222199999988, 1387.882953355429891, 298.2873657394590055 ) ) ;
#14854 = EDGE_CURVE ( 'NONE', #86349, #107294, #10785, .T. ) ;
#14855 = CARTESIAN_POINT ( 'NONE',  ( -17.16924453729999911, 1410.829424874530105, 226.1263841768980001 ) ) ;
#14856 = CARTESIAN_POINT ( 'NONE',  ( -105.8808422670000056, 1391.420045099660001, 301.8793707204590078 ) ) ;
#14857 = CARTESIAN_POINT ( 'NONE',  ( -16.03274444936123899, 1469.111322135198634, 269.3691765490368653 ) ) ;
#14858 = ORIENTED_EDGE ( 'NONE', *, *, #3019, .F. ) ;
#14859 = DIRECTION ( 'NONE',  ( -0.9404331407594663794, 0.3018495643663520744, -0.1564364032222970435 ) ) ;
#14860 = CYLINDRICAL_SURFACE ( 'NONE', #94345, 2.000000000000003109 ) ;
#14861 = CARTESIAN_POINT ( 'NONE',  ( 32.72607202732672249, 1524.152444737676660, 201.1104170367456732 ) ) ;
#14862 = DIRECTION ( 'NONE',  ( 0.8775825618903687619, 0.000000000000000000, 0.4794255386042102218 ) ) ;
#14863 = CARTESIAN_POINT ( 'NONE',  ( -0.2732116802759999574, 1417.283604781830036, 234.8460454422980206 ) ) ;
#14864 = CARTESIAN_POINT ( 'NONE',  ( -13.44006708864586841, 1443.498725820041955, 187.0768896222344324 ) ) ;
#14865 = CARTESIAN_POINT ( 'NONE',  ( -8.640340473127709586, 1437.525024229920064, 208.5374257294450047 ) ) ;
#14866 = CARTESIAN_POINT ( 'NONE',  ( -4.325403553351909736, 1515.219291385429869, 211.4517448057640081 ) ) ;
#14867 = CARTESIAN_POINT ( 'NONE',  ( -4.273773890143617749, 1416.013655775612051, 232.3752477624281312 ) ) ;
#14869 = EDGE_CURVE ( 'NONE', #68723, #32820, #14406, .T. ) ;
#14868 = CARTESIAN_POINT ( 'NONE',  ( -14.73949824312500034, 1415.677402202700023, 206.3522687176919987 ) ) ;
#14870 = CARTESIAN_POINT ( 'NONE',  ( 17.33524322635545545, 1423.908641254848817, 228.7533431997620994 ) ) ;
#14871 = CARTESIAN_POINT ( 'NONE',  ( -12.58564406202428998, 1442.782412299425005, 169.4702538016106814 ) ) ;
#14873 = ORIENTED_EDGE ( 'NONE', *, *, #51415, .F. ) ;
#14872 = CARTESIAN_POINT ( 'NONE',  ( 18.11901460572769906, 1425.007341518409930, 225.3790264464149971 ) ) ;
#14874 = CARTESIAN_POINT ( 'NONE',  ( -0.2193365489855410022, 1416.521607925270018, 191.0676367320770055 ) ) ;
#14875 = CARTESIAN_POINT ( 'NONE',  ( -7.764017272732929520, 1409.184185844869944, 229.1854234326909818 ) ) ;
#14876 = EDGE_CURVE ( 'NONE', #14943, #108182, #100035, .T. ) ;
#14877 = ORIENTED_EDGE ( 'NONE', *, *, #31065, .F. ) ;
#14878 = ORIENTED_EDGE ( 'NONE', *, *, #107689, .F. ) ;
#14879 = CARTESIAN_POINT ( 'NONE',  ( -12.33110954549999860, 1502.406660704589740, 209.5022816524030134 ) ) ;
#14880 = CARTESIAN_POINT ( 'NONE',  ( 13.13145645029999997, 1509.139720533629998, 233.9873431947980009 ) ) ;
#14882 = CARTESIAN_POINT ( 'NONE',  ( -24.79040425310000018, 1444.204229992539922, 216.4501235802679844 ) ) ;
#14881 = CARTESIAN_POINT ( 'NONE',  ( 4.669122900610000571, 1455.239293656489963, 217.7735903674689837 ) ) ;
#14883 = CARTESIAN_POINT ( 'NONE',  ( -8.532458278280000030, 1445.788163739789979, 215.0754535007789912 ) ) ;
#14884 = CARTESIAN_POINT ( 'NONE',  ( -11.66444761839999877, 1433.408000155229956, 150.9992530625980010 ) ) ;
#14885 = CARTESIAN_POINT ( 'NONE',  ( -4.487249775048080203, 1509.038615934839981, 211.6097811040130239 ) ) ;
#14886 = CARTESIAN_POINT ( 'NONE',  ( 28.25086641300000068, 1508.135711190629991, 209.3856964555159834 ) ) ;
#14887 = CARTESIAN_POINT ( 'NONE',  ( -26.05361808410000179, 1437.534443763920081, 137.0219046968979910 ) ) ;
#14888 = CARTESIAN_POINT ( 'NONE',  ( -24.54165285250000039, 1438.756210186880026, 210.7135935008279830 ) ) ;
#14889 = FACE_BOUND ( 'NONE', #40270, .T. ) ;
#14890 = CARTESIAN_POINT ( 'NONE',  ( 1.228114143200000008, 1450.757138824929825, 181.5372585326979902 ) ) ;
#14891 = CARTESIAN_POINT ( 'NONE',  ( 7.243489813520766596, 1364.101810452927566, 209.6218459617148824 ) ) ;
#14892 = CARTESIAN_POINT ( 'NONE',  ( 34.61172972909988488, 1523.342713519622748, 200.0387150244870043 ) ) ;
#14894 = EDGE_LOOP ( 'NONE', ( #22705, #108452, #19846, #29392 ) ) ;
#14893 = CARTESIAN_POINT ( 'NONE',  ( 1.538781636355590080E-08, 1408.254370158240135, 262.4690811517129418 ) ) ;
#14895 = ORIENTED_EDGE ( 'NONE', *, *, #73385, .F. ) ;
#14896 = FACE_OUTER_BOUND ( 'NONE', #39182, .T. ) ;
#14897 = CARTESIAN_POINT ( 'NONE',  ( -18.92739547204800132, 1503.346040100430173, 222.1981696246060096 ) ) ;
#14898 = CARTESIAN_POINT ( 'NONE',  ( -3.409545297029999755, 1471.487073322530023, 269.6161692879980478 ) ) ;
#14899 = CARTESIAN_POINT ( 'NONE',  ( -3.282353412611801691, 1474.704843300428365, 218.8718926834540639 ) ) ;
#14901 = EDGE_CURVE ( 'NONE', #64419, #42748, #48108, .T. ) ;
#14900 = CARTESIAN_POINT ( 'NONE',  ( -113.4000000000000057, 1320.102705746890251, 317.4872039844590290 ) ) ;
#14902 = CARTESIAN_POINT ( 'NONE',  ( 35.28300974739020290, 1451.608449428380027, 134.6903707226859979 ) ) ;
#14903 = CARTESIAN_POINT ( 'NONE',  ( 18.91838588339999916, 1497.713060387329961, 197.2233373248979831 ) ) ;
#14904 = LINE ( 'NONE', #91627, #103334 ) ;
#14905 = CARTESIAN_POINT ( 'NONE',  ( -7.713496591364999766, 1516.704809569559984, 214.3604687893070206 ) ) ;
#14906 = CARTESIAN_POINT ( 'NONE',  ( -4.708696172490000720, 1457.421299317690000, 217.4082516364489948 ) ) ;
#14907 = CARTESIAN_POINT ( 'NONE',  ( 11.52816579256459306, 1363.237826914502875, 208.3718459617010978 ) ) ;
#14908 = CARTESIAN_POINT ( 'NONE',  ( -28.90140687091280114, 1413.853327124249972, 268.9772634007230181 ) ) ;
#14909 = ORIENTED_EDGE ( 'NONE', *, *, #7895, .F. ) ;
#14910 = CARTESIAN_POINT ( 'NONE',  ( -22.03465957474532999, 1512.187213306747481, 235.4136513321633117 ) ) ;
#14911 = VERTEX_POINT ( 'NONE', #48035 ) ;
#14912 = EDGE_LOOP ( 'NONE', ( #51320, #25244, #92057, #41977 ) ) ;
#14913 = CARTESIAN_POINT ( 'NONE',  ( 4.625359524845000792, 1517.025470194390209, 211.6020329869469947 ) ) ;
#14914 = CARTESIAN_POINT ( 'NONE',  ( 16.68463225827361995, 1445.052233488289630, 162.0935120918203154 ) ) ;
#14915 = CARTESIAN_POINT ( 'NONE',  ( 33.28034951413924603, 1522.382868172863937, 200.8029765415137433 ) ) ;
#14917 = CARTESIAN_POINT ( 'NONE',  ( -17.62549087743260046, 1419.742512564495883, 206.8807750381302242 ) ) ;
#14916 = CARTESIAN_POINT ( 'NONE',  ( 4.042417777704999438, 1516.904492006980036, 212.5700528489170154 ) ) ;
#14918 = CARTESIAN_POINT ( 'NONE',  ( -16.35848859230000230, 1455.453302215730218, 189.3475188266980069 ) ) ;
#14919 = CARTESIAN_POINT ( 'NONE',  ( -1.835536242490369840, 1450.383119622699951, 182.7750508701979868 ) ) ;
#14920 = ORIENTED_EDGE ( 'NONE', *, *, #34575, .F. ) ;
#14921 = CARTESIAN_POINT ( 'NONE',  ( -26.61235046579999874, 1435.626708122829996, 136.0714870250980084 ) ) ;
#14922 = CARTESIAN_POINT ( 'NONE',  ( -0.7543882209519990889, 1516.727502608469877, 202.5709757879969857 ) ) ;
#14923 = DIRECTION ( 'NONE',  ( -0.000000000000000000, -1.000000000000000000, -0.000000000000000000 ) ) ;
#14924 = CARTESIAN_POINT ( 'NONE',  ( -9.123736379228210680, 1384.508619151900120, 199.9712811155520171 ) ) ;
#14925 = CARTESIAN_POINT ( 'NONE',  ( -27.50230175260729837, 1417.006653921450152, 270.1128687280570375 ) ) ;
#14926 = CARTESIAN_POINT ( 'NONE',  ( -1.800870875340000010, 1483.727879433689850, 201.4520989251889773 ) ) ;
#14927 = CARTESIAN_POINT ( 'NONE',  ( -2.290042571849999931, 1395.993030436130084, 197.9397562440980209 ) ) ;
#14929 = ORIENTED_EDGE ( 'NONE', *, *, #359, .F. ) ;
#14928 = CARTESIAN_POINT ( 'NONE',  ( 29.86461515634908892, 1525.960063244516959, 197.2746849027934957 ) ) ;
#14930 = EDGE_LOOP ( 'NONE', ( #171, #105307, #52537, #19094 ) ) ;
#14931 = CARTESIAN_POINT ( 'NONE',  ( 0.2831897529540000069, 1451.162134428330091, 182.5531190971980209 ) ) ;
#14932 = AXIS2_PLACEMENT_3D ( 'NONE', #97133, #20951, #54607 ) ;
#14933 = CARTESIAN_POINT ( 'NONE',  ( 3.796654292859254376, 1425.671869022633928, 185.2437681722715581 ) ) ;
#14934 = CARTESIAN_POINT ( 'NONE',  ( 10.84031051884389818, 1460.610437092660050, 207.7000986127219733 ) ) ;
#14935 = CARTESIAN_POINT ( 'NONE',  ( -24.59692435790000076, 1435.635346037049885, 137.3894803190979985 ) ) ;
#14936 = CARTESIAN_POINT ( 'NONE',  ( -24.39471558800000039, 1441.818671265830062, 212.1017248396279911 ) ) ;
#14937 = CARTESIAN_POINT ( 'NONE',  ( 4.044321679994999919, 1517.001127920769704, 211.4073335515969916 ) ) ;
#14938 = CARTESIAN_POINT ( 'NONE',  ( -68.77190080519999071, 1379.747925807450201, 280.3125203366930123 ) ) ;
#14939 = CARTESIAN_POINT ( 'NONE',  ( -2.120283308187459692, 1484.250716573789987, 183.0521180702210131 ) ) ;
#14940 = CARTESIAN_POINT ( 'NONE',  ( 5.025113536143859250, 1441.506992453729936, 216.4625214299290121 ) ) ;
#14941 = CARTESIAN_POINT ( 'NONE',  ( -20.71343476517491311, 1522.382868172863937, 238.3377464195766890 ) ) ;
#14942 = CARTESIAN_POINT ( 'NONE',  ( -5.788436372295000076, 1517.116049120239950, 206.8334885244969712 ) ) ;
#14943 = VERTEX_POINT ( 'NONE', #31223 ) ;
#14944 = CARTESIAN_POINT ( 'NONE',  ( -2.852604639739960035, 1451.959738234309953, 184.7483465814129886 ) ) ;
#14945 = CARTESIAN_POINT ( 'NONE',  ( -9.966716235978671179, 1439.480426183019972, 208.4307555467810005 ) ) ;
#14946 = CARTESIAN_POINT ( 'NONE',  ( 34.77865709045956066, 1512.187213306747481, 191.3609956664886624 ) ) ;
#14947 = ORIENTED_EDGE ( 'NONE', *, *, #98035, .F. ) ;
#14948 = CARTESIAN_POINT ( 'NONE',  ( -22.65254426311538083, 1509.725512665801261, 228.2121030422732701 ) ) ;
#14949 = B_SPLINE_CURVE_WITH_KNOTS ( 'NONE', 3,
 ( #33916, #26619, #103886, #36143, #50728, #51845, #85982, #42888, #1432, #26050, #18210, #60244, #95489, #27187, #35576, #94362, #86531, #52406, #16537, #59154, #17643, #68111, #9281, #102224, #52953, #103311, #77592, #87088, #898, #93274, #2008, #84860, #35023, #8710, #9825, #93806, #10372 ),
 .UNSPECIFIED., .F., .F.,
 ( 4, 3, 3, 3, 3, 3, 3, 3, 3, 3, 3, 3, 4 ),
 ( -12.95412176402940041, -12.81270172653739969, -12.11377028864190031, -11.37640253426160086, -10.60196073214190093, -9.777136418881470448, -8.810301696189478449, -7.829449850869419691, -7.084615941809260242, -6.173206107712330137, -5.351908026777899785, -4.634020098607701144, -3.959746331690000787 ),
 .UNSPECIFIED. ) ;
#14950 = B_SPLINE_SURFACE_WITH_KNOTS ( 'NONE', 5, 5, ( 
 ( #38157, #72338, #29752, #47124, #82370, #4566 ),
 ( #47671, #26303, #33054, #68351, #42569, #101898 ),
 ( #8398, #50439, #7855, #34165, #75087, #51524 ),
 ( #93505, #109237, #25191, #15675, #43131, #42024 ),
 ( #85659, #8959, #67788, #34714, #75638, #76721 ),
 ( #24628, #49879, #60494, #59394, #40907, #16777 ),
 ( #110320, #7313, #33, #50981, #94614, #49328 ),
 ( #77289, #68905, #102457, #85110, #67243, #25744 ),
 ( #100800, #92962, #16235, #76171, #587, #103006 ) ),
 .UNSPECIFIED., .F., .F., .F.,
 ( 6, 3, 6 ),
 ( 6, 6 ),
 ( 13.33598741418959932, 23.39129113199999921, 32.68035051645690459 ),
 ( -0.0006151925569443899948, 2.000000000000000000 ),
 .UNSPECIFIED. ) ;
#14951 = CARTESIAN_POINT ( 'NONE',  ( 13.57909981250000087, 1416.568813547830132, 196.3459685238979944 ) ) ;
#14952 = CARTESIAN_POINT ( 'NONE',  ( -4.001284449659999964, 1413.820567198780054, 207.0461413201589949 ) ) ;
#14953 = CARTESIAN_POINT ( 'NONE',  ( 15.93623140273500027, 1516.904916668740043, 224.2983129015669874 ) ) ;
#14954 = CARTESIAN_POINT ( 'NONE',  ( -26.79413167943010166, 1436.761919080860025, 136.7821860765010058 ) ) ;
#14955 = CARTESIAN_POINT ( 'NONE',  ( 5.393840585100000418, 1486.194748859389847, 199.7804271763089901 ) ) ;
#14956 = DIRECTION ( 'NONE',  ( 0.8775825618903754233, 0.000000000000000000, 0.4794255386041978984 ) ) ;
#14957 = CARTESIAN_POINT ( 'NONE',  ( 23.34067364815647494, 1449.548550064944266, 217.2395114868710095 ) ) ;
#14958 = CARTESIAN_POINT ( 'NONE',  ( -11.91321771470000002, 1435.943783413959864, 147.6429393588979906 ) ) ;
#14959 = CARTESIAN_POINT ( 'NONE',  ( -7.012921583605000286, 1508.551704408389924, 214.6352815282469919 ) ) ;
#14960 = CARTESIAN_POINT ( 'NONE',  ( 0.01126491619350150110, 1516.939530130779985, 216.0663127125970107 ) ) ;
#14961 = ORIENTED_EDGE ( 'NONE', *, *, #20045, .F. ) ;
#14962 = CARTESIAN_POINT ( 'NONE',  ( 7.709487153813650018, 1516.551696783219995, 206.3620776923469862 ) ) ;
#14963 = B_SPLINE_CURVE_WITH_KNOTS ( 'NONE', 5,
 ( #16259, #7877, #61088, #34189, #86798, #76746, #103029, #43155, #1163, #59418, #52661, #609 ),
 .UNSPECIFIED., .F., .F.,
 ( 6, 3, 3, 6 ),
 ( 0.000000000000000000, 0.3833332903980340434, 0.7666665807883968897, 1.000000000000000000 ),
 .UNSPECIFIED. ) ;
#14964 = B_SPLINE_SURFACE_WITH_KNOTS ( 'NONE', 3, 3, ( 
 ( #18278, #43512, #60312, #59220 ),
 ( #35094, #87159, #25018, #27251 ),
 ( #51343, #52471, #44062, #94431 ),
 ( #85477, #8776, #9892, #35645 ) ),
 .UNSPECIFIED., .F., .F., .F.,
 ( 4, 4 ),
 ( 4, 4 ),
 ( 0.000000000000000000, 13.62591263460000057 ),
 ( 7.105427357600000794E-15, 6.790838053299999899 ),
 .UNSPECIFIED. ) ;
#14965 = CARTESIAN_POINT ( 'NONE',  ( 2.409586283469999923, 1426.663880916129983, 144.1938086916980239 ) ) ;
#14966 = CARTESIAN_POINT ( 'NONE',  ( -16.34938676670969926, 1508.551704408389924, 213.4150739050749905 ) ) ;
#14967 = CARTESIAN_POINT ( 'NONE',  ( -14.87836745164769958, 1508.449846342590035, 215.6161849205319925 ) ) ;
#14968 = CARTESIAN_POINT ( 'NONE',  ( -2.562742973329999785, 1475.717683561390004, 219.5239615403990001 ) ) ;
#14969 = CARTESIAN_POINT ( 'NONE',  ( -21.08979015450000105, 1504.838394598090190, 213.3139657128890008 ) ) ;
#14970 = CARTESIAN_POINT ( 'NONE',  ( -31.50799703744299762, 1524.382868172863937, 201.8203724569136739 ) ) ;
#14971 = CARTESIAN_POINT ( 'NONE',  ( 1.814287398422984365, 1416.723938728748408, 232.7280257503442158 ) ) ;
#14972 = CARTESIAN_POINT ( 'NONE',  ( 17.08600013005979790, 1422.205976245335933, 226.7881206011809354 ) ) ;
#14973 = CARTESIAN_POINT ( 'NONE',  ( -106.7897227899999990, 1379.694571751269905, 299.8550812676590454 ) ) ;
#14974 = CARTESIAN_POINT ( 'NONE',  ( -3.829619994797929916, 1515.551704292389786, 210.9648097401420159 ) ) ;
#14975 = CARTESIAN_POINT ( 'NONE',  ( 33.00780592730710339, 1440.913060383419861, 246.6091112861189742 ) ) ;
#14977 = CARTESIAN_POINT ( 'NONE',  ( 4.327741874859650117, 1515.129976808880201, 208.3983552552599861 ) ) ;
#14976 = CARTESIAN_POINT ( 'NONE',  ( -10.21402431085859952, 1471.431448933499951, 210.3618840756950021 ) ) ;
#14978 = PLANE ( 'NONE',  #60007 ) ;
#14979 = VERTEX_POINT ( 'NONE', #65405 ) ;
#14980 = CARTESIAN_POINT ( 'NONE',  ( -4.045182518055000287, 1517.057265928030120, 207.4180663268770104 ) ) ;
#14981 = VERTEX_POINT ( 'NONE', #63220 ) ;
#14982 = CARTESIAN_POINT ( 'NONE',  ( 10.55618159092670005, 1481.139606696229976, 209.6439938450050136 ) ) ;
#14983 = CARTESIAN_POINT ( 'NONE',  ( 16.19087789078229989, 1409.478458302130093, 193.2334102746530107 ) ) ;
#14984 = CARTESIAN_POINT ( 'NONE',  ( -28.63451944679999883, 1509.912999839430086, 211.5264680655480163 ) ) ;
#14985 = CARTESIAN_POINT ( 'NONE',  ( 11.67995417459249907, 1501.899375693250022, 211.4228182329390222 ) ) ;
#14986 = CARTESIAN_POINT ( 'NONE',  ( -18.19590854888122422, 1522.862737210649584, 238.2026672068776634 ) ) ;
#14987 = CARTESIAN_POINT ( 'NONE',  ( 9.467588392827540389, 1422.608842469059937, 212.7560699654940208 ) ) ;
#14988 = CARTESIAN_POINT ( 'NONE',  ( -1.850909961131140147, 1508.551704408389924, 220.0758087861170225 ) ) ;
#14989 = CARTESIAN_POINT ( 'NONE',  ( -41.04806346289370111, 1383.826527834990202, 243.6424592814190078 ) ) ;
#14990 = CARTESIAN_POINT ( 'NONE',  ( -15.52081487708860053, 1478.411708281340225, 223.8101585285860153 ) ) ;
#14991 = DIRECTION ( 'NONE',  ( 0.5219928277095973179, -0.8520822723975763902, -0.03846152474253997089 ) ) ;
#14992 = CARTESIAN_POINT ( 'NONE',  ( -11.65438896117129808, 1501.787989776810036, 208.8020054899499769 ) ) ;
#14993 = CARTESIAN_POINT ( 'NONE',  ( 11.74550440620560110, 1492.414915879079899, 211.0460056930020016 ) ) ;
#14995 = ORIENTED_EDGE ( 'NONE', *, *, #101680, .T. ) ;
#14994 = CARTESIAN_POINT ( 'NONE',  ( -0.9377529295590010250, 1456.788838343890120, 218.9786281422690024 ) ) ;
#14996 = CARTESIAN_POINT ( 'NONE',  ( -1.273048297609999935, 1451.180663451930059, 183.3072205426980190 ) ) ;
#14997 = CARTESIAN_POINT ( 'NONE',  ( -55.58991683120000005, 1380.431293333419944, 241.3934034463590024 ) ) ;
#14998 = CARTESIAN_POINT ( 'NONE',  ( 8.174873262491109571, 1436.356241397249960, 206.4284659498850090 ) ) ;
#14999 = ORIENTED_EDGE ( 'NONE', *, *, #15065, .T. ) ;
#15000 = ORIENTED_EDGE ( 'NONE', *, *, #73545, .F. ) ;
#15001 = CARTESIAN_POINT ( 'NONE',  ( 1.188403172992487766, 1416.818673809778147, 190.1193007443792453 ) ) ;
#15002 = CARTESIAN_POINT ( 'NONE',  ( -2.000000019065000245, 1520.551704408390151, 222.4523892994670007 ) ) ;
#15004 = CARTESIAN_POINT ( 'NONE',  ( 6.232532001850000114, 1407.162969929529936, 220.5304192662980256 ) ) ;
#15003 = CARTESIAN_POINT ( 'NONE',  ( -11.87328627558470018, 1482.014094172719979, 208.6022272904490080 ) ) ;
#15005 = AXIS2_PLACEMENT_3D ( 'NONE', #84258, #83164, #32753 ) ;
#15006 = CARTESIAN_POINT ( 'NONE',  ( -8.107801870790000365, 1463.844143246390104, 201.5100198155989801 ) ) ;
#15007 = CARTESIAN_POINT ( 'NONE',  ( -103.6765714240000023, 1379.937512265609939, 302.8207899414589974 ) ) ;
#15008 = DIRECTION ( 'NONE',  ( 5.980589973904019347E-17, -1.000000000000000000, 1.736889445713099699E-16 ) ) ;
#15009 = DIRECTION ( 'NONE',  ( -1.000000000000000000, 0.000000000000000000, 0.000000000000000000 ) ) ;
#15010 = CARTESIAN_POINT ( 'NONE',  ( 9.726491193908251375E-12, 1408.913060387299993, 194.1220083575990145 ) ) ;
#15011 = CARTESIAN_POINT ( 'NONE',  ( 18.03150314649800023, 1424.669146068439886, 225.2932228502139935 ) ) ;
#15012 = FACE_OUTER_BOUND ( 'NONE', #105412, .T. ) ;
#15013 = CARTESIAN_POINT ( 'NONE',  ( 2.180749907540250110, 1433.190219894490156, 200.8861995550460051 ) ) ;
#15014 = CARTESIAN_POINT ( 'NONE',  ( -2.500000055771189889, 1440.197962455250035, 166.9350719905560254 ) ) ;
#15015 = AXIS2_PLACEMENT_3D ( 'NONE', #13755, #90479, #47396 ) ;
#15016 = FACE_OUTER_BOUND ( 'NONE', #66767, .T. ) ;
#15017 = VERTEX_POINT ( 'NONE', #22794 ) ;
#15018 =( BOUNDED_SURFACE ( )  B_SPLINE_SURFACE ( 3, 2, ( 
 ( #14182, #82511, #99281 ),
 ( #40494, #107706, #30991 ),
 ( #107148, #14738, #74672 ),
 ( #108805, #56204, #66286 ) ),
 .UNSPECIFIED., .F., .F., .F. ) 
 B_SPLINE_SURFACE_WITH_KNOTS ( ( 4, 4 ),
 ( 3, 3 ),
 ( 0.008319848492105399312, 0.01047023456112128326 ),
 ( 0.6817855796338941898, 1.000000000000000000 ),
 .UNSPECIFIED. ) 
 GEOMETRIC_REPRESENTATION_ITEM ( )  RATIONAL_B_SPLINE_SURFACE ( (
 ( 0.8701819858983746991, 0.9047955706460268921, 1.000000000000000000),
 ( 0.8701112842800549085, 0.9047437203132890904, 1.000000000000000000),
 ( 0.8701364165503382431, 0.9047621515261470293, 1.000000000000000000),
 ( 0.8702549240939394526, 0.9048490612138414546, 1.000000000000000000) ) ) 
 REPRESENTATION_ITEM ( '' )  SURFACE ( )  );
#15019 = CARTESIAN_POINT ( 'NONE',  ( -0.8090580814599999115, 1427.166763959530044, 147.9649995502979891 ) ) ;
#15020 = CARTESIAN_POINT ( 'NONE',  ( 18.61241607401199616, 1457.060397574680110, 228.8782662039849924 ) ) ;
#15021 = CARTESIAN_POINT ( 'NONE',  ( -12.94539156839999983, 1434.910719961430004, 150.0942592413979924 ) ) ;
#15022 = CARTESIAN_POINT ( 'NONE',  ( 12.40160258794860049, 1420.584110727309962, 200.5244627772079866 ) ) ;
#15023 = CARTESIAN_POINT ( 'NONE',  ( 6.824596843277944913, 1424.786834349993342, 213.4892281956427098 ) ) ;
#15024 = CARTESIAN_POINT ( 'NONE',  ( -14.65275159090000123, 1420.238444720549978, 213.8660283808390261 ) ) ;
#15025 = CARTESIAN_POINT ( 'NONE',  ( -109.8667940760000050, 1385.713658988820043, 311.3767387042589689 ) ) ;
#15026 = CARTESIAN_POINT ( 'NONE',  ( -0.5542659975529999894, 1483.385152224330113, 181.9510117909979954 ) ) ;
#15027 = CARTESIAN_POINT ( 'NONE',  ( -9.761853366963894274, 1361.142561771200917, 208.3718459617010978 ) ) ;
#15028 = CARTESIAN_POINT ( 'NONE',  ( -45.85454091276539401, 1440.913070276949838, 268.7563665289580399 ) ) ;
#15029 = CARTESIAN_POINT ( 'NONE',  ( 13.62520701428609904, 1508.937755598840113, 233.7142831108280063 ) ) ;
#15030 = DIRECTION ( 'NONE',  ( 5.980589973904019347E-17, -1.000000000000000000, 1.736889445713099699E-16 ) ) ;
#15031 = EDGE_CURVE ( 'NONE', #13046, #93687, #48185, .T. ) ;
#15032 = CARTESIAN_POINT ( 'NONE',  ( -1.133653179125000188, 1516.978425811520083, 208.3843950493249793 ) ) ;
#15033 = CARTESIAN_POINT ( 'NONE',  ( -23.28626003949876377, 1507.873436380149997, 195.0116325568262710 ) ) ;
#15034 = DIRECTION ( 'NONE',  ( -0.9510565162951566398, 0.000000000000000000, -0.3090169943749382919 ) ) ;
#15035 = CARTESIAN_POINT ( 'NONE',  ( 11.15268687969999917, 1425.700851675330114, 101.7515397216980091 ) ) ;
#15036 = CARTESIAN_POINT ( 'NONE',  ( 7.408918475326540687, 1425.143336949030072, 212.4352455266580080 ) ) ;
#15037 = VERTEX_POINT ( 'NONE', #102681 ) ;
#15038 = CARTESIAN_POINT ( 'NONE',  ( 17.30165530980000099, 1424.236263306130013, 225.6855429073979735 ) ) ;
#15039 = FACE_OUTER_BOUND ( 'NONE', #60897, .T. ) ;
#15041 = CARTESIAN_POINT ( 'NONE',  ( -14.89373269229610131, 1512.150422497879845, 221.5012839471549739 ) ) ;
#15040 = CARTESIAN_POINT ( 'NONE',  ( 0.5071369118009999566, 1469.874380101830184, 182.5356705811979907 ) ) ;
#15042 = B_SPLINE_CURVE_WITH_KNOTS ( 'NONE', 3,
 ( #78111, #23962, #69749, #87067 ),
 .UNSPECIFIED., .F., .F.,
 ( 4, 4 ),
 ( 0.000000000000000000, 0.0002220129587134776663 ),
 .UNSPECIFIED. ) ;
#15043 = B_SPLINE_CURVE_WITH_KNOTS ( 'NONE', 5,
 ( #55946, #72744, #4440, #107426, #22850, #106871 ),
 .UNSPECIFIED., .F., .F.,
 ( 6, 6 ),
 ( 0.000000000000000000, 1.000000000000000000 ),
 .UNSPECIFIED. ) ;
#15044 = CARTESIAN_POINT ( 'NONE',  ( -1.534154776998204239, 1488.212794018828845, 219.8849755564752115 ) ) ;
#15045 = CARTESIAN_POINT ( 'NONE',  ( -8.163757246560001235, 1420.362486717730008, 225.2112877850979942 ) ) ;
#15046 = CARTESIAN_POINT ( 'NONE',  ( -29.48232863870257603, 1509.960453018734142, 206.3162625148400764 ) ) ;
#15047 = CARTESIAN_POINT ( 'NONE',  ( -6.943015404634899745, 1452.670604946809817, 151.6351347268530105 ) ) ;
#15048 = CARTESIAN_POINT ( 'NONE',  ( 13.33054332923500063, 1517.051704408389924, 211.1218459511669892 ) ) ;
#15049 = VERTEX_POINT ( 'NONE', #1364 ) ;
#15050 = CARTESIAN_POINT ( 'NONE',  ( -5.362275202304809696, 1424.093369006069906, 150.3042897941160163 ) ) ;
#15051 = CARTESIAN_POINT ( 'NONE',  ( 17.84054674791004302, 1523.580204110583509, 237.8810931398604680 ) ) ;
#15052 = CARTESIAN_POINT ( 'NONE',  ( 15.63428379070249896, 1422.707660709189895, 229.1465903752480244 ) ) ;
#15053 = CARTESIAN_POINT ( 'NONE',  ( 9.744365386780000193, 1462.929680191989974, 209.8474545865749974 ) ) ;
#15054 = ORIENTED_EDGE ( 'NONE', *, *, #85786, .T. ) ;
#15055 = VERTEX_POINT ( 'NONE', #109051 ) ;
#15056 = CARTESIAN_POINT ( 'NONE',  ( -75.49415276370000072, 1384.770980541030212, 276.6885382114589902 ) ) ;
#15057 = CARTESIAN_POINT ( 'NONE',  ( -23.95203783885379778, 1410.422133454150071, 208.8949471922620091 ) ) ;
#15058 = ORIENTED_EDGE ( 'NONE', *, *, #88299, .T. ) ;
#15059 = CARTESIAN_POINT ( 'NONE',  ( 4.426499554645539902, 1508.728286212990042, 204.9620041230130312 ) ) ;
#15060 = CARTESIAN_POINT ( 'NONE',  ( -106.9474174639999973, 1379.784802923450115, 308.7531441963589600 ) ) ;
#15061 = CARTESIAN_POINT ( 'NONE',  ( -1.395300564360000051, 1498.352961133030021, 236.7605676195980209 ) ) ;
#15062 = CARTESIAN_POINT ( 'NONE',  ( 4.987082593000310204, 1508.551704408389924, 212.3948883545009778 ) ) ;
#15063 = EDGE_CURVE ( 'NONE', #52165, #69390, #24246, .T. ) ;
#15064 = CARTESIAN_POINT ( 'NONE',  ( 41.51622458814379257, 1455.223082529530075, 269.0892613835300153 ) ) ;
#15065 = EDGE_CURVE ( 'NONE', #22209, #3563, #39373, .T. ) ;
#15066 = CARTESIAN_POINT ( 'NONE',  ( -4.487249399419609652, 1509.038630936360050, 205.6342588683990016 ) ) ;
#15067 = CARTESIAN_POINT ( 'NONE',  ( -0.2357814831160000291, 1418.572813431130044, 184.6863074503980044 ) ) ;
#15068 = CARTESIAN_POINT ( 'NONE',  ( -5.784638357945000031, 1516.939574742129935, 204.5080835752170003 ) ) ;
#15069 = EDGE_LOOP ( 'NONE', ( #72372, #80247, #49966, #52840, #36696 ) ) ;
#15071 = EDGE_CURVE ( 'NONE', #59860, #60953, #31434, .T. ) ;
#15070 = CARTESIAN_POINT ( 'NONE',  ( 6.683036765369180010, 1483.419246594629840, 218.8825796861059985 ) ) ;
#15072 = CARTESIAN_POINT ( 'NONE',  ( 15.30573751214310008, 1512.900351074040145, 195.3517817113319950 ) ) ;
#15073 = CARTESIAN_POINT ( 'NONE',  ( 6.154344797466830386, 1434.513861532099781, 226.5897845999569995 ) ) ;
#15074 = ORIENTED_EDGE ( 'NONE', *, *, #108277, .F. ) ;
#15075 = CARTESIAN_POINT ( 'NONE',  ( -11.22704429269360027, 1481.056718734030028, 211.0225828912199972 ) ) ;
#15076 = EDGE_CURVE ( 'NONE', #66885, #78702, #96457, .T. ) ;
#15077 = CARTESIAN_POINT ( 'NONE',  ( 5.681834224037626058, 1434.688408934563313, 202.7553282809922166 ) ) ;
#15078 = ADVANCED_FACE ( 'NONE', ( #95421 ), #6024, .F. ) ;
#15079 = CARTESIAN_POINT ( 'NONE',  ( -13.83393990147829911, 1512.951873711579992, 193.8224831105249848 ) ) ;
#15080 = CARTESIAN_POINT ( 'NONE',  ( 3.725874866239260008, 1452.782949969990113, 152.2831223846509943 ) ) ;
#15081 = CARTESIAN_POINT ( 'NONE',  ( 8.247379814629999473, 1421.181889050119935, 196.1087402428989890 ) ) ;
#15082 = CARTESIAN_POINT ( 'NONE',  ( 22.57032379820000045, 1409.701233462030132, 209.8663284536589799 ) ) ;
#15083 = CARTESIAN_POINT ( 'NONE',  ( -11.90229160620850024, 1491.340589200470049, 206.1196870462119932 ) ) ;
#15084 = FACE_OUTER_BOUND ( 'NONE', #74086, .T. ) ;
#15085 = VECTOR ( 'NONE', #945, 1000.000000000000114 ) ;
#15086 = CARTESIAN_POINT ( 'NONE',  ( 1.988761914397050079, 1408.982509483710146, 186.9246551635189917 ) ) ;
#15088 = CARTESIAN_POINT ( 'NONE',  ( -18.41706550949158938, 1424.167467087569776, 225.1579557749482774 ) ) ;
#15087 = CARTESIAN_POINT ( 'NONE',  ( -13.01189509148379919, 1434.786097740819969, 149.1479131938150147 ) ) ;
#15089 = CARTESIAN_POINT ( 'NONE',  ( 3.307325631547500144, 1441.238735741373148, 170.5343657987176300 ) ) ;
#15090 = CARTESIAN_POINT ( 'NONE',  ( -11.81825512610000040, 1379.647206402889879, 214.1905352636190116 ) ) ;
#15091 = CARTESIAN_POINT ( 'NONE',  ( 11.16223122930000144, 1428.970455832429934, 101.8807690336980016 ) ) ;
#15092 = ORIENTED_EDGE ( 'NONE', *, *, #5003, .T. ) ;
#15093 = CARTESIAN_POINT ( 'NONE',  ( 16.42420380379999756, 1507.212883763329955, 193.5443561786979956 ) ) ;
#15094 = CIRCLE ( 'NONE', #65172, 1.000000000000000888 ) ;
#15095 = DIRECTION ( 'NONE',  ( 0.0008672850459984940506, -0.9990096763985240047, -0.04448498936456254937 ) ) ;
#15096 = CARTESIAN_POINT ( 'NONE',  ( 19.34100150109859939, 1467.084855511749993, 225.9993250057500234 ) ) ;
#15097 = B_SPLINE_SURFACE_WITH_KNOTS ( 'NONE', 5, 5, ( 
 ( #16087, #63393, #29204, #32369, #97508, #92266 ),
 ( #107000, #15536, #98597, #29741, #80711, #75494 ),
 ( #89648, #4557, #41324, #12934, #63929, #98043 ),
 ( #64482, #109628, #50294, #32899, #101197, #24493 ),
 ( #41866, #76018, #20777, #54978, #89103, #86076 ),
 ( #10475, #59789, #44646, #8799, #110723, #9916 ) ),
 .UNSPECIFIED., .F., .F., .F.,
 ( 6, 6 ),
 ( 6, 6 ),
 ( 2.324858856890000158, 4.991117563610000474 ),
 ( 0.000000000000000000, 0.5000000000000000000 ),
 .UNSPECIFIED. ) ;
#15098 = CARTESIAN_POINT ( 'NONE',  ( -8.162781193059998941, 1386.079686460999937, 199.6931303246190055 ) ) ;
#15099 = CARTESIAN_POINT ( 'NONE',  ( -15.91912926760000246, 1415.990061217859875, 209.7496671253580018 ) ) ;
#15100 = EDGE_CURVE ( 'NONE', #62781, #39872, #96895, .T. ) ;
#15101 = CARTESIAN_POINT ( 'NONE',  ( 11.66448423075249963, 1421.851407392159899, 203.4123043171020129 ) ) ;
#15102 = CYLINDRICAL_SURFACE ( 'NONE', #78145, 1.000000000000000888 ) ;
#15103 = CARTESIAN_POINT ( 'NONE',  ( -43.50000000000000000, 1445.861068816730040, 271.1218459616979999 ) ) ;
#15104 = CARTESIAN_POINT ( 'NONE',  ( -13.58268883510000080, 1416.851343894929869, 221.9096085503980191 ) ) ;
#15105 = CARTESIAN_POINT ( 'NONE',  ( 11.94146967429999862, 1433.521468468569992, 150.1184368365979935 ) ) ;
#15106 = CARTESIAN_POINT ( 'NONE',  ( 10.04572263220000039, 1464.202968133530021, 255.3819207742980097 ) ) ;
#15107 = B_SPLINE_SURFACE_WITH_KNOTS ( 'NONE', 5, 5, ( 
 ( #16824, #86268, #43181, #94669, #42619, #35880 ),
 ( #76771, #87, #103625, #102502, #77333, #68951 ),
 ( #52136, #26351, #43724, #61112, #77877, #104176 ),
 ( #1185, #18491, #95227, #69503, #52686, #10114 ),
 ( #70064, #106917, #47042, #88482, #98520, #21786 ),
 ( #44848, #30206, #70606, #96885, #20695, #2303 ) ),
 .UNSPECIFIED., .F., .F., .F.,
 ( 6, 6 ),
 ( 6, 6 ),
 ( 3.171299407250000257, 3.535033821230000317 ),
 ( 0.000000000000000000, 0.2999999999999999889 ),
 .UNSPECIFIED. ) ;
#15108 = PLANE ( 'NONE',  #38367 ) ;
#15109 = EDGE_CURVE ( 'NONE', #44371, #79447, #40755, .T. ) ;
#15110 = CARTESIAN_POINT ( 'NONE',  ( -29.00779973304138437, 1526.382868172864164, 200.9494832830839073 ) ) ;
#15111 = CARTESIAN_POINT ( 'NONE',  ( -108.1042440287333193, 1389.151938345616145, 298.3733779900309173 ) ) ;
#15112 = ADVANCED_FACE ( 'NONE', ( #64045 ), #51716, .F. ) ;
#15113 = CARTESIAN_POINT ( 'NONE',  ( -14.63705847081953593, 1422.169902665600603, 229.4588690542234417 ) ) ;
#15114 = CARTESIAN_POINT ( 'NONE',  ( -17.71284803180000011, 1486.217784300129779, 188.1321109405980110 ) ) ;
#15115 = FACE_OUTER_BOUND ( 'NONE', #16765, .T. ) ;
#15116 = CARTESIAN_POINT ( 'NONE',  ( 18.58720762869999987, 1416.311719779230089, 209.7162280979700029 ) ) ;
#15117 = CARTESIAN_POINT ( 'NONE',  ( 0.4151546846821903003, 1501.977400791986611, 242.9330574173806951 ) ) ;
#15118 = CARTESIAN_POINT ( 'NONE',  ( -3.156438986539999991, 1479.750519982490005, 229.2993030149989977 ) ) ;
#15119 = DIRECTION ( 'NONE',  ( -0.1010290445074252530, 0.000000000000000000, 0.9948834766775036531 ) ) ;
#15120 = CARTESIAN_POINT ( 'NONE',  ( 1.117126662530000036, 1515.456827602489966, 204.9211030669989952 ) ) ;
#15121 = CARTESIAN_POINT ( 'NONE',  ( -2.127574403379840273, 1524.244163922423468, 173.7332312662362597 ) ) ;
#15122 = CYLINDRICAL_SURFACE ( 'NONE', #81365, 2.000000000000003553 ) ;
#15123 = CARTESIAN_POINT ( 'NONE',  ( -6.250808155840000602, 1416.216596894629902, 226.2958911897979988 ) ) ;
#15124 = AXIS2_PLACEMENT_3D ( 'NONE', #100885, #41566, #39905 ) ;
#15125 = CARTESIAN_POINT ( 'NONE',  ( 0.1699996708203529716, 1480.329832774919851, 182.0802225456559995 ) ) ;
#15127 = EDGE_LOOP ( 'NONE', ( #74852, #214, #55923, #40549 ) ) ;
#15126 = CARTESIAN_POINT ( 'NONE',  ( 0.02192821825021479959, 1407.539782046369965, 222.1835171484239879 ) ) ;
#15128 = FACE_OUTER_BOUND ( 'NONE', #24934, .T. ) ;
#15129 = CARTESIAN_POINT ( 'NONE',  ( 13.80567663220000085, 1434.979608490319833, 147.6248746541980097 ) ) ;
#15130 = CARTESIAN_POINT ( 'NONE',  ( -39.77086281159900238, 1438.526156311480008, 134.0999999980039945 ) ) ;
#15131 = CARTESIAN_POINT ( 'NONE',  ( -11.15738487964140013, 1390.939238811560017, 203.8452351040699853 ) ) ;
#15132 = ORIENTED_EDGE ( 'NONE', *, *, #40559, .T. ) ;
#15133 = CARTESIAN_POINT ( 'NONE',  ( -16.51370421206452122, 1525.137906803775877, 181.0453479566121189 ) ) ;
#15134 = CARTESIAN_POINT ( 'NONE',  ( 11.26937487549999872, 1478.652699893289991, 205.8601903476990174 ) ) ;
#15135 = CARTESIAN_POINT ( 'NONE',  ( -104.5385623544569285, 1380.577965172966742, 307.6528342442834969 ) ) ;
#15136 = CARTESIAN_POINT ( 'NONE',  ( 1.925297170580940076, 1517.151704408390060, 230.6853930747409720 ) ) ;
#15137 = CARTESIAN_POINT ( 'NONE',  ( -1.743457682199999859, 1468.969847108790191, 189.2470145170989895 ) ) ;
#15138 = B_SPLINE_CURVE_WITH_KNOTS ( 'NONE', 5,
 ( #69801, #105593, #37279, #20444, #63072, #79285, #97172, #78725, #103919, #54653, #61399, #46254 ),
 .UNSPECIFIED., .F., .F.,
 ( 6, 3, 3, 6 ),
 ( 0.000000000000000000, 0.2842603455368540866, 0.7006323907210947333, 1.000000000000000000 ),
 .UNSPECIFIED. ) ;
#15139 = CARTESIAN_POINT ( 'NONE',  ( 31.52040524782195874, 1416.197860221249357, 269.3256485028547331 ) ) ;
#15140 = CARTESIAN_POINT ( 'NONE',  ( -15.07756690969999980, 1414.162796065500061, 212.4126893105689931 ) ) ;
#15141 = CARTESIAN_POINT ( 'NONE',  ( -12.95282315900000114, 1379.746587813670203, 210.9367672650590180 ) ) ;
#15142 = CARTESIAN_POINT ( 'NONE',  ( 4.138543392800865917, 1515.492058412107781, 210.9648081769078374 ) ) ;
#15143 = CARTESIAN_POINT ( 'NONE',  ( -53.74734980331459866, 1385.033272470989914, 231.5355373840500022 ) ) ;
#15144 = CARTESIAN_POINT ( 'NONE',  ( -11.08783833967420129, 1391.913060387289988, 212.3049891749950291 ) ) ;
#15145 = CARTESIAN_POINT ( 'NONE',  ( 10.65988927221830096, 1426.698688119150120, 208.4127383140620111 ) ) ;
#15146 = ORIENTED_EDGE ( 'NONE', *, *, #8408, .F. ) ;
#15147 = CARTESIAN_POINT ( 'NONE',  ( -29.80701629120000007, 1451.872188912029969, 134.8363203424979986 ) ) ;
#15148 = CARTESIAN_POINT ( 'NONE',  ( -16.26157404866599876, 1409.582217294140037, 225.7367796582349797 ) ) ;
#15150 = EDGE_LOOP ( 'NONE', ( #71746, #72518, #14076, #45593 ) ) ;
#15149 = CARTESIAN_POINT ( 'NONE',  ( 3.401541474470889614, 1468.225229937070026, 218.5224292273400124 ) ) ;
#15151 = CARTESIAN_POINT ( 'NONE',  ( -109.3074459189999885, 1384.922471985850279, 311.2646699492589732 ) ) ;
#15152 = CARTESIAN_POINT ( 'NONE',  ( 11.37306528310140052, 1471.269141200139984, 210.1781679118379884 ) ) ;
#15153 = CARTESIAN_POINT ( 'NONE',  ( -19.30538610943497346, 1410.948714638366710, 222.3723562416497259 ) ) ;
#15154 = CARTESIAN_POINT ( 'NONE',  ( -109.1345257920000051, 1384.812366243020051, 311.2635679502590165 ) ) ;
#15155 = CARTESIAN_POINT ( 'NONE',  ( -0.3961054703501400431, 1418.676517288780133, 184.7143626773449796 ) ) ;
#15156 = CARTESIAN_POINT ( 'NONE',  ( 21.76795527650000039, 1409.673214137629884, 214.0268462324280279 ) ) ;
#15157 = CARTESIAN_POINT ( 'NONE',  ( -2.919750075684910406, 1419.523100886769953, 186.2043985311460119 ) ) ;
#15158 = CARTESIAN_POINT ( 'NONE',  ( -17.58914910740000082, 1423.039930255530180, 226.3751546217980035 ) ) ;
#15159 = CARTESIAN_POINT ( 'NONE',  ( -4.963932502907999478, 1511.398736650825185, 200.6109342551562804 ) ) ;
#15160 = CARTESIAN_POINT ( 'NONE',  ( 10.10679549600000193, 1451.115179940190046, 206.1347980303889926 ) ) ;
#15161 = CARTESIAN_POINT ( 'NONE',  ( -101.4843241977000758, 1368.558218059089995, 292.3061701549589770 ) ) ;
#15162 = CARTESIAN_POINT ( 'NONE',  ( 3.871411596960000256, 1475.513060387329915, 229.5852438705979921 ) ) ;
#15163 = VECTOR ( 'NONE', #21243, 1000.000000000000114 ) ;
#15164 = CARTESIAN_POINT ( 'NONE',  ( -29.00779973304124582, 1526.382868172864164, 217.2942086403127178 ) ) ;
#15165 = EDGE_CURVE ( 'NONE', #44275, #35203, #4672, .T. ) ;
#15166 = CARTESIAN_POINT ( 'NONE',  ( -2.298369507954999946, 1516.779243033999819, 205.8702346062869992 ) ) ;
#15168 = ADVANCED_FACE ( 'NONE', ( #71921 ), #42518, .T. ) ;
#15167 = CARTESIAN_POINT ( 'NONE',  ( -6.358070405449739226, 1484.270638837799879, 183.8946224230450355 ) ) ;
#15169 = EDGE_LOOP ( 'NONE', ( #3415, #96183, #5041, #53963 ) ) ;
#15170 = CIRCLE ( 'NONE', #2683, 1.999999999999998668 ) ;
#15171 = DIRECTION ( 'NONE',  ( -7.436362843295819681E-17, 1.000000000000000000, -1.457576885956999882E-16 ) ) ;
#15172 = CARTESIAN_POINT ( 'NONE',  ( -4.221801104570530150, 1441.602310353549910, 168.2831674553420100 ) ) ;
#15174 = ORIENTED_EDGE ( 'NONE', *, *, #99268, .T. ) ;
#15173 = CARTESIAN_POINT ( 'NONE',  ( -68.75556014300001095, 1379.747888069970031, 280.3281857314590297 ) ) ;
#15175 = CARTESIAN_POINT ( 'NONE',  ( -9.268081120116850258, 1380.504154720858878, 217.3372005545678292 ) ) ;
#15176 = ORIENTED_EDGE ( 'NONE', *, *, #60710, .F. ) ;
#15177 = CARTESIAN_POINT ( 'NONE',  ( 1.673908112249919977, 1485.355439722810161, 220.8689413507970016 ) ) ;
#15178 = CARTESIAN_POINT ( 'NONE',  ( 11.27569180979999963, 1501.931370426789954, 206.9838411614990150 ) ) ;
#15180 = CARTESIAN_POINT ( 'NONE',  ( 15.89852580928170056, 1409.468224213880148, 192.8813377015480057 ) ) ;
#15179 = CARTESIAN_POINT ( 'NONE',  ( -11.73940163521978519, 1426.278578077852444, 144.3763880045744656 ) ) ;
#15181 = CARTESIAN_POINT ( 'NONE',  ( 0.7579262867720020225, 1516.927039499179955, 210.8260166843570005 ) ) ;
#15182 = CARTESIAN_POINT ( 'NONE',  ( 40.26322191559909669, 1439.095366118250240, 135.2291069399360026 ) ) ;
#15183 = EDGE_CURVE ( 'NONE', #34885, #64221, #105409, .T. ) ;
#15184 = B_SPLINE_SURFACE_WITH_KNOTS ( 'NONE', 5, 1, ( 
 ( #65739, #6914 ),
 ( #22030, #14206 ),
 ( #83615, #13636 ),
 ( #99304, #32673 ),
 ( #99858, #5265 ),
 ( #66851, #57356 ),
 ( #14760, #73597 ),
 ( #31012, #41070 ),
 ( #48947, #6372 ) ),
 .UNSPECIFIED., .F., .F., .F.,
 ( 6, 3, 6 ),
 ( 2, 2 ),
 ( 0.7097524320730000946, 4.064565667710000163, 10.06421383387139912 ),
 ( -13.48619596139999999, -1.265881781730000100 ),
 .UNSPECIFIED. ) ;
#15185 = CARTESIAN_POINT ( 'NONE',  ( 33.92724808885991905, 1435.682287743722554, 135.5036907871966037 ) ) ;
#15186 = DIRECTION ( 'NONE',  ( 0.9455185755993178454, 0.000000000000000000, -0.3255681544571539243 ) ) ;
#15187 = CARTESIAN_POINT ( 'NONE',  ( 12.66766512233539821, 1500.805898962940091, 210.1506732187789908 ) ) ;
#15188 = APPLICATION_PROTOCOL_DEFINITION ( 'draft international standard', 'automotive_design', 1998, #83513 ) ;
#15189 = CARTESIAN_POINT ( 'NONE',  ( 13.58268853708210067, 1416.851343896850040, 196.3340833727469885 ) ) ;
#15190 = EDGE_LOOP ( 'NONE', ( #75577, #6786, #101326 ) ) ;
#15191 = CARTESIAN_POINT ( 'NONE',  ( -18.41508126919999810, 1458.154041264329862, 227.7774065783979722 ) ) ;
#15192 = EDGE_LOOP ( 'NONE', ( #57609, #17924, #5711, #84064 ) ) ;
#15193 = ORIENTED_EDGE ( 'NONE', *, *, #24163, .T. ) ;
#15194 = CARTESIAN_POINT ( 'NONE',  ( 11.60004869885203682, 1426.043485606469631, 137.7524099801277657 ) ) ;
#15195 = CARTESIAN_POINT ( 'NONE',  ( -1.757532416683340148, 1451.933574871519795, 184.1885909450070073 ) ) ;
#15196 = CARTESIAN_POINT ( 'NONE',  ( -14.08142637225379978, 1379.709117121690042, 211.5303641152310092 ) ) ;
#15197 = CARTESIAN_POINT ( 'NONE',  ( -3.296302496939999660, 1485.523047861029909, 182.9415910454979723 ) ) ;
#15198 = DIRECTION ( 'NONE',  ( 0.000000000000000000, 0.000000000000000000, -1.000000000000000000 ) ) ;
#15199 = CARTESIAN_POINT ( 'NONE',  ( 18.22873622136830107, 1457.634151734390116, 229.9687917111629929 ) ) ;
#15200 = CARTESIAN_POINT ( 'NONE',  ( -41.65674268029999894, 1443.992461967939789, 135.6790812281979868 ) ) ;
#15201 = CARTESIAN_POINT ( 'NONE',  ( 40.71747595459699909, 1438.773003512770174, 135.6938347574059947 ) ) ;
#15202 = CARTESIAN_POINT ( 'NONE',  ( 2.613239871555069538, 1421.346360341460013, 183.3165747233060188 ) ) ;
#15204 = EDGE_CURVE ( 'NONE', #68277, #31171, #94683, .T. ) ;
#15203 = AXIS2_PLACEMENT_3D ( 'NONE', #15481, #110115, #71342 ) ;
#15205 = CARTESIAN_POINT ( 'NONE',  ( 25.67574771179999971, 1437.591200499259912, 137.2873827178979695 ) ) ;
#15206 = CARTESIAN_POINT ( 'NONE',  ( -10.57866586919999996, 1391.913060534260012, 214.0410642522289777 ) ) ;
#15207 = CARTESIAN_POINT ( 'NONE',  ( -70.27615847020030060, 1384.739003949510106, 266.4825429262279499 ) ) ;
#15208 = ORIENTED_EDGE ( 'NONE', *, *, #20041, .T. ) ;
#15209 = CARTESIAN_POINT ( 'NONE',  ( -2.872700555325000238, 1516.559109716219837, 201.4121646638069763 ) ) ;
#15210 = CARTESIAN_POINT ( 'NONE',  ( -6.564578723344999922, 1517.199196846569976, 207.4137433428170141 ) ) ;
#15211 = ORIENTED_EDGE ( 'NONE', *, *, #17540, .T. ) ;
#15213 = EDGE_CURVE ( 'NONE', #75901, #29531, #53550, .T. ) ;
#15212 = CARTESIAN_POINT ( 'NONE',  ( 42.06232107555830169, 1440.913060387330006, 269.6487541170399709 ) ) ;
#15214 = CARTESIAN_POINT ( 'NONE',  ( -0.0002035089733392563926, 1452.237673957955622, 153.8261543310597688 ) ) ;
#15215 = ORIENTED_EDGE ( 'NONE', *, *, #78076, .T. ) ;
#15216 = CARTESIAN_POINT ( 'NONE',  ( -14.20165756390000134, 1416.819756528530206, 221.7375112866980089 ) ) ;
#15217 = CARTESIAN_POINT ( 'NONE',  ( -11.00562449240939955, 1432.347154516129876, 151.7431427700479958 ) ) ;
#15218 = CARTESIAN_POINT ( 'NONE',  ( 20.91563475928075988, 1525.795403383247276, 233.2509749551239224 ) ) ;
#15219 = CARTESIAN_POINT ( 'NONE',  ( 24.08426297012860218, 1411.115209414830133, 209.6325633951909708 ) ) ;
#15220 = CARTESIAN_POINT ( 'NONE',  ( 21.95096434148669928, 1409.939836231839990, 206.2919199104040331 ) ) ;
#15221 = FACE_OUTER_BOUND ( 'NONE', #27620, .T. ) ;
#15222 = CARTESIAN_POINT ( 'NONE',  ( -16.76078030769999927, 1420.494757909599912, 203.1294657649889928 ) ) ;
#15223 = CARTESIAN_POINT ( 'NONE',  ( -5.768664141499007414, 1510.557600715827675, 201.5810540284795422 ) ) ;
#15224 = CARTESIAN_POINT ( 'NONE',  ( -21.38516915558008336, 1522.382868172863937, 180.3939891059723664 ) ) ;
#15225 = EDGE_CURVE ( 'NONE', #34381, #84728, #104817, .T. ) ;
#15227 = CARTESIAN_POINT ( 'NONE',  ( 7.778981777592010260, 1467.988552340439810, 201.0890001560949827 ) ) ;
#15226 = CARTESIAN_POINT ( 'NONE',  ( 15.19576882900000037, 1461.839785508229852, 229.8993157890980115 ) ) ;
#15228 = CARTESIAN_POINT ( 'NONE',  ( -4.641209657417020296, 1422.124063284806425, 184.6640048031023298 ) ) ;
#15229 = B_SPLINE_SURFACE_WITH_KNOTS ( 'NONE', 5, 5, ( 
 ( #79021, #96350, #2322, #80650, #36432, #63869 ),
 ( #104747, #62224, #19627, #72266, #87968, #106400 ),
 ( #21251, #97984, #100200, #73910, #107490, #98538 ),
 ( #13974, #108038, #48162, #81727, #40845, #31333 ),
 ( #75018, #83390, #6132, #49264, #58212, #5035 ),
 ( #82299, #57677, #64964, #23484, #6688, #56558 ),
 ( #39180, #109168, #91791, #40289, #5597, #15067 ),
 ( #21806, #22913, #92338, #24015, #72810, #32454 ),
 ( #106941, #13413, #15610, #82841, #90686, #66630 ) ),
 .UNSPECIFIED., .F., .F., .F.,
 ( 6, 3, 6 ),
 ( 6, 6 ),
 ( 0.8628043814250000443, 1.314432051750000108, 1.883620747549999974 ),
 ( 0.000000000000000000, 2.000000000000000000 ),
 .UNSPECIFIED. ) ;
#15230 = CARTESIAN_POINT ( 'NONE',  ( 5.004442038985000174, 1516.690345681169902, 216.8349637732169697 ) ) ;
#15231 = ORIENTED_EDGE ( 'NONE', *, *, #106125, .F. ) ;
#15232 = B_SPLINE_CURVE_WITH_KNOTS ( 'NONE', 3,
 ( #103412, #26717, #24771, #92545, #50017, #39402, #84149, #99285, #15813, #66832, #66290, #30995, #48372, #100939, #32103, #82515, #75767, #7450, #48931, #67386, #90903, #40499, #74125, #41613, #24235, #32655, #100407, #22561, #58967, #83593, #14742, #6892, #74676, #108255, #49472, #108810, #109915 ),
 .UNSPECIFIED., .F., .F.,
 ( 4, 3, 3, 3, 3, 3, 3, 3, 3, 3, 3, 3, 4 ),
 ( -8.626417477929999578, -8.230297350330690875, -7.288362325489999627, -6.788184810323580010, -5.950307173050000564, -5.270875643514309594, -4.379860848525059858, -3.500078386716319656, -3.080773698474470024, -2.517080355727370211, -1.669614525887570089, -0.8307986329775687295, 0.000000000000000000 ),
 .UNSPECIFIED. ) ;
#15233 = ADVANCED_FACE ( 'NONE', ( #20754 ), #10736, .T. ) ;
#15234 = CARTESIAN_POINT ( 'NONE',  ( -4.863842518140000237, 1453.445020719190097, 199.8398594391789800 ) ) ;
#15235 = CARTESIAN_POINT ( 'NONE',  ( -0.0001187281342228439996, 1508.967929526819944, 179.3767679645770272 ) ) ;
#15236 = CARTESIAN_POINT ( 'NONE',  ( 2.067604332986444859, 1516.528072456315613, 216.8307144992771498 ) ) ;
#15237 = CARTESIAN_POINT ( 'NONE',  ( -7.710285875814999912, 1516.582197289609894, 212.3822242253069987 ) ) ;
#15238 = CARTESIAN_POINT ( 'NONE',  ( 2.801044513573409667, 1515.551704203360032, 212.9510687777460021 ) ) ;
#15239 = CARTESIAN_POINT ( 'NONE',  ( -11.60004869885203682, 1426.044482836622592, 137.7673702721163238 ) ) ;
#15241 = ORIENTED_EDGE ( 'NONE', *, *, #19994, .T. ) ;
#15240 = CARTESIAN_POINT ( 'NONE',  ( 4.487358445059079770, 1509.034524749680031, 212.9235806931369837 ) ) ;
#15242 = CARTESIAN_POINT ( 'NONE',  ( -1.191524307911313363, 1526.382868172864164, 179.0083900503168479 ) ) ;
#15243 = CARTESIAN_POINT ( 'NONE',  ( 21.19943833389999810, 1451.689670470829924, 217.4746504698680098 ) ) ;
#15244 = CARTESIAN_POINT ( 'NONE',  ( -11.85178780869999926, 1431.281462211560211, 150.3047777764980140 ) ) ;
#15245 = CARTESIAN_POINT ( 'NONE',  ( 19.02706862106219887, 1456.916313564460097, 225.6436289706080345 ) ) ;
#15246 = CARTESIAN_POINT ( 'NONE',  ( -67.65174119259999941, 1379.761245408810282, 278.4852794438589854 ) ) ;
#15247 = CARTESIAN_POINT ( 'NONE',  ( 11.84030397337090079, 1430.235998727099741, 151.0624529839080026 ) ) ;
#15248 = CARTESIAN_POINT ( 'NONE',  ( -4.453607449379680006, 1428.081049923210003, 200.8976384725820026 ) ) ;
#15249 = ADVANCED_FACE ( 'NONE', ( #44909 ), #106115, .T. ) ;
#15250 = CARTESIAN_POINT ( 'NONE',  ( -15.22591321480220117, 1441.486322144610085, 221.1269846435299939 ) ) ;
#15252 = CARTESIAN_POINT ( 'NONE',  ( -10.56985333086790035, 1482.340625775369972, 205.9074429510509958 ) ) ;
#15251 = CARTESIAN_POINT ( 'NONE',  ( -19.32501916510000228, 1470.091136407030035, 227.3171351542980005 ) ) ;
#15253 = CARTESIAN_POINT ( 'NONE',  ( -4.794426340529999386, 1463.608615258990085, 228.2108236244990280 ) ) ;
#15254 = ORIENTED_EDGE ( 'NONE', *, *, #3680, .T. ) ;
#15255 = CARTESIAN_POINT ( 'NONE',  ( -3.267603553834999897, 1516.858171774179937, 205.8687047948669999 ) ) ;
#15256 = CARTESIAN_POINT ( 'NONE',  ( 3.773607150769999752, 1405.866055185730147, 267.5310499900980403 ) ) ;
#15257 = EDGE_CURVE ( 'NONE', #102542, #76097, #6719, .T. ) ;
#15258 = CARTESIAN_POINT ( 'NONE',  ( -0.1764364529069999965, 1409.076774544030059, 185.6010313908980152 ) ) ;
#15259 = CARTESIAN_POINT ( 'NONE',  ( 19.07614737060000110, 1410.874611392730003, 195.4187278566980126 ) ) ;
#15260 = CARTESIAN_POINT ( 'NONE',  ( 21.16486544290946981, 1428.404148231732506, 219.5078859491472656 ) ) ;
#15261 = CARTESIAN_POINT ( 'NONE',  ( 0.000000000000000000, 1502.413060387330006, 209.1218459616979999 ) ) ;
#15262 = CARTESIAN_POINT ( 'NONE',  ( 26.35471571933159751, 1507.985750330240080, 216.6976075425179999 ) ) ;
#15263 = B_SPLINE_CURVE_WITH_KNOTS ( 'NONE', 5,
 ( #96313, #38598, #72778, #29650, #97410, #63837, #71143, #88469, #87932, #96874, #104706, #20680, #72238, #97949, #89004 ),
 .UNSPECIFIED., .F., .F.,
 ( 6, 3, 3, 3, 6 ),
 ( -48.56910781718399761, -39.03858743909999873, -32.22913687700000196, -31.51384161189999844, -29.50806686130000145 ),
 .UNSPECIFIED. ) ;
#15264 = CARTESIAN_POINT ( 'NONE',  ( -18.84860651825824363, 1456.786630790735671, 228.5413354237351768 ) ) ;
#15265 = CARTESIAN_POINT ( 'NONE',  ( -15.31513450300000123, 1417.997849063050126, 203.5151318327289971 ) ) ;
#15266 = CARTESIAN_POINT ( 'NONE',  ( -12.79312897949999872, 1445.016120524290045, 186.3935252196979775 ) ) ;
#15267 = CARTESIAN_POINT ( 'NONE',  ( 2.499999999889860103, 1448.906648695949798, 155.3362529649780015 ) ) ;
#15268 = B_SPLINE_SURFACE_WITH_KNOTS ( 'NONE', 5, 5, ( 
 ( #63671, #45767, #96704, #89395, #13211, #73149 ),
 ( #105096, #54718, #30021, #72603, #107292, #37898 ),
 ( #97783, #54169, #72080, #90485, #106732, #39543 ),
 ( #64214, #106194, #28386, #98336, #55817, #47401 ),
 ( #13760, #3215, #38970, #64775, #98885, #47944 ),
 ( #62587, #19975, #37343, #71540, #105662, #28946 ) ),
 .UNSPECIFIED., .F., .F., .F.,
 ( 6, 6 ),
 ( 6, 6 ),
 ( 0.000000000000000000, 9.314731292829998566 ),
 ( 0.000000000000000000, 2.000000000000000000 ),
 .UNSPECIFIED. ) ;
#15269 = CARTESIAN_POINT ( 'NONE',  ( -8.619624426343268198, 1437.672210802470090, 208.2420778849330247 ) ) ;
#15270 = CARTESIAN_POINT ( 'NONE',  ( -12.31752010984839885, 1377.944433743309901, 209.1218459601290078 ) ) ;
#15271 = CARTESIAN_POINT ( 'NONE',  ( -5.498087649510000396, 1437.444228038389838, 208.8531670801410201 ) ) ;
#15272 = CARTESIAN_POINT ( 'NONE',  ( -27.15947446952620226, 1507.993364321890112, 211.1689828938959863 ) ) ;
#15273 = LINE ( 'NONE', #49466, #33008 ) ;
#15274 = CARTESIAN_POINT ( 'NONE',  ( -1.757373113509999918, 1475.295645524329984, 269.4976378123980112 ) ) ;
#15275 = CARTESIAN_POINT ( 'NONE',  ( -4.229825888870420769, 1446.290640099090069, 165.0045831357620045 ) ) ;
#15276 = CARTESIAN_POINT ( 'NONE',  ( -14.79239591447758606, 1514.564605521402655, 192.8689679281645510 ) ) ;
#15277 = CARTESIAN_POINT ( 'NONE',  ( 17.84759684480400210, 1410.895160446669934, 223.1913782762499920 ) ) ;
#15278 = CARTESIAN_POINT ( 'NONE',  ( -56.94594514817760000, 1384.708275839130010, 275.5160223163470050 ) ) ;
#15279 = CARTESIAN_POINT ( 'NONE',  ( 13.58256589259447011, 1416.843574543525847, 196.3343232356145052 ) ) ;
#15280 = CARTESIAN_POINT ( 'NONE',  ( -21.59687142900000012, 1507.523380033690046, 209.4572543540780032 ) ) ;
#15281 = CARTESIAN_POINT ( 'NONE',  ( -25.17436548464209878, 1470.080601114610090, 212.0235103180719705 ) ) ;
#15282 = CARTESIAN_POINT ( 'NONE',  ( 32.18358323225305639, 1524.059547553519224, 216.7473625276872156 ) ) ;
#15283 = CARTESIAN_POINT ( 'NONE',  ( -2.884599899255949917E-09, 1473.199988346640112, 268.3915997654160037 ) ) ;
#15284 = CIRCLE ( 'NONE', #67123, 1.000000000000000888 ) ;
#15285 = CARTESIAN_POINT ( 'NONE',  ( -4.237827489471030242E-15, 1374.913060387289988, 209.1218459572589836 ) ) ;
#15286 = CARTESIAN_POINT ( 'NONE',  ( -9.906269641306360896, 1380.355646941639407, 201.6945993121081528 ) ) ;
#15287 = CARTESIAN_POINT ( 'NONE',  ( -15.06844210530799977, 1422.391250798362080, 229.4663103607340133 ) ) ;
#15288 = B_SPLINE_CURVE_WITH_KNOTS ( 'NONE', 5,
 ( #103927, #42363, #36182, #42931, #19353, #78170 ),
 .UNSPECIFIED., .F., .F.,
 ( 6, 6 ),
 ( 0.000000000000000000, 1.000000000000000000 ),
 .UNSPECIFIED. ) ;
#15289 = CARTESIAN_POINT ( 'NONE',  ( -25.33241404900000049, 1413.251821757829930, 269.9969244510980388 ) ) ;
#15290 = ORIENTED_EDGE ( 'NONE', *, *, #102111, .T. ) ;
#15291 = CARTESIAN_POINT ( 'NONE',  ( -4.556184579163090831, 1410.448051561546436, 232.0254849714374075 ) ) ;
#15292 = CARTESIAN_POINT ( 'NONE',  ( -8.268898679290179743, 1439.252518696380093, 228.5874792367960140 ) ) ;
#15293 = CARTESIAN_POINT ( 'NONE',  ( 11.45577226660000036, 1502.286415424589904, 208.3140783707030153 ) ) ;
#15294 = VECTOR ( 'NONE', #107907, 1000.000000000000000 ) ;
#15295 = CARTESIAN_POINT ( 'NONE',  ( -3.071486888918079750, 1470.850328545360071, 187.3986291775349855 ) ) ;
#15297 = CARTESIAN_POINT ( 'NONE',  ( -12.35647260227639954, 1378.853423139930101, 211.4877825593519844 ) ) ;
#15296 = CARTESIAN_POINT ( 'NONE',  ( 10.68407736780000050, 1425.006924162730229, 135.9205847407980059 ) ) ;
#15298 = CARTESIAN_POINT ( 'NONE',  ( -3.968827103576990201, 1519.551704408389924, 229.5396913781519856 ) ) ;
#15299 = CARTESIAN_POINT ( 'NONE',  ( -127.5184075663999863, 1336.950374720429863, 296.5089247511289727 ) ) ;
#15300 = CARTESIAN_POINT ( 'NONE',  ( -5.582992786199999280, 1454.196299517489933, 201.5533260997290199 ) ) ;
#15301 = ADVANCED_FACE ( 'NONE', ( #83423 ), #10393, .F. ) ;
#15302 = CARTESIAN_POINT ( 'NONE',  ( 6.941100277744999936, 1516.858069504249897, 202.1782432786469883 ) ) ;
#15303 = CARTESIAN_POINT ( 'NONE',  ( -20.02799630220000182, 1485.574563381989947, 204.1280247810589970 ) ) ;
#15304 = CARTESIAN_POINT ( 'NONE',  ( -11.79165762230000070, 1429.416862815430022, 146.4064176768980019 ) ) ;
#15305 = CARTESIAN_POINT ( 'NONE',  ( 15.08013800783500002, 1512.195694528090144, 196.5109711095670093 ) ) ;
#15306 = CARTESIAN_POINT ( 'NONE',  ( -17.47119686262369953, 1420.005972689359851, 204.6300621421460164 ) ) ;
#15307 = CARTESIAN_POINT ( 'NONE',  ( -39.30087362371570237, 1378.765606774250045, 229.0543489963469881 ) ) ;
#15308 = CARTESIAN_POINT ( 'NONE',  ( 3.577843379407391833, 1368.113851476867239, 207.6218459616988241 ) ) ;
#15310 = ORIENTED_EDGE ( 'NONE', *, *, #67325, .F. ) ;
#15309 = CARTESIAN_POINT ( 'NONE',  ( -29.90839080569999808, 1379.722162691039784, 217.8816187629589933 ) ) ;
#15311 = EDGE_LOOP ( 'NONE', ( #68517, #59588, #40223, #79630 ) ) ;
#15312 = CARTESIAN_POINT ( 'NONE',  ( 11.86993521259999973, 1433.837969291950003, 150.7297411583980136 ) ) ;
#15313 = CARTESIAN_POINT ( 'NONE',  ( -10.98139245720000012, 1398.238761414130067, 216.8837352115380099 ) ) ;
#15314 = CARTESIAN_POINT ( 'NONE',  ( -19.88787437039999872, 1410.102804823130100, 220.6443014318979863 ) ) ;
#15315 = ORIENTED_EDGE ( 'NONE', *, *, #53430, .F. ) ;
#15316 = CARTESIAN_POINT ( 'NONE',  ( -13.39960398253788476, 1444.421273251342882, 169.3685383806885056 ) ) ;
#15317 = CARTESIAN_POINT ( 'NONE',  ( 22.10835456647167874, 1509.702725196560550, 228.7991371166729948 ) ) ;
#15318 = CARTESIAN_POINT ( 'NONE',  ( -7.777794748224999388, 1511.980236064749988, 212.0143493490369906 ) ) ;
#15320 = CARTESIAN_POINT ( 'NONE',  ( -13.70766983986010068, 1507.659368579370266, 184.2581583972360022 ) ) ;
#15319 = CARTESIAN_POINT ( 'NONE',  ( -0.02721485961659890138, 1443.931464463489874, 200.0408948413389965 ) ) ;
#15321 = EDGE_CURVE ( 'NONE', #79507, #20921, #84277, .T. ) ;
#15322 = CARTESIAN_POINT ( 'NONE',  ( 13.43062830470000080, 1488.164680700029976, 186.5792399276980120 ) ) ;
#15323 = CARTESIAN_POINT ( 'NONE',  ( -3.127352221352849959, 1464.808845836910223, 198.5552573355170125 ) ) ;
#15324 = CARTESIAN_POINT ( 'NONE',  ( 3.018932976099999443, 1424.181238483419975, 191.3872096091990045 ) ) ;
#15325 = CARTESIAN_POINT ( 'NONE',  ( 7.892725014381700710, 1396.188680504749982, 201.3838934717110192 ) ) ;
#15326 = CARTESIAN_POINT ( 'NONE',  ( 1.556886619979999997, 1415.063410501330054, 191.4794882261979865 ) ) ;
#15327 = CARTESIAN_POINT ( 'NONE',  ( 11.86596898630000041, 1432.335940955089882, 150.3973237302979840 ) ) ;
#15328 = CARTESIAN_POINT ( 'NONE',  ( 8.170454128426975160, 1509.198649520710887, 180.9503965351503609 ) ) ;
#15329 = ORIENTED_EDGE ( 'NONE', *, *, #72050, .T. ) ;
#15330 = CARTESIAN_POINT ( 'NONE',  ( 13.02655316196230117, 1434.814175597650092, 149.4409609364860216 ) ) ;
#15331 = EDGE_CURVE ( 'NONE', #26097, #93900, #108779, .T. ) ;
#15332 = ORIENTED_EDGE ( 'NONE', *, *, #21681, .F. ) ;
#15333 = ORIENTED_EDGE ( 'NONE', *, *, #105493, .T. ) ;
#15334 = CARTESIAN_POINT ( 'NONE',  ( 12.97436564310944185, 1444.891968944272094, 169.4253161487108059 ) ) ;
#15335 = CARTESIAN_POINT ( 'NONE',  ( -11.13796040809999965, 1464.110348585029897, 231.7316128992979998 ) ) ;
#15336 = CARTESIAN_POINT ( 'NONE',  ( -13.02322702429999879, 1416.825784017130218, 196.6108461441979784 ) ) ;
#15337 = CARTESIAN_POINT ( 'NONE',  ( -1.708102627415000185, 1517.199196846569976, 215.6864246554469844 ) ) ;
#15338 = CARTESIAN_POINT ( 'NONE',  ( -19.78960455480000036, 1467.443448038389988, 207.1734148488289975 ) ) ;
#15339 = ORIENTED_EDGE ( 'NONE', *, *, #95552, .F. ) ;
#15340 = CARTESIAN_POINT ( 'NONE',  ( -11.61154441450000085, 1502.159899280790114, 208.3750068673870146 ) ) ;
#15341 = DIRECTION ( 'NONE',  ( -0.1403878024439498828, 0.9900965937346509760, 0.000000000000000000 ) ) ;
#15342 = CARTESIAN_POINT ( 'NONE',  ( -3.771520293490000064, 1379.460406650380037, 206.9293833799489732 ) ) ;
#15343 = VECTOR ( 'NONE', #26649, 1000.000000000000000 ) ;
#15344 = ORIENTED_EDGE ( 'NONE', *, *, #22611, .F. ) ;
#15345 = CARTESIAN_POINT ( 'NONE',  ( 4.609673241434999902, 1516.754149861460064, 205.8564388142570181 ) ) ;
#15346 = ORIENTED_EDGE ( 'NONE', *, *, #84679, .F. ) ;
#15347 = CARTESIAN_POINT ( 'NONE',  ( 7.337297311985000015, 1517.135701590510052, 209.8615382079770200 ) ) ;
#15348 = CARTESIAN_POINT ( 'NONE',  ( -8.419044950492288848, 1452.206747589980068, 205.1691836855419808 ) ) ;
#15349 = EDGE_CURVE ( 'NONE', #27006, #101083, #36803, .T. ) ;
#15350 = CARTESIAN_POINT ( 'NONE',  ( -32.05312539274948591, 1421.205571191992931, 269.4939401719450416 ) ) ;
#15351 = CARTESIAN_POINT ( 'NONE',  ( -2.933338486410000279, 1410.393077976529867, 232.5461313705979762 ) ) ;
#15352 = EDGE_CURVE ( 'NONE', #42031, #24662, #76139, .T. ) ;
#15354 = VERTEX_POINT ( 'NONE', #93469 ) ;
#15353 = CARTESIAN_POINT ( 'NONE',  ( -2.499989269620250809, 1419.524750234567819, 137.1000002976804808 ) ) ;
#15355 = CARTESIAN_POINT ( 'NONE',  ( 19.81803190540000159, 1427.321367310129972, 222.3183646145980106 ) ) ;
#15356 = CARTESIAN_POINT ( 'NONE',  ( -29.09122759982509976, 1440.913060387109908, 235.2915179107689880 ) ) ;
#15357 = CARTESIAN_POINT ( 'NONE',  ( -47.37590574939999755, 1384.752751010099928, 256.2773158601589785 ) ) ;
#15358 = DIRECTION ( 'NONE',  ( 0.1402804634180439824, -0.9901118076173108795, 0.000000000000000000 ) ) ;
#15359 = EDGE_CURVE ( 'NONE', #22669, #101515, #74095, .T. ) ;
#15360 = CARTESIAN_POINT ( 'NONE',  ( 14.82025145092669938, 1411.931168022049860, 269.8832746614870075 ) ) ;
#15361 = CARTESIAN_POINT ( 'NONE',  ( 7.721907888235000073, 1517.026025493960105, 214.1263215447669950 ) ) ;
#15362 = EDGE_CURVE ( 'NONE', #77632, #69558, #59288, .T. ) ;
#15363 = CARTESIAN_POINT ( 'NONE',  ( 22.71803131159999722, 1409.706390560829959, 209.2188350014689888 ) ) ;
#15364 = VECTOR ( 'NONE', #11269, 1000.000000000000114 ) ;
#15365 = CARTESIAN_POINT ( 'NONE',  ( -20.54538654549999777, 1508.881852289130165, 189.3180432071980022 ) ) ;
#15366 = CARTESIAN_POINT ( 'NONE',  ( 16.84849232383349715, 1428.239404528469777, 202.3949443903100018 ) ) ;
#15368 = CARTESIAN_POINT ( 'NONE',  ( -4.363122647530000009, 1421.971318475729959, 179.5815723472979926 ) ) ;
#15367 = CIRCLE ( 'NONE', #76132, 34.90184096762461508 ) ;
#15369 = CARTESIAN_POINT ( 'NONE',  ( 3.463767257884999839, 1517.014196759610059, 210.8246003415769962 ) ) ;
#15370 = CARTESIAN_POINT ( 'NONE',  ( 0.5000000000152821089, 1448.894380913990062, 155.6080914337030094 ) ) ;
#15371 = CARTESIAN_POINT ( 'NONE',  ( -19.73295319860160291, 1503.904974312793911, 218.6992394349398126 ) ) ;
#15372 =( BOUNDED_CURVE ( )  B_SPLINE_CURVE ( 3, ( #91240, #56551, #40281, #22350 ),
 .UNSPECIFIED., .F., .F. ) 
 B_SPLINE_CURVE_WITH_KNOTS ( ( 4, 4 ),
 ( 2.001957627660153403E-12, 0.4510268114855987553 ),
 .UNSPECIFIED. ) 
 CURVE ( )  GEOMETRIC_REPRESENTATION_ITEM ( )  RATIONAL_B_SPLINE_CURVE ( ( 1.000000000000000000, 0.9831196230105689882, 0.9831196230105689882, 1.000000000000000000 ) ) 
 REPRESENTATION_ITEM ( '' )  );
#15373 = CARTESIAN_POINT ( 'NONE',  ( 10.97941491499529931, 1432.933185717909964, 151.7695633904889974 ) ) ;
#15375 = ORIENTED_EDGE ( 'NONE', *, *, #78509, .T. ) ;
#15374 = CARTESIAN_POINT ( 'NONE',  ( -73.11479823269999656, 1385.127942832860072, 272.3424178700590232 ) ) ;
#15376 = CARTESIAN_POINT ( 'NONE',  ( -43.63441986346529688, 1385.160729704950199, 248.8361117960110107 ) ) ;
#15377 = CARTESIAN_POINT ( 'NONE',  ( 14.25481165789999949, 1474.931993151730012, 267.1910255919980273 ) ) ;
#15378 = CARTESIAN_POINT ( 'NONE',  ( -4.125989513582625889, 1370.398720948539221, 208.4821978858626892 ) ) ;
#15379 = CARTESIAN_POINT ( 'NONE',  ( -11.91935979259999989, 1420.493316629130049, 231.2800121289980098 ) ) ;
#15380 = EDGE_CURVE ( 'NONE', #85956, #15491, #64789, .T. ) ;
#15381 = CARTESIAN_POINT ( 'NONE',  ( 5.170487778963170022, 1484.055109584380034, 219.7711518219039988 ) ) ;
#15382 = CARTESIAN_POINT ( 'NONE',  ( -23.83765245669999899, 1446.530553800920188, 215.3656821590780055 ) ) ;
#15383 = CARTESIAN_POINT ( 'NONE',  ( -0.8350686643532192477, 1526.382868172863937, 177.3106345060153046 ) ) ;
#15385 = CARTESIAN_POINT ( 'NONE',  ( -7.544898869409998987, 1384.902875507950057, 219.0876726552290279 ) ) ;
#15384 = CYLINDRICAL_SURFACE ( 'NONE', #50079, 1.000000000000000888 ) ;
#15386 = DIRECTION ( 'NONE',  ( 0.1400401707400374951, -0.004890310883056902050, 0.9901337462376323950 ) ) ;
#15387 = ORIENTED_EDGE ( 'NONE', *, *, #46251, .T. ) ;
#15388 = CARTESIAN_POINT ( 'NONE',  ( -6.556022232634999725, 1516.833525648419936, 202.1813725979570222 ) ) ;
#15389 = EDGE_CURVE ( 'NONE', #5604, #35589, #55453, .T. ) ;
#15390 = CARTESIAN_POINT ( 'NONE',  ( -16.52887565636499900, 1513.466724478469814, 223.3227970231669985 ) ) ;
#15391 = CARTESIAN_POINT ( 'NONE',  ( 0.2316317416650000294, 1477.419807478629991, 229.8396568727980025 ) ) ;
#15392 = CARTESIAN_POINT ( 'NONE',  ( -20.49599333844833993, 1525.960063244516959, 233.8638087104925489 ) ) ;
#15393 = CARTESIAN_POINT ( 'NONE',  ( 7.229617388605507955, 1438.908991744435752, 154.0610282733643999 ) ) ;
#15394 = EDGE_CURVE ( 'NONE', #50989, #18256, #80691, .T. ) ;
#15395 = CARTESIAN_POINT ( 'NONE',  ( -6.483871891156958611, 1462.197955881078769, 201.8355004268651953 ) ) ;
#15396 = CARTESIAN_POINT ( 'NONE',  ( 26.14468651563449342, 1450.763943277846010, 136.6602026170544377 ) ) ;
#15397 = DIRECTION ( 'NONE',  ( 0.000000000000000000, 0.000000000000000000, -1.000000000000000000 ) ) ;
#15398 = CARTESIAN_POINT ( 'NONE',  ( 27.58302911533250068, 1435.460667994110054, 135.2629876134730011 ) ) ;
#15399 = CARTESIAN_POINT ( 'NONE',  ( 38.58175818029209836, 1448.251245179850002, 136.4584366939950257 ) ) ;
#15400 = CARTESIAN_POINT ( 'NONE',  ( -21.74327147740000044, 1430.168649232730104, 219.0066490272480166 ) ) ;
#15401 = CARTESIAN_POINT ( 'NONE',  ( 10.79528402730720060, 1489.628194868570063, 207.4012257063180016 ) ) ;
#15402 = CARTESIAN_POINT ( 'NONE',  ( -106.2112533720000016, 1391.321897446320236, 300.8491284572590416 ) ) ;
#15403 = CARTESIAN_POINT ( 'NONE',  ( 8.768085951239999787, 1509.161958816129982, 181.7959786723980073 ) ) ;
#15404 = CARTESIAN_POINT ( 'NONE',  ( 5.349014141963440494, 1506.777988995989972, 219.5093220728170138 ) ) ;
#15405 = CARTESIAN_POINT ( 'NONE',  ( -9.579969104820666104, 1470.643550730757852, 269.3463861652618334 ) ) ;
#15406 = ORIENTED_EDGE ( 'NONE', *, *, #59018, .T. ) ;
#15407 = CARTESIAN_POINT ( 'NONE',  ( -4.580855544014999836, 1515.987684277770086, 217.2759425653769938 ) ) ;
#15408 = CARTESIAN_POINT ( 'NONE',  ( 9.336110127025321503, 1506.539416727244770, 189.1210688587442803 ) ) ;
#15409 = CARTESIAN_POINT ( 'NONE',  ( -3.487586739969820382, 1508.731366863229823, 213.6768007669170117 ) ) ;
#15410 = CARTESIAN_POINT ( 'NONE',  ( -5.219497435470000113, 1484.378742230190255, 199.3181751762190004 ) ) ;
#15411 = CARTESIAN_POINT ( 'NONE',  ( -0.02484813282310000329, 1416.432140399929949, 233.7186307104979903 ) ) ;
#15412 = CARTESIAN_POINT ( 'NONE',  ( -28.28208339020000039, 1508.151294418729776, 209.1342425839550287 ) ) ;
#15413 = CARTESIAN_POINT ( 'NONE',  ( -9.783890651532770377, 1438.409856597829958, 210.7792734677780118 ) ) ;
#15414 = CARTESIAN_POINT ( 'NONE',  ( -3.778540308872590181, 1515.551842517600107, 212.4904177570749937 ) ) ;
#15415 = CARTESIAN_POINT ( 'NONE',  ( -3.958671420333373714, 1415.944797298322328, 232.4758296456245716 ) ) ;
#15416 = CARTESIAN_POINT ( 'NONE',  ( -7.776877434901703801, 1451.396943400985947, 153.0106348905935931 ) ) ;
#15417 = CARTESIAN_POINT ( 'NONE',  ( 24.32116265780000219, 1435.530952642309785, 137.6072328918980077 ) ) ;
#15418 = CARTESIAN_POINT ( 'NONE',  ( 3.173602151875000388, 1510.830536680500245, 216.6815192743169973 ) ) ;
#15420 = ORIENTED_EDGE ( 'NONE', *, *, #59024, .F. ) ;
#15419 = CARTESIAN_POINT ( 'NONE',  ( 11.87502392341400004, 1433.007271648830056, 149.9804723818110119 ) ) ;
#15421 = CARTESIAN_POINT ( 'NONE',  ( 1.377258800780170045, 1414.913060387399810, 192.4870635420249982 ) ) ;
#15422 = CARTESIAN_POINT ( 'NONE',  ( -12.02612939183720009, 1377.659857216290220, 211.7505375168460091 ) ) ;
#15423 = VERTEX_POINT ( 'NONE', #45320 ) ;
#15424 = ORIENTED_EDGE ( 'NONE', *, *, #25335, .T. ) ;
#15425 = CARTESIAN_POINT ( 'NONE',  ( 16.36863935783290103, 1414.913057862230062, 208.9007734745979974 ) ) ;
#15426 = FACE_OUTER_BOUND ( 'NONE', #36100, .T. ) ;
#15428 = CARTESIAN_POINT ( 'NONE',  ( -25.01541328220000082, 1442.557000325939953, 216.4497915791480125 ) ) ;
#15427 = CARTESIAN_POINT ( 'NONE',  ( -11.62807272172398498, 1428.982488964479899, 136.1186897298418046 ) ) ;
#15429 = B_SPLINE_CURVE_WITH_KNOTS ( 'NONE', 5,
 ( #5542, #30172, #57625, #56507, #31838, #66024 ),
 .UNSPECIFIED., .F., .F.,
 ( 6, 6 ),
 ( 0.03026097244042860734, 1.000000000000000000 ),
 .UNSPECIFIED. ) ;
#15430 = CARTESIAN_POINT ( 'NONE',  ( -4.716923275420001005, 1446.360134133290103, 217.0074177048290096 ) ) ;
#15431 = CARTESIAN_POINT ( 'NONE',  ( -11.81225577550000061, 1433.099404687269953, 150.5666296323979907 ) ) ;
#15432 = DIRECTION ( 'NONE',  ( 0.000000000000000000, 1.000000000000000000, 0.000000000000000000 ) ) ;
#15433 = CARTESIAN_POINT ( 'NONE',  ( -2.919621720534709919, 1419.522956690290130, 186.2043860719099939 ) ) ;
#15434 = CARTESIAN_POINT ( 'NONE',  ( 6.916306201240000284, 1423.889214271699984, 213.5479170703790146 ) ) ;
#15435 = CARTESIAN_POINT ( 'NONE',  ( -24.38244995200000176, 1440.343059974619791, 211.3205732649580000 ) ) ;
#15436 = FACE_BOUND ( 'NONE', #32076, .T. ) ;
#15437 = DIRECTION ( 'NONE',  ( 0.7063774289747313251, 0.04540766091858282338, 0.7063774289747313251 ) ) ;
#15438 = CARTESIAN_POINT ( 'NONE',  ( 8.379275254590000443, 1362.454991452509830, 207.6218459616989946 ) ) ;
#15439 = CARTESIAN_POINT ( 'NONE',  ( -28.16265580408766667, 1510.008130024179991, 219.4883605467473160 ) ) ;
#15440 = CIRCLE ( 'NONE', #56634, 24.00543915299668640 ) ;
#15442 = ORIENTED_EDGE ( 'NONE', *, *, #67205, .F. ) ;
#15441 = CARTESIAN_POINT ( 'NONE',  ( -2.521777220032119811E-09, 1415.593833303999872, 242.3213147721250209 ) ) ;
#15443 = ORIENTED_EDGE ( 'NONE', *, *, #44217, .F. ) ;
#15444 = CARTESIAN_POINT ( 'NONE',  ( -11.77777284958320081, 1427.343273226020074, 146.9184637112259963 ) ) ;
#15445 = CARTESIAN_POINT ( 'NONE',  ( 24.10516660284129742, 1496.435767336129857, 206.8622324630100309 ) ) ;
#15446 = CARTESIAN_POINT ( 'NONE',  ( -4.235651747309999493, 1473.118544177530111, 270.4270856384979993 ) ) ;
#15447 = CARTESIAN_POINT ( 'NONE',  ( 37.66849513895419932, 1445.052233489950140, 137.0436250799990034 ) ) ;
#15448 = CARTESIAN_POINT ( 'NONE',  ( -124.1837824923999989, 1366.350733876289951, 304.2218459572590064 ) ) ;
#15449 = CARTESIAN_POINT ( 'NONE',  ( 39.65045748264740411, 1446.880369190260126, 136.6574868213660068 ) ) ;
#15450 = CARTESIAN_POINT ( 'NONE',  ( 1.912903644476265042, 1526.104292489129193, 240.8844628569918882 ) ) ;
#15451 = CARTESIAN_POINT ( 'NONE',  ( 19.75084982879439721, 1455.504334177440114, 226.5702129464319796 ) ) ;
#15452 = DIRECTION ( 'NONE',  ( -5.329070518200752183E-15, 0.000000000000000000, -1.000000000000000000 ) ) ;
#15453 = CARTESIAN_POINT ( 'NONE',  ( -33.42844755917204225, 1522.382868172863937, 196.1165140606796058 ) ) ;
#15454 = CARTESIAN_POINT ( 'NONE',  ( 11.81974299095224801, 1364.123681825266203, 208.3718459617010978 ) ) ;
#15455 = CARTESIAN_POINT ( 'NONE',  ( -33.44259286938519438, 1416.839468587309966, 266.5282928195520071 ) ) ;
#15456 = AXIS2_PLACEMENT_3D ( 'NONE', #49929, #15728, #83508 ) ;
#15457 = ORIENTED_EDGE ( 'NONE', *, *, #878, .F. ) ;
#15458 = CARTESIAN_POINT ( 'NONE',  ( 0.000000000000000000, 1523.051704408389696, 233.8211094035767985 ) ) ;
#15459 = EDGE_LOOP ( 'NONE', ( #678, #24417, #41589, #79926, #61967 ) ) ;
#15460 = EDGE_LOOP ( 'NONE', ( #73341, #77496 ) ) ;
#15461 = CARTESIAN_POINT ( 'NONE',  ( -1.118353254094999860, 1516.977201124959947, 211.6155430111569729 ) ) ;
#15462 = B_SPLINE_CURVE_WITH_KNOTS ( 'NONE', 3,
 ( #29225, #20802, #55001, #46597 ),
 .UNSPECIFIED., .F., .F.,
 ( 4, 4 ),
 ( -49.62857927099999955, -30.39441596882049978 ),
 .UNSPECIFIED. ) ;
#15463 = CARTESIAN_POINT ( 'NONE',  ( -5.153093391039999638, 1380.759461119849902, 203.4632808174290233 ) ) ;
#15464 = CARTESIAN_POINT ( 'NONE',  ( 17.66967187227356817, 1517.051704408389924, 223.1030594000600900 ) ) ;
#15466 = CARTESIAN_POINT ( 'NONE',  ( 0.000000000000000000, 1512.187213306747481, 209.1218459616979999 ) ) ;
#15465 = CARTESIAN_POINT ( 'NONE',  ( -1.119439127814999990, 1517.026534522949987, 212.3908711059869745 ) ) ;
#15467 = CARTESIAN_POINT ( 'NONE',  ( -17.21868475540000176, 1485.486038110229856, 188.3681669011979807 ) ) ;
#15468 = DIRECTION ( 'NONE',  ( 1.755985294532469921E-16, -1.000000000000000000, 1.338183447452831989E-16 ) ) ;
#15469 = ORIENTED_EDGE ( 'NONE', *, *, #22282, .T. ) ;
#15470 = CARTESIAN_POINT ( 'NONE',  ( -26.01569841849999776, 1436.364670503799744, 136.8463858237979878 ) ) ;
#15471 = CARTESIAN_POINT ( 'NONE',  ( 4.033653264325000265, 1517.028034847769959, 202.5611037067669997 ) ) ;
#15472 = EDGE_CURVE ( 'NONE', #90117, #81438, #88400, .T. ) ;
#15473 = CARTESIAN_POINT ( 'NONE',  ( -7.526515395903619954, 1517.051704408389924, 208.6825894896870182 ) ) ;
#15474 = CARTESIAN_POINT ( 'NONE',  ( -30.25652781387339729, 1384.556785492720110, 205.7254385433210189 ) ) ;
#15475 = CARTESIAN_POINT ( 'NONE',  ( -43.01346508794090084, 1430.448015371199972, 270.1100027560920580 ) ) ;
#15476 = CARTESIAN_POINT ( 'NONE',  ( -2.620823360909999789, 1483.467906750489874, 201.7239643817090098 ) ) ;
#15478 = ORIENTED_EDGE ( 'NONE', *, *, #109804, .F. ) ;
#15477 = CARTESIAN_POINT ( 'NONE',  ( -37.65047686723229958, 1442.773887284729881, 137.1096749952629921 ) ) ;
#15479 = ORIENTED_EDGE ( 'NONE', *, *, #86, .F. ) ;
#15480 = CARTESIAN_POINT ( 'NONE',  ( 5.745386292849999244, 1451.922981708390125, 211.2075068023790152 ) ) ;
#15481 = CARTESIAN_POINT ( 'NONE',  ( -31.23437356469455040, 1511.187213306747708, 195.3468678195118287 ) ) ;
#15482 = CARTESIAN_POINT ( 'NONE',  ( -12.96458870010000020, 1380.564911143250129, 203.9320203105589826 ) ) ;
#15483 = CARTESIAN_POINT ( 'NONE',  ( -24.81662394629999824, 1435.862065122790000, 137.5270316210979900 ) ) ;
#15484 = CARTESIAN_POINT ( 'NONE',  ( -24.90625602310000275, 1442.467917342170267, 210.4928140592879799 ) ) ;
#15485 = CARTESIAN_POINT ( 'NONE',  ( -0.7350232362959980836, 1516.970035769810011, 211.4194755912870107 ) ) ;
#15486 = CARTESIAN_POINT ( 'NONE',  ( -68.76593665590000626, 1379.747941725510145, 280.1891108434590478 ) ) ;
#15487 = EDGE_CURVE ( 'NONE', #12262, #58610, #102237, .T. ) ;
#15488 = DIRECTION ( 'NONE',  ( 0.000000000000000000, 1.000000000000000000, 0.000000000000000000 ) ) ;
#15489 = CARTESIAN_POINT ( 'NONE',  ( 3.672250414928510676, 1440.842333270420340, 156.5454195792117673 ) ) ;
#15490 = CARTESIAN_POINT ( 'NONE',  ( -6.563595907815000352, 1517.154223579619838, 206.8322214998769937 ) ) ;
#15491 = VERTEX_POINT ( 'NONE', #71082 ) ;
#15492 = DIRECTION ( 'NONE',  ( 0.000000000000000000, 0.000000000000000000, -1.000000000000000000 ) ) ;
#15493 = CARTESIAN_POINT ( 'NONE',  ( -11.44291211132249941, 1428.994970299889928, 123.0295630242879952 ) ) ;
#15494 = CARTESIAN_POINT ( 'NONE',  ( -1.512515161746819920E-15, 1385.198152793140025, 218.6122691739390120 ) ) ;
#15495 = ORIENTED_EDGE ( 'NONE', *, *, #13498, .F. ) ;
#15496 = CARTESIAN_POINT ( 'NONE',  ( 19.87935007599999793, 1476.501528767390027, 213.0784012132189957 ) ) ;
#15497 = DIRECTION ( 'NONE',  ( 0.4604555384065119883, -0.2169306526911162492, 0.8607681389745879263 ) ) ;
#15498 = CARTESIAN_POINT ( 'NONE',  ( 4.380088106299919737, 1459.297325631019930, 233.6318968629059896 ) ) ;
#15499 = CARTESIAN_POINT ( 'NONE',  ( 17.12015143466563671, 1526.107880201381477, 182.3088744090234172 ) ) ;
#15500 = CARTESIAN_POINT ( 'NONE',  ( 23.96868460540000001, 1452.076057926130034, 136.6875046473980149 ) ) ;
#15501 = CARTESIAN_POINT ( 'NONE',  ( 10.57339846829999885, 1490.054618766489966, 202.8450963736189863 ) ) ;
#15502 = CARTESIAN_POINT ( 'NONE',  ( 0.000000000000000000, 1523.382868172864164, 209.1218459616979999 ) ) ;
#15503 = CARTESIAN_POINT ( 'NONE',  ( 23.33267522454316278, 1449.572396795839040, 217.2601772566924581 ) ) ;
#15505 = CARTESIAN_POINT ( 'NONE',  ( -12.00000000000000000, 1443.913060387330006, 147.5878346084980137 ) ) ;
#15504 = CARTESIAN_POINT ( 'NONE',  ( -1.704794841465000044, 1517.096587378560116, 213.7484378375869767 ) ) ;
#15506 = CARTESIAN_POINT ( 'NONE',  ( 18.30025784240000064, 1431.961054190390087, 210.0255047360110154 ) ) ;
#15507 = CARTESIAN_POINT ( 'NONE',  ( -1.708747662384999977, 1517.213554313520035, 216.0740123525270064 ) ) ;
#15508 = VERTEX_POINT ( 'NONE', #79999 ) ;
#15509 = DIRECTION ( 'NONE',  ( 1.000000000000000000, 0.000000000000000000, 0.000000000000000000 ) ) ;
#15510 = ADVANCED_FACE ( 'NONE', ( #62124 ), #8541, .T. ) ;
#15511 = CARTESIAN_POINT ( 'NONE',  ( -16.57637045210000082, 1420.575130030530090, 203.2586717730690111 ) ) ;
#15512 = CARTESIAN_POINT ( 'NONE',  ( 2.347483145930000070, 1420.008254648030061, 185.1099769671980084 ) ) ;
#15513 = CARTESIAN_POINT ( 'NONE',  ( 1.458875156680665475, 1414.913372219064740, 192.1265211809087532 ) ) ;
#15514 = EDGE_CURVE ( 'NONE', #67100, #69813, #30036, .T. ) ;
#15515 = CARTESIAN_POINT ( 'NONE',  ( 3.237065521149570912, 1524.843416604498543, 176.5220937283001774 ) ) ;
#15516 = CARTESIAN_POINT ( 'NONE',  ( 11113.05219665069490, 50.13405481564041821, 8751.225064238969935 ) ) ;
#15517 = CARTESIAN_POINT ( 'NONE',  ( -11.32617949625089970, 1471.108170639839955, 207.7151593947669994 ) ) ;
#15518 = CARTESIAN_POINT ( 'NONE',  ( 1.762089052713846193, 1416.154897214564016, 232.4884135401189269 ) ) ;
#15519 = B_SPLINE_CURVE_WITH_KNOTS ( 'NONE', 3,
 ( #88479, #55437, #99055, #89567, #39723, #72246 ),
 .UNSPECIFIED., .F., .F.,
 ( 4, 2, 4 ),
 ( 0.000000000000000000, 0.5000000000000000000, 1.000000000000000000 ),
 .UNSPECIFIED. ) ;
#15520 = CARTESIAN_POINT ( 'NONE',  ( 17.67984484133276979, 1423.296779864863993, 226.2374533289532224 ) ) ;
#15521 = CARTESIAN_POINT ( 'NONE',  ( -32.02808312589908013, 1512.187213306747481, 220.9649204700466782 ) ) ;
#15522 = DIRECTION ( 'NONE',  ( 0.000000000000000000, 0.000000000000000000, -1.000000000000000000 ) ) ;
#15523 = CARTESIAN_POINT ( 'NONE',  ( 40.10692519302580195, 1440.913060364430066, 259.4359539563330372 ) ) ;
#15525 = CARTESIAN_POINT ( 'NONE',  ( 4.328142686769970382, 1515.114670419599861, 208.1949246329089931 ) ) ;
#15524 = CARTESIAN_POINT ( 'NONE',  ( -11.36188915788260090, 1470.553325319990108, 210.0693210479820152 ) ) ;
#15526 = CARTESIAN_POINT ( 'NONE',  ( 13.07075197220000184, 1426.017600903129960, 222.5644795257979922 ) ) ;
#15527 = ORIENTED_EDGE ( 'NONE', *, *, #90425, .F. ) ;
#15528 = ORIENTED_EDGE ( 'NONE', *, *, #31835, .F. ) ;
#15529 = CARTESIAN_POINT ( 'NONE',  ( -6.599309851546266259, 1506.776552836644441, 230.5385063488150479 ) ) ;
#15530 = VECTOR ( 'NONE', #7801, 999.9999999999998863 ) ;
#15531 = CARTESIAN_POINT ( 'NONE',  ( -28.32265151400000036, 1509.673549454329759, 210.9825397456980056 ) ) ;
#15532 = CARTESIAN_POINT ( 'NONE',  ( 11.35657976162540095, 1502.829282324059932, 211.1038090253330211 ) ) ;
#15533 = CARTESIAN_POINT ( 'NONE',  ( 1847.405368200919384, -8387.357407334282470, 1585.835250321477815 ) ) ;
#15534 = CARTESIAN_POINT ( 'NONE',  ( 24.63413957469291304, 1509.887610572149470, 226.3134076709914382 ) ) ;
#15535 = CARTESIAN_POINT ( 'NONE',  ( -11.78824854703250047, 1517.051704408389924, 206.8304425649369875 ) ) ;
#15536 = CARTESIAN_POINT ( 'NONE',  ( -4.325805487360000257, 1515.203924463989779, 207.6586276196590006 ) ) ;
#15537 = CARTESIAN_POINT ( 'NONE',  ( -65.17440126354809138, 1383.790278610199948, 288.6850384825009996 ) ) ;
#15538 = CARTESIAN_POINT ( 'NONE',  ( 24.24033398420000296, 1452.066569271830076, 137.1576855576979881 ) ) ;
#15539 = CARTESIAN_POINT ( 'NONE',  ( 4.550353367526756898, 1466.224087956547919, 218.4072860836689927 ) ) ;
#15540 = FACE_OUTER_BOUND ( 'NONE', #70237, .T. ) ;
#15542 = ORIENTED_EDGE ( 'NONE', *, *, #103236, .T. ) ;
#15541 = CARTESIAN_POINT ( 'NONE',  ( -2.137491047500000185, 1455.891788169089978, 218.3487140958189912 ) ) ;
#15543 = CARTESIAN_POINT ( 'NONE',  ( 19.53786426059039982, 1512.187213306747481, 237.7197124308265188 ) ) ;
#15544 = CARTESIAN_POINT ( 'NONE',  ( -57.73766270559999469, 1379.143380400379783, 257.1610347018590232 ) ) ;
#15545 = CARTESIAN_POINT ( 'NONE',  ( -16.64778510051399962, 1409.494413853340120, 224.2640743094200104 ) ) ;
#15546 = ORIENTED_EDGE ( 'NONE', *, *, #70127, .T. ) ;
#15547 = ORIENTED_EDGE ( 'NONE', *, *, #110208, .T. ) ;
#15548 = CARTESIAN_POINT ( 'NONE',  ( -8.210973799569998732, 1501.032796100090081, 209.1036754092109788 ) ) ;
#15549 = CARTESIAN_POINT ( 'NONE',  ( 34.63223096084099950, 1437.077591941980018, 136.5438288522229868 ) ) ;
#15551 = CYLINDRICAL_SURFACE ( 'NONE', #16216, 1.999999999999998668 ) ;
#15550 = LINE ( 'NONE', #41883, #26282 ) ;
#15552 = CARTESIAN_POINT ( 'NONE',  ( -8.494781050700002112, 1461.600995454589793, 204.2538046751789977 ) ) ;
#15553 = CARTESIAN_POINT ( 'NONE',  ( -107.1873477440000073, 1379.571931949629970, 299.3438537678590023 ) ) ;
#15554 = CARTESIAN_POINT ( 'NONE',  ( -7.628773549489999972, 1416.913060387330006, 201.4930723711279938 ) ) ;
#15555 = CARTESIAN_POINT ( 'NONE',  ( -18.19590854888121356, 1522.382868172863937, 238.2026672068777202 ) ) ;
#15556 = CARTESIAN_POINT ( 'NONE',  ( -8.229900059930191247, 1508.551704408389924, 218.8850718935309771 ) ) ;
#15557 = DIRECTION ( 'NONE',  ( -1.755985294532469921E-16, 1.000000000000000000, -1.338183447452831989E-16 ) ) ;
#15558 = CARTESIAN_POINT ( 'NONE',  ( 18.28913704150000186, 1425.363277320230054, 225.3253160533980122 ) ) ;
#15559 = CARTESIAN_POINT ( 'NONE',  ( 4.401092417150000102, 1420.174153566729956, 185.7217845719979721 ) ) ;
#15560 = CARTESIAN_POINT ( 'NONE',  ( 4.082546718995279988, 1433.473438342260124, 201.5982916962979914 ) ) ;
#15561 = CARTESIAN_POINT ( 'NONE',  ( -2.500000000000000000, 1439.625347662559989, 166.9460400830979836 ) ) ;
#15562 = AXIS2_PLACEMENT_3D ( 'NONE', #61471, #60921, #1008 ) ;
#15563 = CARTESIAN_POINT ( 'NONE',  ( -3.179421471999289928, 1451.291958863610262, 184.8185991936910000 ) ) ;
#15564 = EDGE_LOOP ( 'NONE', ( #44976, #64853, #58273, #63332 ) ) ;
#15565 = FACE_OUTER_BOUND ( 'NONE', #75820, .T. ) ;
#15566 = CARTESIAN_POINT ( 'NONE',  ( 15.71062681160000096, 1468.834934971430130, 189.3083005990980041 ) ) ;
#15567 = CARTESIAN_POINT ( 'NONE',  ( -1.145689533615760081E-08, 1473.590260269789951, 262.5080731529990317 ) ) ;
#15568 = CARTESIAN_POINT ( 'NONE',  ( 1.842963721827329815, 1515.551704300040001, 212.9514659606769840 ) ) ;
#15569 = CARTESIAN_POINT ( 'NONE',  ( -2.657845259230000146, 1476.012816621789852, 198.9905392320989961 ) ) ;
#15570 = CARTESIAN_POINT ( 'NONE',  ( -106.7983762909999967, 1389.555420353100089, 308.8839675026590044 ) ) ;
#15571 = CARTESIAN_POINT ( 'NONE',  ( -0.9017680944290000777, 1482.202343265330001, 182.1243025875980095 ) ) ;
#15572 = CARTESIAN_POINT ( 'NONE',  ( -9.122811643198552645, 1360.526723316428388, 209.6218459617033432 ) ) ;
#15573 = DIRECTION ( 'NONE',  ( -5.980589973904019347E-17, 1.000000000000000000, -1.736889445713099699E-16 ) ) ;
#15574 = CARTESIAN_POINT ( 'NONE',  ( 1.197195770085190070, 1429.524192212559910, 217.3433698247590087 ) ) ;
#15575 = CARTESIAN_POINT ( 'NONE',  ( -8.255467494119999472, 1424.664513863459888, 207.0640964688590202 ) ) ;
#15576 = CARTESIAN_POINT ( 'NONE',  ( 5.781585778145000631, 1516.939646076049939, 209.1093989964429909 ) ) ;
#15577 = CARTESIAN_POINT ( 'NONE',  ( 6.224176841430179685, 1407.473636843709983, 220.5349837105389668 ) ) ;
#15578 = CIRCLE ( 'NONE', #49602, 2.000000000000003553 ) ;
#15579 = CARTESIAN_POINT ( 'NONE',  ( -2.453592884419999615E-14, 1422.045703177329870, 122.9811571859980006 ) ) ;
#15580 = CARTESIAN_POINT ( 'NONE',  ( 7.445112198176509821, 1425.205606764170170, 212.3599477002399851 ) ) ;
#15581 = CARTESIAN_POINT ( 'NONE',  ( -27.01426103600620365, 1451.969699918799961, 134.9176446824099855 ) ) ;
#15582 = ORIENTED_EDGE ( 'NONE', *, *, #104815, .T. ) ;
#15583 = CARTESIAN_POINT ( 'NONE',  ( 27.84455140360000058, 1437.266142704849926, 231.9094040490980149 ) ) ;
#15585 = CARTESIAN_POINT ( 'NONE',  ( -15.16811422921670172, 1512.319979277489892, 221.9811700865099908 ) ) ;
#15584 = CARTESIAN_POINT ( 'NONE',  ( -3.465864926880000141, 1452.704890687129819, 183.2873751387980121 ) ) ;
#15586 = DIRECTION ( 'NONE',  ( -0.000000000000000000, -1.000000000000000000, -0.000000000000000000 ) ) ;
#15587 = CARTESIAN_POINT ( 'NONE',  ( -19.74442643839703138, 1455.875379727006475, 227.8590200339708929 ) ) ;
#15588 = CARTESIAN_POINT ( 'NONE',  ( 7.722580314247720068, 1517.051704408590012, 209.5565402419049974 ) ) ;
#15589 = CARTESIAN_POINT ( 'NONE',  ( -13.44062186829930106, 1452.443703529229879, 148.8745159939319933 ) ) ;
#15590 = CARTESIAN_POINT ( 'NONE',  ( 5.615127104817687176, 1507.508085020990166, 219.4002671829225619 ) ) ;
#15591 = EDGE_LOOP ( 'NONE', ( #42562, #44273 ) ) ;
#15592 = CARTESIAN_POINT ( 'NONE',  ( -5.360343714066329923, 1422.242870833739971, 144.1500373561570143 ) ) ;
#15593 = CARTESIAN_POINT ( 'NONE',  ( 17.84338787552646366, 1523.481610118012441, 237.8836641335914237 ) ) ;
#15594 = CARTESIAN_POINT ( 'NONE',  ( 13.40016148240000149, 1419.519095471729997, 228.7855739235980082 ) ) ;
#15595 = CARTESIAN_POINT ( 'NONE',  ( -3.303457341579222550, 1448.967173816104150, 184.7286116801498395 ) ) ;
#15596 = VERTEX_POINT ( 'NONE', #23383 ) ;
#15597 = ORIENTED_EDGE ( 'NONE', *, *, #44069, .F. ) ;
#15598 = CARTESIAN_POINT ( 'NONE',  ( -73.12043787219998592, 1384.880583958779880, 272.3393879815590140 ) ) ;
#15599 = CARTESIAN_POINT ( 'NONE',  ( -23.70979485039999801, 1410.153424641430092, 209.4799370654980066 ) ) ;
#15600 = EDGE_LOOP ( 'NONE', ( #95176, #26120, #41531, #3794, #5621 ) ) ;
#15601 = CARTESIAN_POINT ( 'NONE',  ( -102.0933291366000049, 1371.894749952190068, 310.3987084017590519 ) ) ;
#15602 = AXIS2_PLACEMENT_3D ( 'NONE', #17025, #68594, #93748 ) ;
#15603 = CARTESIAN_POINT ( 'NONE',  ( -45.59505516556443183, 1438.873040481220869, 266.1907254621848438 ) ) ;
#15604 = CARTESIAN_POINT ( 'NONE',  ( -2.491473724000000001, 1498.351190470029906, 236.5406736864979962 ) ) ;
#15605 = CARTESIAN_POINT ( 'NONE',  ( -18.88570507609999893, 1415.855488934629875, 223.6420118195979967 ) ) ;
#15606 = EDGE_LOOP ( 'NONE', ( #103627, #50737, #93540, #5336, #99801 ) ) ;
#15607 = EDGE_CURVE ( 'NONE', #93915, #69834, #83378, .T. ) ;
#15608 = CARTESIAN_POINT ( 'NONE',  ( 45.72295278579319699, 1446.162187926870047, 266.9864112351669974 ) ) ;
#15609 = CARTESIAN_POINT ( 'NONE',  ( -10.92223504695139980, 1391.913060387089899, 205.7923380047099897 ) ) ;
#15610 = CARTESIAN_POINT ( 'NONE',  ( -0.02429775703179999635, 1420.196383118029871, 183.9091808095979843 ) ) ;
#15611 = CARTESIAN_POINT ( 'NONE',  ( -2.877744984375000037, 1516.723920667490120, 204.5127816287269980 ) ) ;
#15612 = ORIENTED_EDGE ( 'NONE', *, *, #3058, .T. ) ;
#15613 = CARTESIAN_POINT ( 'NONE',  ( -11.32027785699999889, 1433.946929803360035, 151.5080542412979980 ) ) ;
#15614 = CARTESIAN_POINT ( 'NONE',  ( 15.23581456386730082, 1513.231391185889834, 194.9678178315319883 ) ) ;
#15615 = CARTESIAN_POINT ( 'NONE',  ( 2.898715468759999858, 1428.109906398889962, 213.6762267714089774 ) ) ;
#15616 = ORIENTED_EDGE ( 'NONE', *, *, #71049, .T. ) ;
#15617 = CARTESIAN_POINT ( 'NONE',  ( -10.41425093117460143, 1479.497781561380179, 210.3960398642789755 ) ) ;
#15619 = EDGE_CURVE ( 'NONE', #43462, #36571, #107534, .T. ) ;
#15618 = CARTESIAN_POINT ( 'NONE',  ( 26.54187722018520290, 1451.986211319630002, 134.9387109740829942 ) ) ;
#15620 = CARTESIAN_POINT ( 'NONE',  ( -13.46561928155499999, 1512.674009804160050, 193.8142106494929919 ) ) ;
#15621 = CARTESIAN_POINT ( 'NONE',  ( 11.18883130367080092, 1502.419542440489977, 215.1996028960269882 ) ) ;
#15622 = CARTESIAN_POINT ( 'NONE',  ( 7.634170062339999063, 1421.957731401030060, 195.7691812542990135 ) ) ;
#15623 = CARTESIAN_POINT ( 'NONE',  ( -2.295483817934420134, 1432.805523517590018, 218.3736922701850176 ) ) ;
#15624 = CARTESIAN_POINT ( 'NONE',  ( 10.93777210243689879, 1478.839323300969909, 205.9316688570750102 ) ) ;
#15625 = CARTESIAN_POINT ( 'NONE',  ( 1.948679763128840170, 1408.981109784140017, 186.9136448737170042 ) ) ;
#15627 = CARTESIAN_POINT ( 'NONE',  ( -18.58256518043385341, 1424.379116010960161, 224.8999308456852191 ) ) ;
#15626 = CARTESIAN_POINT ( 'NONE',  ( 1.586289890350000009, 1417.233044477530029, 233.5609223597980133 ) ) ;
#15628 = CARTESIAN_POINT ( 'NONE',  ( 3.869327377972110682, 1441.524549520183427, 170.5363237134393160 ) ) ;
#15629 = CARTESIAN_POINT ( 'NONE',  ( -10.60340555500000015, 1379.609174620120029, 215.5963861307990044 ) ) ;
#15630 = CARTESIAN_POINT ( 'NONE',  ( 2.446787376320000096, 1432.353341358199941, 150.2884730787980061 ) ) ;
#15631 = ORIENTED_EDGE ( 'NONE', *, *, #71960, .F. ) ;
#15632 = CARTESIAN_POINT ( 'NONE',  ( 12.58433072604259984, 1415.426207913209964, 221.2617180145470002 ) ) ;
#15633 = CARTESIAN_POINT ( 'NONE',  ( 11.54407487136669985, 1432.339775672029873, 151.1365564868350191 ) ) ;
#15634 = CIRCLE ( 'NONE', #28227, 2.000010703461589490 ) ;
#15635 = CARTESIAN_POINT ( 'NONE',  ( -2.603248992506880022, 1366.156374083119999, 209.1218459584009963 ) ) ;
#15636 = CARTESIAN_POINT ( 'NONE',  ( -13.72218023960000011, 1389.845687919130114, 205.4181164005090068 ) ) ;
#15637 = CARTESIAN_POINT ( 'NONE',  ( 9.217393380133168890, 1426.476016588670063, 210.2456940754379957 ) ) ;
#15638 = CARTESIAN_POINT ( 'NONE',  ( 12.34756956475129996, 1421.260964715650061, 203.4353636828009826 ) ) ;
#15639 = CARTESIAN_POINT ( 'NONE',  ( -10.93951897979770038, 1462.702982771529832, 207.5546680835130076 ) ) ;
#15640 = CARTESIAN_POINT ( 'NONE',  ( -1.633469776390000128, 1432.353341358199941, 150.3624711946980028 ) ) ;
#15641 = CARTESIAN_POINT ( 'NONE',  ( -9.129309581573130217, 1383.864686136899991, 218.5281989956060045 ) ) ;
#15642 = CARTESIAN_POINT ( 'NONE',  ( 31.81407709660769001, 1522.382868172863937, 196.2902540610627682 ) ) ;
#15643 = CARTESIAN_POINT ( 'NONE',  ( 14.73695825029999895, 1462.639194746130215, 255.3819207682979595 ) ) ;
#15644 = CARTESIAN_POINT ( 'NONE',  ( 12.37273845029059949, 1415.932840154009909, 196.2621238876739937 ) ) ;
#15645 = CARTESIAN_POINT ( 'NONE',  ( 0.2550773510242848041, 1467.133396122514569, 235.6299148654997282 ) ) ;
#15646 = CARTESIAN_POINT ( 'NONE',  ( -106.8244771589985049, 1390.652608569862423, 299.9266001010461764 ) ) ;
#15647 = CARTESIAN_POINT ( 'NONE',  ( 5.253642672657390378, 1466.463266540510176, 217.7249926852120154 ) ) ;
#15648 = CARTESIAN_POINT ( 'NONE',  ( -18.36047073010000119, 1486.213210630329968, 188.6962080947980098 ) ) ;
#15649 = CARTESIAN_POINT ( 'NONE',  ( 4.606382372549210125, 1474.138419553830090, 219.5757164701410034 ) ) ;
#15650 = CARTESIAN_POINT ( 'NONE',  ( -17.39555449230000050, 1409.685578510729783, 224.7181607083980168 ) ) ;
#15651 = CIRCLE ( 'NONE', #105060, 1.999999999999998668 ) ;
#15652 = CARTESIAN_POINT ( 'NONE',  ( 23.95220588820000174, 1410.918936072130236, 210.1545993587979808 ) ) ;
#15653 = CARTESIAN_POINT ( 'NONE',  ( 1.433806162063078204, 1478.005084112435952, 198.7945331361510171 ) ) ;
#15654 = DIRECTION ( 'NONE',  ( -1.761221539070279927E-08, 1.000000000000000000, 5.441036071155500311E-09 ) ) ;
#15655 = CARTESIAN_POINT ( 'NONE',  ( -3.340600809453960203E-09, 1406.914525921759832, 196.1218459609590070 ) ) ;
#15656 = DIRECTION ( 'NONE',  ( -4.343610028670000616E-15, 1.498801083240000065E-15, -1.000000000000000000 ) ) ;
#15657 =( BOUNDED_CURVE ( )  B_SPLINE_CURVE ( 3, ( #78733, #44588, #87699, #3707 ),
 .UNSPECIFIED., .F., .T. ) 
 B_SPLINE_CURVE_WITH_KNOTS ( ( 4, 4 ),
 ( 3.320448054550920070, 3.390722914990644821 ),
 .UNSPECIFIED. ) 
 CURVE ( )  GEOMETRIC_REPRESENTATION_ITEM ( )  RATIONAL_B_SPLINE_CURVE ( ( 1.000000000000000000, 0.9995884960067018543, 0.9995884960067018543, 1.000000000000000000 ) ) 
 REPRESENTATION_ITEM ( '' )  );
#15658 = FACE_OUTER_BOUND ( 'NONE', #107184, .T. ) ;
#15659 = CARTESIAN_POINT ( 'NONE',  ( -3.877169465260000170, 1415.932617990029939, 227.1226588283979879 ) ) ;
#15660 = CARTESIAN_POINT ( 'NONE',  ( -15.18482336544590083, 1421.253453350580003, 203.4821423529160143 ) ) ;
#15661 = CARTESIAN_POINT ( 'NONE',  ( 0.2055174958574400024, 1459.873963670999956, 182.9584848020919878 ) ) ;
#15663 = ORIENTED_EDGE ( 'NONE', *, *, #66624, .T. ) ;
#15662 = CARTESIAN_POINT ( 'NONE',  ( 6.486349823423054772, 1465.915338427141933, 201.5941921811669886 ) ) ;
#15664 = CARTESIAN_POINT ( 'NONE',  ( -20.24673233129999872, 1444.324653571829913, 162.1129423953979938 ) ) ;
#15665 = CARTESIAN_POINT ( 'NONE',  ( -33.82146843645519851, 1444.740067931809335, 154.8031860135564273 ) ) ;
#15666 = CARTESIAN_POINT ( 'NONE',  ( 13.50070407659999994, 1434.968958018969943, 149.9809230249979919 ) ) ;
#15667 = CARTESIAN_POINT ( 'NONE',  ( -41.66155871503109864, 1443.633333536269902, 134.0999999981970063 ) ) ;
#15668 = CARTESIAN_POINT ( 'NONE',  ( -20.11385680769999951, 1487.601373209189887, 204.1067431612489997 ) ) ;
#15669 = ORIENTED_EDGE ( 'NONE', *, *, #20964, .F. ) ;
#15670 = CARTESIAN_POINT ( 'NONE',  ( -17.34064885126208466, 1525.506916460679804, 181.3217002936585516 ) ) ;
#15671 = PLANE ( 'NONE',  #79650 ) ;
#15672 = CARTESIAN_POINT ( 'NONE',  ( -105.6076294414992418, 1381.326326253046773, 309.0868219927184555 ) ) ;
#15673 = DIRECTION ( 'NONE',  ( 0.000000000000000000, 1.000000000000000000, 0.000000000000000000 ) ) ;
#15674 = B_SPLINE_CURVE_WITH_KNOTS ( 'NONE', 3,
 ( #81278, #56099, #57770, #91349, #92986, #6229, #91889, #6773, #14629, #75115, #5698, #57222, #41501, #25214, #67814, #101928, #23018 ),
 .UNSPECIFIED., .F., .F.,
 ( 4, 2, 2, 1, 1, 1, 1, 1, 2, 2, 4 ),
 ( 0.000000000000000000, 0.2499999999998790412, 0.4999999999997580824, 0.6249999999997010169, 0.6874999999996719291, 0.7187499999996564970, 0.7343749999996487254, 0.7421874999996495026, 0.7460937499996537214, 0.7499999999996578293, 1.000000000000000000 ),
 .UNSPECIFIED. ) ;
#15675 = CARTESIAN_POINT ( 'NONE',  ( -8.055949302434040504, 1436.374732820499958, 213.3353392178869967 ) ) ;
#15676 = CIRCLE ( 'NONE', #17531, 2.000000175757499665 ) ;
#15677 = DIRECTION ( 'NONE',  ( 0.000000000000000000, -0.7041802892087485333, -0.7100212111549085714 ) ) ;
#15678 = CARTESIAN_POINT ( 'NONE',  ( -14.13509333269999857, 1379.975727635469866, 211.1783289813689919 ) ) ;
#15679 = CARTESIAN_POINT ( 'NONE',  ( 4.261736552472805251, 1515.372048948338943, 210.9648081765028849 ) ) ;
#15680 = CARTESIAN_POINT ( 'NONE',  ( -58.69938589393059658, 1385.055105096270154, 241.2266681709880061 ) ) ;
#15681 = CARTESIAN_POINT ( 'NONE',  ( 12.74111629471100038, 1416.830086716310007, 196.2606222955850228 ) ) ;
#15682 = CARTESIAN_POINT ( 'NONE',  ( 10.23375359582179911, 1424.446042691910179, 207.3832406123669898 ) ) ;
#15683 = ORIENTED_EDGE ( 'NONE', *, *, #49785, .F. ) ;
#15684 = CARTESIAN_POINT ( 'NONE',  ( -33.30821264389999925, 1450.888620760030108, 136.1896499959979678 ) ) ;
#15685 = CARTESIAN_POINT ( 'NONE',  ( 16.68498601116327151, 1442.773887286369018, 162.0933193695679222 ) ) ;
#15687 = EDGE_LOOP ( 'NONE', ( #11090, #28742 ) ) ;
#15686 = CARTESIAN_POINT ( 'NONE',  ( 3.947090874974254149, 1427.113278099589934, 137.0999999980980704 ) ) ;
#15688 = CARTESIAN_POINT ( 'NONE',  ( 5.013709187000000789, 1473.458530729089944, 218.4934638050989975 ) ) ;
#15689 = EDGE_CURVE ( 'NONE', #23328, #13274, #68249, .T. ) ;
#15690 = CARTESIAN_POINT ( 'NONE',  ( -18.08558846253097485, 1410.907777525342681, 224.6300668642674907 ) ) ;
#15691 = FACE_OUTER_BOUND ( 'NONE', #92258, .T. ) ;
#15692 = CARTESIAN_POINT ( 'NONE',  ( -11.33192158569999819, 1414.988017870030035, 195.9133765299980041 ) ) ;
#15693 = ADVANCED_FACE ( 'NONE', ( #7148 ), #36025, .T. ) ;
#15694 = CARTESIAN_POINT ( 'NONE',  ( 2.500000000000000000, 1425.929641636930000, 126.8043280305979863 ) ) ;
#15695 = CARTESIAN_POINT ( 'NONE',  ( 15.87603342115862581, 1512.359593911811089, 198.0975645610432707 ) ) ;
#15696 = ADVANCED_FACE ( 'NONE', ( #59770 ), #27377, .F. ) ;
#15697 = CARTESIAN_POINT ( 'NONE',  ( -16.57130798100000035, 1422.287820404829972, 227.1266126762980093 ) ) ;
#15698 = CARTESIAN_POINT ( 'NONE',  ( 6.500020221522261110, 1497.924676537463711, 198.3229680000449662 ) ) ;
#15699 = CARTESIAN_POINT ( 'NONE',  ( 8.286340681629999594, 1448.851909210790154, 205.0448464285690306 ) ) ;
#15700 = CARTESIAN_POINT ( 'NONE',  ( -104.0419184806740134, 1314.643966242388842, 309.3341893170371577 ) ) ;
#15701 = CARTESIAN_POINT ( 'NONE',  ( 9.668109322589998555, 1408.913060387329779, 224.6723891271980165 ) ) ;
#15702 = AXIS2_PLACEMENT_3D ( 'NONE', #54032, #42975, #62996 ) ;
#15703 = CARTESIAN_POINT ( 'NONE',  ( -9.173749095941850840, 1450.559996438570124, 208.1432995907519796 ) ) ;
#15704 = CARTESIAN_POINT ( 'NONE',  ( 2.864972116015000125, 1516.859514182039902, 206.2412530031170093 ) ) ;
#15705 = VECTOR ( 'NONE', #14859, 1000.000000000000114 ) ;
#15706 = CARTESIAN_POINT ( 'NONE',  ( 2.705316712519999722, 1447.083576631230017, 165.9366036590980116 ) ) ;
#15707 = VERTEX_POINT ( 'NONE', #79878 ) ;
#15708 = CARTESIAN_POINT ( 'NONE',  ( 3.152929577590128929, 1465.382732736859225, 199.7633066961682857 ) ) ;
#15709 = CARTESIAN_POINT ( 'NONE',  ( -16.68599179819999989, 1461.099982565929849, 230.2790296985980092 ) ) ;
#15711 = ORIENTED_EDGE ( 'NONE', *, *, #38378, .F. ) ;
#15710 = CARTESIAN_POINT ( 'NONE',  ( -68.52665777820699589, 1379.747389946890053, 280.1435722370280246 ) ) ;
#15712 = CARTESIAN_POINT ( 'NONE',  ( -17.50517576071650083, 1417.698423450930022, 206.6604295572749947 ) ) ;
#15713 = ORIENTED_EDGE ( 'NONE', *, *, #35715, .T. ) ;
#15714 = AXIS2_PLACEMENT_3D ( 'NONE', #86137, #101811, #51997 ) ;
#15715 = CARTESIAN_POINT ( 'NONE',  ( -16.53955851760778373, 1513.001574290527287, 221.0043300851906451 ) ) ;
#15716 = CARTESIAN_POINT ( 'NONE',  ( 11.45577226660000036, 1502.286415424589904, 208.3140783707030153 ) ) ;
#15718 = CARTESIAN_POINT ( 'NONE',  ( 15.87459988598749838, 1409.570044024510025, 192.3777976961339959 ) ) ;
#15717 = CARTESIAN_POINT ( 'NONE',  ( 1.470421131539999982, 1428.420680932830237, 91.31218443469779800 ) ) ;
#15719 = CARTESIAN_POINT ( 'NONE',  ( 5.012938863775000087, 1517.051603658920158, 211.6026598552170128 ) ) ;
#15720 = CARTESIAN_POINT ( 'NONE',  ( 41.66134369672110438, 1443.796896187320044, 135.6885329911860083 ) ) ;
#15721 = CARTESIAN_POINT ( 'NONE',  ( -13.01666274260000122, 1409.302079604029814, 262.4458674292980049 ) ) ;
#15722 = DIRECTION ( 'NONE',  ( 1.755985294532464991E-16, -1.000000000000000000, 1.338183447452830017E-16 ) ) ;
#15723 = CARTESIAN_POINT ( 'NONE',  ( 15.67195723210528691, 1461.477347166320897, 229.6037306798920383 ) ) ;
#15724 = CARTESIAN_POINT ( 'NONE',  ( 39.75236484272360116, 1448.901857782450179, 134.0999999981239910 ) ) ;
#15725 = CARTESIAN_POINT ( 'NONE',  ( 7.105427357599999217E-15, 1410.913060387329779, 146.1721969590979882 ) ) ;
#15726 = ORIENTED_EDGE ( 'NONE', *, *, #52831, .F. ) ;
#15727 = CARTESIAN_POINT ( 'NONE',  ( -13.05162051250000133, 1467.538720777590015, 191.8992815354989716 ) ) ;
#15728 = DIRECTION ( 'NONE',  ( -1.755985294532469921E-16, 1.000000000000000000, -1.338183447452831989E-16 ) ) ;
#15729 = EDGE_LOOP ( 'NONE', ( #13813, #62398, #45571, #85347, #11825 ) ) ;
#15730 = ORIENTED_EDGE ( 'NONE', *, *, #76199, .T. ) ;
#15731 = CARTESIAN_POINT ( 'NONE',  ( -2.218918655950000041, 1431.115532604589816, 203.8893403826889994 ) ) ;
#15732 = CARTESIAN_POINT ( 'NONE',  ( 10.54758761917650034, 1452.770155221380037, 210.0494888551049826 ) ) ;
#15733 = CARTESIAN_POINT ( 'NONE',  ( -5.106228707209799822, 1507.795005401549815, 220.9628779089179886 ) ) ;
#15734 = AXIS2_PLACEMENT_3D ( 'NONE', #58267, #50427, #92389 ) ;
#15735 = CARTESIAN_POINT ( 'NONE',  ( -10.86173877940340127, 1417.961625830270577, 198.2022571467911405 ) ) ;
#15736 = CARTESIAN_POINT ( 'NONE',  ( 2.626093229311771804, 1468.533706331386838, 218.7919682226666112 ) ) ;
#15737 = CARTESIAN_POINT ( 'NONE',  ( -12.61779677260000021, 1379.111305426719809, 208.5419189764980104 ) ) ;
#15738 = CARTESIAN_POINT ( 'NONE',  ( 42.60628462810000627, 1443.705283505709758, 134.0999992373979808 ) ) ;
#15739 = CARTESIAN_POINT ( 'NONE',  ( 3.879787089154707491, 1516.685805519455926, 215.5416050467851221 ) ) ;
#15740 = PLANE ( 'NONE',  #37359 ) ;
#15741 = CARTESIAN_POINT ( 'NONE',  ( -11.28091541760000105, 1391.913060106340026, 212.5574219731489620 ) ) ;
#15742 = CARTESIAN_POINT ( 'NONE',  ( -78.28135749134220589, 1384.785472859150104, 280.7109069974439990 ) ) ;
#15743 = ORIENTED_EDGE ( 'NONE', *, *, #32296, .F. ) ;
#15744 = CARTESIAN_POINT ( 'NONE',  ( -4.036119682645000317, 1516.647924054489977, 201.7978713257969900 ) ) ;
#15745 = CARTESIAN_POINT ( 'NONE',  ( -5.789394700334999477, 1517.164987839469859, 207.4150481461570052 ) ) ;
#15746 = ORIENTED_EDGE ( 'NONE', *, *, #21409, .T. ) ;
#15747 = CARTESIAN_POINT ( 'NONE',  ( 11.76561647296150070, 1427.008901819209996, 146.1381330989469802 ) ) ;
#15748 = CARTESIAN_POINT ( 'NONE',  ( 4.822579926217737345, 1511.395344347225546, 217.5857078699854696 ) ) ;
#15749 = VERTEX_POINT ( 'NONE', #79325 ) ;
#15750 = CARTESIAN_POINT ( 'NONE',  ( 12.48860275614654824, 1384.926148861439970, 208.5962672545927603 ) ) ;
#15751 = EDGE_CURVE ( 'NONE', #93599, #94948, #52477, .T. ) ;
#15752 = CARTESIAN_POINT ( 'NONE',  ( -11.07540131138789974, 1432.346177062760034, 151.6859278047610076 ) ) ;
#15753 = CARTESIAN_POINT ( 'NONE',  ( -18.70861292059999670, 1442.610498708490013, 207.2775239616889849 ) ) ;
#15754 = CARTESIAN_POINT ( 'NONE',  ( -10.04998969390729968, 1462.307699121839960, 207.4528283373930151 ) ) ;
#15755 = CARTESIAN_POINT ( 'NONE',  ( -13.16128509840000049, 1426.050756123429892, 222.2185317868979837 ) ) ;
#15756 = CARTESIAN_POINT ( 'NONE',  ( 9.935891866850850462, 1468.906047781809775, 207.5492993768060046 ) ) ;
#15757 = CARTESIAN_POINT ( 'NONE',  ( -9.915987190420000985, 1473.542783144990153, 206.4139885101390064 ) ) ;
#15758 = CARTESIAN_POINT ( 'NONE',  ( 7.378495474280000188, 1492.475726123489949, 217.4190488244389883 ) ) ;
#15759 = CARTESIAN_POINT ( 'NONE',  ( -47.60661184359999254, 1379.710340994259923, 235.3636715871589900 ) ) ;
#15760 = CARTESIAN_POINT ( 'NONE',  ( -16.63654591560000284, 1507.631725828329991, 224.7122666342980040 ) ) ;
#15762 = DIRECTION ( 'NONE',  ( 0.7067700363771036720, 0.03085824620770448445, 0.7067700363771035610 ) ) ;
#15761 = CARTESIAN_POINT ( 'NONE',  ( 16.23843642359999606, 1460.007519691929929, 229.4167189755979734 ) ) ;
#15763 = PLANE ( 'NONE',  #15124 ) ;
#15764 = AXIS2_PLACEMENT_3D ( 'NONE', #87082, #102749, #2559 ) ;
#15765 = CARTESIAN_POINT ( 'NONE',  ( 2.485845998894999909, 1516.545806094630279, 216.4433018439569878 ) ) ;
#15766 = VERTEX_POINT ( 'NONE', #2636 ) ;
#15767 = DIRECTION ( 'NONE',  ( 0.000000000000000000, -1.000000000000000000, 0.000000000000000000 ) ) ;
#15768 = CARTESIAN_POINT ( 'NONE',  ( -21.80586012576711852, 1523.954924407825956, 234.9031818917333112 ) ) ;
#15769 = CARTESIAN_POINT ( 'NONE',  ( -4.999456428534999830, 1516.830644417779922, 213.7431138541670066 ) ) ;
#15770 = CARTESIAN_POINT ( 'NONE',  ( 3.582801916543969512, 1515.224507089990084, 213.1990874413949939 ) ) ;
#15771 = LINE ( 'NONE', #66794, #63523 ) ;
#15773 = ORIENTED_EDGE ( 'NONE', *, *, #27051, .T. ) ;
#15772 = CARTESIAN_POINT ( 'NONE',  ( 4.236980904132630066, 1508.610336716400070, 213.6558567133870099 ) ) ;
#15774 = CARTESIAN_POINT ( 'NONE',  ( 0.7130140427719999785, 1416.844618642330033, 190.3244982829980074 ) ) ;
#15775 = CARTESIAN_POINT ( 'NONE',  ( -15.57416828428110023, 1507.336004463039899, 192.5523032500569798 ) ) ;
#15776 = CARTESIAN_POINT ( 'NONE',  ( -11.21188824190000055, 1426.389936183530153, 148.4979915517980089 ) ) ;
#15777 = CARTESIAN_POINT ( 'NONE',  ( -0.2109842154640010070, 1429.925335880790271, 214.7594818389389957 ) ) ;
#15778 = CARTESIAN_POINT ( 'NONE',  ( -5.303217579353759703, 1442.879282873410148, 200.5942580338080177 ) ) ;
#15779 = CARTESIAN_POINT ( 'NONE',  ( 6.356853389496330387, 1423.329118960190044, 150.6733088057929990 ) ) ;
#15780 = FACE_OUTER_BOUND ( 'NONE', #55730, .T. ) ;
#15781 = CARTESIAN_POINT ( 'NONE',  ( 0.2730630983163809811, 1490.297625679229895, 187.5574216619969832 ) ) ;
#15782 = EDGE_CURVE ( 'NONE', #65683, #52693, #45741, .T. ) ;
#15784 = CARTESIAN_POINT ( 'NONE',  ( -10.77555132091760015, 1482.134168720230036, 206.6918653029249811 ) ) ;
#15783 = CARTESIAN_POINT ( 'NONE',  ( -19.34905394389999955, 1482.734125384130039, 228.2119762798980105 ) ) ;
#15785 = CARTESIAN_POINT ( 'NONE',  ( -8.540055685515531181, 1393.051435267420175, 234.7075627498410029 ) ) ;
#15786 = ORIENTED_EDGE ( 'NONE', *, *, #32901, .T. ) ;
#15788 = AXIS2_PLACEMENT_3D ( 'NONE', #42323, #33912, #59150 ) ;
#15787 = CARTESIAN_POINT ( 'NONE',  ( 2.284526458645000258, 1516.956048353049937, 205.6588971355569981 ) ) ;
#15789 = CARTESIAN_POINT ( 'NONE',  ( 12.52700422740000086, 1408.033343574530136, 269.6003762864979763 ) ) ;
#15790 = CARTESIAN_POINT ( 'NONE',  ( -0.0001187281342228439996, 1508.967929526819944, 179.3767679645770272 ) ) ;
#15791 = CARTESIAN_POINT ( 'NONE',  ( 25.15310117689999814, 1469.151800109529859, 206.3831926792579736 ) ) ;
#15792 = VECTOR ( 'NONE', #34654, 1000.000000000000000 ) ;
#15793 = CARTESIAN_POINT ( 'NONE',  ( 3.938313870213109524, 1506.361927106564735, 230.7614585987053886 ) ) ;
#15794 = CARTESIAN_POINT ( 'NONE',  ( -10.17157269315458556, 1390.403795797951034, 216.1384918992431494 ) ) ;
#15795 = FACE_OUTER_BOUND ( 'NONE', #17942, .T. ) ;
#15796 = CARTESIAN_POINT ( 'NONE',  ( 7.878537825433329367, 1522.051704408389924, 200.0586249522280013 ) ) ;
#15797 = CARTESIAN_POINT ( 'NONE',  ( -15.48826635719999878, 1416.228753145889868, 207.4514652343489729 ) ) ;
#15798 = CARTESIAN_POINT ( 'NONE',  ( -13.37869130550000030, 1446.597787909739964, 188.1529836615980003 ) ) ;
#15799 = CARTESIAN_POINT ( 'NONE',  ( -20.46339790889999932, 1475.513060387329915, 212.9932575586580015 ) ) ;
#15800 = CARTESIAN_POINT ( 'NONE',  ( -16.45418660414503975, 1419.665052300104435, 209.4254846085501072 ) ) ;
#15801 = CARTESIAN_POINT ( 'NONE',  ( -3.685267454909999962, 1496.073671761789910, 219.7127564024990249 ) ) ;
#15802 = CARTESIAN_POINT ( 'NONE',  ( 1.464172579227420057, 1491.938057517099878, 181.7751837965830077 ) ) ;
#15803 = CARTESIAN_POINT ( 'NONE',  ( -6.215408291180000155, 1427.423536210930024, 214.3676144197379756 ) ) ;
#15804 = CARTESIAN_POINT ( 'NONE',  ( 10.57423073640600109, 1481.617106639790109, 209.5624278184519937 ) ) ;
#15805 = DIRECTION ( 'NONE',  ( 0.000000000000000000, 0.000000000000000000, 1.000000000000000000 ) ) ;
#15806 = CARTESIAN_POINT ( 'NONE',  ( -3.427369262309999609, 1475.739996263529974, 266.9564229772980752 ) ) ;
#15808 = AXIS2_PLACEMENT_3D ( 'NONE', #45527, #2973, #79668 ) ;
#15807 = CARTESIAN_POINT ( 'NONE',  ( -5.489226980809999823, 1448.625211962289995, 211.5470588626189965 ) ) ;
#15809 = CARTESIAN_POINT ( 'NONE',  ( -22.01225108839999933, 1509.713483275730141, 189.1785030504979943 ) ) ;
#15810 = EDGE_CURVE ( 'NONE', #328, #21613, #53029, .T. ) ;
#15811 = CARTESIAN_POINT ( 'NONE',  ( -3.527569048119670203, 1486.518325592330029, 181.8541486797999767 ) ) ;
#15812 = CARTESIAN_POINT ( 'NONE',  ( -53.13680734357709667, 1384.725240562959925, 268.1326697647110109 ) ) ;
#15813 = CARTESIAN_POINT ( 'NONE',  ( -106.4392312446289992, 1391.913060387289988, 303.5569487479260147 ) ) ;
#15814 = CARTESIAN_POINT ( 'NONE',  ( -3.282394052629999948, 1438.199601172570055, 155.5836490844979778 ) ) ;
#15815 = CARTESIAN_POINT ( 'NONE',  ( -106.8359495019999912, 1379.429462365020072, 299.8958288151589500 ) ) ;
#15816 = CARTESIAN_POINT ( 'NONE',  ( 4.138993644310000164, 1515.551749209589843, 208.7474387692110156 ) ) ;
#15817 = CARTESIAN_POINT ( 'NONE',  ( -14.28127427822060014, 1474.301216932419948, 223.9347614794640151 ) ) ;
#15818 = ADVANCED_FACE ( 'NONE', ( #3192 ), #80174, .F. ) ;
#15819 = CARTESIAN_POINT ( 'NONE',  ( -17.84692650809999748, 1410.032952996529957, 195.3924047753979778 ) ) ;
#15820 = EDGE_CURVE ( 'NONE', #31171, #29814, #25269, .T. ) ;
#15821 = CARTESIAN_POINT ( 'NONE',  ( -12.18433968541703116, 1377.735202854164072, 207.2844700481445841 ) ) ;
#15822 = CARTESIAN_POINT ( 'NONE',  ( -1.317811661047102678, 1522.051704408389924, 194.7136484256038500 ) ) ;
#15823 = CARTESIAN_POINT ( 'NONE',  ( 10.17199984938910085, 1480.651875719519921, 206.3463171831010072 ) ) ;
#15824 = EDGE_CURVE ( 'NONE', #63638, #45257, #63403, .T. ) ;
#15825 = ORIENTED_EDGE ( 'NONE', *, *, #64415, .F. ) ;
#15826 = FACE_OUTER_BOUND ( 'NONE', #58034, .T. ) ;
#15827 = EDGE_CURVE ( 'NONE', #54724, #49707, #14300, .T. ) ;
#15828 = CARTESIAN_POINT ( 'NONE',  ( 4.770050319527739724, 1435.280277859259968, 228.7600612000269678 ) ) ;
#15829 = CARTESIAN_POINT ( 'NONE',  ( -7.545803654736770838, 1510.531931302273733, 214.8296908414164363 ) ) ;
#15830 = CARTESIAN_POINT ( 'NONE',  ( 5.140110055453729565, 1436.845560459350054, 228.7442478949189990 ) ) ;
#15832 = CARTESIAN_POINT ( 'NONE',  ( -15.21523573936500107, 1514.242353506929931, 194.1595280392670020 ) ) ;
#15831 = CARTESIAN_POINT ( 'NONE',  ( 11.73701142390000030, 1426.696005485330033, 144.1689090389980095 ) ) ;
#15833 = CARTESIAN_POINT ( 'NONE',  ( 11.70306882791220104, 1426.718062415309987, 141.7392483422370049 ) ) ;
#15834 = CARTESIAN_POINT ( 'NONE',  ( 17.12660205615345888, 1524.374578187333555, 237.3020490138461867 ) ) ;
#15835 = DIRECTION ( 'NONE',  ( 0.9996573249755517088, 0.02617694830808744988, 0.000000000000000000 ) ) ;
#15836 = CYLINDRICAL_SURFACE ( 'NONE', #14135, 2.999999999999996447 ) ;
#15837 = EDGE_CURVE ( 'NONE', #101369, #35225, #43359, .T. ) ;
#15838 = CARTESIAN_POINT ( 'NONE',  ( -33.35590117750189876, 1523.678648413191695, 216.3310373540461171 ) ) ;
#15839 = CARTESIAN_POINT ( 'NONE',  ( 3.451033388965000004, 1517.025653221279981, 203.3353183697670090 ) ) ;
#15840 = DIRECTION ( 'NONE',  ( 1.000000000000000000, 0.000000000000000000, 0.000000000000000000 ) ) ;
#15841 = CARTESIAN_POINT ( 'NONE',  ( -12.84729496320930409, 1398.293704436309099, 206.6733356016319476 ) ) ;
#15842 = CARTESIAN_POINT ( 'NONE',  ( 16.62677414043499979, 1512.592133792520144, 196.9623649671669909 ) ) ;
#15843 = DIRECTION ( 'NONE',  ( 0.000000000000000000, -0.4134839022732319513, 0.9105114291215131717 ) ) ;
#15844 = CARTESIAN_POINT ( 'NONE',  ( -7.459448365662689540, 1377.973318082249989, 211.7927975196730017 ) ) ;
#15845 = CARTESIAN_POINT ( 'NONE',  ( 3.005276066430000448, 1369.205039411269809, 207.6218459616989946 ) ) ;
#15847 = ORIENTED_EDGE ( 'NONE', *, *, #86062, .T. ) ;
#15846 = CARTESIAN_POINT ( 'NONE',  ( -29.87190587263160069, 1379.676854917029914, 217.9309857436469997 ) ) ;
#15848 = B_SPLINE_CURVE_WITH_KNOTS ( 'NONE', 3,
 ( #66518, #74904, #23905, #13299, #82735, #82175, #73804, #83283, #23368, #65959 ),
 .UNSPECIFIED., .F., .F.,
 ( 4, 3, 3, 4 ),
 ( -24.01273564469999755, -23.57996764826259906, -22.12139829086160248, -20.66572445029999727 ),
 .UNSPECIFIED. ) ;
#15849 = ORIENTED_EDGE ( 'NONE', *, *, #40174, .T. ) ;
#15850 = CARTESIAN_POINT ( 'NONE',  ( 11.99679312889339933, 1433.670206490089868, 149.8488618923190359 ) ) ;
#15851 = CARTESIAN_POINT ( 'NONE',  ( -2.680633533590000006, 1397.680629565529898, 222.1367961445980086 ) ) ;
#15852 = ORIENTED_EDGE ( 'NONE', *, *, #78829, .F. ) ;
#15853 = CARTESIAN_POINT ( 'NONE',  ( -106.3126565290000087, 1379.599899938080171, 307.8895711306589646 ) ) ;
#15854 = CARTESIAN_POINT ( 'NONE',  ( -26.80004305949999832, 1509.848938513930079, 198.9467878708979924 ) ) ;
#15855 = FACE_OUTER_BOUND ( 'NONE', #59873, .T. ) ;
#15857 = DIRECTION ( 'NONE',  ( -1.836970198721029688E-16, -1.000000000000000000, 0.000000000000000000 ) ) ;
#15856 = CARTESIAN_POINT ( 'NONE',  ( -0.2549939780409989920, 1442.897942418790080, 200.2186398693189915 ) ) ;
#15858 = CARTESIAN_POINT ( 'NONE',  ( 19.99034456412450211, 1507.818693454599952, 229.1208657279370016 ) ) ;
#15859 = ADVANCED_FACE ( 'NONE', ( #89370 ), #76424, .F. ) ;
#15860 = CARTESIAN_POINT ( 'NONE',  ( 2.856234944690000166, 1468.704783001229771, 183.0951156081980002 ) ) ;
#15861 = CARTESIAN_POINT ( 'NONE',  ( -9.382530293249999431, 1414.913060387329779, 195.0067469954979913 ) ) ;
#15862 = LINE ( 'NONE', #50067, #47650 ) ;
#15863 = FILL_AREA_STYLE ('',( #26493 ) ) ;
#15864 = B_SPLINE_SURFACE_WITH_KNOTS ( 'NONE', 5, 5, ( 
 ( #80464, #64227, #22714, #88858, #63684, #46878 ),
 ( #107852, #22166, #89408, #46334, #37910, #30599 ),
 ( #91045, #63147, #31141, #56913, #72615, #97248 ),
 ( #72092, #14333, #82096, #97795, #21072, #12696 ),
 ( #64787, #55828, #38984, #73161, #4312, #106746 ),
 ( #20524, #48523, #98897, #47414, #81005, #13223 ),
 ( #3228, #4837, #13771, #37355, #71555, #56364 ),
 ( #90496, #47955, #105675, #58022, #49074, #93785 ),
 ( #74280, #15976, #108967, #32793, #40650, #110062 ) ),
 .UNSPECIFIED., .F., .F., .F.,
 ( 6, 3, 6 ),
 ( 6, 6 ),
 ( 134.5636516019999931, 157.0233722590000127, 167.1797832720000088 ),
 ( -2.775557561569999727E-17, 2.000000000000000000 ),
 .UNSPECIFIED. ) ;
#15866 = ADVANCED_FACE ( 'NONE', ( #108377 ), #15942, .F. ) ;
#15865 = CARTESIAN_POINT ( 'NONE',  ( -13.92686555291570194, 1517.051704405520013, 226.1812314194930025 ) ) ;
#15867 = CARTESIAN_POINT ( 'NONE',  ( 14.45750538832999865, 1416.828039266780024, 196.8520486936070029 ) ) ;
#15868 = CARTESIAN_POINT ( 'NONE',  ( 11.57344360939999994, 1432.104224190049990, 151.1935562510979878 ) ) ;
#15869 = CARTESIAN_POINT ( 'NONE',  ( 8.342231075979542609, 1509.204540318783074, 181.0076993523580313 ) ) ;
#15870 = EDGE_LOOP ( 'NONE', ( #87541, #13318, #68405, #100643 ) ) ;
#15871 = CARTESIAN_POINT ( 'NONE',  ( 13.22834362140159925, 1435.940882500919997, 150.6028531436949720 ) ) ;
#15872 = ORIENTED_EDGE ( 'NONE', *, *, #70919, .F. ) ;
#15873 = EDGE_CURVE ( 'NONE', #79125, #9730, #90121, .T. ) ;
#15874 = ORIENTED_EDGE ( 'NONE', *, *, #78050, .F. ) ;
#15875 = CARTESIAN_POINT ( 'NONE',  ( 13.18758814857034167, 1444.720776282646966, 169.3929990596218431 ) ) ;
#15876 = CARTESIAN_POINT ( 'NONE',  ( -12.55989168380000187, 1462.260622135130006, 231.0244227316980243 ) ) ;
#15877 = CARTESIAN_POINT ( 'NONE',  ( -106.6554729947317526, 1390.652008648487936, 308.2807419479074724 ) ) ;
#15878 = CARTESIAN_POINT ( 'NONE',  ( 5.780232077335000440, 1516.760434454289907, 216.4486414936069991 ) ) ;
#15879 = CARTESIAN_POINT ( 'NONE',  ( -6.945821722360000727, 1473.074358042890026, 208.3699044046250037 ) ) ;
#15880 = B_SPLINE_SURFACE_WITH_KNOTS ( 'NONE', 5, 5, ( 
 ( #99355, #75301, #91532, #107224, #40019, #64703, #48996, #99912, #65790 ),
 ( #109444, #74198, #83129, #98268, #21539, #98820, #22082, #90968, #31613 ),
 ( #57407, #13689, #6426, #40571, #5317, #74742, #32173, #56278, #47874 ),
 ( #82012, #66357, #100476, #23758, #50095, #16986, #42235, #103215, #76947 ),
 ( #68557, #85315, #84767, #42787, #41680, #85885, #9188, #256, #33818 ),
 ( #101555, #16441, #75840, #59050, #92618, #110532, #8610, #102656, #51186 ),
 ( #34383, #15895, #109989, #58491, #25400, #67455, #84222, #68011, #34927 ),
 ( #77498, #59593, #8065, #43350, #94272, #33266, #7522, #76383, #25956 ),
 ( #24847, #93171, #17548, #60151, #93709, #51750, #798, #102121, #50637 ) ),
 .UNSPECIFIED., .F., .F., .F.,
 ( 6, 3, 6 ),
 ( 6, 3, 6 ),
 ( 3.580107477800000382, 6.558749095639999638, 9.700153431669999549 ),
 ( 0.000000000000000000, 0.5000000000000000000, 1.000000000000000000 ),
 .UNSPECIFIED. ) ;
#15881 = VECTOR ( 'NONE', #100076, 1000.000000000000000 ) ;
#15882 = EDGE_CURVE ( 'NONE', #99683, #26950, #94087, .T. ) ;
#15883 = ORIENTED_EDGE ( 'NONE', *, *, #22127, .F. ) ;
#15884 = CARTESIAN_POINT ( 'NONE',  ( -11.93513138720000022, 1502.470134631589872, 208.6121448500909992 ) ) ;
#15885 = CARTESIAN_POINT ( 'NONE',  ( 13.85929416875070075, 1410.325639211550197, 191.1496550842730073 ) ) ;
#15886 = CARTESIAN_POINT ( 'NONE',  ( -19.31603552179999994, 1379.367063215299822, 208.2524156231729933 ) ) ;
#15887 = AXIS2_PLACEMENT_3D ( 'NONE', #57011, #37992, #40186 ) ;
#15888 = B_SPLINE_CURVE_WITH_KNOTS ( 'NONE', 3,
 ( #89016, #97961, #2841, #72790, #3945, #96330, #36965, #19608, #12308, #71156, #97426, #105279, #62770, #11767 ),
 .UNSPECIFIED., .F., .F.,
 ( 4, 2, 2, 2, 2, 2, 4 ),
 ( 0.000000000000000000, 0.1249999999999999445, 0.2499999999999998890, 0.3749999999999998335, 0.4999999999999997780, 0.7499999999999998890, 1.000000000000000000 ),
 .UNSPECIFIED. ) ;
#15889 = ORIENTED_EDGE ( 'NONE', *, *, #60493, .F. ) ;
#15890 = CARTESIAN_POINT ( 'NONE',  ( 3.253462060665000433, 1516.874084700499907, 205.6604858388269861 ) ) ;
#15891 = VERTEX_POINT ( 'NONE', #83720 ) ;
#15892 = CARTESIAN_POINT ( 'NONE',  ( 3.267039691854999983, 1517.012231669750008, 209.8574146130079896 ) ) ;
#15893 = CARTESIAN_POINT ( 'NONE',  ( -18.85941459980000445, 1507.948893464629919, 229.7112672258979842 ) ) ;
#15894 = CARTESIAN_POINT ( 'NONE',  ( -12.27459264500000025, 1410.274824613030205, 189.3792765279980017 ) ) ;
#15895 = CARTESIAN_POINT ( 'NONE',  ( 7.942826972685000264, 1514.298059036119867, 215.9745877768969819 ) ) ;
#15897 = ORIENTED_EDGE ( 'NONE', *, *, #107452, .T. ) ;
#15896 = CARTESIAN_POINT ( 'NONE',  ( -0.5259141656838780543, 1414.913057855109855, 225.6201700896280045 ) ) ;
#15898 = CARTESIAN_POINT ( 'NONE',  ( 24.55711019350000157, 1439.571810943109995, 212.6863966501479979 ) ) ;
#15899 = CARTESIAN_POINT ( 'NONE',  ( 21.60894078575200439, 1519.551704408389924, 218.5714488936601470 ) ) ;
#15900 = CARTESIAN_POINT ( 'NONE',  ( -109.9987472819999965, 1384.028067710840105, 311.1749645552590096 ) ) ;
#15901 = CARTESIAN_POINT ( 'NONE',  ( 0.003700947952980240298, 1466.041018871260121, 235.8553854568179986 ) ) ;
#15902 = AXIS2_PLACEMENT_3D ( 'NONE', #79538, #87385, #54891 ) ;
#15903 = CARTESIAN_POINT ( 'NONE',  ( 7.320732157969690235, 1410.234431376039993, 270.0738234895199525 ) ) ;
#15904 = CARTESIAN_POINT ( 'NONE',  ( 5.784008635194999748, 1516.911981270829983, 214.1231845985469988 ) ) ;
#15905 = CARTESIAN_POINT ( 'NONE',  ( 24.11306831329999767, 1410.846617931330002, 209.3308953604909846 ) ) ;
#15906 = EDGE_CURVE ( 'NONE', #109266, #94371, #68743, .T. ) ;
#15907 = CARTESIAN_POINT ( 'NONE',  ( 24.07913373210075747, 1410.980207854583796, 209.6302519821946930 ) ) ;
#15908 = CARTESIAN_POINT ( 'NONE',  ( 2.901791247649999850, 1441.419505434789926, 218.6084270491589905 ) ) ;
#15909 = CARTESIAN_POINT ( 'NONE',  ( -7.721740324595189442, 1517.019662593890189, 208.8141823649340267 ) ) ;
#15910 = CARTESIAN_POINT ( 'NONE',  ( 1.136814033864999907, 1516.854133554269993, 211.4058994415870245 ) ) ;
#15912 = EDGE_CURVE ( 'NONE', #67505, #32529, #303, .T. ) ;
#15911 = CARTESIAN_POINT ( 'NONE',  ( -2.552678418909050340, 1448.464024222542548, 154.6753740974435232 ) ) ;
#15913 = CARTESIAN_POINT ( 'NONE',  ( 17.19739463999625784, 1525.960063244516959, 181.9833109756548595 ) ) ;
#15914 = DIRECTION ( 'NONE',  ( -1.000000000000000000, 0.000000000000000000, 0.000000000000000000 ) ) ;
#15916 = ORIENTED_EDGE ( 'NONE', *, *, #9200, .T. ) ;
#15915 = CARTESIAN_POINT ( 'NONE',  ( -61.45349693709999883, 1390.736557064060207, 266.8826925622589670 ) ) ;
#15917 = CARTESIAN_POINT ( 'NONE',  ( -40.39009907441349867, 1385.179773408669917, 242.7937635241629835 ) ) ;
#15918 = CARTESIAN_POINT ( 'NONE',  ( 6.814843616780000168, 1474.725755692929852, 264.8987716706979541 ) ) ;
#15919 = CARTESIAN_POINT ( 'NONE',  ( -5.563540966273840205, 1516.551188145990182, 218.9354434241149931 ) ) ;
#15920 = CARTESIAN_POINT ( 'NONE',  ( -2.443421232577144497, 1495.151577762832858, 220.0241338615849145 ) ) ;
#15921 = CARTESIAN_POINT ( 'NONE',  ( 6.260663917511189780, 1483.739111220829955, 218.7790172297789866 ) ) ;
#15922 = CARTESIAN_POINT ( 'NONE',  ( 11.82607906839999856, 1426.795487707440088, 206.5339109993589943 ) ) ;
#15923 = CARTESIAN_POINT ( 'NONE',  ( -0.3488295727624319831, 1444.725433255539201, 218.0942056312121622 ) ) ;
#15924 = EDGE_CURVE ( 'NONE', #69928, #61329, #82529, .T. ) ;
#15926 = CARTESIAN_POINT ( 'NONE',  ( -7.769235965580000070, 1384.905329033560065, 218.9178834839189847 ) ) ;
#15925 = CARTESIAN_POINT ( 'NONE',  ( 0.01010282929720150019, 1516.939452820819952, 216.8414868732370167 ) ) ;
#15927 = CARTESIAN_POINT ( 'NONE',  ( -9.560134974813159658, 1448.417707445359838, 209.4104641123290094 ) ) ;
#15928 = CARTESIAN_POINT ( 'NONE',  ( 10.75213062065016345, 1424.456471968840106, 137.8384151154668018 ) ) ;
#15929 = ORIENTED_EDGE ( 'NONE', *, *, #42540, .T. ) ;
#15930 = CARTESIAN_POINT ( 'NONE',  ( -0.7543882209519990889, 1516.727502608469877, 202.5709757879969857 ) ) ;
#15931 = CARTESIAN_POINT ( 'NONE',  ( 5.775165619278840978, 1509.036904577107407, 216.6345513647272298 ) ) ;
#15932 = AXIS2_PLACEMENT_3D ( 'NONE', #76388, #94848, #33825 ) ;
#15933 = CARTESIAN_POINT ( 'NONE',  ( 12.80114668729999927, 1422.763074512629828, 223.5079147161980018 ) ) ;
#15934 = CARTESIAN_POINT ( 'NONE',  ( -31.50799703744286262, 1524.382868172863937, 216.4233194664829796 ) ) ;
#15935 = CARTESIAN_POINT ( 'NONE',  ( -8.959719548958744895, 1461.371917847066470, 205.3598266504384355 ) ) ;
#15936 = CARTESIAN_POINT ( 'NONE',  ( 4.513979691470000333, 1467.746749492790059, 218.0203306744990357 ) ) ;
#15937 = CARTESIAN_POINT ( 'NONE',  ( 0.000000000000000000, 1408.913060387329779, 226.8598803041980148 ) ) ;
#15939 = B_SPLINE_CURVE_WITH_KNOTS ( 'NONE', 3,
 ( #30769, #64948, #99062, #22341, #56541, #6115, #13953, #5579, #39729, #73895, #108021, #31318, #65501, #22894, #48699, #74456, #11517, #94962, #26639, #2586, #36710, #27206, #61389, #45692, #43465, #103908, #96623, #28869, #79277, #95508, #18779, #77611, #52977, #922, #28313, #79831, #78151, #18230, #35045, #104459, #105020, #27752, #9300, #10398, #70903, #105582, #3137, #9847, #37271, #62504, #19334, #61945 ),
 .UNSPECIFIED., .F., .F.,
 ( 4, 3, 3, 3, 3, 3, 3, 3, 3, 3, 3, 3, 3, 3, 3, 3, 3, 4 ),
 ( -13.54897587289999983, -13.17531786724759968, -12.47907539720000081, -12.15554221928960033, -11.39789929992029904, -10.56585940365520138, -9.637960392618930783, -8.269156193220000617, -7.517475011647490213, -6.592826046528001527, -5.699782786179998340, -5.491406205670669394, -4.662291499253420568, -3.881037718147339888, -3.127721678440000375, -2.865801632923298925, -2.150110822952852274, -1.461586381269999180 ),
 .UNSPECIFIED. ) ;
#15938 = CARTESIAN_POINT ( 'NONE',  ( 27.07064927763860140, 1436.337874274649948, 136.7243984374310060 ) ) ;
#15940 = CIRCLE ( 'NONE', #107162, 0.4999999999999449329 ) ;
#15941 = ADVANCED_FACE ( 'NONE', ( #95441 ), #63230, .F. ) ;
#15942 = CYLINDRICAL_SURFACE ( 'NONE', #109317, 2.000000000000003553 ) ;
#15943 = CARTESIAN_POINT ( 'NONE',  ( -23.63778291159999867, 1435.985561032100122, 212.2556568964579924 ) ) ;
#15944 = CARTESIAN_POINT ( 'NONE',  ( -41.97830496582596282, 1454.330232234711730, 269.0763006382472895 ) ) ;
#15945 = CARTESIAN_POINT ( 'NONE',  ( -108.6385992050000056, 1386.360677242800193, 297.3882613995589850 ) ) ;
#15946 = CARTESIAN_POINT ( 'NONE',  ( 12.20572978030000044, 1508.837378189130050, 184.1963009972980103 ) ) ;
#15947 = CARTESIAN_POINT ( 'NONE',  ( 4.792731738917410667, 1506.992693111409835, 219.7839786367459851 ) ) ;
#15948 = CARTESIAN_POINT ( 'NONE',  ( -37.97313029066103240, 1453.984394254719291, 269.5760461896424545 ) ) ;
#15949 = ORIENTED_EDGE ( 'NONE', *, *, #56328, .F. ) ;
#15951 = EDGE_CURVE ( 'NONE', #32742, #44146, #37986, .T. ) ;
#15950 = DIRECTION ( 'NONE',  ( -0.9455185755993178454, 0.000000000000000000, 0.3255681544571537578 ) ) ;
#15952 = CARTESIAN_POINT ( 'NONE',  ( -29.77764972417399747, 1414.913285559889800, 269.3620624046142780 ) ) ;
#15953 = CARTESIAN_POINT ( 'NONE',  ( -4.987078467651929969, 1508.551704408389924, 212.6094300751769879 ) ) ;
#15954 = CARTESIAN_POINT ( 'NONE',  ( 14.38095606289810036, 1427.056691244839840, 190.6162741030670134 ) ) ;
#15955 = LINE ( 'NONE', #22144, #109014 ) ;
#15956 = CARTESIAN_POINT ( 'NONE',  ( 24.24036431055581886, 1452.066555927197214, 137.1576988608119336 ) ) ;
#15957 = CARTESIAN_POINT ( 'NONE',  ( -13.62888597016050163, 1517.051704413129983, 226.2994540733420195 ) ) ;
#15958 = CARTESIAN_POINT ( 'NONE',  ( -4.261662193653090291, 1515.372228416479857, 211.4517523182709908 ) ) ;
#15959 = CARTESIAN_POINT ( 'NONE',  ( -1.186412362116890051, 1486.884137111580230, 199.7737105367970116 ) ) ;
#15960 = CARTESIAN_POINT ( 'NONE',  ( -7.862669792100661859, 1451.394032558670915, 152.9856753053126965 ) ) ;
#15961 = VECTOR ( 'NONE', #78246, 1000.000000000000000 ) ;
#15962 = CARTESIAN_POINT ( 'NONE',  ( -18.02416168173120070, 1416.221314539589912, 209.1763259735849942 ) ) ;
#15963 = CARTESIAN_POINT ( 'NONE',  ( 24.06727922369999817, 1435.337950089560081, 136.6674132985980066 ) ) ;
#15964 = EDGE_CURVE ( 'NONE', #89576, #31839, #75067, .T. ) ;
#15965 = CARTESIAN_POINT ( 'NONE',  ( -13.13272715366738908, 1443.052901350239608, 169.4010147687362178 ) ) ;
#15966 = ORIENTED_EDGE ( 'NONE', *, *, #60370, .T. ) ;
#15967 = CARTESIAN_POINT ( 'NONE',  ( 0.7266101759286229811, 1414.971717244350202, 192.1881877811019876 ) ) ;
#15968 = EDGE_CURVE ( 'NONE', #66900, #90799, #79758, .T. ) ;
#15969 = CARTESIAN_POINT ( 'NONE',  ( -0.2331143941452460122, 1408.921200921389982, 231.7611568498559791 ) ) ;
#15970 = ORIENTED_EDGE ( 'NONE', *, *, #31807, .F. ) ;
#15971 = VERTEX_POINT ( 'NONE', #56604 ) ;
#15972 = CARTESIAN_POINT ( 'NONE',  ( 17.48265144437409901, 1415.426207913209964, 208.8075662200119780 ) ) ;
#15973 = DIRECTION ( 'NONE',  ( -0.6736849260863841948, 0.000000000000000000, 0.7390186874254148774 ) ) ;
#15975 = CARTESIAN_POINT ( 'NONE',  ( -24.58004528950000278, 1449.381385745619809, 225.2788513490980051 ) ) ;
#15974 = CARTESIAN_POINT ( 'NONE',  ( 41.23894881901300380, 1434.940505294187687, 269.6330775959622201 ) ) ;
#15976 = CARTESIAN_POINT ( 'NONE',  ( -20.23498361140000057, 1507.901949647030051, 189.1924027903980061 ) ) ;
#15977 = CARTESIAN_POINT ( 'NONE',  ( -11.08092061109999982, 1433.166019614319794, 151.6958383069980130 ) ) ;
#15978 = EDGE_CURVE ( 'NONE', #68958, #54399, #44516, .T. ) ;
#15979 = CARTESIAN_POINT ( 'NONE',  ( -16.14609365299999766, 1380.312263807889849, 210.2238755387789979 ) ) ;
#15980 = CARTESIAN_POINT ( 'NONE',  ( -2.774956468634210083, 1419.962269928060323, 186.1082814807396630 ) ) ;
#15981 = CARTESIAN_POINT ( 'NONE',  ( 7.486774210370000127, 1423.123604678139827, 213.9129862981389749 ) ) ;
#15982 = CARTESIAN_POINT ( 'NONE',  ( -24.40197519060000175, 1440.339844854569947, 212.0083896061380244 ) ) ;
#15983 = FACE_BOUND ( 'NONE', #108999, .T. ) ;
#15984 = CARTESIAN_POINT ( 'NONE',  ( -2.935740620858350081, 1409.954266029739983, 186.6342734442710025 ) ) ;
#15985 = CARTESIAN_POINT ( 'NONE',  ( 7.523183757958989304, 1364.306666347853707, 209.6218459617148824 ) ) ;
#15986 = ADVANCED_FACE ( 'NONE', ( #73409 ), #28792, .F. ) ;
#15987 = CARTESIAN_POINT ( 'NONE',  ( -20.87684431077013159, 1509.759617029159699, 230.6676771160481394 ) ) ;
#15989 = VERTEX_POINT ( 'NONE', #20365 ) ;
#15988 = LINE ( 'NONE', #41761, #42570 ) ;
#15990 = VERTEX_POINT ( 'NONE', #66129 ) ;
#15991 = CARTESIAN_POINT ( 'NONE',  ( -11.79841937739680091, 1428.159348747910144, 148.1013020209979913 ) ) ;
#15992 = CARTESIAN_POINT ( 'NONE',  ( -21.56347740270249957, 1506.734670034049941, 209.3230842351990191 ) ) ;
#15993 = CARTESIAN_POINT ( 'NONE',  ( -6.470863364639999560, 1473.558147035430238, 270.2848116644980223 ) ) ;
#15994 = CARTESIAN_POINT ( 'NONE',  ( 13.18025012471355240, 1434.856279462562952, 146.8601961898365005 ) ) ;
#15995 = CARTESIAN_POINT ( 'NONE',  ( -119.6058480740469463, 1348.229899472570878, 302.6372327872264236 ) ) ;
#15996 = VECTOR ( 'NONE', #75789, 1000.000000000000227 ) ;
#15997 = FACE_OUTER_BOUND ( 'NONE', #16008, .T. ) ;
#15998 = CARTESIAN_POINT ( 'NONE',  ( -8.164317912589998727, 1384.513847593510036, 199.6670242607489740 ) ) ;
#15999 = CARTESIAN_POINT ( 'NONE',  ( -11.83466398015730725, 1517.051704408389924, 228.0588040460849015 ) ) ;
#16000 = CARTESIAN_POINT ( 'NONE',  ( -18.82191891289999930, 1431.113060387329824, 204.7612636155780024 ) ) ;
#16001 = CARTESIAN_POINT ( 'NONE',  ( 9.532517564019999057, 1366.286862064870093, 207.6218459616989946 ) ) ;
#16002 = CARTESIAN_POINT ( 'NONE',  ( -9.559179497712129603, 1447.160234701620084, 211.6757039224950177 ) ) ;
#16003 = CARTESIAN_POINT ( 'NONE',  ( -8.335204523141790389, 1406.805845115979992, 269.2693966864819686 ) ) ;
#16004 = CARTESIAN_POINT ( 'NONE',  ( -13.66554182117469907, 1436.203183890759874, 150.4225340564210001 ) ) ;
#16005 = ORIENTED_EDGE ( 'NONE', *, *, #104995, .F. ) ;
#16006 = CARTESIAN_POINT ( 'NONE',  ( 2.404980717409123336, 1525.211477436245787, 242.0950474068928884 ) ) ;
#16007 = ADVANCED_FACE ( 'NONE', ( #90740 ), #77419, .T. ) ;
#16008 = EDGE_LOOP ( 'NONE', ( #60789, #45996, #45820, #103863, #30593 ) ) ;
#16009 = ORIENTED_EDGE ( 'NONE', *, *, #25237, .F. ) ;
#16010 = CARTESIAN_POINT ( 'NONE',  ( 7.812463224191407818, 1516.551704356460050, 206.2591310155938515 ) ) ;
#16011 = DIRECTION ( 'NONE',  ( 0.9455185755993178454, 0.000000000000000000, -0.3255681544571537578 ) ) ;
#16012 = ADVANCED_FACE ( 'NONE', ( #57173 ), #20251, .T. ) ;
#16014 =( NAMED_UNIT ( * ) PLANE_ANGLE_UNIT ( ) SI_UNIT ( $, .RADIAN. ) );
#16013 = CARTESIAN_POINT ( 'NONE',  ( 2.491188358395000080, 1516.733363207009916, 213.1488973760370129 ) ) ;
#16015 = CARTESIAN_POINT ( 'NONE',  ( -18.30299290700000014, 1485.488320381530002, 189.0823417877979864 ) ) ;
#16016 = B_SPLINE_SURFACE_WITH_KNOTS ( 'NONE', 5, 5, ( 
 ( #69425, #41993, #101306, #110831, #103538, #16204 ),
 ( #76688, #43098, #60462, #77801, #102429, #50951 ),
 ( #58249, #51493, #17298, #92372, #76142, #75610 ),
 ( #109740, #49850, #85624, #77259, #83982, #558 ),
 ( #7281, #41445, #92933, #101868, #25160, #93474 ),
 ( #2225, #62693, #78919, #46426, #88944, #53163 ),
 ( #54819, #79461, #28498, #87305, #37451, #88403 ),
 ( #27388, #97346, #71651, #104097, #95151, #36339 ),
 ( #105770, #20617, #18968, #2772, #3874, #11162 ) ),
 .UNSPECIFIED., .F., .F., .F.,
 ( 6, 3, 6 ),
 ( 6, 6 ),
 ( 2.990692062960830011, 5.133895727739999693, 7.277090745855540277 ),
 ( -0.0004094007421257130183, 2.000000000000000000 ),
 .UNSPECIFIED. ) ;
#16017 = EDGE_LOOP ( 'NONE', ( #50211, #81905, #71994, #108858 ) ) ;
#16018 = CARTESIAN_POINT ( 'NONE',  ( -113.4000000000000057, 1379.105522877179965, 302.6503168488589495 ) ) ;
#16019 =( BOUNDED_CURVE ( )  B_SPLINE_CURVE ( 3, ( #103112, #95833, #77932, #94727 ),
 .UNSPECIFIED., .F., .F. ) 
 B_SPLINE_CURVE_WITH_KNOTS ( ( 4, 4 ),
 ( 1.800053338152554971, 2.115542295163019837 ),
 .UNSPECIFIED. ) 
 CURVE ( )  GEOMETRIC_REPRESENTATION_ITEM ( )  RATIONAL_B_SPLINE_CURVE ( ( 1.000000000000000000, 0.9917227450084913354, 0.9917227450084913354, 1.000000000000000000 ) ) 
 REPRESENTATION_ITEM ( '' )  );
#16020 = CARTESIAN_POINT ( 'NONE',  ( 1.708102589285000139, 1517.199196846569976, 202.5572672468869939 ) ) ;
#16021 = AXIS2_PLACEMENT_3D ( 'NONE', #29353, #73029, #13087 ) ;
#16022 = B_SPLINE_SURFACE_WITH_KNOTS ( 'NONE', 5, 5, ( 
 ( #56293, #73659, #13700, #5328, #74754, #107791 ),
 ( #108891, #32184, #99368, #48458, #23217, #66368 ),
 ( #57955, #57417, #22641, #56847, #14267, #74214 ),
 ( #91543, #14820, #92088, #15365, #8075, #16451 ),
 ( #101023, #102132, #94283, #75849, #43363, #9740 ),
 ( #102667, #101570, #59603, #50107, #93720, #77510 ),
 ( #109999, #17560, #51762, #34937, #34394, #68569 ),
 ( #42799, #50648, #33276, #52327, #76959, #110545 ),
 ( #18129, #69124, #33833, #43906, #109455, #85896 ) ),
 .UNSPECIFIED., .F., .F., .F.,
 ( 6, 3, 6 ),
 ( 6, 6 ),
 ( 6.548035129179999636, 9.290526163740000953, 11.10277561180000028 ),
 ( 0.000000000000000000, 2.000000000000000000 ),
 .UNSPECIFIED. ) ;
#16023 = CARTESIAN_POINT ( 'NONE',  ( 1.455000209906389896, 1507.073729425429974, 236.7651043255590082 ) ) ;
#16024 = CARTESIAN_POINT ( 'NONE',  ( -37.07348200565930085, 1384.574303191529907, 210.3284201765650039 ) ) ;
#16025 = CARTESIAN_POINT ( 'NONE',  ( -14.52363634152899863, 1379.696035566400042, 208.2603442536380101 ) ) ;
#16026 = CARTESIAN_POINT ( 'NONE',  ( 11.13973214860000027, 1470.272411968090182, 206.9146623037889867 ) ) ;
#16027 = AXIS2_PLACEMENT_3D ( 'NONE', #24105, #6766, #5120 ) ;
#16029 = ORIENTED_EDGE ( 'NONE', *, *, #91939, .F. ) ;
#16028 = CARTESIAN_POINT ( 'NONE',  ( 31.32995031131189378, 1523.678648413191695, 196.3423562208913324 ) ) ;
#16030 = CARTESIAN_POINT ( 'NONE',  ( -25.82127556856010031, 1449.911323258540051, 209.1126152976609944 ) ) ;
#16031 = CARTESIAN_POINT ( 'NONE',  ( 28.24200347700000080, 1508.135538548330260, 209.4469796410679976 ) ) ;
#16032 = CARTESIAN_POINT ( 'NONE',  ( -28.62766089293190674, 1526.344110814220357, 220.1997210291906129 ) ) ;
#16033 = CARTESIAN_POINT ( 'NONE',  ( -6.954065720117950100, 1521.551704408389924, 183.5505540514350002 ) ) ;
#16034 = CARTESIAN_POINT ( 'NONE',  ( -13.21274905972310165, 1436.080685154540106, 150.6465363514350031 ) ) ;
#16035 = CARTESIAN_POINT ( 'NONE',  ( -24.40357955099999998, 1441.574771106910021, 212.0768376842780185 ) ) ;
#16037 = CARTESIAN_POINT ( 'NONE',  ( -7.321193745875000047, 1516.534976163889951, 211.4135222436570132 ) ) ;
#16036 = CIRCLE ( 'NONE', #94795, 1.000000000000000888 ) ;
#16038 = CARTESIAN_POINT ( 'NONE',  ( -68.45900093969999034, 1379.747219870859908, 279.4339011000590176 ) ) ;
#16039 = DIRECTION ( 'NONE',  ( 0.000000000000000000, 0.000000000000000000, 1.000000000000000000 ) ) ;
#16040 = CARTESIAN_POINT ( 'NONE',  ( -14.29468279409999987, 1410.759725306329983, 226.8458938957979854 ) ) ;
#16041 = CARTESIAN_POINT ( 'NONE',  ( 3.711480272509555256, 1440.856594891422901, 156.5043989337177379 ) ) ;
#16042 = CARTESIAN_POINT ( 'NONE',  ( 3.251611325815000342, 1516.779243033999819, 206.8234764622770001 ) ) ;
#16043 = ORIENTED_EDGE ( 'NONE', *, *, #78924, .T. ) ;
#16044 = CARTESIAN_POINT ( 'NONE',  ( -2.155272317154649730, 1451.949265150150040, 184.4961430247039971 ) ) ;
#16045 = CARTESIAN_POINT ( 'NONE',  ( -10.07108938579999879, 1472.689539964090045, 207.5339997831590040 ) ) ;
#16046 = CARTESIAN_POINT ( 'NONE',  ( -20.87663001988034139, 1455.029843775830841, 223.4912394292003341 ) ) ;
#16047 = EDGE_LOOP ( 'NONE', ( #107356, #28800, #21253 ) ) ;
#16048 = CARTESIAN_POINT ( 'NONE',  ( -3.300164695495766853, 1524.538768545233779, 241.8639374637165815 ) ) ;
#16049 = CARTESIAN_POINT ( 'NONE',  ( 12.76237656848210023, 1434.657230989279924, 149.5328040805229932 ) ) ;
#16050 = CARTESIAN_POINT ( 'NONE',  ( -4.170414335751749135, 1441.567394449320091, 183.8415942696151433 ) ) ;
#16051 = CARTESIAN_POINT ( 'NONE',  ( -17.60447252379999838, 1417.354189540510106, 207.6029927142990061 ) ) ;
#16052 = CARTESIAN_POINT ( 'NONE',  ( 24.77519968700000064, 1452.047894330230065, 135.6623939816980169 ) ) ;
#16053 = CARTESIAN_POINT ( 'NONE',  ( 4.414384251610000476, 1487.467097172089780, 197.9737507085990273 ) ) ;
#16054 = CARTESIAN_POINT ( 'NONE',  ( 1.729065141746580103, 1431.231418718420173, 218.4534901915430112 ) ) ;
#16055 = CARTESIAN_POINT ( 'NONE',  ( 4.221769150835829265, 1441.602571462190099, 168.1843695343990248 ) ) ;
#16056 = AXIS2_PLACEMENT_3D ( 'NONE', #85343, #8639, #6997 ) ;
#16058 = CARTESIAN_POINT ( 'NONE',  ( 36.40062690906153620, 1436.005110274238632, 135.0217588575150955 ) ) ;
#16057 = CARTESIAN_POINT ( 'NONE',  ( 2.296124850935000072, 1516.677239312369920, 213.7299927514870319 ) ) ;
#16059 = CARTESIAN_POINT ( 'NONE',  ( -8.873656775930450991, 1385.220332894750072, 218.6703658329330153 ) ) ;
#16060 = CARTESIAN_POINT ( 'NONE',  ( 0.7538707352880020807, 1516.719999691880048, 216.0603247549969979 ) ) ;
#16061 = ORIENTED_EDGE ( 'NONE', *, *, #10083, .T. ) ;
#16062 = CARTESIAN_POINT ( 'NONE',  ( -18.25588481898620330, 1498.276152301830052, 229.4258147717129930 ) ) ;
#16063 = CARTESIAN_POINT ( 'NONE',  ( -16.98381430819999949, 1420.348059816200021, 203.5840860547189948 ) ) ;
#16064 = CARTESIAN_POINT ( 'NONE',  ( 0.9538458998259999877, 1420.753719637230006, 182.9132178711979861 ) ) ;
#16065 = CARTESIAN_POINT ( 'NONE',  ( -2.155783482819999985, 1476.003253452089893, 220.3848946179990094 ) ) ;
#16066 = DIRECTION ( 'NONE',  ( 1.000000000000000000, 0.000000000000000000, 0.000000000000000000 ) ) ;
#16067 = CARTESIAN_POINT ( 'NONE',  ( -1232.316865285500171, 2833.596074015639715, -9639.481875266528732 ) ) ;
#16068 = CARTESIAN_POINT ( 'NONE',  ( -11.37853563926020151, 1470.969474876900222, 208.2620529163870060 ) ) ;
#16069 = CARTESIAN_POINT ( 'NONE',  ( -4.336924793510721798, 1508.178691706793870, 220.5928148824004040 ) ) ;
#16070 = AXIS2_PLACEMENT_3D ( 'NONE', #37250, #78700, #2013 ) ;
#16071 = CARTESIAN_POINT ( 'NONE',  ( 17.43505318546112193, 1422.809578927221992, 226.5206943312184933 ) ) ;
#16072 = CARTESIAN_POINT ( 'NONE',  ( 18.25262555440377099, 1425.320047386311671, 224.8456491439040121 ) ) ;
#16073 = CARTESIAN_POINT ( 'NONE',  ( -7.435066116149999793, 1441.600846913620217, 149.7516446007980164 ) ) ;
#16074 = CARTESIAN_POINT ( 'NONE',  ( 17.17241001986506888, 1523.382868172864164, 237.6251415217915053 ) ) ;
#16076 = CARTESIAN_POINT ( 'NONE',  ( 4.328570061217780207, 1515.098349647940040, 207.9863157841529926 ) ) ;
#16075 = CARTESIAN_POINT ( 'NONE',  ( -2.022195510094900506, 1421.024483011140092, 193.8502759697570070 ) ) ;
#16077 = CARTESIAN_POINT ( 'NONE',  ( 13.12320631909999946, 1422.961664926129970, 221.9290738727979999 ) ) ;
#16078 = EDGE_LOOP ( 'NONE', ( #13804, #110006, #14237, #21390 ) ) ;
#16079 = ORIENTED_EDGE ( 'NONE', *, *, #3941, .T. ) ;
#16080 = CARTESIAN_POINT ( 'NONE',  ( 29.13504683812232798, 1526.073434386619056, 221.0961479590759495 ) ) ;
#16081 = DIRECTION ( 'NONE',  ( 0.6638413684297217454, -0.7475172610820757235, 0.02307773701440622716 ) ) ;
#16082 = CARTESIAN_POINT ( 'NONE',  ( -2.596261494520225366, 1525.907212628473644, 177.4701144822246874 ) ) ;
#16083 = CARTESIAN_POINT ( 'NONE',  ( 7.835586116740000051, 1423.724600923389971, 195.8439878601990074 ) ) ;
#16084 = CARTESIAN_POINT ( 'NONE',  ( -18.07041998555256868, 1523.313115944345100, 238.0891100728149183 ) ) ;
#16085 = CARTESIAN_POINT ( 'NONE',  ( 9.863053695384421005, 1422.516288235769935, 212.3150749887220172 ) ) ;
#16086 = CARTESIAN_POINT ( 'NONE',  ( -2.642143157096769723, 1488.503634608570110, 219.7172765930159812 ) ) ;
#16087 = CARTESIAN_POINT ( 'NONE',  ( -4.329448776040000446, 1515.064792882589927, 207.2788837304390199 ) ) ;
#16088 = CARTESIAN_POINT ( 'NONE',  ( -62.13084746230200039, 1383.793921180840016, 284.1282107610300045 ) ) ;
#16089 = CARTESIAN_POINT ( 'NONE',  ( 10.91400993090000071, 1451.290521646029902, 152.3073314843979915 ) ) ;
#16090 = CARTESIAN_POINT ( 'NONE',  ( 10.52942987710000011, 1470.684214315490181, 209.6684282404120268 ) ) ;
#16091 = CARTESIAN_POINT ( 'NONE',  ( 10.71868385741180063, 1491.403514958749838, 211.6561026201489994 ) ) ;
#16093 = EDGE_LOOP ( 'NONE', ( #60326, #78683, #47011, #27357, #68475 ) ) ;
#16092 = CARTESIAN_POINT ( 'NONE',  ( -2.406810632960000085, 1456.459620267289893, 218.3084222088889987 ) ) ;
#16094 = CARTESIAN_POINT ( 'NONE',  ( 34.68852446352944696, 1522.382868172863937, 218.2490599186007216 ) ) ;
#16095 = EDGE_CURVE ( 'NONE', #26746, #98016, #66178, .T. ) ;
#16096 = AXIS2_PLACEMENT_3D ( 'NONE', #30900, #109822, #67291 ) ;
#16097 = B_SPLINE_SURFACE_WITH_KNOTS ( 'NONE', 5, 5, ( 
 ( #67684, #72367, #64520, #6230, #65059, #47154, #65614, #110209, #50866 ),
 ( #99172, #22454, #47701, #14630, #5133, #23019, #57223, #101792, #16668 ),
 ( #63972, #91350, #48817, #21357, #38186, #82939, #84995, #29785, #55564 ),
 ( #89689, #81279, #4596, #38730, #72904, #107045, #30331, #21903, #95075 ),
 ( #27313, #1580, #43574, #18341, #76612, #87226, #35714, #69902, #60380 ),
 ( #44131, #36267, #78266, #51412, #61494, #86665, #68246, #52532, #18892 ),
 ( #85544, #95624, #104577, #9959, #1036, #42453, #77723, #35159, #86118 ),
 ( #110764, #104018, #78835, #17217, #10516, #53088, #34054, #60947, #94501 ),
 ( #44690, #2146, #69343, #102354, #9411, #70456, #27871, #62053, #103452 ),
 ( #26758, #96178, #19453, #25637, #59829, #93950, #8840, #17774, #8290 ),
 ( #43023, #77181, #53652, #484, #34607, #68793, #102893, #26192, #51976 ),
 ( #30059, #87796, #29515, #45247, #63706, #36822, #97272, #97816, #46355 ),
 ( #11080, #62623, #4335, #37378, #63170, #106768, #79934, #20546, #21095 ),
 ( #46903, #107329, #71012, #106230, #54750, #3251, #37935, #88880, #55298 ),
 ( #89972, #81026, #81560, #45801, #96740, #89429, #12165, #79384, #38466 ) ),
 .UNSPECIFIED., .F., .F., .F.,
 ( 6, 3, 3, 3, 6 ),
 ( 6, 3, 6 ),
 ( 20.95182776320000073, 25.72519398600000073, 33.50811105449999872, 41.29102812299999670, 53.47486354659999819 ),
 ( 0.000000000000000000, 1.000000000000000000, 2.000000000000000000 ),
 .UNSPECIFIED. ) ;
#16098 = CARTESIAN_POINT ( 'NONE',  ( -37.85704848470000172, 1380.929536399250082, 234.3704980780590006 ) ) ;
#16099 = ADVANCED_FACE ( 'NONE', ( #76697 ), #34145, .F. ) ;
#16100 = CARTESIAN_POINT ( 'NONE',  ( -16.97531057559999823, 1409.505851295029970, 223.7086794493979767 ) ) ;
#16101 = ORIENTED_EDGE ( 'NONE', *, *, #50292, .T. ) ;
#16102 = EDGE_LOOP ( 'NONE', ( #24915, #86046, #66509, #57107, #75335, #29282 ) ) ;
#16103 = CARTESIAN_POINT ( 'NONE',  ( -2.031883754679999932, 1464.998375783689880, 198.3053765207990011 ) ) ;
#16104 = CARTESIAN_POINT ( 'NONE',  ( 37.47794244721399792, 1438.218164175530092, 136.5783189908810016 ) ) ;
#16106 = CARTESIAN_POINT ( 'NONE',  ( 31.33756689035249110, 1523.580203803270933, 196.3415365178082368 ) ) ;
#16105 = CARTESIAN_POINT ( 'NONE',  ( -109.1112710710209939, 1384.400207420500237, 313.2414003153020303 ) ) ;
#16107 = B_SPLINE_CURVE_WITH_KNOTS ( 'NONE', 3,
 ( #6442, #110002, #40587, #110549, #84782, #67469, #33279, #41137, #65809, #49560, #23221, #50651, #74759, #102135, #24325, #57421, #84238, #16456, #92638 ),
 .UNSPECIFIED., .F., .F.,
 ( 4, 3, 3, 3, 3, 3, 4 ),
 ( -6.749361099460109870, -6.540428904467110449, -5.576190169441640698, -4.758631760330019667, -4.110056285970450141, -3.404977062924410269, -2.767901846390000031 ),
 .UNSPECIFIED. ) ;
#16108 = CARTESIAN_POINT ( 'NONE',  ( 11.74864212650039796, 1479.742741897189944, 210.0210730748829917 ) ) ;
#16109 = CARTESIAN_POINT ( 'NONE',  ( -108.0400389039999851, 1380.595742417440078, 298.4240030958590069 ) ) ;
#16110 = LINE ( 'NONE', #67113, #5256 ) ;
#16111 = CARTESIAN_POINT ( 'NONE',  ( -11.65606946387948462, 1435.045539906245040, 151.3529213300715242 ) ) ;
#16112 = CARTESIAN_POINT ( 'NONE',  ( 18.70459388984919968, 1509.566239199539950, 186.5372755781170042 ) ) ;
#16113 = CARTESIAN_POINT ( 'NONE',  ( 0.1274748778641759950, 1507.111760713879903, 180.9260797659750040 ) ) ;
#16114 = CARTESIAN_POINT ( 'NONE',  ( 1.431683340829999818, 1410.342262983229830, 185.2915050568979893 ) ) ;
#16115 = CARTESIAN_POINT ( 'NONE',  ( 1.716045945209999868, 1509.007693206030126, 179.5167849949980052 ) ) ;
#16116 = CARTESIAN_POINT ( 'NONE',  ( -11.86629850686009924, 1432.349867577580198, 149.9824227077560010 ) ) ;
#16117 = CARTESIAN_POINT ( 'NONE',  ( -3.691951647117269530, 1441.076583034890064, 158.1234524560840100 ) ) ;
#16118 = AXIS2_PLACEMENT_3D ( 'NONE', #37124, #86419, #53965 ) ;
#16119 = EDGE_CURVE ( 'NONE', #36240, #5765, #59564, .T. ) ;
#16120 = CARTESIAN_POINT ( 'NONE',  ( 11.76598824432590185, 1428.979787898590075, 145.3127963841559733 ) ) ;
#16121 = ORIENTED_EDGE ( 'NONE', *, *, #85697, .F. ) ;
#16122 = CARTESIAN_POINT ( 'NONE',  ( -19.72225066010199868, 1467.596931137250067, 204.3544451804700088 ) ) ;
#16123 = CARTESIAN_POINT ( 'NONE',  ( 16.87900699709421204, 1524.382868172804365, 237.0109764097478546 ) ) ;
#16124 = CARTESIAN_POINT ( 'NONE',  ( 18.99989700328560360, 1457.426100493899867, 226.6523199981070036 ) ) ;
#16125 = CARTESIAN_POINT ( 'NONE',  ( 16.53426867370000153, 1488.224675751930135, 188.8661511851979640 ) ) ;
#16126 = CARTESIAN_POINT ( 'NONE',  ( 2.330134126718832910, 1515.372048949687041, 213.3835825136068536 ) ) ;
#16127 = CARTESIAN_POINT ( 'NONE',  ( 20.52035477951934084, 1436.445808972336636, 144.8704347017549594 ) ) ;
#16128 = CARTESIAN_POINT ( 'NONE',  ( -1.969513130946940027, 1420.780713718789912, 193.8325181973079907 ) ) ;
#16129 = CARTESIAN_POINT ( 'NONE',  ( 1.616750372209999842, 1476.357240329989963, 198.1368238248990110 ) ) ;
#16130 = CARTESIAN_POINT ( 'NONE',  ( -108.2565521540000049, 1386.661487099380111, 310.8214570342590264 ) ) ;
#16131 = CARTESIAN_POINT ( 'NONE',  ( -7.558249345183369883, 1510.689985724130111, 214.8113843319750060 ) ) ;
#16132 = CARTESIAN_POINT ( 'NONE',  ( -8.910387285849060035, 1362.858511851213962, 210.6218459616991936 ) ) ;
#16133 = CARTESIAN_POINT ( 'NONE',  ( -46.05541984167459901, 1438.448880790329895, 266.9752125373910303 ) ) ;
#16134 = CARTESIAN_POINT ( 'NONE',  ( -2.695375846180000146, 1439.665988598389958, 184.6458907360980106 ) ) ;
#16135 = CARTESIAN_POINT ( 'NONE',  ( -8.112557822769998594, 1425.521057321509943, 208.4541235294330193 ) ) ;
#16136 = CARTESIAN_POINT ( 'NONE',  ( 7.332063939445000678, 1516.939491476980038, 209.1111146381379911 ) ) ;
#16137 = AXIS2_PLACEMENT_3D ( 'NONE', #65159, #98187, #107142 ) ;
#16138 = CARTESIAN_POINT ( 'NONE',  ( -13.72218023960000011, 1389.845687919130114, 205.4181164005090068 ) ) ;
#16139 = B_SPLINE_CURVE_WITH_KNOTS ( 'NONE', 3,
 ( #40210, #58679, #16625, #50821, #14987, #41322, #23401, #92814, #16085, #33441, #67640, #84952, #42412, #82765, #76566, #57036, #91163, #14438, #48635, #6057, #31806, #100115 ),
 .UNSPECIFIED., .F., .F.,
 ( 4, 3, 3, 3, 3, 3, 3, 4 ),
 ( -8.540286635490000222, -8.454071259740000954, -7.782260918187459353, -6.926036427371090376, -6.070163583882830061, -5.213710336174729676, -4.355629079344280008, -3.495541850680000451 ),
 .UNSPECIFIED. ) ;
#16140 = B_SPLINE_SURFACE_WITH_KNOTS ( 'NONE', 5, 5, ( 
 ( #5734, #14664, #23051, #99762, #6810, #65095 ),
 ( #39325, #75148, #32021, #66210, #65645, #32580 ),
 ( #91386, #82977, #73498, #98675, #6270, #21937 ),
 ( #81314, #66756, #100858, #24149, #74044, #108173 ),
 ( #47187, #58339, #30916, #4629, #38765, #47733 ),
 ( #31465, #58887, #17953, #93020, #42632, #16293 ),
 ( #49935, #101397, #85723, #69518, #1197, #35329 ),
 ( #59452, #93563, #25804, #51591, #109836, #7372 ),
 ( #26366, #41535, #67304, #84619, #67851, #75693 ) ),
 .UNSPECIFIED., .F., .F., .F.,
 ( 6, 3, 6 ),
 ( 6, 6 ),
 ( 106.4131865259999898, 113.5701753800000091, 117.7436754830000041 ),
 ( 0.000000000000000000, 1.000000014787439939 ),
 .UNSPECIFIED. ) ;
#16141 = ADVANCED_FACE ( 'NONE', ( #17308 ), #85635, .F. ) ;
#16142 = CARTESIAN_POINT ( 'NONE',  ( -8.147283189284854288, 1471.380150889464176, 215.1678129514797320 ) ) ;
#16143 = CARTESIAN_POINT ( 'NONE',  ( 7.295790646376310029, 1426.429901798619994, 212.8040195462420172 ) ) ;
#16144 = CARTESIAN_POINT ( 'NONE',  ( -27.02103266032270312, 1451.952429640200080, 135.1697984406160344 ) ) ;
#16145 = VERTEX_POINT ( 'NONE', #58803 ) ;
#16146 = CARTESIAN_POINT ( 'NONE',  ( 24.09667807370000148, 1426.479303835230212, 238.1639188848979813 ) ) ;
#16148 = DIRECTION ( 'NONE',  ( 0.2054769195713296581, -0.000000000000000000, 0.9786619618251632957 ) ) ;
#16147 = CARTESIAN_POINT ( 'NONE',  ( -2.136371660471462874, 1525.856064936157054, 176.8742965270300544 ) ) ;
#16149 = EDGE_CURVE ( 'NONE', #36359, #2313, #45920, .T. ) ;
#16150 = CARTESIAN_POINT ( 'NONE',  ( -3.350338079455601026, 1523.604703353109699, 176.1628856388066708 ) ) ;
#16151 = CARTESIAN_POINT ( 'NONE',  ( -3.625385342379999987, 1422.360590018430003, 211.7205299729980084 ) ) ;
#16152 = CARTESIAN_POINT ( 'NONE',  ( 13.45406242349999992, 1426.801272845689937, 196.6926870375990006 ) ) ;
#16153 = CARTESIAN_POINT ( 'NONE',  ( 29.22958591724099975, 1509.933780020319773, 206.4713313096740137 ) ) ;
#16154 = CARTESIAN_POINT ( 'NONE',  ( 4.952364187259999717, 1425.023410992210302, 209.4642470625779822 ) ) ;
#16155 = VERTEX_POINT ( 'NONE', #26851 ) ;
#16156 = CARTESIAN_POINT ( 'NONE',  ( 17.83486663330510424, 1523.678648413191695, 237.8759530894959084 ) ) ;
#16157 = CARTESIAN_POINT ( 'NONE',  ( 16.32987610974730330, 1422.497371498959865, 227.4665333559439944 ) ) ;
#16158 = CARTESIAN_POINT ( 'NONE',  ( 9.881164057279999469, 1462.277409695889901, 209.5389570254230023 ) ) ;
#16159 = ORIENTED_EDGE ( 'NONE', *, *, #32082, .F. ) ;
#16160 = ORIENTED_EDGE ( 'NONE', *, *, #70554, .T. ) ;
#16161 = CARTESIAN_POINT ( 'NONE',  ( -22.63974427064189854, 1409.703621529829888, 209.3606225731330142 ) ) ;
#16162 = ORIENTED_EDGE ( 'NONE', *, *, #45458, .T. ) ;
#16163 = CARTESIAN_POINT ( 'NONE',  ( -100.0318980807000031, 1325.797319984390015, 311.5248733202390099 ) ) ;
#16164 = CARTESIAN_POINT ( 'NONE',  ( -9.110233712619999480, 1428.462521060929930, 112.4493539157979995 ) ) ;
#16165 = CARTESIAN_POINT ( 'NONE',  ( -0.9772301425810001607, 1507.642725251929960, 237.2369517814979929 ) ) ;
#16166 = CARTESIAN_POINT ( 'NONE',  ( 3.224559923908230097, 1508.551704408090018, 213.9552828354289886 ) ) ;
#16167 = CARTESIAN_POINT ( 'NONE',  ( 46.23666873409530353, 1442.813199615530038, 267.5908865687479761 ) ) ;
#16168 = CARTESIAN_POINT ( 'NONE',  ( -11.22869580998730044, 1391.913060387200176, 206.6514090535289938 ) ) ;
#16169 = CARTESIAN_POINT ( 'NONE',  ( -15.97230738210199696, 1420.722887419069821, 227.0315163971459924 ) ) ;
#16170 = CARTESIAN_POINT ( 'NONE',  ( -5.785582951674999919, 1516.981965530290154, 205.0894480302270040 ) ) ;
#16171 = EDGE_LOOP ( 'NONE', ( #474, #41390 ) ) ;
#16172 = CARTESIAN_POINT ( 'NONE',  ( 19.00569199371070539, 1457.306189793003114, 226.5295724121195065 ) ) ;
#16173 = CARTESIAN_POINT ( 'NONE',  ( 14.81793322097859900, 1514.080593477140155, 194.2006236339620102 ) ) ;
#16174 = TOROIDAL_SURFACE ( 'NONE', #5418, 14.90133124319999780, 0.5000000000000000000 ) ;
#16175 = DIRECTION ( 'NONE',  ( 0.5969061220947440294, -0.8023110876747339137, 0.000000000000000000 ) ) ;
#16176 = ORIENTED_EDGE ( 'NONE', *, *, #70801, .F. ) ;
#16177 = CARTESIAN_POINT ( 'NONE',  ( -10.98190293991350153, 1481.156708494670283, 209.8541006977949905 ) ) ;
#16178 = CARTESIAN_POINT ( 'NONE',  ( 26.83111240151620080, 1451.219512166529967, 136.2764200117410098 ) ) ;
#16179 = B_SPLINE_SURFACE_WITH_KNOTS ( 'NONE', 5, 5, ( 
 ( #35870, #37514, #19597, #29113, #69492, #28005, #19032, #63299, #11228, #62193, #71148, #36404 ),
 ( #27451, #36951, #17928, #61634, #45929, #96320, #105271, #95765, #53233, #87375, #10669, #44835 ),
 ( #52126, #79529, #53800, #28563, #70596, #104711, #86253, #62761, #35305, #96878, #103614, #20147 ),
 ( #54344, #11759, #9544, #43714, #77865, #29656, #80623, #64390, #97953, #40262, #31307, #73883 ),
 ( #4474, #54884, #81159, #12298, #13386, #82813, #99051, #64937, #22330, #55980, #13942, #5568 ),
 ( #48132, #90103, #63842, #81698, #55432, #65490, #72783, #38603, #39719, #106369, #108011, #89563 ),
 ( #12853, #21223, #47573, #82270, #14499, #20687, #106910, #47034, #5005, #22883, #73326, #89009 ),
 ( #30198, #72242, #3937, #99600, #98510, #21778, #39152, #57093, #107461, #91218, #30756, #48689 ),
 ( #6106, #74445, #56531, #108571, #46490, #90659, #31860, #97417, #38065, #49238, #75545, #58731 ),
 ( #67146, #110780, #92868, #6661, #49786, #16146, #74993, #83361, #8857, #40814, #50350, #59304 ),
 ( #101807, #51430, #17236, #68264, #76627, #93969, #85560, #8308, #109681, #15583, #66603, #43040 ),
 ( #102371, #32957, #109142, #84475, #15038, #92312, #77197, #67698, #500, #32424, #76085, #101244 ),
 ( #93418, #110223, #42469, #7762, #34071, #83919, #50882, #66048, #7223, #100171, #33497, #85014 ),
 ( #41381, #100707, #24543, #58184, #25099, #23456, #16685, #25654, #59845, #23988, #41929, #57650 ),
 ( #91762, #13126, #18355, #94517, #106650, #35176, #87242, #69920, #87812, #18907, #53669, #89856 ) ),
 .UNSPECIFIED., .F., .F., .F.,
 ( 6, 3, 3, 3, 6 ),
 ( 6, 3, 3, 6 ),
 ( 1.933760083099999916, 17.84603210599999912, 29.17820978809999843, 40.51038747020000130, 62.31975385239999810 ),
 ( 253.0908261109999842, 295.2726304679999885, 316.3635326440000313, 337.4544348200000172 ),
 .UNSPECIFIED. ) ;
#16180 = CARTESIAN_POINT ( 'NONE',  ( -2.487935123020000194, 1508.551704408389924, 214.1089243778970115 ) ) ;
#16181 = CARTESIAN_POINT ( 'NONE',  ( 11.04300719229690131, 1502.511714738169985, 215.4559327082369862 ) ) ;
#16182 = CARTESIAN_POINT ( 'NONE',  ( 7.729057984899998957, 1421.712257409790027, 195.7954043856990154 ) ) ;
#16183 = CARTESIAN_POINT ( 'NONE',  ( 0.8539859765994233243, 1391.413060387289988, 208.6015499384857321 ) ) ;
#16184 = CARTESIAN_POINT ( 'NONE',  ( -5.445057622820000276, 1494.866989841090117, 198.0707108858990182 ) ) ;
#16185 = CARTESIAN_POINT ( 'NONE',  ( 10.21005717583030048, 1409.269603440459832, 190.4196895962099916 ) ) ;
#16187 = CARTESIAN_POINT ( 'NONE',  ( 28.27139721233048419, 1526.382868172863937, 219.5606225550385489 ) ) ;
#16186 = CARTESIAN_POINT ( 'NONE',  ( 2.250613398900000117, 1417.526871923430008, 235.1186440458980087 ) ) ;
#16188 = CARTESIAN_POINT ( 'NONE',  ( -16.58770733237527395, 1524.425415513989265, 180.6486613107830976 ) ) ;
#16189 = CARTESIAN_POINT ( 'NONE',  ( -12.29441139609999922, 1379.981535577770046, 214.2870256391589976 ) ) ;
#16190 = CARTESIAN_POINT ( 'NONE',  ( 9.251407843868516778, 1419.243067687219764, 232.8166381639402118 ) ) ;
#16191 = ORIENTED_EDGE ( 'NONE', *, *, #46375, .F. ) ;
#16192 = CARTESIAN_POINT ( 'NONE',  ( -32.38601978689752769, 1523.530870145309564, 202.1199661129167851 ) ) ;
#16193 = AXIS2_PLACEMENT_3D ( 'NONE', #110218, #51987, #9970 ) ;
#16194 = FACE_OUTER_BOUND ( 'NONE', #86581, .T. ) ;
#16195 = CARTESIAN_POINT ( 'NONE',  ( -11.15230584153099969, 1482.963738427830094, 204.9460026512250010 ) ) ;
#16196 = CARTESIAN_POINT ( 'NONE',  ( -12.44451260820000016, 1390.433100873249941, 205.6563933776689908 ) ) ;
#16197 = CARTESIAN_POINT ( 'NONE',  ( 10.09736402354529794, 1428.020344045030015, 211.7362985889099889 ) ) ;
#16198 = CARTESIAN_POINT ( 'NONE',  ( 11.80143010066550069, 1421.702045332599937, 203.4210871111559982 ) ) ;
#16199 = CARTESIAN_POINT ( 'NONE',  ( -2.759740495412019712, 1516.551695078709827, 201.4123589199890034 ) ) ;
#16200 = CARTESIAN_POINT ( 'NONE',  ( 4.367411321880000158E-15, 1433.447543843880112, 150.4377610267980003 ) ) ;
#16201 = CARTESIAN_POINT ( 'NONE',  ( -21.83810666687164570, 1509.467311522997079, 191.4893092206315259 ) ) ;
#16202 = CARTESIAN_POINT ( 'NONE',  ( 11.91537912909999974, 1433.481023094019747, 150.2490204454979903 ) ) ;
#16203 = CARTESIAN_POINT ( 'NONE',  ( 8.009058649040055045, 1433.461145011983263, 203.5451010711497872 ) ) ;
#16204 = CARTESIAN_POINT ( 'NONE',  ( -11.03351704759920082, 1462.446871292220067, 208.7211331332790110 ) ) ;
#16205 = VECTOR ( 'NONE', #52533, 1000.000000000000000 ) ;
#16206 = CARTESIAN_POINT ( 'NONE',  ( -16.42371827013585062, 1409.486589267243062, 195.5290734195434936 ) ) ;
#16207 = CARTESIAN_POINT ( 'NONE',  ( 10.73757766294639993, 1423.674038311519780, 203.2439027591769900 ) ) ;
#16208 = CARTESIAN_POINT ( 'NONE',  ( 6.068309900360460141, 1465.453006015229903, 217.9033581894499889 ) ) ;
#16209 = CARTESIAN_POINT ( 'NONE',  ( -15.58089241750000120, 1485.971873082329921, 186.8153789246979954 ) ) ;
#16210 = CIRCLE ( 'NONE', #43033, 1.999999999999999556 ) ;
#16211 = CARTESIAN_POINT ( 'NONE',  ( 13.01309781538156507, 1398.298637390604881, 208.7135361888869625 ) ) ;
#16212 = CARTESIAN_POINT ( 'NONE',  ( -18.02348485499999953, 1410.905797795330045, 224.7336264866979718 ) ) ;
#16213 = CARTESIAN_POINT ( 'NONE',  ( 20.29535750659999849, 1430.346966363130150, 221.2589603778980063 ) ) ;
#16214 = CARTESIAN_POINT ( 'NONE',  ( 34.68852446352948959, 1501.977400791986611, 218.2490599186006932 ) ) ;
#16215 = DIRECTION ( 'NONE',  ( 0.4999999999998399058, 0.7071067811867739472, 0.4999999999998399058 ) ) ;
#16216 = AXIS2_PLACEMENT_3D ( 'NONE', #49751, #93925, #34031 ) ;
#16217 = CARTESIAN_POINT ( 'NONE',  ( -15.70334894381019986, 1383.857901626470039, 219.4107432652749878 ) ) ;
#16218 = CARTESIAN_POINT ( 'NONE',  ( 32.38845791999500534, 1523.382868172864164, 216.1254071228445639 ) ) ;
#16219 = CARTESIAN_POINT ( 'NONE',  ( 2.475018581880529922, 1497.111080376900190, 196.9667223532030107 ) ) ;
#16220 = CARTESIAN_POINT ( 'NONE',  ( -15.33279031426130068, 1420.632256028889969, 207.8836982448250126 ) ) ;
#16221 = CARTESIAN_POINT ( 'NONE',  ( 0.1855511662499469971, 1471.274342563620166, 182.4691293643950019 ) ) ;
#16223 = ORIENTED_EDGE ( 'NONE', *, *, #49063, .T. ) ;
#16222 = CARTESIAN_POINT ( 'NONE',  ( 0.06979890406090000221, 1408.910622955929966, 224.1218459632979716 ) ) ;
#16224 = CARTESIAN_POINT ( 'NONE',  ( -17.22592482065197927, 1443.913060387330233, 162.9227486220069920 ) ) ;
#16225 = CIRCLE ( 'NONE', #225, 1.500000000000001332 ) ;
#16226 = CARTESIAN_POINT ( 'NONE',  ( -16.65152936259426042, 1461.099982565929849, 228.2793266355078856 ) ) ;
#16227 = CARTESIAN_POINT ( 'NONE',  ( -105.0428569062679145, 1377.913060387289988, 308.7873740373456144 ) ) ;
#16228 = CARTESIAN_POINT ( 'NONE',  ( -41.21983904267550258, 1446.341078050689703, 134.0999999985669717 ) ) ;
#16229 = DIRECTION ( 'NONE',  ( -1.000000000000000000, 1.836970198721029688E-16, 0.000000000000000000 ) ) ;
#16230 = EDGE_LOOP ( 'NONE', ( #32557, #17878, #25240, #22997 ) ) ;
#16231 = CARTESIAN_POINT ( 'NONE',  ( -10.16240513719999861, 1472.558925768189965, 209.8189303923120121 ) ) ;
#16232 = CARTESIAN_POINT ( 'NONE',  ( 3.347801439373501609, 1523.456924617337791, 176.1543725842045660 ) ) ;
#16233 = CARTESIAN_POINT ( 'NONE',  ( -104.5039857551601443, 1380.553604562968530, 307.5917977560359873 ) ) ;
#16234 = CARTESIAN_POINT ( 'NONE',  ( -6.123233995736771213E-16, 1379.913060387289988, 209.1218459616989946 ) ) ;
#16235 = CARTESIAN_POINT ( 'NONE',  ( -3.163504309968519834, 1432.488551548530268, 217.0769143716860015 ) ) ;
#16236 = CARTESIAN_POINT ( 'NONE',  ( -17.84338787571901364, 1501.977400791986611, 237.8836641337663309 ) ) ;
#16237 = CARTESIAN_POINT ( 'NONE',  ( 22.95227133490000071, 1507.624369720630057, 210.2367868482679967 ) ) ;
#16238 = CARTESIAN_POINT ( 'NONE',  ( -44.93136599389160324, 1440.913052653349951, 269.6838063022050278 ) ) ;
#16239 = CARTESIAN_POINT ( 'NONE',  ( 8.324963398134689996, 1511.468585895311890, 203.7405340362687411 ) ) ;
#16240 = CARTESIAN_POINT ( 'NONE',  ( -80.12029132004148835, 1385.158018703190010, 283.2668441326100037 ) ) ;
#16241 = CARTESIAN_POINT ( 'NONE',  ( -11.22781813603899792, 1391.913060387289988, 211.9257311578400049 ) ) ;
#16242 = CARTESIAN_POINT ( 'NONE',  ( 11.04921975785680033, 1422.238644613519909, 209.3273474340340101 ) ) ;
#16243 = ORIENTED_EDGE ( 'NONE', *, *, #105682, .F. ) ;
#16244 = CARTESIAN_POINT ( 'NONE',  ( -29.81974126589999941, 1451.871786491030207, 135.2695870736979771 ) ) ;
#16245 = CARTESIAN_POINT ( 'NONE',  ( 13.31970894439976583, 1443.086052842850222, 169.4013815678758306 ) ) ;
#16246 = ADVANCED_FACE ( 'NONE', ( #83992 ), #2062, .T. ) ;
#16248 = ORIENTED_EDGE ( 'NONE', *, *, #40030, .F. ) ;
#16247 = CARTESIAN_POINT ( 'NONE',  ( 0.7056569705168199702, 1437.738171567159952, 227.6607474309619761 ) ) ;
#16249 = CARTESIAN_POINT ( 'NONE',  ( 2.873384031200000077, 1474.047582638690074, 219.3741047921989775 ) ) ;
#16250 = DIRECTION ( 'NONE',  ( 0.7067700477513105817, -0.03085664260695931277, -0.7067700950157954631 ) ) ;
#16251 = CARTESIAN_POINT ( 'NONE',  ( -9.655745333052619728, 1363.739547551583883, 210.6218459616987957 ) ) ;
#16252 = CARTESIAN_POINT ( 'NONE',  ( -10.78591527280000051, 1493.388845731089987, 206.2900157096790110 ) ) ;
#16253 = ADVANCED_FACE ( 'NONE', ( #7291 ), #92943, .T. ) ;
#16254 = CARTESIAN_POINT ( 'NONE',  ( 2.621457251729791160, 1522.051704408389924, 190.1820379210428200 ) ) ;
#16255 = CARTESIAN_POINT ( 'NONE',  ( 13.64529111084437574, 1409.389564452892728, 192.7393524575074082 ) ) ;
#16256 = CARTESIAN_POINT ( 'NONE',  ( 14.93435719577100329, 1430.577349657391323, 220.1736567016903052 ) ) ;
#16257 = CARTESIAN_POINT ( 'NONE',  ( 1.711020842750000215, 1415.875572146229842, 232.5272861542979967 ) ) ;
#16258 = FACE_OUTER_BOUND ( 'NONE', #8995, .T. ) ;
#16259 = CARTESIAN_POINT ( 'NONE',  ( -24.02854066789229748, 1507.902906607559999, 222.3115874531950169 ) ) ;
#16260 = FACE_OUTER_BOUND ( 'NONE', #63398, .T. ) ;
#16261 = CARTESIAN_POINT ( 'NONE',  ( -3.187121981100000223, 1456.171761825189833, 200.1942474277390147 ) ) ;
#16262 = CARTESIAN_POINT ( 'NONE',  ( 5.772403774305000290, 1516.676340709600026, 205.8583240277470168 ) ) ;
#16263 = CARTESIAN_POINT ( 'NONE',  ( 2.499999999909999993, 1447.637843966240098, 170.5315787512979853 ) ) ;
#16264 = ORIENTED_EDGE ( 'NONE', *, *, #80365, .T. ) ;
#16265 = AXIS2_PLACEMENT_3D ( 'NONE', #9131, #103166, #8017 ) ;
#16266 = CARTESIAN_POINT ( 'NONE',  ( -16.67046855446390197, 1516.551188146170034, 196.0483986024819956 ) ) ;
#16267 = CARTESIAN_POINT ( 'NONE',  ( -3.403507246419999799, 1496.471359390990074, 198.2852391338990117 ) ) ;
#16269 = VERTEX_POINT ( 'NONE', #11174 ) ;
#16268 = CARTESIAN_POINT ( 'NONE',  ( -68.47067291010000645, 1379.747730938300265, 280.0399411558590259 ) ) ;
#16270 = CARTESIAN_POINT ( 'NONE',  ( -18.14245636085959745, 1424.695485258009057, 227.8876350735791618 ) ) ;
#16271 = VERTEX_POINT ( 'NONE', #71097 ) ;
#16272 = CARTESIAN_POINT ( 'NONE',  ( -16.31974137077875397, 1514.485057817183815, 223.8138502433834276 ) ) ;
#16273 = CARTESIAN_POINT ( 'NONE',  ( -24.89847827690000059, 1430.363150117730129, 208.6174969999159998 ) ) ;
#16275 = CARTESIAN_POINT ( 'NONE',  ( 15.78263224276630083, 1409.464194525379753, 192.9576963222289976 ) ) ;
#16274 = CARTESIAN_POINT ( 'NONE',  ( -10.15536310392529984, 1425.168171719249813, 103.9028244493299979 ) ) ;
#16276 = CARTESIAN_POINT ( 'NONE',  ( 4.625693865015000128, 1517.042661899400173, 211.4082922958669997 ) ) ;
#16277 = CARTESIAN_POINT ( 'NONE',  ( 36.39711325428599764, 1436.006149706799988, 135.4589782244629816 ) ) ;
#16278 = DIRECTION ( 'NONE',  ( 7.303600220002790452E-17, 1.000000000000000000, -3.615388577796539518E-17 ) ) ;
#16279 = CARTESIAN_POINT ( 'NONE',  ( -39.71667698630000132, 1440.913060382720005, 259.0958797466979604 ) ) ;
#16280 = CARTESIAN_POINT ( 'NONE',  ( 8.001917699090000724, 1477.391948627790043, 200.4742795864889899 ) ) ;
#16281 = CARTESIAN_POINT ( 'NONE',  ( 12.67493581254619883, 1500.776964490709815, 210.0452443345189977 ) ) ;
#16282 = CARTESIAN_POINT ( 'NONE',  ( 4.877535505899020407, 1508.551704408389924, 212.3411737844989773 ) ) ;
#16283 = FACE_OUTER_BOUND ( 'NONE', #101099, .T. ) ;
#16284 = VERTEX_POINT ( 'NONE', #20627 ) ;
#16285 = CARTESIAN_POINT ( 'NONE',  ( 0.4151546846821903003, 1512.187213306747481, 175.3106345060153046 ) ) ;
#16286 = CARTESIAN_POINT ( 'NONE',  ( -18.31479797789999964, 1458.692617178530099, 227.8150927488979960 ) ) ;
#16287 = ORIENTED_EDGE ( 'NONE', *, *, #101450, .T. ) ;
#16288 = ORIENTED_EDGE ( 'NONE', *, *, #30765, .T. ) ;
#16289 = CARTESIAN_POINT ( 'NONE',  ( 0.4279777614790010176, 1433.008008888489940, 203.3794752007089812 ) ) ;
#16290 = CARTESIAN_POINT ( 'NONE',  ( -17.41346946009999996, 1410.020394389830017, 194.0661810129979870 ) ) ;
#16291 = CIRCLE ( 'NONE', #39589, 1.999999999999939826 ) ;
#16292 = DIRECTION ( 'NONE',  ( 0.1403901532130616969, 0.9900962604114879051, 0.000000000000000000 ) ) ;
#16293 = CARTESIAN_POINT ( 'NONE',  ( -15.30294433438259993, 1508.551704408389924, 210.3674297289989852 ) ) ;
#16294 = DIRECTION ( 'NONE',  ( 0.000000000000000000, -1.000000000000000000, 6.123233995736769734E-17 ) ) ;
#16295 = CARTESIAN_POINT ( 'NONE',  ( -5.720967295801010266, 1454.603207479829962, 201.6563704129750079 ) ) ;
#16296 = CARTESIAN_POINT ( 'NONE',  ( 40.71747597329999735, 1448.637563247759999, 134.0999997049979982 ) ) ;
#16297 = CARTESIAN_POINT ( 'NONE',  ( -11.60004869885203682, 1426.786830457828273, 134.3786150874268799 ) ) ;
#16298 = CARTESIAN_POINT ( 'NONE',  ( 9.181048108447960487, 1450.963731741589982, 210.1938350974689911 ) ) ;
#16299 = CARTESIAN_POINT ( 'NONE',  ( -11.38303023819999993, 1391.412213333949921, 213.8762289909089986 ) ) ;
#16300 = CARTESIAN_POINT ( 'NONE',  ( -97.56323068563240497, 1384.866207655270046, 295.7272966331869952 ) ) ;
#16301 = ORIENTED_EDGE ( 'NONE', *, *, #80260, .T. ) ;
#16302 = CARTESIAN_POINT ( 'NONE',  ( 1.125509850285000280, 1517.203017563489766, 201.7827387294869936 ) ) ;
#16303 = CARTESIAN_POINT ( 'NONE',  ( 2.486220101774999858, 1516.939658295650133, 209.1086089184300079 ) ) ;
#16304 = ORIENTED_EDGE ( 'NONE', *, *, #95175, .F. ) ;
#16305 = CARTESIAN_POINT ( 'NONE',  ( 11.77337650133179991, 1427.210515917729936, 146.6415292692670107 ) ) ;
#16306 = B_SPLINE_CURVE_WITH_KNOTS ( 'NONE', 5,
 ( #13893, #64896, #106322, #105228, #62716, #13337, #20104, #48079, #88425 ),
 .UNSPECIFIED., .F., .F.,
 ( 6, 3, 6 ),
 ( 395.8612471010000036, 395.8828220460000011, 406.1136973210000178 ),
 .UNSPECIFIED. ) ;
#16307 = AXIS2_PLACEMENT_3D ( 'NONE', #5475, #48601, #98427 ) ;
#16308 = CARTESIAN_POINT ( 'NONE',  ( 3.699323150121441639, 1511.553933485618018, 217.2221040787129027 ) ) ;
#16309 = EDGE_LOOP ( 'NONE', ( #44227, #44040, #96477, #71606 ) ) ;
#16310 = CARTESIAN_POINT ( 'NONE',  ( -13.25967437340000110, 1414.983773852929744, 220.4242586887980053 ) ) ;
#16311 = CARTESIAN_POINT ( 'NONE',  ( -14.82726497260570042, 1470.530551423540146, 223.5668439764989728 ) ) ;
#16312 = CARTESIAN_POINT ( 'NONE',  ( -17.53631869671869836, 1419.865669823370126, 206.1936457225280321 ) ) ;
#16313 = CIRCLE ( 'NONE', #78947, 2.000000000000003553 ) ;
#16314 = CARTESIAN_POINT ( 'NONE',  ( -9.843061056976221579, 1461.614501156679808, 208.6143076776489806 ) ) ;
#16315 = CARTESIAN_POINT ( 'NONE',  ( -13.01583361319999810, 1416.817366565030170, 221.9085595701980083 ) ) ;
#16316 = CARTESIAN_POINT ( 'NONE',  ( 10.23972724447879834, 1469.612255671459934, 207.2726204608819955 ) ) ;
#16317 = CARTESIAN_POINT ( 'NONE',  ( -10.17586086920000099, 1472.204187410889972, 204.7702763186189827 ) ) ;
#16318 = CARTESIAN_POINT ( 'NONE',  ( -10.90539778630000001, 1489.991646564889834, 212.3805117938089779 ) ) ;
#16319 = CARTESIAN_POINT ( 'NONE',  ( -60.03859995180000197, 1379.727664477899907, 261.7965084652589667 ) ) ;
#16320 = CARTESIAN_POINT ( 'NONE',  ( 22.83994680308489933, 1417.789777542400088, 206.2015004188589842 ) ) ;
#16322 = CARTESIAN_POINT ( 'NONE',  ( -1.738161548016574631, 1451.890872115781576, 184.1703666583102006 ) ) ;
#16321 = CARTESIAN_POINT ( 'NONE',  ( -113.4000000000000057, 1308.913060387289988, 304.2218459572590064 ) ) ;
#16323 = DIRECTION ( 'NONE',  ( 0.000000000000000000, 1.000000000000000000, 0.000000000000000000 ) ) ;
#16324 = CARTESIAN_POINT ( 'NONE',  ( -5.220193992062974964, 1506.416684590318710, 187.7825589291392134 ) ) ;
#16325 = ORIENTED_EDGE ( 'NONE', *, *, #39548, .T. ) ;
#16326 = AXIS2_PLACEMENT_3D ( 'NONE', #63114, #54146, #62562 ) ;
#16327 = DIRECTION ( 'NONE',  ( -0.000000000000000000, -1.000000000000000000, -0.000000000000000000 ) ) ;
#16328 = CARTESIAN_POINT ( 'NONE',  ( -21.78049460968791351, 1524.843416604514914, 233.5929001568862873 ) ) ;
#16329 = CARTESIAN_POINT ( 'NONE',  ( 7.334328272665000092, 1517.005755693489846, 214.1256940922069987 ) ) ;
#16330 = CARTESIAN_POINT ( 'NONE',  ( -2.912453515366174805, 1484.777513947625039, 183.2264124078621705 ) ) ;
#16331 =( BOUNDED_SURFACE ( )  B_SPLINE_SURFACE ( 3, 2, ( 
 ( #106471, #99699, #48233 ),
 ( #63407, #99147, #80725 ),
 ( #89117, #46040, #98058 ),
 ( #13484, #97522, #38703 ) ),
 .UNSPECIFIED., .F., .F., .F. ) 
 B_SPLINE_SURFACE_WITH_KNOTS ( ( 4, 4 ),
 ( 3, 3 ),
 ( 0.000000000000000000, 0.0002960034161023847852 ),
 ( 0.000000000000000000, 1.000000000000000000 ),
 .UNSPECIFIED. ) 
 GEOMETRIC_REPRESENTATION_ITEM ( )  RATIONAL_B_SPLINE_SURFACE ( (
 ( 1.000000000000000000, 0.8070209408750061986, 1.000000000000000000),
 ( 1.000000000000000000, 0.8071723757218256523, 1.000000000000000000),
 ( 1.000000000000000000, 0.8072480346917807470, 1.000000000000000000),
 ( 1.000000000000000000, 0.8072480644198134492, 1.000000000000000000) ) ) 
 REPRESENTATION_ITEM ( '' )  SURFACE ( )  );
#16332 = CARTESIAN_POINT ( 'NONE',  ( -11.44770140791566782, 1425.800648919538389, 139.0556806801066898 ) ) ;
#16334 = ORIENTED_EDGE ( 'NONE', *, *, #31174, .F. ) ;
#16333 = CARTESIAN_POINT ( 'NONE',  ( -11.41430924156969873, 1500.917495223069864, 211.1256234948569954 ) ) ;
#16335 = CARTESIAN_POINT ( 'NONE',  ( -8.848352085069999262, 1384.928008052449968, 199.9247643512989896 ) ) ;
#16336 = CARTESIAN_POINT ( 'NONE',  ( -0.3395211818530010084, 1508.109360918889934, 220.9281624441990175 ) ) ;
#16337 = CARTESIAN_POINT ( 'NONE',  ( -11.77100579110000034, 1426.695143653130117, 146.7217168237980047 ) ) ;
#16338 = CARTESIAN_POINT ( 'NONE',  ( 1.749019635934000005, 1431.032422837999775, 199.8154693994979993 ) ) ;
#16339 = B_SPLINE_CURVE_WITH_KNOTS ( 'NONE', 3,
 ( #62372, #70784, #88661, #104897, #28186, #107648, #108188, #65109, #81881, #66225, #91940, #40433, #99221, #56700, #73514, #90836, #99776, #108745, #15214, #74059, #98133, #39891, #22499, #14120, #48310, #107092, #91403, #21408, #6285, #75163, #56143, #23633, #74610, #49405, #64571, #100345, #14680, #82452, #83530, #57815, #55618, #6824, #31478, #5749, #64020, #65659, #23066, #13560, #57275 ),
 .UNSPECIFIED., .F., .F.,
 ( 4, 2, 2, 2, 1, 1, 2, 2, 2, 2, 1, 1, 1, 2, 2, 2, 2, 1, 1, 1, 1, 2, 2, 2, 2, 1, 1, 2, 2, 4 ),
 ( 0.000000000000000000, 0.2499999999899412129, 0.3749999999849299992, 0.4374999999824081831, 0.4687499999812275164, 0.4843749999805378459, 0.4921874999802942630, 0.4999999999800506245, 0.6249999999766993053, 0.6874999999750367463, 0.7187499999741949752, 0.7343749999738907741, 0.7421874999738452550, 0.7460937499738223844, 0.7499999999737995138, 0.8124999999729637379, 0.8437499999725540656, 0.8593749999723369060, 0.8671874999722284372, 0.8710937499721960187, 0.8730468749726765232, 0.8740234374729166644, 0.8749999999731568057, 0.9062499999781312710, 0.9218749999807583917, 0.9296874999823528940, 0.9335937499831684638, 0.9355468749835762488, 0.9374999999839840337, 1.000000000000000000 ),
 .UNSPECIFIED. ) ;
#16340 = CARTESIAN_POINT ( 'NONE',  ( -11.36959371680000075, 1503.847165134090119, 207.0750569533189775 ) ) ;
#16341 = DIRECTION ( 'NONE',  ( -0.6736849260863841948, 0.000000000000000000, 0.7390186874254148774 ) ) ;
#16342 = LINE ( 'NONE', #75739, #61050 ) ;
#16343 = DIRECTION ( 'NONE',  ( 1.000000000000000000, 0.000000000000000000, 0.000000000000000000 ) ) ;
#16345 = CARTESIAN_POINT ( 'NONE',  ( -11.84683861278779915, 1482.181305081889832, 208.0213636573200233 ) ) ;
#16344 = CARTESIAN_POINT ( 'NONE',  ( -21.65371239889999799, 1482.726465196330082, 224.5928689438979973 ) ) ;
#16346 = DIRECTION ( 'NONE',  ( 1.000000000000000000, -0.000000000000000000, 1.224646799147353207E-16 ) ) ;
#16347 = ORIENTED_EDGE ( 'NONE', *, *, #96276, .F. ) ;
#16348 = CARTESIAN_POINT ( 'NONE',  ( 1.119439089684999944, 1517.026534522949987, 205.8528207963470038 ) ) ;
#16349 = CARTESIAN_POINT ( 'NONE',  ( 21.73145256330000308, 1410.542624686630234, 269.3317000074980001 ) ) ;
#16350 = MECHANICAL_DESIGN_GEOMETRIC_PRESENTATION_REPRESENTATION (  '', ( #27106 ), #86153 ) ;
#16351 = CARTESIAN_POINT ( 'NONE',  ( -32.22536377336267321, 1523.621879633028584, 216.8351145222433445 ) ) ;
#16352 = CARTESIAN_POINT ( 'NONE',  ( 19.46859404899999646, 1449.731791413250221, 192.7299627095979986 ) ) ;
#16353 = CARTESIAN_POINT ( 'NONE',  ( 9.033549554615403210, 1506.660407547515661, 229.3903933438921285 ) ) ;
#16354 = CARTESIAN_POINT ( 'NONE',  ( -8.297485596343202374, 1387.805263089111804, 218.3696328644297751 ) ) ;
#16355 = CARTESIAN_POINT ( 'NONE',  ( -1.772878804569999911, 1450.437861259890042, 182.6449559054979659 ) ) ;
#16356 = DIRECTION ( 'NONE',  ( 0.000000000000000000, 0.000000000000000000, -1.000000000000000000 ) ) ;
#16357 = CARTESIAN_POINT ( 'NONE',  ( -15.51485357750000205, 1417.141638888899934, 205.6853114639490059 ) ) ;
#16358 = CARTESIAN_POINT ( 'NONE',  ( -13.59250350780000005, 1443.952310951140134, 187.6074426047979955 ) ) ;
#16359 = CARTESIAN_POINT ( 'NONE',  ( -18.70730727500000157, 1431.113060387329824, 209.1218459618889938 ) ) ;
#16360 = CARTESIAN_POINT ( 'NONE',  ( -16.22004022801489143, 1419.733241725250082, 209.9150677488009933 ) ) ;
#16361 = CARTESIAN_POINT ( 'NONE',  ( -3.703568344589999839, 1497.311626104689822, 220.9591690177990131 ) ) ;
#16362 = CARTESIAN_POINT ( 'NONE',  ( -2.483162238130000254, 1476.934831443589928, 201.9767984309089854 ) ) ;
#16363 = CARTESIAN_POINT ( 'NONE',  ( -18.56011888160000112, 1441.602307344989867, 211.8044997558990303 ) ) ;
#16364 = CARTESIAN_POINT ( 'NONE',  ( 10.55629857124240090, 1481.744597751460105, 209.9319926063880075 ) ) ;
#16365 = CARTESIAN_POINT ( 'NONE',  ( -22.59589169830000088, 1507.700907224229923, 190.9355248029980032 ) ) ;
#16366 = VECTOR ( 'NONE', #26878, 1000.000000000000114 ) ;
#16367 = CARTESIAN_POINT ( 'NONE',  ( -12.58443858789999936, 1474.054838308030185, 269.4439571418980108 ) ) ;
#16368 = CARTESIAN_POINT ( 'NONE',  ( -30.95230591800407893, 1524.659802833171625, 196.4586593495655507 ) ) ;
#16369 = CARTESIAN_POINT ( 'NONE',  ( -14.69197387124563292, 1514.485034114827613, 192.8020852113455135 ) ) ;
#16370 = CARTESIAN_POINT ( 'NONE',  ( -24.05485985184647646, 1444.308342016315237, 212.3257452429839987 ) ) ;
#16371 = CARTESIAN_POINT ( 'NONE',  ( -55.35023455054019337, 1384.715211743480040, 272.4935865345279922 ) ) ;
#16372 = CARTESIAN_POINT ( 'NONE',  ( -22.90005503110699792, 1384.955863742640076, 202.5115359936190202 ) ) ;
#16373 = CARTESIAN_POINT ( 'NONE',  ( -9.704564366399999642, 1443.913060387330006, 153.0477571643979786 ) ) ;
#16374 = CARTESIAN_POINT ( 'NONE',  ( -106.9496064929999903, 1379.185917738360104, 299.9942942488589779 ) ) ;
#16375 = CARTESIAN_POINT ( 'NONE',  ( -16.51111913633352302, 1525.159196711359755, 237.1918705644680756 ) ) ;
#16376 = CARTESIAN_POINT ( 'NONE',  ( -46.15244900134240424, 1440.913028098642371, 268.2044261680690624 ) ) ;
#16377 = CARTESIAN_POINT ( 'NONE',  ( -22.86371263479999882, 1409.875940094530051, 206.1192440645280044 ) ) ;
#16378 = CARTESIAN_POINT ( 'NONE',  ( -9.449812779362575910, 1380.957496575889991, 201.0964360788809131 ) ) ;
#16379 = AXIS2_PLACEMENT_3D ( 'NONE', #100901, #90866, #73542 ) ;
#16380 = CARTESIAN_POINT ( 'NONE',  ( 4.650698360960000777, 1484.263765184789918, 220.0138998524990086 ) ) ;
#16381 = DIRECTION ( 'NONE',  ( 5.980589973904019347E-17, -1.000000000000000000, 1.736889445713099699E-16 ) ) ;
#16382 = CARTESIAN_POINT ( 'NONE',  ( 1.633469776390000128, 1432.353341358199941, 150.3624711946980028 ) ) ;
#16383 = CARTESIAN_POINT ( 'NONE',  ( -8.069527880069999881, 1440.230228425089763, 228.7261013027990089 ) ) ;
#16384 = CARTESIAN_POINT ( 'NONE',  ( -6.455447987151660350, 1508.551704612109916, 215.9494998419519902 ) ) ;
#16385 = CARTESIAN_POINT ( 'NONE',  ( -29.35128565762720143, 1441.653456051720013, 137.2693278004479964 ) ) ;
#16387 = CARTESIAN_POINT ( 'NONE',  ( -12.10275407134929893, 1377.603811883519938, 211.3932643068179971 ) ) ;
#16386 = CARTESIAN_POINT ( 'NONE',  ( -16.94686494584989944, 1417.489848084730056, 207.8186904396790169 ) ) ;
#16388 = CARTESIAN_POINT ( 'NONE',  ( 11.69528020852439987, 1426.723312899609937, 141.1826440969780094 ) ) ;
#16389 = CARTESIAN_POINT ( 'NONE',  ( -15.76859352898596356, 1409.463696381290220, 225.2884038137482037 ) ) ;
#16390 = DIRECTION ( 'NONE',  ( -1.000000000000000000, 0.000000000000000000, 0.000000000000000000 ) ) ;
#16391 = CARTESIAN_POINT ( 'NONE',  ( 7.889297498873377279, 1517.051704408389924, 211.8362768761033124 ) ) ;
#16392 = DIRECTION ( 'NONE',  ( 0.000000000000000000, 0.000000000000000000, 1.000000000000000000 ) ) ;
#16393 = CARTESIAN_POINT ( 'NONE',  ( -3.262264688434999726, 1516.633288330999903, 202.5742890007669814 ) ) ;
#16394 = PLANE ( 'NONE',  #55363 ) ;
#16395 = CARTESIAN_POINT ( 'NONE',  ( -13.01602554077795304, 1398.298692311873083, 208.8134195757005500 ) ) ;
#16396 = CYLINDRICAL_SURFACE ( 'NONE', #81940, 29.99999999999999645 ) ;
#16397 = DIRECTION ( 'NONE',  ( 0.7063774289747313251, 0.04540766091858282338, 0.7063774289747313251 ) ) ;
#16398 = CARTESIAN_POINT ( 'NONE',  ( -24.48072446064930219, 1378.898509916240073, 215.5032166125519950 ) ) ;
#16399 = CIRCLE ( 'NONE', #70111, 1.000000000000000888 ) ;
#16400 = CARTESIAN_POINT ( 'NONE',  ( 20.53373553494599690, 1507.794785362809989, 228.2241617207620266 ) ) ;
#16402 = ORIENTED_EDGE ( 'NONE', *, *, #4413, .T. ) ;
#16401 = CARTESIAN_POINT ( 'NONE',  ( -52.38592625916200518, 1379.720821623890060, 249.9316393081959973 ) ) ;
#16403 = VERTEX_POINT ( 'NONE', #106314 ) ;
#16404 = CARTESIAN_POINT ( 'NONE',  ( 11.38192139399690106, 1434.162350676260075, 151.4680933403080019 ) ) ;
#16405 = CARTESIAN_POINT ( 'NONE',  ( -6.969102451020000366, 1396.156426807830030, 218.5728573129879919 ) ) ;
#16406 = ORIENTED_EDGE ( 'NONE', *, *, #51819, .F. ) ;
#16407 = CARTESIAN_POINT ( 'NONE',  ( -15.96075179420000367, 1466.903945902690111, 196.1521398069990312 ) ) ;
#16408 = CARTESIAN_POINT ( 'NONE',  ( -109.3074459329999968, 1384.922460900670103, 311.2646700692590116 ) ) ;
#16409 = CARTESIAN_POINT ( 'NONE',  ( -8.002723402924999618, 1516.551704408390151, 212.1748218667169965 ) ) ;
#16411 = CARTESIAN_POINT ( 'NONE',  ( 17.55317606050000023, 1419.032763066429879, 226.2188323924980011 ) ) ;
#16410 = CARTESIAN_POINT ( 'NONE',  ( 2.370970874524634286, 1427.002265528474027, 137.0999999980979851 ) ) ;
#16412 = CARTESIAN_POINT ( 'NONE',  ( 14.67020375005709987, 1498.108088576179853, 231.9734902996929975 ) ) ;
#16413 = TOROIDAL_SURFACE ( 'NONE', #88004, 24.69926344187880929, 1.000000000000000000 ) ;
#16414 = CARTESIAN_POINT ( 'NONE',  ( 1.204114676109999893, 1468.707964903529955, 182.7289636863979752 ) ) ;
#16415 = CARTESIAN_POINT ( 'NONE',  ( 2.158120808530000101, 1468.703739625189883, 218.9192338835489977 ) ) ;
#16416 = FACE_OUTER_BOUND ( 'NONE', #76385, .T. ) ;
#16417 = SURFACE_STYLE_FILL_AREA ( #15863 ) ;
#16418 = CARTESIAN_POINT ( 'NONE',  ( 4.660514127639999060, 1441.207016471189945, 213.1086252044090088 ) ) ;
#16419 = CARTESIAN_POINT ( 'NONE',  ( 0.9518847404210000196, 1415.296882282229944, 191.1939211731979924 ) ) ;
#16420 = CARTESIAN_POINT ( 'NONE',  ( 11.28896394650000090, 1431.382221484100000, 151.4573443959979784 ) ) ;
#16421 = CARTESIAN_POINT ( 'NONE',  ( 7.777075013794999769, 1512.220794350750111, 202.5940153888870157 ) ) ;
#16422 = ORIENTED_EDGE ( 'NONE', *, *, #90884, .T. ) ;
#16423 = CARTESIAN_POINT ( 'NONE',  ( 13.25659408744109946, 1435.807411741510123, 150.5347871980940226 ) ) ;
#16424 = ORIENTED_EDGE ( 'NONE', *, *, #38611, .F. ) ;
#16425 = ORIENTED_EDGE ( 'NONE', *, *, #75423, .F. ) ;
#16426 = EDGE_CURVE ( 'NONE', #16271, #81031, #9497, .T. ) ;
#16427 = CARTESIAN_POINT ( 'NONE',  ( -18.91742159790479860, 1507.874522033449921, 229.7221451244979846 ) ) ;
#16428 = CARTESIAN_POINT ( 'NONE',  ( -5.248956291309999855, 1464.339271744430107, 236.4982892100979939 ) ) ;
#16429 = CARTESIAN_POINT ( 'NONE',  ( -7.313058470103319664, 1475.195669987933570, 201.8552237540184535 ) ) ;
#16430 = CARTESIAN_POINT ( 'NONE',  ( 2.872700517194999748, 1516.559109716219837, 216.8315272385270021 ) ) ;
#16431 = CARTESIAN_POINT ( 'NONE',  ( -7.910120449074414140, 1511.948750844499273, 212.1811042407670129 ) ) ;
#16432 = CARTESIAN_POINT ( 'NONE',  ( 11.58978176042640129, 1422.008781663779928, 209.7162554888329851 ) ) ;
#16433 = CARTESIAN_POINT ( 'NONE',  ( 2.500000000000000000, 1448.240804457780087, 166.0721002888749922 ) ) ;
#16434 = CARTESIAN_POINT ( 'NONE',  ( -3.771520293490000064, 1376.318813996809922, 206.9293833799489732 ) ) ;
#16435 = ORIENTED_EDGE ( 'NONE', *, *, #10873, .F. ) ;
#16436 = CARTESIAN_POINT ( 'NONE',  ( -1.716392779905000054, 1516.788317650260069, 206.2580580763669786 ) ) ;
#16437 = ORIENTED_EDGE ( 'NONE', *, *, #46604, .F. ) ;
#16438 = CARTESIAN_POINT ( 'NONE',  ( 1.715743480078970019E-15, 1374.913060387289988, 209.1218459572589836 ) ) ;
#16439 = CARTESIAN_POINT ( 'NONE',  ( -19.94169788180000324, 1509.369061779629874, 230.2160215658979894 ) ) ;
#16440 = CARTESIAN_POINT ( 'NONE',  ( -12.98407978699999887, 1410.739677414529979, 189.6949195340980054 ) ) ;
#16441 = CARTESIAN_POINT ( 'NONE',  ( 7.809063913224999709, 1513.978875661350230, 216.3009730514370119 ) ) ;
#16443 = ORIENTED_EDGE ( 'NONE', *, *, #55659, .T. ) ;
#16442 = CARTESIAN_POINT ( 'NONE',  ( -0.1558546717220200273, 1414.913057860449953, 225.5221266254029899 ) ) ;
#16444 = CARTESIAN_POINT ( 'NONE',  ( 20.84789745129999972, 1428.606193423530158, 221.9193905426979825 ) ) ;
#16445 = CARTESIAN_POINT ( 'NONE',  ( 3.960829545962760267, 1442.649591851693231, 217.0772145634146284 ) ) ;
#16446 = CARTESIAN_POINT ( 'NONE',  ( 5.407632277616277072, 1505.250895293119584, 219.8892970404575919 ) ) ;
#16447 = CARTESIAN_POINT ( 'NONE',  ( 7.122515158009999681, 1452.871264857790266, 215.2372064891289654 ) ) ;
#16448 = CARTESIAN_POINT ( 'NONE',  ( 22.52214966617865599, 1524.244163922423013, 181.7424121231467211 ) ) ;
#16449 = CARTESIAN_POINT ( 'NONE',  ( 3.459156578084999989, 1516.769879638719885, 213.7318425517769924 ) ) ;
#16450 = CARTESIAN_POINT ( 'NONE',  ( -3.188751157463979968, 1428.815501146380029, 200.3155279938000035 ) ) ;
#16451 = CARTESIAN_POINT ( 'NONE',  ( -20.34464802829999996, 1507.870840051529967, 189.3862473984979999 ) ) ;
#16453 = EDGE_CURVE ( 'NONE', #13558, #27509, #71352, .T. ) ;
#16452 = CARTESIAN_POINT ( 'NONE',  ( 15.69795926888880189, 1517.051704408389924, 222.7678737654429995 ) ) ;
#16454 = CARTESIAN_POINT ( 'NONE',  ( 0.01319650876840149957, 1516.941178807709775, 211.4140629809269853 ) ) ;
#16455 = EDGE_CURVE ( 'NONE', #4488, #29284, #61059, .T. ) ;
#16456 = CARTESIAN_POINT ( 'NONE',  ( 9.367166360012699755, 1434.455447298550098, 206.3420816845940067 ) ) ;
#16457 = CARTESIAN_POINT ( 'NONE',  ( -11.75537608917499810, 1482.386081586160117, 207.2708069926649728 ) ) ;
#16458 = CARTESIAN_POINT ( 'NONE',  ( -11.41379966406813296, 1486.020606230438489, 184.4293688767625667 ) ) ;
#16459 = EDGE_CURVE ( 'NONE', #95667, #74706, #46744, .T. ) ;
#16461 = ORIENTED_EDGE ( 'NONE', *, *, #98671, .F. ) ;
#16460 = CARTESIAN_POINT ( 'NONE',  ( -58.30163007960000243, 1385.052442321870103, 240.0694839391589994 ) ) ;
#16463 = VECTOR ( 'NONE', #61045, 1000.000000000000114 ) ;
#16462 = CARTESIAN_POINT ( 'NONE',  ( -77.48449076556670434, 1385.000788814369798, 302.0789985806010236 ) ) ;
#16464 = CARTESIAN_POINT ( 'NONE',  ( 41.23308670169999601, 1446.065286249370047, 261.5842860979980173 ) ) ;
#16465 = ADVANCED_FACE ( 'NONE', ( #38014 ), #20935, .F. ) ;
#16466 = CARTESIAN_POINT ( 'NONE',  ( -4.473512919476954508, 1370.472450005593828, 209.0513769001518654 ) ) ;
#16467 = EDGE_CURVE ( 'NONE', #105726, #714, #81104, .T. ) ;
#16468 = CARTESIAN_POINT ( 'NONE',  ( -17.58460349159999936, 1489.029732347030176, 229.1403505218980001 ) ) ;
#16469 = DIRECTION ( 'NONE',  ( -1.755985294532469921E-16, 1.000000000000000000, -1.338183447452831989E-16 ) ) ;
#16470 = CARTESIAN_POINT ( 'NONE',  ( 11.92849869073500102, 1511.839858410419993, 224.1270719350669935 ) ) ;
#16472 = CARTESIAN_POINT ( 'NONE',  ( -7.768842288750000158, 1384.896297089410155, 218.9179251193689879 ) ) ;
#16471 = CARTESIAN_POINT ( 'NONE',  ( -9.642223397419670050, 1460.679120766980077, 208.4218084076549928 ) ) ;
#16473 = DIRECTION ( 'NONE',  ( -8.832268201338159945E-47, 1.000000000000000000, -1.836970198721029688E-16 ) ) ;
#16474 = CARTESIAN_POINT ( 'NONE',  ( -107.3898476250000016, 1380.885722407379944, 309.4972360872590116 ) ) ;
#16475 = ORIENTED_EDGE ( 'NONE', *, *, #57143, .F. ) ;
#16476 = CARTESIAN_POINT ( 'NONE',  ( -4.618749106614999711, 1516.729202374750002, 202.5720834851169911 ) ) ;
#16477 = VECTOR ( 'NONE', #51330, 1000.000000000000000 ) ;
#16478 = CARTESIAN_POINT ( 'NONE',  ( 15.47624034080000222, 1495.631162584530102, 224.0604253471979916 ) ) ;
#16479 = CARTESIAN_POINT ( 'NONE',  ( 13.06218954519999897, 1425.740256908130050, 222.9850514811979849 ) ) ;
#16480 = CARTESIAN_POINT ( 'NONE',  ( -33.23421991949448540, 1522.906363951597314, 217.4142352873258517 ) ) ;
#16481 = CARTESIAN_POINT ( 'NONE',  ( -7.615310476975459153, 1461.877859386345108, 203.0812156602634957 ) ) ;
#16482 = ADVANCED_FACE ( 'NONE', ( #72725 ), #98577, .F. ) ;
#16483 = CARTESIAN_POINT ( 'NONE',  ( 25.39696813641784701, 1450.809552082115033, 137.2718642792816297 ) ) ;
#16484 = CARTESIAN_POINT ( 'NONE',  ( 2.921131820879320440, 1415.930151663460038, 231.8786077272699799 ) ) ;
#16485 = CARTESIAN_POINT ( 'NONE',  ( 29.70034115211240078, 1436.430129212750217, 136.6408550299620117 ) ) ;
#16486 = CARTESIAN_POINT ( 'NONE',  ( -105.4593524538789211, 1391.263055996386356, 303.4133149664163511 ) ) ;
#16487 = CARTESIAN_POINT ( 'NONE',  ( -4.161595075237580765, 1448.982995846620042, 185.0801961897900298 ) ) ;
#16488 = DIRECTION ( 'NONE',  ( 0.9983395709201744461, -0.05760296116452706672, 0.000000000000000000 ) ) ;
#16489 = CARTESIAN_POINT ( 'NONE',  ( 8.991745348219998490, 1509.227059053930134, 181.2342631838979798 ) ) ;
#16490 = CARTESIAN_POINT ( 'NONE',  ( -20.92528168612626871, 1525.790286462515724, 184.9905026533984937 ) ) ;
#16491 = ADVANCED_FACE ( 'NONE', ( #107407 ), #30141, .F. ) ;
#16492 = DIRECTION ( 'NONE',  ( 0.000000000000000000, 1.000000000000000000, 0.000000000000000000 ) ) ;
#16493 = ORIENTED_EDGE ( 'NONE', *, *, #69502, .F. ) ;
#16494 = CARTESIAN_POINT ( 'NONE',  ( -7.834251258605340773, 1439.563479556370112, 205.1891270341679956 ) ) ;
#16495 = CARTESIAN_POINT ( 'NONE',  ( -42.04388406582121007, 1427.611912910882893, 269.0746004808472662 ) ) ;
#16496 = EDGE_CURVE ( 'NONE', #4497, #39082, #25851, .T. ) ;
#16497 = CARTESIAN_POINT ( 'NONE',  ( 11.40506975472390039, 1471.056480956299993, 209.4187964280920085 ) ) ;
#16498 = CARTESIAN_POINT ( 'NONE',  ( 14.07564986092039838, 1417.487964905419858, 190.9160242924600084 ) ) ;
#16499 = CARTESIAN_POINT ( 'NONE',  ( -0.3298027038899999930, 1417.349066637030091, 235.5653369626979838 ) ) ;
#16500 = CARTESIAN_POINT ( 'NONE',  ( 12.23427440210000050, 1501.005680718390067, 210.1402780287790222 ) ) ;
#16501 = CARTESIAN_POINT ( 'NONE',  ( 25.16854151965715047, 1451.224510553128539, 137.5711253996577739 ) ) ;
#16502 = CARTESIAN_POINT ( 'NONE',  ( 8.071448428540000108, 1423.066654972070182, 213.1913406456689870 ) ) ;
#16503 = CARTESIAN_POINT ( 'NONE',  ( -4.082778200585359230, 1515.071394777460000, 212.7081675216069812 ) ) ;
#16504 = EDGE_CURVE ( 'NONE', #86231, #92059, #16313, .T. ) ;
#16505 = CARTESIAN_POINT ( 'NONE',  ( 44.13011777698019955, 1440.913039006840108, 270.2165842967739877 ) ) ;
#16506 = CARTESIAN_POINT ( 'NONE',  ( -20.87972035156535355, 1450.952513135669733, 144.6011053034232248 ) ) ;
#16507 = CARTESIAN_POINT ( 'NONE',  ( 24.50330256149999997, 1435.537756670989893, 137.2482190513979958 ) ) ;
#16508 = CARTESIAN_POINT ( 'NONE',  ( -13.14482159525874394, 1443.063907452323292, 169.3991812976872211 ) ) ;
#16509 = ORIENTED_EDGE ( 'NONE', *, *, #64587, .T. ) ;
#16510 = CYLINDRICAL_SURFACE ( 'NONE', #85581, 2.000000000000003109 ) ;
#16511 = CARTESIAN_POINT ( 'NONE',  ( -13.71394807775421754, 1379.587227311490551, 211.8543316273178334 ) ) ;
#16512 = ORIENTED_EDGE ( 'NONE', *, *, #13086, .F. ) ;
#16513 = ORIENTED_EDGE ( 'NONE', *, *, #85173, .F. ) ;
#16514 = DIRECTION ( 'NONE',  ( -0.6709778558543689764, 0.000000000000000000, 0.7414773880254701410 ) ) ;
#16515 = CARTESIAN_POINT ( 'NONE',  ( 6.795238182784275160, 1516.616925273614470, 205.9304268409078702 ) ) ;
#16517 = CARTESIAN_POINT ( 'NONE',  ( -12.01188880439999984, 1460.226730015830071, 225.2520635090980079 ) ) ;
#16516 = CARTESIAN_POINT ( 'NONE',  ( 42.06232107555830169, 1440.913060387330006, 269.6487541170399709 ) ) ;
#16518 = CARTESIAN_POINT ( 'NONE',  ( -8.747337044410000928, 1447.713205128089839, 212.1116229988289774 ) ) ;
#16519 = CARTESIAN_POINT ( 'NONE',  ( -11.46138297819999963, 1433.011133141609889, 151.3008369595980014 ) ) ;
#16520 = CARTESIAN_POINT ( 'NONE',  ( -12.30145601893210028, 1378.350113758880070, 209.9325833000719967 ) ) ;
#16521 = CARTESIAN_POINT ( 'NONE',  ( -2.911024527881161283, 1419.547881642413813, 186.2020241882692915 ) ) ;
#16522 = CARTESIAN_POINT ( 'NONE',  ( -2.180465155517607556, 1524.667648926078982, 244.2585483383492715 ) ) ;
#16523 = CARTESIAN_POINT ( 'NONE',  ( -24.60027558000000170, 1439.385484703360135, 210.6880631153979664 ) ) ;
#16524 = FACE_BOUND ( 'NONE', #18189, .T. ) ;
#16525 = CARTESIAN_POINT ( 'NONE',  ( 2.175561048050000057, 1450.072456872719840, 182.0601473783979998 ) ) ;
#16526 = CARTESIAN_POINT ( 'NONE',  ( 8.776071739740523014, 1364.218562676873489, 207.6218459616988241 ) ) ;
#16527 = CARTESIAN_POINT ( 'NONE',  ( -28.81191669830696611, 1510.030278085835562, 217.4830671067354899 ) ) ;
#16529 = ORIENTED_EDGE ( 'NONE', *, *, #94649, .T. ) ;
#16528 = CARTESIAN_POINT ( 'NONE',  ( -2.798875629058170013E-09, 1414.961829792250001, 244.5380620272480030 ) ) ;
#16530 = ORIENTED_EDGE ( 'NONE', *, *, #57775, .F. ) ;
#16531 = CARTESIAN_POINT ( 'NONE',  ( -11.78013554155059950, 1427.423339285529892, 147.0626577189019883 ) ) ;
#16532 = CARTESIAN_POINT ( 'NONE',  ( 7.396545043095000160, 1511.069621805459974, 202.7496783316070150 ) ) ;
#16533 = CARTESIAN_POINT ( 'NONE',  ( -4.188706515999999880, 1472.474584819730126, 270.3708462686980170 ) ) ;
#16534 = CARTESIAN_POINT ( 'NONE',  ( 10.64883854889802706, 1501.422591975932619, 204.8277787321165135 ) ) ;
#16535 = CARTESIAN_POINT ( 'NONE',  ( -120.3440751137400895, 1358.631207110789774, 311.1659210709988770 ) ) ;
#16536 = CARTESIAN_POINT ( 'NONE',  ( 17.35500899530000041, 1519.913060387329779, 193.1522642759980215 ) ) ;
#16537 = CARTESIAN_POINT ( 'NONE',  ( -0.2312796901443630038, 1475.734222155040015, 197.6677150511999912 ) ) ;
#16538 = DIRECTION ( 'NONE',  ( 0.000000000000000000, 0.000000000000000000, 1.000000000000000000 ) ) ;
#16539 = CARTESIAN_POINT ( 'NONE',  ( 5.705396399765596094, 1370.592093591774528, 208.3718459617010978 ) ) ;
#16540 = CARTESIAN_POINT ( 'NONE',  ( -15.05358279999999915, 1410.831827720429828, 226.7261506157979909 ) ) ;
#16541 = CARTESIAN_POINT ( 'NONE',  ( -10.66017895455560094, 1406.634972685779985, 267.8057047216510114 ) ) ;
#16542 = CARTESIAN_POINT ( 'NONE',  ( -14.48276039151240013, 1435.993670758189865, 149.8592331176449761 ) ) ;
#16543 = ORIENTED_EDGE ( 'NONE', *, *, #68643, .F. ) ;
#16544 = CARTESIAN_POINT ( 'NONE',  ( -4.326992699990039881, 1515.158586642889986, 209.1858684987689969 ) ) ;
#16545 = CARTESIAN_POINT ( 'NONE',  ( 14.41410989250000085, 1444.046959656890067, 189.7051000925980020 ) ) ;
#16546 = ORIENTED_EDGE ( 'NONE', *, *, #100359, .F. ) ;
#16547 = EDGE_LOOP ( 'NONE', ( #65930, #18094, #116, #39249, #109308, #51984 ) ) ;
#16548 = EDGE_CURVE ( 'NONE', #59443, #52693, #79238, .T. ) ;
#16549 = CARTESIAN_POINT ( 'NONE',  ( 4.948917002315981861, 1423.300699232361467, 184.2784904492603744 ) ) ;
#16550 = CARTESIAN_POINT ( 'NONE',  ( 8.314894252674610797, 1425.054012563349943, 194.6595790585679993 ) ) ;
#16551 = CARTESIAN_POINT ( 'NONE',  ( 2.295485501044999932, 1516.651306816259876, 214.1175719399469983 ) ) ;
#16552 = CARTESIAN_POINT ( 'NONE',  ( -6.487916422619999679, 1485.477811444930012, 183.8195409892980194 ) ) ;
#16553 = FACE_OUTER_BOUND ( 'NONE', #41727, .T. ) ;
#16554 = ORIENTED_EDGE ( 'NONE', *, *, #56227, .T. ) ;
#16555 = CARTESIAN_POINT ( 'NONE',  ( -113.4000000000000057, 1376.913060387289988, 301.4143084471589873 ) ) ;
#16556 = CARTESIAN_POINT ( 'NONE',  ( -1.710004586925000236, 1516.557392317769882, 202.5758445815369839 ) ) ;
#16557 = EDGE_CURVE ( 'NONE', #77352, #98841, #75282, .T. ) ;
#16558 = CARTESIAN_POINT ( 'NONE',  ( -26.35475474280000086, 1507.985742568630030, 201.5462048709279941 ) ) ;
#16559 = LINE ( 'NONE', #77614, #48068 ) ;
#16560 = CARTESIAN_POINT ( 'NONE',  ( -32.90424402952790217, 1384.563281534569796, 207.2982514105669907 ) ) ;
#16561 = CARTESIAN_POINT ( 'NONE',  ( -1.299927615229999889, 1406.964219534829908, 196.1218459552979994 ) ) ;
#16562 = CARTESIAN_POINT ( 'NONE',  ( -108.9389063659999977, 1385.729741725900112, 311.1830050262590248 ) ) ;
#16564 = VERTEX_POINT ( 'NONE', #22832 ) ;
#16563 = LINE ( 'NONE', #85439, #110171 ) ;
#16565 = CARTESIAN_POINT ( 'NONE',  ( 19.28191951490000022, 1455.753434004590190, 211.0002536610790003 ) ) ;
#16566 = CARTESIAN_POINT ( 'NONE',  ( 24.29269244049999799, 1508.123907550730110, 221.3514521437980136 ) ) ;
#16567 = CARTESIAN_POINT ( 'NONE',  ( -57.28255472204047294, 1379.717548595288235, 260.3994659975323884 ) ) ;
#16568 = CARTESIAN_POINT ( 'NONE',  ( 10.63748064366419932, 1460.271151926629955, 206.6808178792470017 ) ) ;
#16569 = CARTESIAN_POINT ( 'NONE',  ( -12.96423123134679933, 1435.988822720060170, 150.7593588700239877 ) ) ;
#16570 = CARTESIAN_POINT ( 'NONE',  ( -2.864043456445000135, 1516.811292230880099, 211.4208600009669965 ) ) ;
#16571 = CARTESIAN_POINT ( 'NONE',  ( -68.55439833990000409, 1379.747438846910200, 279.6432152850590001 ) ) ;
#16572 = CARTESIAN_POINT ( 'NONE',  ( -5.909698491649999497, 1449.521837735690042, 210.1656816284789784 ) ) ;
#16573 = B_SPLINE_CURVE_WITH_KNOTS ( 'NONE', 5,
 ( #89893, #56307, #62538, #3720, #63094, #89350, #64732, #4252, #19929 ),
 .UNSPECIFIED., .F., .F.,
 ( 6, 3, 6 ),
 ( 7.637039622810000594, 12.23404602909999994, 12.63071162247140045 ),
 .UNSPECIFIED. ) ;
#16574 = CARTESIAN_POINT ( 'NONE',  ( 4.050793647536233166, 1440.940971268299108, 156.1560896747039067 ) ) ;
#16575 = EDGE_CURVE ( 'NONE', #6139, #43805, #44993, .T. ) ;
#16576 = CARTESIAN_POINT ( 'NONE',  ( 3.449647440015000122, 1516.829948096479939, 208.3645479958780129 ) ) ;
#16577 = EDGE_LOOP ( 'NONE', ( #905, #13727, #69289, #102941, #68421 ) ) ;
#16578 = CARTESIAN_POINT ( 'NONE',  ( -42.60628463180169945, 1443.705283475299893, 134.4203400610479946 ) ) ;
#16579 = CARTESIAN_POINT ( 'NONE',  ( -11.73563908010000034, 1425.610159190430068, 144.1657657165980027 ) ) ;
#16580 = CARTESIAN_POINT ( 'NONE',  ( -5.958828918510000072, 1385.041501276899908, 218.5259373746190192 ) ) ;
#16581 = ORIENTED_EDGE ( 'NONE', *, *, #32467, .F. ) ;
#16582 = CARTESIAN_POINT ( 'NONE',  ( 7.357707608180000136, 1481.868694410790113, 209.7897133371670009 ) ) ;
#16583 = CARTESIAN_POINT ( 'NONE',  ( -21.75051292122820712, 1509.709027869026613, 229.3696503746045607 ) ) ;
#16584 = CARTESIAN_POINT ( 'NONE',  ( -4.071011801012067721, 1440.982759184028509, 184.9244102487123200 ) ) ;
#16585 = B_SPLINE_CURVE_WITH_KNOTS ( 'NONE', 3,
 ( #107583, #15155, #98624, #66710, #23569, #49346, #7331, #56090, #90216, #82930, #13501, #82390, #40928, #39276, #108126, #31420, #31978, #66168, #73450, #21890, #100818, #99715, #49898, #48807, #58297, #30319, #100289, #14060, #72892, #48247, #91882, #23008, #83472, #30869, #92419, #99161, #107033, #64507, #22441, #90777, #56643, #34182, #7872 ),
 .UNSPECIFIED., .F., .F.,
 ( 4, 3, 3, 3, 3, 3, 3, 3, 3, 3, 3, 3, 3, 3, 4 ),
 ( -2.000000000000000000, -1.991901403786979996, -1.843562329601740046, -1.687124659203469879, -1.535545284513649911, -1.380727046018200177, -1.226212339367769966, -1.070990695444660190, -0.9154280613754459672, -0.7599146134399699104, -0.6053024803659901032, -0.4517551365012870690, -0.2995620430569270187, -0.1489321397233329680, -3.117070652702835787E-07 ),
 .UNSPECIFIED. ) ;
#16586 = CARTESIAN_POINT ( 'NONE',  ( -6.895941952979999456, 1414.058355658300115, 207.6209997343590032 ) ) ;
#16587 = CARTESIAN_POINT ( 'NONE',  ( -113.4000000000000057, 1384.899971913130003, 304.2218459572590064 ) ) ;
#16588 = CARTESIAN_POINT ( 'NONE',  ( 3.702952669180000100, 1486.443463639589936, 198.8438389633990084 ) ) ;
#16589 = DIRECTION ( 'NONE',  ( -5.980589973904019347E-17, 1.000000000000000000, -1.736889445713099699E-16 ) ) ;
#16590 = CARTESIAN_POINT ( 'NONE',  ( -1.906499791370919845E-08, 1509.038615934239942, 213.6090957241370063 ) ) ;
#16591 = EDGE_CURVE ( 'NONE', #29937, #17762, #43985, .T. ) ;
#16593 = CARTESIAN_POINT ( 'NONE',  ( 37.55019124142308584, 1436.545190195376108, 135.0428483764136445 ) ) ;
#16592 = CARTESIAN_POINT ( 'NONE',  ( -3.255967424474999650, 1516.989560013210166, 214.1335248082570217 ) ) ;
#16594 = CARTESIAN_POINT ( 'NONE',  ( 20.01039973129999794, 1508.355603643830136, 189.0623068450979929 ) ) ;
#16595 = CARTESIAN_POINT ( 'NONE',  ( -1.600048698852036821, 1411.254281879943164, 135.5999999980979851 ) ) ;
#16596 = EDGE_LOOP ( 'NONE', ( #89325, #52739, #2134, #62792 ) ) ;
#16597 = CARTESIAN_POINT ( 'NONE',  ( -12.78776258870000149, 1416.851343894929869, 195.5391574245979882 ) ) ;
#16598 = CARTESIAN_POINT ( 'NONE',  ( -8.324962519149999840E-16, 1519.913060387329779, 209.1218459616979999 ) ) ;
#16599 = ORIENTED_EDGE ( 'NONE', *, *, #45206, .F. ) ;
#16600 = CARTESIAN_POINT ( 'NONE',  ( -16.47162245365960231, 1508.551704408389924, 213.2650820600849784 ) ) ;
#16601 = EDGE_CURVE ( 'NONE', #97770, #61519, #1071, .T. ) ;
#16602 = CARTESIAN_POINT ( 'NONE',  ( -114.8382766158126174, 1305.913060387289988, 306.8545936429301264 ) ) ;
#16603 = CARTESIAN_POINT ( 'NONE',  ( 2.389870119416070082, 1525.253996226948402, 176.1935146752628611 ) ) ;
#16604 = UNCERTAINTY_MEASURE_WITH_UNIT (LENGTH_MEASURE( 1.000000000000000082E-05 ), #86941, 'distance_accuracy_value', 'NONE');
#16605 = CARTESIAN_POINT ( 'NONE',  ( -8535.261851438322992, 2833.596074015641989, 11230.49242346659776 ) ) ;
#16606 = CARTESIAN_POINT ( 'NONE',  ( -11.37017053985569959, 1470.996082497490079, 208.1552749488289749 ) ) ;
#16607 = CARTESIAN_POINT ( 'NONE',  ( -4.317515543852133320, 1508.177212360263866, 220.5973697276004657 ) ) ;
#16608 = DIRECTION ( 'NONE',  ( 0.000000000000000000, 0.000000000000000000, 1.000000000000000000 ) ) ;
#16609 = CARTESIAN_POINT ( 'NONE',  ( -22.03465957474591619, 1522.382868172863937, 182.8300405912331144 ) ) ;
#16610 = CARTESIAN_POINT ( 'NONE',  ( 9.170460176685850229, 1461.406028138000238, 205.9602226471569963 ) ) ;
#16611 = CARTESIAN_POINT ( 'NONE',  ( -2.455820327400000114, 1434.541746329560056, 150.3615916412979914 ) ) ;
#16612 = CARTESIAN_POINT ( 'NONE',  ( 39.54663510683320027, 1440.913060369859977, 258.6366483742290256 ) ) ;
#16614 = CARTESIAN_POINT ( 'NONE',  ( 10.78159850099999950, 1461.896569178690015, 211.1674767183390031 ) ) ;
#16613 = CARTESIAN_POINT ( 'NONE',  ( -4.882940650389359760, 1421.798898707020044, 193.0164659316789937 ) ) ;
#16615 = CARTESIAN_POINT ( 'NONE',  ( 13.40566205799999899, 1429.098591196430107, 222.0107402513980333 ) ) ;
#16616 = ORIENTED_EDGE ( 'NONE', *, *, #40642, .F. ) ;
#16617 = ORIENTED_EDGE ( 'NONE', *, *, #21997, .F. ) ;
#16618 = CARTESIAN_POINT ( 'NONE',  ( 11.81780673814840021, 1517.051704408389924, 195.5270144474869767 ) ) ;
#16619 = EDGE_CURVE ( 'NONE', #48466, #59575, #29654, .T. ) ;
#16620 = DIRECTION ( 'NONE',  ( 0.000000000000000000, 1.000000000000000000, 0.000000000000000000 ) ) ;
#16621 = CARTESIAN_POINT ( 'NONE',  ( -24.41126182779999709, 1441.219864612629863, 212.0468573075179961 ) ) ;
#16622 = CARTESIAN_POINT ( 'NONE',  ( 1.703662692062522188, 1410.351485318999721, 185.3575011929372636 ) ) ;
#16623 = CARTESIAN_POINT ( 'NONE',  ( -3.612067548279275453, 1426.010407914519874, 185.9361413070191986 ) ) ;
#16624 = EDGE_CURVE ( 'NONE', #14981, #45960, #55249, .T. ) ;
#16625 = CARTESIAN_POINT ( 'NONE',  ( 9.368311761950069538, 1422.630913921370166, 212.8603802799670177 ) ) ;
#16626 = CARTESIAN_POINT ( 'NONE',  ( 2.724649121582150002, 1508.551704408389924, 219.4861637980260127 ) ) ;
#16627 = CARTESIAN_POINT ( 'NONE',  ( 2.740701793870000014, 1426.136123009330049, 188.7843822941989913 ) ) ;
#16628 = CARTESIAN_POINT ( 'NONE',  ( -70.66573123358719499, 1383.784603572710239, 295.5469044946160011 ) ) ;
#16629 = CARTESIAN_POINT ( 'NONE',  ( 10.80972683769999954, 1452.101161015629941, 151.9897701840980062 ) ) ;
#16630 = B_SPLINE_CURVE_WITH_KNOTS ( 'NONE', 3,
 ( #102469, #83465, #24640, #43142, #75100, #58838, #6760, #109248, #100812, #16247, #101910, #16788, #9521, #95191, #19005, #77841, #53778, #87346, #11202, #61076, #10076, #62169, #19575, #1150, #60505 ),
 .UNSPECIFIED., .F., .F.,
 ( 4, 3, 3, 3, 3, 3, 3, 3, 4 ),
 ( 0.000000000000000000, 0.9296916835059300110, 1.856438681794639889, 2.777847123387560124, 3.503639760140000003, 4.428889518077550491, 5.349465545739890082, 6.262071350648260371, 6.986073851990000527 ),
 .UNSPECIFIED. ) ;
#16631 = CARTESIAN_POINT ( 'NONE',  ( 4.789673499540000101, 1465.867933640490037, 219.0700355186390027 ) ) ;
#16632 = CARTESIAN_POINT ( 'NONE',  ( 31.23437356469434789, 1523.382868172864164, 195.3468678195113739 ) ) ;
#16634 = ORIENTED_EDGE ( 'NONE', *, *, #20132, .F. ) ;
#16633 = CARTESIAN_POINT ( 'NONE',  ( -0.07060758185340119952, 1456.122775716790102, 218.7382961870089844 ) ) ;
#16635 = CARTESIAN_POINT ( 'NONE',  ( 15.20184466319999927, 1507.442701412029919, 186.5339258382980177 ) ) ;
#16636 = B_SPLINE_CURVE_WITH_KNOTS ( 'NONE', 5,
 ( #49910, #84044, #75665, #14077, #6237, #33088 ),
 .UNSPECIFIED., .F., .F.,
 ( 6, 6 ),
 ( -93.34500910270000418, -16.36816738400000304 ),
 .UNSPECIFIED. ) ;
#16637 = CARTESIAN_POINT ( 'NONE',  ( -59.79588189159999700, 1380.471087561269997, 250.5313864223589917 ) ) ;
#16638 = CARTESIAN_POINT ( 'NONE',  ( 4.963083874980020127, 1508.551704408389924, 206.2781155379609856 ) ) ;
#16639 = ORIENTED_EDGE ( 'NONE', *, *, #12530, .F. ) ;
#16640 = ORIENTED_EDGE ( 'NONE', *, *, #4509, .F. ) ;
#16641 = CARTESIAN_POINT ( 'NONE',  ( 18.20120699554579957, 1508.790952174090080, 230.6639428141660346 ) ) ;
#16642 = CARTESIAN_POINT ( 'NONE',  ( -8.925728462962421617, 1385.954551176779887, 218.5383989427139966 ) ) ;
#16643 = DIRECTION ( 'NONE',  ( 0.000000000000000000, 0.000000000000000000, 1.000000000000000000 ) ) ;
#16645 = CARTESIAN_POINT ( 'NONE',  ( -0.7896334281179979708, 1469.097698168490069, 189.0743330492990140 ) ) ;
#16644 = DIRECTION ( 'NONE',  ( 0.9455185755993182894, 0.000000000000000000, -0.3255681544571521480 ) ) ;
#16646 = B_SPLINE_CURVE_WITH_KNOTS ( 'NONE', 3,
 ( #93401, #42450, #66588, #75530, #84459, #102352, #100691, #8288, #32939, #58169, #7207, #24528, #92851, #8838, #6646, #16127, #59827, #84993, #16666 ),
 .UNSPECIFIED., .F., .F.,
 ( 4, 2, 2, 2, 1, 1, 1, 1, 1, 2, 2, 4 ),
 ( 0.000000000000000000, 0.2500000000002616796, 0.3750000000003925194, 0.4375000000004576339, 0.4687500000004921619, 0.4843750000005068723, 0.4921875000005165868, 0.4960937500005219158, 0.4980468750005243583, 0.4990234375005250245, 0.5000000000005256906, 1.000000000000000000 ),
 .UNSPECIFIED. ) ;
#16647 = CARTESIAN_POINT ( 'NONE',  ( 11.59475102981150130, 1480.142125814169958, 211.2619558011750200 ) ) ;
#16648 = CARTESIAN_POINT ( 'NONE',  ( -109.7649665430000141, 1383.250791452569956, 297.1361542659589645 ) ) ;
#16649 = DIRECTION ( 'NONE',  ( -0.7384854939282339270, 8.827210057988519180E-16, 0.6742693640212139572 ) ) ;
#16650 = CARTESIAN_POINT ( 'NONE',  ( -11.21009720348472882, 1434.253606524949873, 151.6059541307748191 ) ) ;
#16651 = CARTESIAN_POINT ( 'NONE',  ( -3.387218493868067171, 1485.678307060469024, 182.9053799028293383 ) ) ;
#16652 = CARTESIAN_POINT ( 'NONE',  ( 4.382233832780000782, 1409.233371194429992, 186.7458337506980115 ) ) ;
#16653 = CARTESIAN_POINT ( 'NONE',  ( 4.519805968770000071, 1423.798844936530031, 183.7327313443980188 ) ) ;
#16654 = CARTESIAN_POINT ( 'NONE',  ( 2.454239291473280016, 1432.341654353290096, 200.8702472344759826 ) ) ;
#16655 = CARTESIAN_POINT ( 'NONE',  ( -2.500000010717490007, 1439.743081382919854, 158.2290103479810170 ) ) ;
#16656 = CARTESIAN_POINT ( 'NONE',  ( 11.73563886785350086, 1425.610159375979947, 144.1657481682890136 ) ) ;
#16657 = CARTESIAN_POINT ( 'NONE',  ( 0.5195835033840000561, 1465.018085799629944, 237.7479754663980032 ) ) ;
#16658 = EDGE_LOOP ( 'NONE', ( #19202, #82286, #24933, #70345, #95139 ) ) ;
#16659 = CARTESIAN_POINT ( 'NONE',  ( 11.10812020650000065, 1480.085810737090014, 229.8010407196990172 ) ) ;
#16660 = CARTESIAN_POINT ( 'NONE',  ( -1.116585105924089969E-07, 1397.914279478820163, 196.1218459578329885 ) ) ;
#16661 = CARTESIAN_POINT ( 'NONE',  ( -26.36916569686470169, 1446.546730999289821, 137.7167333428670020 ) ) ;
#16662 =( BOUNDED_SURFACE ( )  B_SPLINE_SURFACE ( 3, 2, ( 
 ( #71711, #12290, #29107 ),
 ( #97408, #54878, #89003 ),
 ( #80616, #6102, #57088 ),
 ( #48126, #108006, #91758 ),
 ( #99596, #23450, #91212 ),
 ( #74439, #57645, #40257 ) ),
 .UNSPECIFIED., .F., .F., .T. ) 
 B_SPLINE_SURFACE_WITH_KNOTS ( ( 4, 2, 4 ),
 ( 3, 3 ),
 ( -3.642919299551294898E-17, 0.001312027981647369626, 0.002624055963294775681 ),
 ( 0.000000000000000000, 1.000000000000000000 ),
 .UNSPECIFIED. ) 
 GEOMETRIC_REPRESENTATION_ITEM ( )  RATIONAL_B_SPLINE_SURFACE ( (
 ( 1.000000000000000000, 0.9376006582765852304, 1.000000000000000000),
 ( 1.000000000000000000, 0.9569320108022569826, 1.000000000000000000),
 ( 1.000000000000000000, 0.9725743441618890373, 1.000000000000000000),
 ( 1.000000000000000000, 0.9942095667135610881, 1.000000000000000000),
 ( 1.000000000000000000, 1.000043666450710411, 1.000000000000000000),
 ( 1.000000000000000000, 1.000000000000000000, 1.000000000000000000) ) ) 
 REPRESENTATION_ITEM ( '' )  SURFACE ( )  );
#16663 = LINE ( 'NONE', #84456, #41463 ) ;
#16664 = CARTESIAN_POINT ( 'NONE',  ( -6.402980167960000024, 1474.343588456390080, 205.7752103392290337 ) ) ;
#16665 = CARTESIAN_POINT ( 'NONE',  ( -1.163550753797859917E-08, 1474.117094278439936, 263.5999159951250022 ) ) ;
#16666 = CARTESIAN_POINT ( 'NONE',  ( 25.00977876991279913, 1436.598012848749931, 137.9330263815630246 ) ) ;
#16667 = CARTESIAN_POINT ( 'NONE',  ( -2.168811436099340018, 1421.535665163839894, 193.6021455940999942 ) ) ;
#16668 = CARTESIAN_POINT ( 'NONE',  ( -1.347852712580000167, 1417.336052002229962, 235.7060345899980121 ) ) ;
#16669 = CARTESIAN_POINT ( 'NONE',  ( -0.7261436049189990971, 1476.159678178889862, 198.3924679319989934 ) ) ;
#16670 = CARTESIAN_POINT ( 'NONE',  ( -105.6600088659999983, 1389.882499440619995, 307.5167961107590031 ) ) ;
#16671 = CARTESIAN_POINT ( 'NONE',  ( -7.550412427349730393, 1510.476657126699820, 214.6722958288490020 ) ) ;
#16672 = CARTESIAN_POINT ( 'NONE',  ( 3.745961299822565760, 1358.679437168825416, 209.6218459617033432 ) ) ;
#16673 = CARTESIAN_POINT ( 'NONE',  ( -46.11540523431960281, 1439.221583252120126, 266.9731953717790134 ) ) ;
#16674 = CARTESIAN_POINT ( 'NONE',  ( 1.635180021967760133, 1429.354063412989944, 217.2616352817560141 ) ) ;
#16675 = CARTESIAN_POINT ( 'NONE',  ( -8.133195396499999674, 1425.296577659349850, 209.0165728948540220 ) ) ;
#16676 = AXIS2_PLACEMENT_3D ( 'NONE', #93761, #26575, #43401 ) ;
#16677 = VERTEX_POINT ( 'NONE', #62217 ) ;
#16678 = CARTESIAN_POINT ( 'NONE',  ( -4.618583430005000601, 1516.939762005280045, 209.1349059721700030 ) ) ;
#16679 = EDGE_CURVE ( 'NONE', #61380, #54399, #87363, .T. ) ;
#16680 = DIRECTION ( 'NONE',  ( 5.980589973904019347E-17, -1.000000000000000000, 1.736889445713099699E-16 ) ) ;
#16681 = CARTESIAN_POINT ( 'NONE',  ( -6.915664125854886990, 1471.020592902175622, 216.5103502196423051 ) ) ;
#16682 = CARTESIAN_POINT ( 'NONE',  ( 7.539441653064500315, 1425.666433134689896, 212.1875851909779840 ) ) ;
#16683 = CARTESIAN_POINT ( 'NONE',  ( -26.75564819202289968, 1450.885958589989968, 136.4275090895790186 ) ) ;
#16684 = ORIENTED_EDGE ( 'NONE', *, *, #20788, .T. ) ;
#16685 = CARTESIAN_POINT ( 'NONE',  ( 21.16722375039999804, 1430.152617814430187, 217.2719924742480089 ) ) ;
#16687 = CARTESIAN_POINT ( 'NONE',  ( -15.29490965391659962, 1512.594488815719842, 222.4682760166489857 ) ) ;
#16686 = CARTESIAN_POINT ( 'NONE',  ( -11.03241518813069888, 1492.218220261629995, 207.1401972973099816 ) ) ;
#16688 = CARTESIAN_POINT ( 'NONE',  ( 14.45760366715495593, 1416.831922878981004, 196.8518846270366396 ) ) ;
#16689 = CARTESIAN_POINT ( 'NONE',  ( -7.240818526079999984, 1422.864346058830051, 211.7372259730379938 ) ) ;
#16690 = CARTESIAN_POINT ( 'NONE',  ( 7.998636686930000295, 1425.977676336709919, 211.5360327896089814 ) ) ;
#16691 = EDGE_CURVE ( 'NONE', #45174, #13629, #91317, .T. ) ;
#16692 = CYLINDRICAL_SURFACE ( 'NONE', #53448, 2.000000000000003553 ) ;
#16693 = CARTESIAN_POINT ( 'NONE',  ( -17.40764085468179800, 1414.996442620800053, 207.5654756526599840 ) ) ;
#16694 = ORIENTED_EDGE ( 'NONE', *, *, #63923, .F. ) ;
#16695 = CARTESIAN_POINT ( 'NONE',  ( -6.760649935883880524, 1408.923413865439898, 270.4241599285139728 ) ) ;
#16696 = CARTESIAN_POINT ( 'NONE',  ( 4.766109705707320288, 1416.570715930979986, 231.5949414777570041 ) ) ;
#16697 = CARTESIAN_POINT ( 'NONE',  ( 8.602846452805209765, 1434.993060077820019, 206.5683719099479845 ) ) ;
#16698 = EDGE_LOOP ( 'NONE', ( #91172, #53618, #74611, #81134 ) ) ;
#16699 = ORIENTED_EDGE ( 'NONE', *, *, #72771, .T. ) ;
#16700 = LINE ( 'NONE', #95655, #54588 ) ;
#16701 = LINE ( 'NONE', #50901, #96737 ) ;
#16702 = CARTESIAN_POINT ( 'NONE',  ( -109.9849858529770046, 1384.909542710179949, 311.4561255368179786 ) ) ;
#16703 = CARTESIAN_POINT ( 'NONE',  ( -7.097634907420000694, 1427.571433844230114, 133.6118001900980232 ) ) ;
#16704 = CARTESIAN_POINT ( 'NONE',  ( -19.47585981394729870, 1458.049649394619792, 193.7545121080359820 ) ) ;
#16705 = CARTESIAN_POINT ( 'NONE',  ( -17.66551749759999979, 1410.882307517030085, 225.3279256837980142 ) ) ;
#16706 = CARTESIAN_POINT ( 'NONE',  ( 33.13841419969649849, 1465.588173225519995, 268.0170166519210397 ) ) ;
#16707 = CARTESIAN_POINT ( 'NONE',  ( -3.910140144818339714, 1508.551704408389924, 204.2884083085430120 ) ) ;
#16708 = CARTESIAN_POINT ( 'NONE',  ( -6.054480185420000993, 1427.105311845340111, 201.8413580458289971 ) ) ;
#16709 = CARTESIAN_POINT ( 'NONE',  ( 2.865588684285000021, 1516.890356958860139, 205.8536102114670143 ) ) ;
#16710 = VERTEX_POINT ( 'NONE', #1757 ) ;
#16711 = CARTESIAN_POINT ( 'NONE',  ( 18.94699345070725016, 1457.564172839218827, 226.7977625303617515 ) ) ;
#16712 = CARTESIAN_POINT ( 'NONE',  ( -1.379923010975170117, 1444.345884097049975, 199.1632244479729934 ) ) ;
#16713 = CARTESIAN_POINT ( 'NONE',  ( 11.18076303840565977, 1517.151704408390060, 204.2578997804941707 ) ) ;
#16714 = ORIENTED_EDGE ( 'NONE', *, *, #51368, .T. ) ;
#16715 = CARTESIAN_POINT ( 'NONE',  ( -22.96901158596647008, 1517.151704408390060, 211.6943887467578236 ) ) ;
#16716 = ADVANCED_FACE ( 'NONE', ( #96344 ), #22516, .F. ) ;
#16717 = CARTESIAN_POINT ( 'NONE',  ( 27.03067664649999813, 1451.714498883330180, 135.7945611549980072 ) ) ;
#16718 = CARTESIAN_POINT ( 'NONE',  ( -4.865329319845380418, 1508.551704408389924, 212.3847752591109668 ) ) ;
#16719 = CARTESIAN_POINT ( 'NONE',  ( -13.60512064039999913, 1388.590188594380152, 217.4599908286989773 ) ) ;
#16720 = ADVANCED_FACE ( 'NONE', ( #79016 ), #104740, .F. ) ;
#16721 = CARTESIAN_POINT ( 'NONE',  ( 7.706547837850000526, 1421.685151551939953, 195.7783216092990131 ) ) ;
#16722 = CARTESIAN_POINT ( 'NONE',  ( -2.162991289744210288, 1432.744035697870004, 218.4013281355300080 ) ) ;
#16723 = DIRECTION ( 'NONE',  ( 0.9235695684098328417, -0.3795957984897049275, 0.05409512063244299035 ) ) ;
#16724 = CARTESIAN_POINT ( 'NONE',  ( 1.854665035029979814, 1408.977826717500193, 186.8880553776029956 ) ) ;
#16725 = CARTESIAN_POINT ( 'NONE',  ( 3.892685920875734951, 1515.551704408391060, 210.6723607687643494 ) ) ;
#16726 = FACE_OUTER_BOUND ( 'NONE', #41781, .T. ) ;
#16727 = ADVANCED_FACE ( 'NONE', ( #18504 ), #52701, .F. ) ;
#16728 = CARTESIAN_POINT ( 'NONE',  ( -12.53694325390000053, 1380.612673806029761, 215.4769779826689842 ) ) ;
#16729 = CARTESIAN_POINT ( 'NONE',  ( 2.136371660471265255, 1525.856064936157281, 241.3693953963658316 ) ) ;
#16730 = VERTEX_POINT ( 'NONE', #2316 ) ;
#16731 = CARTESIAN_POINT ( 'NONE',  ( 11.74432248201719986, 1415.089118586279938, 221.6914046880520175 ) ) ;
#16732 = CARTESIAN_POINT ( 'NONE',  ( 11.19478300405899951, 1432.344513976420103, 151.5793324132870055 ) ) ;
#16733 = CARTESIAN_POINT ( 'NONE',  ( -11.41675697748640061, 1482.775670443970057, 205.7339590229720159 ) ) ;
#16734 = ADVANCED_FACE ( 'NONE', ( #648 ), #87399, .F. ) ;
#16735 = CARTESIAN_POINT ( 'NONE',  ( -13.72145621289999973, 1390.430903341090016, 208.3849667214680039 ) ) ;
#16736 = LINE ( 'NONE', #50943, #45609 ) ;
#16737 = CARTESIAN_POINT ( 'NONE',  ( 0.6988675025901418536, 1421.239614905253347, 193.7316982519299131 ) ) ;
#16738 = CARTESIAN_POINT ( 'NONE',  ( -10.96494705889580068, 1462.661034221799810, 207.7545830336519828 ) ) ;
#16739 = CARTESIAN_POINT ( 'NONE',  ( -0.8167354255590000278, 1432.353341358199941, 150.3995506339979897 ) ) ;
#16740 = DIRECTION ( 'NONE',  ( -0.9417419115949662300, -0.2378257470769920556, 0.2378257470769920556 ) ) ;
#16741 = CARTESIAN_POINT ( 'NONE',  ( 11.23711414429999955, 1433.375750033149870, 151.5590630604979765 ) ) ;
#16742 = CARTESIAN_POINT ( 'NONE',  ( 5.969073325650000150, 1453.512197679029896, 209.1218459616979999 ) ) ;
#16743 = CARTESIAN_POINT ( 'NONE',  ( 12.87305953246699985, 1416.529254608160045, 196.3216546659990058 ) ) ;
#16744 = B_SPLINE_CURVE_WITH_KNOTS ( 'NONE', 3,
 ( #50683, #67506, #101610, #84815 ),
 .UNSPECIFIED., .F., .F.,
 ( 4, 4 ),
 ( 0.000000000000000000, 1.000000000000000000 ),
 .UNSPECIFIED. ) ;
#16745 = CARTESIAN_POINT ( 'NONE',  ( -12.28855869350000063, 1378.253616442990051, 210.0769077263690008 ) ) ;
#16746 = CARTESIAN_POINT ( 'NONE',  ( 11.17229582740980121, 1425.728672638270154, 197.4068991129149993 ) ) ;
#16747 = VECTOR ( 'NONE', #34632, 1000.000000000000000 ) ;
#16748 = CARTESIAN_POINT ( 'NONE',  ( 7.590528390105199641, 1465.207167611649993, 215.7443336111830092 ) ) ;
#16749 = CARTESIAN_POINT ( 'NONE',  ( -10.06499177390000099, 1481.481388711089949, 205.8730018957789980 ) ) ;
#16750 = CARTESIAN_POINT ( 'NONE',  ( 12.87601703102835593, 1398.294686622125255, 207.2957931138314507 ) ) ;
#16751 = CARTESIAN_POINT ( 'NONE',  ( -27.67723492755769854, 1509.879570728590124, 222.2494832413370034 ) ) ;
#16752 = EDGE_CURVE ( 'NONE', #73277, #33349, #10129, .T. ) ;
#16753 = CARTESIAN_POINT ( 'NONE',  ( -7.749759000068385362, 1426.484231355699649, 206.4869615271631460 ) ) ;
#16754 = AXIS2_PLACEMENT_3D ( 'NONE', #109716, #58769, #41963 ) ;
#16755 = CARTESIAN_POINT ( 'NONE',  ( 1.770954783930000165, 1478.892269184689894, 229.4302748609989919 ) ) ;
#16756 = DIRECTION ( 'NONE',  ( 0.9942586961433742543, 0.000000000000000000, -0.1070030146457445069 ) ) ;
#16757 = CARTESIAN_POINT ( 'NONE',  ( -12.66789338582930036, 1383.860718371299981, 218.8636147899300113 ) ) ;
#16758 = CARTESIAN_POINT ( 'NONE',  ( -4.994371530956574823, 1391.698117826116459, 203.8075142969990168 ) ) ;
#16759 = CARTESIAN_POINT ( 'NONE',  ( -18.65941878286419708, 1468.219764057670091, 201.0822022773610058 ) ) ;
#16760 = EDGE_CURVE ( 'NONE', #61195, #41530, #27473, .T. ) ;
#16761 = CARTESIAN_POINT ( 'NONE',  ( -2.866857931135000204, 1516.951766529250108, 213.1652121904069759 ) ) ;
#16762 = CARTESIAN_POINT ( 'NONE',  ( -16.30825986473579903, 1420.539997913489970, 204.8045917016430053 ) ) ;
#16763 = CARTESIAN_POINT ( 'NONE',  ( 0.1717492930638790105, 1479.302881201929949, 182.1243356784760010 ) ) ;
#16765 = EDGE_LOOP ( 'NONE', ( #8630, #25565, #93984, #90565, #81327 ) ) ;
#16764 = CARTESIAN_POINT ( 'NONE',  ( -2.983724533230000198, 1408.833818059829809, 223.1998287106980001 ) ) ;
#16766 = CARTESIAN_POINT ( 'NONE',  ( -13.59716640859999970, 1444.740067931808653, 176.5566119326980754 ) ) ;
#16767 = DIRECTION ( 'NONE',  ( 0.000000000000000000, -0.9990482215818579093, 0.04361938736533144123 ) ) ;
#16768 = CARTESIAN_POINT ( 'NONE',  ( 12.91279240200000089, 1434.774393157829991, 149.9807649658980040 ) ) ;
#16769 = CARTESIAN_POINT ( 'NONE',  ( -40.71250048055519954, 1447.497876395859976, 134.0999999984609872 ) ) ;
#16770 = CARTESIAN_POINT ( 'NONE',  ( -109.7185680580000025, 1384.890266421910155, 297.0862365493590005 ) ) ;
#16771 = ORIENTED_EDGE ( 'NONE', *, *, #102365, .T. ) ;
#16772 = B_SPLINE_SURFACE_WITH_KNOTS ( 'NONE', 5, 1, ( 
 ( #92225, #108482 ),
 ( #7123, #75453 ),
 ( #84911, #84379 ),
 ( #109045, #110130 ),
 ( #16582, #15496 ),
 ( #49694, #67050 ) ),
 .UNSPECIFIED., .F., .F., .F.,
 ( 6, 6 ),
 ( 2, 2 ),
 ( 0.000000000000000000, 3.826360078679999610 ),
 ( 0.000000000000000000, 14.00000000000000000 ),
 .UNSPECIFIED. ) ;
#16773 = CARTESIAN_POINT ( 'NONE',  ( -38.64592363268830155, 1443.862568456279860, 137.1880729353390223 ) ) ;
#16774 = DIRECTION ( 'NONE',  ( 0.000000000000000000, 1.000000000000000000, 0.000000000000000000 ) ) ;
#16775 = CARTESIAN_POINT ( 'NONE',  ( -16.64491379450000252, 1416.823872462229929, 216.8740446600579901 ) ) ;
#16776 = DIRECTION ( 'NONE',  ( 0.000000000000000000, 1.000000000000000000, 0.000000000000000000 ) ) ;
#16777 = CARTESIAN_POINT ( 'NONE',  ( -5.888139897268749756, 1434.739753164839840, 216.8789263783159811 ) ) ;
#16778 = CARTESIAN_POINT ( 'NONE',  ( -13.62020111877600215, 1443.814707039050063, 195.1253454527559938 ) ) ;
#16779 = CARTESIAN_POINT ( 'NONE',  ( -16.24206877649999825, 1420.056535900020208, 209.7634690437569986 ) ) ;
#16780 = CARTESIAN_POINT ( 'NONE',  ( -113.4000000000000057, 1375.913060387289988, 304.2218459572590064 ) ) ;
#16781 = CARTESIAN_POINT ( 'NONE',  ( -12.11669130219999957, 1391.856317166560075, 209.2336078948329998 ) ) ;
#16782 = CARTESIAN_POINT ( 'NONE',  ( -85.14792482515179017, 1385.176708844659743, 288.8829841967900052 ) ) ;
#16783 = MECHANICAL_DESIGN_GEOMETRIC_PRESENTATION_REPRESENTATION (  '', ( #102645 ), #93697 ) ;
#16784 = CARTESIAN_POINT ( 'NONE',  ( -17.89234610336693265, 1523.611961620354123, 237.9279674222335359 ) ) ;
#16785 = CARTESIAN_POINT ( 'NONE',  ( 10.26114059010819979, 1426.067723122690040, 208.3384717249140010 ) ) ;
#16786 = VERTEX_POINT ( 'NONE', #77890 ) ;
#16787 = CARTESIAN_POINT ( 'NONE',  ( -29.82725620059999727, 1451.718533343729860, 135.7071959994979977 ) ) ;
#16789 = ORIENTED_EDGE ( 'NONE', *, *, #62096, .T. ) ;
#16788 = CARTESIAN_POINT ( 'NONE',  ( 0.08317272321623850329, 1437.870240068480143, 227.6823673113509869 ) ) ;
#16790 = CARTESIAN_POINT ( 'NONE',  ( 1.617203238019999878, 1473.963834990890064, 219.3699067192990242 ) ) ;
#16791 = CARTESIAN_POINT ( 'NONE',  ( 22.59263393849999702, 1509.026251551730184, 224.5515445014980003 ) ) ;
#16792 = CARTESIAN_POINT ( 'NONE',  ( -8.538839991170000587, 1362.569232148550100, 207.6218459616989946 ) ) ;
#16793 = CARTESIAN_POINT ( 'NONE',  ( -8.009280784559999589, 1493.871781897389837, 199.6961107241290279 ) ) ;
#16794 = CARTESIAN_POINT ( 'NONE',  ( 42.06232107018946920, 1441.883906795105304, 269.6487541092193396 ) ) ;
#16795 = CARTESIAN_POINT ( 'NONE',  ( -4.097009089535903037, 1512.187213306747481, 201.1608118946569448 ) ) ;
#16796 = CARTESIAN_POINT ( 'NONE',  ( 14.95071165534215929, 1430.594940584589040, 220.1523712821232550 ) ) ;
#16797 = CARTESIAN_POINT ( 'NONE',  ( 1778.930368298719941, -2340.220200558880151, -8899.082583863100808 ) ) ;
#16798 = CARTESIAN_POINT ( 'NONE',  ( 8.992866426550000014, 1449.909640413290163, 206.9381849123989809 ) ) ;
#16799 = LINE ( 'NONE', #77311, #109207 ) ;
#16800 = B_SPLINE_CURVE_WITH_KNOTS ( 'NONE', 3,
 ( #100111, #61326, #74931, #40204, #74386, #31799, #23392, #103259, #57582, #83308 ),
 .UNSPECIFIED., .F., .F.,
 ( 4, 2, 2, 2, 4 ),
 ( 0.000000000000000000, 0.2500000000000000000, 0.5000000000000000000, 0.7500000000000000000, 1.000000000000000000 ),
 .UNSPECIFIED. ) ;
#16801 = CARTESIAN_POINT ( 'NONE',  ( -4.517103279549999684, 1368.953374755989898, 207.6218459616989946 ) ) ;
#16802 = CARTESIAN_POINT ( 'NONE',  ( -29.71163624023675354, 1526.333389947989644, 217.1029916164691826 ) ) ;
#16803 = CARTESIAN_POINT ( 'NONE',  ( 1.118903270415000151, 1517.003078582959688, 206.2405205581369785 ) ) ;
#16804 = CARTESIAN_POINT ( 'NONE',  ( 2.500000000000000000, 1448.685390747959900, 157.9322671792980088 ) ) ;
#16805 = B_SPLINE_SURFACE_WITH_KNOTS ( 'NONE', 5, 5, ( 
 ( #49278, #31351, #75589, #65535, #109720, #16184 ),
 ( #83407, #66643, #22932, #14543, #82314, #6702 ),
 ( #40305, #100744, #24029, #110261, #82858, #58228 ),
 ( #39765, #74488, #101846, #108615, #6148, #7802 ),
 ( #41968, #33537, #31904, #67737, #59343, #93452 ),
 ( #69401, #36316, #1637, #94012, #35775, #50925 ),
 ( #2202, #42508, #538, #62107, #69957, #78325 ),
 ( #8344, #18947, #85599, #27366, #102409, #8900 ),
 ( #110818, #10015, #70513, #43077, #17276, #34110 ) ),
 .UNSPECIFIED., .F., .F., .F.,
 ( 6, 3, 6 ),
 ( 6, 6 ),
 ( 21.89878892990000026, 23.58501803260000074, 25.27124713539999945 ),
 ( 0.000000000000000000, 2.000000000000000000 ),
 .UNSPECIFIED. ) ;
#16806 = FACE_OUTER_BOUND ( 'NONE', #19261, .T. ) ;
#16807 = CARTESIAN_POINT ( 'NONE',  ( -2.228719191530000199, 1497.815835837290024, 198.0391072666990055 ) ) ;
#16809 = ORIENTED_EDGE ( 'NONE', *, *, #104233, .F. ) ;
#16808 = CARTESIAN_POINT ( 'NONE',  ( -68.53362818316249161, 1379.747368904349969, 280.1371498460779321 ) ) ;
#16810 = B_SPLINE_CURVE_WITH_KNOTS ( 'NONE', 5,
 ( #13312, #106836, #14973, #5492, #22258, #56457, #72713, #48620, #90592 ),
 .UNSPECIFIED., .F., .F.,
 ( 6, 3, 6 ),
 ( 0.000000000000000000, 0.4368039669223903743, 1.000000000000000000 ),
 .UNSPECIFIED. ) ;
#16811 = B_SPLINE_CURVE_WITH_KNOTS ( 'NONE', 3,
 ( #34555, #17722, #17163, #26136, #77130, #9906, #2090, #35658, #52484, #18840 ),
 .UNSPECIFIED., .F., .F.,
 ( 4, 2, 2, 2, 4 ),
 ( 0.000000000000000000, 0.2500000000000000000, 0.5000000000000000000, 0.7500000000000000000, 1.000000000000000000 ),
 .UNSPECIFIED. ) ;
#16812 = DIRECTION ( 'NONE',  ( 1.755985294532464991E-16, -1.000000000000000000, 1.338183447452830017E-16 ) ) ;
#16813 = ORIENTED_EDGE ( 'NONE', *, *, #102204, .F. ) ;
#16814 = CARTESIAN_POINT ( 'NONE',  ( -16.26362611520470836, 1514.552098283620808, 223.8986760177197368 ) ) ;
#16815 = CARTESIAN_POINT ( 'NONE',  ( -19.06924802629999860, 1449.793579044900071, 193.8241538110980287 ) ) ;
#16817 = CARTESIAN_POINT ( 'NONE',  ( 17.30265999255270160, 1410.882230744779918, 192.3281541713860179 ) ) ;
#16816 = CARTESIAN_POINT ( 'NONE',  ( -11.42633400283000000, 1426.449296649120015, 121.9050361278559933 ) ) ;
#16818 = CARTESIAN_POINT ( 'NONE',  ( -0.7350232362959980836, 1516.970035769810011, 211.4194755912870107 ) ) ;
#16819 = CARTESIAN_POINT ( 'NONE',  ( 28.29401033920189334, 1510.012592320659451, 219.1028198056735050 ) ) ;
#16820 = FACE_OUTER_BOUND ( 'NONE', #102866, .T. ) ;
#16821 = CARTESIAN_POINT ( 'NONE',  ( 16.87646696224889808, 1509.508879493530003, 233.2953025406949905 ) ) ;
#16822 = CARTESIAN_POINT ( 'NONE',  ( 10.91472019480807099, 1464.331604664801262, 232.0109029648223498 ) ) ;
#16823 = ITEM_DEFINED_TRANSFORMATION ( 'NONE', 'NONE', #107571,  #21632 ) ;
#16824 = CARTESIAN_POINT ( 'NONE',  ( -4.993299342540000296, 1391.657172602489936, 214.7214461112690174 ) ) ;
#16825 = CARTESIAN_POINT ( 'NONE',  ( -36.67418371293260293, 1437.731587266990118, 136.5491800809179779 ) ) ;
#16826 = ORIENTED_EDGE ( 'NONE', *, *, #62279, .F. ) ;
#16827 = CARTESIAN_POINT ( 'NONE',  ( 6.518255528160000090, 1396.140682886129980, 199.2813087664480065 ) ) ;
#16828 = CARTESIAN_POINT ( 'NONE',  ( 9.742380785638999896, 1461.526748617359999, 207.6421447878750257 ) ) ;
#16829 = CARTESIAN_POINT ( 'NONE',  ( -17.49295792170000041, 1458.163342941830024, 229.7618723593980121 ) ) ;
#16830 = ORIENTED_EDGE ( 'NONE', *, *, #40626, .F. ) ;
#16831 = ORIENTED_EDGE ( 'NONE', *, *, #65048, .F. ) ;
#16832 = CIRCLE ( 'NONE', #22198, 1.999999999999998668 ) ;
#16833 = CARTESIAN_POINT ( 'NONE',  ( 16.27717394516742644, 1410.853839490788232, 226.7437855747935771 ) ) ;
#16834 = CARTESIAN_POINT ( 'NONE',  ( 10.13545575494789830, 1453.511789163979984, 212.2748783515349942 ) ) ;
#16835 = B_SPLINE_CURVE_WITH_KNOTS ( 'NONE', 3,
 ( #43111, #94044, #110299, #26853, #35251, #50961, #101880, #34694, #61041, #94592 ),
 .UNSPECIFIED., .F., .F.,
 ( 4, 2, 2, 2, 4 ),
 ( 0.000000000000000000, 0.2500000000000000000, 0.5000000000000000000, 0.7500000000000000000, 1.000000000000000000 ),
 .UNSPECIFIED. ) ;
#16836 = CARTESIAN_POINT ( 'NONE',  ( 16.66231036550703593, 1523.604703353109699, 180.4882076302513099 ) ) ;
#16837 = CARTESIAN_POINT ( 'NONE',  ( -12.16875361000624345, 1417.446348406323750, 199.6775038949584768 ) ) ;
#16838 = CARTESIAN_POINT ( 'NONE',  ( 4.138993644619999301, 1515.551749209489799, 209.1218459616910081 ) ) ;
#16839 = CIRCLE ( 'NONE', #79472, 2.000000000000001776 ) ;
#16840 = CARTESIAN_POINT ( 'NONE',  ( -6.679608332860329512, 1453.902887168129837, 202.5437545341480075 ) ) ;
#16841 = CARTESIAN_POINT ( 'NONE',  ( -6.546422875089999316, 1461.189193418830200, 233.6698635447980053 ) ) ;
#16842 = CARTESIAN_POINT ( 'NONE',  ( 19.25375188179999952, 1464.258769156330118, 224.0689215379980226 ) ) ;
#16843 = CARTESIAN_POINT ( 'NONE',  ( 9.703365291897300793, 1451.752702013299995, 208.6594554766439842 ) ) ;
#16844 = CARTESIAN_POINT ( 'NONE',  ( 33.43619682799734250, 1442.831169986189025, 154.5918098732002477 ) ) ;
#16845 = CARTESIAN_POINT ( 'NONE',  ( -100.7279122188340068, 1384.876502697709839, 296.3975145639699349 ) ) ;
#16846 = ORIENTED_EDGE ( 'NONE', *, *, #87030, .F. ) ;
#16847 = CARTESIAN_POINT ( 'NONE',  ( 3.259729297834999873, 1517.119374999550018, 201.7846921639870175 ) ) ;
#16848 = CARTESIAN_POINT ( 'NONE',  ( 2.297629621054999571, 1516.970035769810011, 209.8568691683980205 ) ) ;
#16849 = ORIENTED_EDGE ( 'NONE', *, *, #105647, .F. ) ;
#16850 = DIRECTION ( 'NONE',  ( 0.000000000000000000, 0.000000000000000000, -1.000000000000000000 ) ) ;
#16851 = CARTESIAN_POINT ( 'NONE',  ( 4.993685203717481258, 1511.399999645683920, 217.6426921449797476 ) ) ;
#16852 = ORIENTED_EDGE ( 'NONE', *, *, #46636, .F. ) ;
#16853 = CARTESIAN_POINT ( 'NONE',  ( -14.34604702270000054, 1416.547221147930031, 221.5678632711980072 ) ) ;
#16854 = EDGE_CURVE ( 'NONE', #18098, #98801, #2854, .T. ) ;
#16855 = CARTESIAN_POINT ( 'NONE',  ( -12.94068535313328816, 1442.831169986190844, 169.4787936161724531 ) ) ;
#16856 = CARTESIAN_POINT ( 'NONE',  ( 2.918143513847768445E-16, 1426.814114634534008, 137.0999999980979851 ) ) ;
#16857 = CARTESIAN_POINT ( 'NONE',  ( -7.121746155459253380, 1489.817813860794558, 217.4260952101665225 ) ) ;
#16858 = CARTESIAN_POINT ( 'NONE',  ( -4.649632428550000363, 1420.176632528429991, 186.4708458343980055 ) ) ;
#16859 = CARTESIAN_POINT ( 'NONE',  ( 9.951576027860420837, 1468.973797990169942, 207.5249271240780047 ) ) ;
#16861 = B_SPLINE_CURVE_WITH_KNOTS ( 'NONE', 5,
 ( #25878, #94194, #51665, #7443, #41607, #101477, #24764, #50564, #84690 ),
 .UNSPECIFIED., .F., .F.,
 ( 6, 3, 6 ),
 ( 0.000000000000000000, 0.3017171891571077680, 1.000000000000000000 ),
 .UNSPECIFIED. ) ;
#16860 = CARTESIAN_POINT ( 'NONE',  ( -10.75661188380004418, 1470.034926440792788, 212.8112178691188490 ) ) ;
#16862 = CARTESIAN_POINT ( 'NONE',  ( 5.551014600700000301, 1493.954207117990109, 218.9115156736490064 ) ) ;
#16863 = CARTESIAN_POINT ( 'NONE',  ( -62.89799739219998997, 1379.732086956869807, 267.9971866538590461 ) ) ;
#16864 = CYLINDRICAL_SURFACE ( 'NONE', #71478, 0.5000000000000022204 ) ;
#16866 = CARTESIAN_POINT ( 'NONE',  ( 8.171970832046620004, 1468.167223887809996, 201.4642853819800052 ) ) ;
#16865 = CARTESIAN_POINT ( 'NONE',  ( 18.22874257970000400, 1457.634144810630005, 229.9687939399979939 ) ) ;
#16867 = CARTESIAN_POINT ( 'NONE',  ( -4.921467313154969325, 1423.360444961196208, 184.6901157546226671 ) ) ;
#16868 = CARTESIAN_POINT ( 'NONE',  ( -5.690944892507480368, 1423.249492944180020, 98.05123491677301217 ) ) ;
#16869 = ORIENTED_EDGE ( 'NONE', *, *, #91388, .F. ) ;
#16870 = CARTESIAN_POINT ( 'NONE',  ( 18.15379326206519650, 1424.500835680889850, 223.9151983833729957 ) ) ;
#16871 = EDGE_CURVE ( 'NONE', #79128, #76640, #40892, .T. ) ;
#16872 = CARTESIAN_POINT ( 'NONE',  ( -21.59932114087497013, 1525.137906803776787, 233.5034269868583294 ) ) ;
#16873 = CARTESIAN_POINT ( 'NONE',  ( -2.911525634509525950, 1484.758356318058532, 183.2323580766349096 ) ) ;
#16874 = CARTESIAN_POINT ( 'NONE',  ( -14.77492446850000007, 1416.181292664740113, 213.5220302499890010 ) ) ;
#16875 = VECTOR ( 'NONE', #97192, 1000.000000000000114 ) ;
#16877 = ORIENTED_EDGE ( 'NONE', *, *, #74029, .F. ) ;
#16876 = CARTESIAN_POINT ( 'NONE',  ( 3.958629193967660331, 1508.551704408389924, 214.1089270130739806 ) ) ;
#16878 = CARTESIAN_POINT ( 'NONE',  ( 0.9116193683959998850, 1471.312091221629998, 187.8213723156979995 ) ) ;
#16879 = CARTESIAN_POINT ( 'NONE',  ( -0.3666539600740010285, 1508.474565598290155, 220.5579631546989958 ) ) ;
#16880 = EDGE_CURVE ( 'NONE', #74855, #52007, #11218, .T. ) ;
#16881 = CARTESIAN_POINT ( 'NONE',  ( -10.90096434610000031, 1427.628183919430057, 150.0868075714980137 ) ) ;
#16882 = CARTESIAN_POINT ( 'NONE',  ( 1.547463896846929865, 1414.913060387349788, 192.3096116128920130 ) ) ;
#16883 = CARTESIAN_POINT ( 'NONE',  ( -7.472928504960000495, 1442.056855012459891, 184.7838669167980186 ) ) ;
#16884 = CARTESIAN_POINT ( 'NONE',  ( 27.01620368378947035, 1451.969623355777230, 135.0020654903796640 ) ) ;
#16885 = CARTESIAN_POINT ( 'NONE',  ( 3.555115653736739510E-15, 1384.926148861439970, 209.1218459572589836 ) ) ;
#16886 = DIRECTION ( 'NONE',  ( 0.0002641870098999210353, 0.9990417697183311407, 0.04376611204218300993 ) ) ;
#16888 = CARTESIAN_POINT ( 'NONE',  ( -11.60387529539999996, 1481.105535806189891, 211.4044418315190228 ) ) ;
#16887 = CARTESIAN_POINT ( 'NONE',  ( -20.21775582709999952, 1495.373515144229941, 227.9074475250980072 ) ) ;
#16889 = CARTESIAN_POINT ( 'NONE',  ( -16.61577472324600180, 1459.965097909202086, 228.4923730740709971 ) ) ;
#16890 = ORIENTED_EDGE ( 'NONE', *, *, #45387, .F. ) ;
#16891 = CARTESIAN_POINT ( 'NONE',  ( -3.461047329755000401, 1516.858765657450249, 205.6745815831370123 ) ) ;
#16892 = CARTESIAN_POINT ( 'NONE',  ( 21.91814464780000193, 1410.042932703930092, 267.0360865957980536 ) ) ;
#16893 = LINE ( 'NONE', #86888, #58922 ) ;
#16894 = CARTESIAN_POINT ( 'NONE',  ( 23.43244672160000164, 1469.150049903229956, 198.8857204875980074 ) ) ;
#16895 = CARTESIAN_POINT ( 'NONE',  ( -0.2265857601506459928, 1508.856173191960124, 238.3683916615930229 ) ) ;
#16896 = CARTESIAN_POINT ( 'NONE',  ( 3.409608495353340096, 1454.219151911930112, 217.8661643445310006 ) ) ;
#16897 = CARTESIAN_POINT ( 'NONE',  ( -1.331441941370000048, 1451.289091497329991, 183.6056191985979922 ) ) ;
#16898 = ADVANCED_FACE ( 'NONE', ( #3407, #88497 ), #56974, .T. ) ;
#16899 = CARTESIAN_POINT ( 'NONE',  ( -33.93019615848938741, 1522.382868172863937, 220.5829544587966211 ) ) ;
#16900 = CARTESIAN_POINT ( 'NONE',  ( -16.42372150539999964, 1417.596044428880077, 205.5727566756989972 ) ) ;
#16901 = CARTESIAN_POINT ( 'NONE',  ( -13.49844358240000020, 1443.565604340589971, 187.1529031832980081 ) ) ;
#16902 = CARTESIAN_POINT ( 'NONE',  ( -22.58439900540000167, 1519.913060387329779, 209.1218459616979999 ) ) ;
#16903 = LINE ( 'NONE', #43259, #26876 ) ;
#16904 = CARTESIAN_POINT ( 'NONE',  ( -7.485183872730000409, 1498.430015208389932, 218.3832652741589868 ) ) ;
#16905 = ORIENTED_EDGE ( 'NONE', *, *, #62580, .T. ) ;
#16906 = CARTESIAN_POINT ( 'NONE',  ( 1.462581545746759915, 1493.452708605139833, 181.7091337628779968 ) ) ;
#16907 = CARTESIAN_POINT ( 'NONE',  ( -14.91623439969129983, 1409.433946770479906, 209.8509277100439760 ) ) ;
#16908 = AXIS2_PLACEMENT_3D ( 'NONE', #70522, #1650, #96802 ) ;
#16909 = CARTESIAN_POINT ( 'NONE',  ( 10.52884532342740087, 1481.875038510340119, 210.3006225101370035 ) ) ;
#16910 = CARTESIAN_POINT ( 'NONE',  ( -12.05837087505603833, 1377.636358387990413, 211.6001473997702362 ) ) ;
#16911 = CARTESIAN_POINT ( 'NONE',  ( -21.98433884700000007, 1471.929809744629893, 267.6462616537980352 ) ) ;
#16912 = CARTESIAN_POINT ( 'NONE',  ( -30.57064947821499246, 1523.844789899200805, 196.3873363930073879 ) ) ;
#16913 = CARTESIAN_POINT ( 'NONE',  ( -12.54019733330000008, 1391.397793261360221, 209.7548870936209937 ) ) ;
#16914 = CIRCLE ( 'NONE', #31254, 29.83173541461230727 ) ;
#16915 = CARTESIAN_POINT ( 'NONE',  ( -24.61293950550089704, 1444.770188684140066, 210.8869336946189890 ) ) ;
#16916 = CARTESIAN_POINT ( 'NONE',  ( -70.90293112098160577, 1384.660040799420130, 296.0611682970840093 ) ) ;
#16917 = CARTESIAN_POINT ( 'NONE',  ( -25.74505365984370187, 1384.960943526260053, 203.5578757433129908 ) ) ;
#16918 = VECTOR ( 'NONE', #75220, 1000.000000000000000 ) ;
#16919 = CARTESIAN_POINT ( 'NONE',  ( -6.733046173459999117, 1443.913060387330006, 154.8821828340979891 ) ) ;
#16920 = B_SPLINE_SURFACE_WITH_KNOTS ( 'NONE', 3, 5, ( 
 ( #21311, #55514, #28091, #70691, #89642, #79621 ),
 ( #81235, #4550, #38684, #72859, #106993, #104803 ),
 ( #62278, #96409, #6185, #7294, #14579, #49310 ),
 ( #56053, #66674, #99126, #82351, #83436, #23532 ) ),
 .UNSPECIFIED., .F., .F., .F.,
 ( 4, 4 ),
 ( 6, 6 ),
 ( 5.479555871690000579, 5.505626611740000342 ),
 ( 0.000000000000000000, 1.000000000000000000 ),
 .UNSPECIFIED. ) ;
#16921 = CARTESIAN_POINT ( 'NONE',  ( -106.4005663920000018, 1378.913060486199811, 301.5683367484589894 ) ) ;
#16922 = LINE ( 'NONE', #103149, #50156 ) ;
#16923 = DIRECTION ( 'NONE',  ( 0.9531756543815217420, 0.2975207091418809457, -0.05419962662297508199 ) ) ;
#16924 = CARTESIAN_POINT ( 'NONE',  ( -23.55015523019999790, 1410.657012870829931, 206.5846774848380107 ) ) ;
#16925 = CARTESIAN_POINT ( 'NONE',  ( -11.77674179528174569, 1378.208832213107371, 205.4865746833227718 ) ) ;
#16926 = CARTESIAN_POINT ( 'NONE',  ( 4.146834721160000292, 1484.913268816489790, 219.4317166241989980 ) ) ;
#16927 = CARTESIAN_POINT ( 'NONE',  ( 11.60982339427470045, 1478.971968693290137, 207.2338189534640094 ) ) ;
#16928 = B_SPLINE_SURFACE_WITH_KNOTS ( 'NONE', 5, 5, ( 
 ( #34422, #843, #93749, #58538, #69150, #84269 ),
 ( #68053, #102700, #57988, #33303, #15938, #34968 ),
 ( #92122, #25445, #77538, #41719, #42829, #101054 ),
 ( #15398, #50142, #60192, #296, #75879, #102163 ),
 ( #94311, #25994, #17590, #51224, #92664, #49587 ),
 ( #7013, #59638, #83718, #24352, #7564, #76990 ),
 ( #41171, #59093, #75345, #23797, #16485, #110027 ),
 ( #66945, #109485, #93218, #84807, #32762, #51789 ),
 ( #67498, #101602, #24886, #50674, #76423, #8106 ),
 ( #85929, #42273, #110577, #33862, #17026, #85357 ),
 ( #68596, #8652, #9232, #43389, #65218, #38332 ),
 ( #20970, #80904, #63045, #72512, #71989, #99329 ) ),
 .UNSPECIFIED., .F., .F., .F.,
 ( 6, 3, 3, 6 ),
 ( 6, 6 ),
 ( 24.09973612510790275, 25.95605821120000201, 29.66855005029999859, 34.15088587921729868 ),
 ( 0.000000000000000000, 1.506138665727279946 ),
 .UNSPECIFIED. ) ;
#16929 = CARTESIAN_POINT ( 'NONE',  ( 2.488082932330000219, 1441.600846913620217, 150.5962877614979902 ) ) ;
#16930 = CARTESIAN_POINT ( 'NONE',  ( 20.44998473589999932, 1433.812659856489972, 214.5407056977390141 ) ) ;
#16931 = CARTESIAN_POINT ( 'NONE',  ( 17.59789087266998919, 1524.659148609499425, 180.6834670445046811 ) ) ;
#16932 = CARTESIAN_POINT ( 'NONE',  ( 22.14279730894140030, 1473.984189750450014, 210.1089390468149816 ) ) ;
#16934 = CARTESIAN_POINT ( 'NONE',  ( -10.30967637289999850, 1381.062970967459705, 201.9668772049490144 ) ) ;
#16933 = CARTESIAN_POINT ( 'NONE',  ( -17.00797328670000397, 1417.537217351680056, 207.7155449971589860 ) ) ;
#16935 = CARTESIAN_POINT ( 'NONE',  ( 11.70540788988509817, 1426.716494867529946, 141.9064542283970241 ) ) ;
#16936 = CARTESIAN_POINT ( 'NONE',  ( 9.814145740701999188, 1435.717597957500175, 209.6091522368750191 ) ) ;
#16937 = CARTESIAN_POINT ( 'NONE',  ( -20.12564951288306858, 1511.187213306747708, 180.7149624981946658 ) ) ;
#16938 = CARTESIAN_POINT ( 'NONE',  ( 4.382345708037679977, 1446.936631694319885, 199.9395551071150123 ) ) ;
#16939 = CARTESIAN_POINT ( 'NONE',  ( -16.93613037863659798, 1507.562498015370011, 224.5799860225920099 ) ) ;
#16940 = CARTESIAN_POINT ( 'NONE',  ( 7.713117802984999827, 1516.690345681169902, 204.1174038931170003 ) ) ;
#16941 = CARTESIAN_POINT ( 'NONE',  ( -8.104953377315247565, 1398.153764496908934, 219.2861827199897107 ) ) ;
#16942 = CARTESIAN_POINT ( 'NONE',  ( -3.592552031026975179, 1440.810949641668003, 156.6291991093122249 ) ) ;
#16943 = CARTESIAN_POINT ( 'NONE',  ( 11.65102058319489764, 1433.170051679079961, 223.4015529330449965 ) ) ;
#16944 = CARTESIAN_POINT ( 'NONE',  ( 1.622533072389999997, 1508.277906825730042, 236.9750079829979654 ) ) ;
#16946 = ORIENTED_EDGE ( 'NONE', *, *, #93320, .T. ) ;
#16945 = CARTESIAN_POINT ( 'NONE',  ( -25.90124155867470179, 1379.608127361219886, 215.5185761863660048 ) ) ;
#16947 = ORIENTED_EDGE ( 'NONE', *, *, #61279, .T. ) ;
#16948 = CARTESIAN_POINT ( 'NONE',  ( 11.73789100506060024, 1434.215254847310007, 151.1141485369599877 ) ) ;
#16949 = CARTESIAN_POINT ( 'NONE',  ( 21.28823305372374719, 1525.253996226948630, 183.8869967656500819 ) ) ;
#16950 = ORIENTED_EDGE ( 'NONE', *, *, #6907, .T. ) ;
#16951 = CARTESIAN_POINT ( 'NONE',  ( -4.675540975309999681, 1462.620895424390028, 200.5633310686890241 ) ) ;
#16952 = AXIS2_PLACEMENT_3D ( 'NONE', #20308, #65093, #29818 ) ;
#16953 = DIRECTION ( 'NONE',  ( -0.9125304618754024322, 0.000000000000000000, -0.4090087482554191078 ) ) ;
#16954 = CYLINDRICAL_SURFACE ( 'NONE', #60613, 4.000000000000001776 ) ;
#16956 = CARTESIAN_POINT ( 'NONE',  ( -13.92066065641689931, 1508.898256883639988, 183.7940940037009909 ) ) ;
#16955 = DIRECTION ( 'NONE',  ( -1.000000000000000000, -8.646726228680001294E-15, 8.117787186050000125E-15 ) ) ;
#16957 = CARTESIAN_POINT ( 'NONE',  ( 18.84417403770989807, 1488.414032370149926, 228.9378882694660149 ) ) ;
#16958 = CARTESIAN_POINT ( 'NONE',  ( 0.5822587378750000431, 1468.709556387730117, 182.6088673434980194 ) ) ;
#16959 = CARTESIAN_POINT ( 'NONE',  ( 0.9486209649339989447, 1468.174413863890095, 219.2298037005990068 ) ) ;
#16960 = CARTESIAN_POINT ( 'NONE',  ( -24.11922042919299614, 1444.793574266630003, 211.7007084662699867 ) ) ;
#16961 = PRESENTATION_STYLE_ASSIGNMENT (( #85858 ) ) ;
#16962 = CARTESIAN_POINT ( 'NONE',  ( 5.296889735339999739, 1440.180353386090019, 211.9351589163190113 ) ) ;
#16964 = CIRCLE ( 'NONE', #79604, 1.999999999999999556 ) ;
#16963 = CARTESIAN_POINT ( 'NONE',  ( 14.13162141313959985, 1415.651572961190141, 197.1859206090720136 ) ) ;
#16965 = CARTESIAN_POINT ( 'NONE',  ( 11.86651437599999959, 1432.376750741719889, 150.3970641568979829 ) ) ;
#16966 = CARTESIAN_POINT ( 'NONE',  ( 5.986375103784999929, 1514.050458741980037, 201.4853999038570009 ) ) ;
#16967 = EDGE_LOOP ( 'NONE', ( #21388, #69655, #36508 ) ) ;
#16968 = CARTESIAN_POINT ( 'NONE',  ( 13.74968914389999952, 1435.188641123959997, 149.5600858840979868 ) ) ;
#16969 = EDGE_LOOP ( 'NONE', ( #18221, #87671, #34909, #13237 ) ) ;
#16970 = ORIENTED_EDGE ( 'NONE', *, *, #13827, .T. ) ;
#16971 = CARTESIAN_POINT ( 'NONE',  ( 13.51157294017894017, 1444.017624626980023, 169.3518533014032243 ) ) ;
#16972 = CARTESIAN_POINT ( 'NONE',  ( -11.45446824389999918, 1462.185551541130053, 233.9517322583979819 ) ) ;
#16973 = CARTESIAN_POINT ( 'NONE',  ( -7.719721968511599641, 1475.003672383036246, 202.3105564095348825 ) ) ;
#16974 = CARTESIAN_POINT ( 'NONE',  ( -2.291514335905000088, 1517.194972660189933, 216.8481778957070105 ) ) ;
#16975 = CARTESIAN_POINT ( 'NONE',  ( -8.463898933797024071, 1511.395345385101564, 213.9445291291372939 ) ) ;
#16976 = CARTESIAN_POINT ( 'NONE',  ( -18.98174732980886859, 1443.401523302673013, 211.6634804359809152 ) ) ;
#16977 = DIRECTION ( 'NONE',  ( 0.000000000000000000, 0.000000000000000000, 1.000000000000000000 ) ) ;
#16978 = CARTESIAN_POINT ( 'NONE',  ( 8.233576870951500105E-14, 1375.413060387289988, 209.1218459572589836 ) ) ;
#16979 =( BOUNDED_CURVE ( )  B_SPLINE_CURVE ( 3, ( #73205, #6546, #92200, #56409 ),
 .UNSPECIFIED., .F., .F. ) 
 B_SPLINE_CURVE_WITH_KNOTS ( ( 4, 4 ),
 ( 3.107150058479552168, 3.118904538992639086 ),
 .UNSPECIFIED. ) 
 CURVE ( )  GEOMETRIC_REPRESENTATION_ITEM ( )  RATIONAL_B_SPLINE_CURVE ( ( 1.000000000000000000, 0.9999884860487986415, 0.9999884860487986415, 1.000000000000000000 ) ) 
 REPRESENTATION_ITEM ( '' )  );
#16980 = ORIENTED_EDGE ( 'NONE', *, *, #9132, .F. ) ;
#16981 = CARTESIAN_POINT ( 'NONE',  ( -2.299656354225000143, 1516.843453247299749, 206.6453952679669896 ) ) ;
#16982 = VERTEX_POINT ( 'NONE', #99486 ) ;
#16983 = CARTESIAN_POINT ( 'NONE',  ( -105.5730645133519943, 1377.937125738340228, 304.5637690312989889 ) ) ;
#16984 = DIRECTION ( 'NONE',  ( 0.000000000000000000, 0.000000000000000000, 1.000000000000000000 ) ) ;
#16985 = CARTESIAN_POINT ( 'NONE',  ( -9.049519031959999182, 1409.396208824930000, 188.6360524509980223 ) ) ;
#16986 = CARTESIAN_POINT ( 'NONE',  ( 6.775684820614999992, 1512.341575225289944, 216.5029582879269867 ) ) ;
#16988 = ORIENTED_EDGE ( 'NONE', *, *, #79504, .T. ) ;
#16987 = FACE_OUTER_BOUND ( 'NONE', #9556, .T. ) ;
#16989 = CARTESIAN_POINT ( 'NONE',  ( 19.98583999950000134, 1427.549906271330201, 222.6473461575979798 ) ) ;
#16990 = CARTESIAN_POINT ( 'NONE',  ( -17.13479123734510168, 1508.551704408389924, 210.3956667297300100 ) ) ;
#16991 = CARTESIAN_POINT ( 'NONE',  ( -96.25814220559999512, 1384.042779414059851, 310.4933417822589377 ) ) ;
#16992 = DIRECTION ( 'NONE',  ( 0.9942586961433742543, -0.000000000000000000, -0.1070030146457445069 ) ) ;
#16993 = CARTESIAN_POINT ( 'NONE',  ( 21.41758936356361076, 1524.330813522192102, 184.2067724269726909 ) ) ;
#16994 = CARTESIAN_POINT ( 'NONE',  ( -5.775236830874999505, 1516.804776704140068, 214.1294346171470124 ) ) ;
#16995 = CARTESIAN_POINT ( 'NONE',  ( -2.963941339955419974, 1428.941128588449828, 200.2350009049089863 ) ) ;
#16996 = DIRECTION ( 'NONE',  ( 0.000000000000000000, 0.000000000000000000, 1.000000000000000000 ) ) ;
#16997 = EDGE_CURVE ( 'NONE', #83528, #10270, #20170, .T. ) ;
#16998 = CARTESIAN_POINT ( 'NONE',  ( 7.012466281656729805, 1508.551704615640119, 214.6351047168390096 ) ) ;
#16999 = CARTESIAN_POINT ( 'NONE',  ( -0.7351098092479989576, 1516.977504706749869, 211.6135016956469883 ) ) ;
#17000 = AXIS2_PLACEMENT_3D ( 'NONE', #57189, #16774, #50977 ) ;
#17001 = CARTESIAN_POINT ( 'NONE',  ( -11.87061842454789939, 1482.038080002969991, 208.5196970344390195 ) ) ;
#17002 = CARTESIAN_POINT ( 'NONE',  ( 30.11857922865945270, 1525.055427061254477, 221.6904370749649047 ) ) ;
#17004 = EDGE_LOOP ( 'NONE', ( #93134, #47052 ) ) ;
#17003 = CARTESIAN_POINT ( 'NONE',  ( -62.39649109850000031, 1386.686758807429896, 249.3285297428589899 ) ) ;
#17005 = CARTESIAN_POINT ( 'NONE',  ( -62.96821258457789838, 1385.052146392690247, 285.7569334418829499 ) ) ;
#17006 = CARTESIAN_POINT ( 'NONE',  ( -1.026416548450000011E-08, 1474.725755678329961, 264.8987716733979596 ) ) ;
#17007 = ADVANCED_FACE ( 'NONE', ( #83807 ), #29220, .T. ) ;
#17008 = CARTESIAN_POINT ( 'NONE',  ( 10.92413054773749970, 1490.487280210450081, 210.1135723924519993 ) ) ;
#17009 = CYLINDRICAL_SURFACE ( 'NONE', #2142, 0.9999999999999983347 ) ;
#17010 = CARTESIAN_POINT ( 'NONE',  ( -5.589046920511240302, 1509.019018111649984, 237.4740947115990082 ) ) ;
#17011 = CARTESIAN_POINT ( 'NONE',  ( -23.32672961829999991, 1448.440545525210155, 217.0581287948379838 ) ) ;
#17012 = CARTESIAN_POINT ( 'NONE',  ( 12.07722019553499848, 1511.957228877180114, 223.9708055708669860 ) ) ;
#17014 = CARTESIAN_POINT ( 'NONE',  ( 19.75084982839999981, 1455.504334175230042, 226.5702129394979920 ) ) ;
#17013 = CARTESIAN_POINT ( 'NONE',  ( 13.84742034927229959, 1420.584111001059910, 203.1248729974179810 ) ) ;
#17015 = CARTESIAN_POINT ( 'NONE',  ( -9.294437129912410001, 1449.358304634600017, 208.4206774063060266 ) ) ;
#17016 = CARTESIAN_POINT ( 'NONE',  ( -108.1487418590059946, 1381.161261816019760, 310.1575172367179789 ) ) ;
#17017 = EDGE_LOOP ( 'NONE', ( #12113, #53962, #87646, #64550 ) ) ;
#17018 = CARTESIAN_POINT ( 'NONE',  ( -0.01171164408179850049, 1516.939568781210028, 202.5649949355269825 ) ) ;
#17019 = CARTESIAN_POINT ( 'NONE',  ( -12.43204788642049863, 1508.443254155279874, 217.5037917836490067 ) ) ;
#17020 = CARTESIAN_POINT ( 'NONE',  ( 27.70707300099999770, 1508.597282344630003, 207.6634441784080138 ) ) ;
#17021 = CIRCLE ( 'NONE', #86759, 1.999999999999998668 ) ;
#17022 = CARTESIAN_POINT ( 'NONE',  ( 13.00580119799999856, 1425.728651690429842, 223.4081755709979973 ) ) ;
#17023 = CARTESIAN_POINT ( 'NONE',  ( -5.307053063608348609, 1425.580201077015545, 186.3543702352812659 ) ) ;
#17024 = CARTESIAN_POINT ( 'NONE',  ( 3.970758181649999496, 1467.502840618489927, 218.2663495880690050 ) ) ;
#17025 = CARTESIAN_POINT ( 'NONE',  ( -1.331958139231829923E-15, 1375.413060387289988, 209.1218459616989946 ) ) ;
#17026 = CARTESIAN_POINT ( 'NONE',  ( 32.65729098489229898, 1436.532483134479889, 136.5492245839050156 ) ) ;
#17027 = DIRECTION ( 'NONE',  ( 1.000000000000000000, 0.000000000000000000, 0.000000000000000000 ) ) ;
#17028 = CARTESIAN_POINT ( 'NONE',  ( -31.96358366148169949, 1465.307028659348589, 269.3165098066044152 ) ) ;
#17029 = CARTESIAN_POINT ( 'NONE',  ( -2.480175263330000046, 1429.207669914089820, 200.0830570310090195 ) ) ;
#17030 = CARTESIAN_POINT ( 'NONE',  ( 11.99724100530000115, 1508.052968999630139, 184.6308883575979962 ) ) ;
#17031 = CARTESIAN_POINT ( 'NONE',  ( 6.263489101080928378, 1465.252787188384445, 218.2607468416194365 ) ) ;
#17032 = CARTESIAN_POINT ( 'NONE',  ( -21.39312961732860785, 1524.775785348137561, 184.2561049718586048 ) ) ;
#17033 = CIRCLE ( 'NONE', #49300, 2.000000000000001776 ) ;
#17034 = CARTESIAN_POINT ( 'NONE',  ( -8.134103169834999036, 1515.224164712790071, 203.4316902230170001 ) ) ;
#17035 = VERTEX_POINT ( 'NONE', #65383 ) ;
#17036 = CARTESIAN_POINT ( 'NONE',  ( 14.72576938353500076, 1512.123542805230272, 196.9321265835669976 ) ) ;
#17037 = CARTESIAN_POINT ( 'NONE',  ( 11.94171318090000078, 1433.614828344280113, 146.4341826372979938 ) ) ;
#17038 = CARTESIAN_POINT ( 'NONE',  ( -4.119399150550410837, 1508.879003890470131, 213.4915664277669975 ) ) ;
#17039 = CARTESIAN_POINT ( 'NONE',  ( 16.05002729776590087, 1479.562477948200012, 188.9730107742090013 ) ) ;
#17040 = CARTESIAN_POINT ( 'NONE',  ( 11.32679319035097443, 1425.526293419519106, 138.7440965005115743 ) ) ;
#17042 = CARTESIAN_POINT ( 'NONE',  ( -18.09135377717698034, 1468.316747749531032, 200.5084487035089751 ) ) ;
#17041 = CARTESIAN_POINT ( 'NONE',  ( 12.44780703220000184, 1501.268281258290017, 211.7240718627089962 ) ) ;
#17043 = CARTESIAN_POINT ( 'NONE',  ( -28.27930516629999858, 1508.150008668130113, 209.2731387451690068 ) ) ;
#17044 = B_SPLINE_SURFACE_WITH_KNOTS ( 'NONE', 5, 1, ( 
 ( #96012, #96575 ),
 ( #64089, #19282 ),
 ( #10348, #1984 ),
 ( #99296, #22571 ),
 ( #99851, #107721 ),
 ( #55691, #48940 ) ),
 .UNSPECIFIED., .F., .F., .F.,
 ( 6, 6 ),
 ( 2, 2 ),
 ( 0.000000000000000000, 3.632392088579999623 ),
 ( 0.000000000000000000, 14.00000000000000000 ),
 .UNSPECIFIED. ) ;
#17045 = CARTESIAN_POINT ( 'NONE',  ( 7.788301635029999836, 1423.125804053390084, 213.4136639638890074 ) ) ;
#17046 = FACE_OUTER_BOUND ( 'NONE', #17723, .T. ) ;
#17047 = CARTESIAN_POINT ( 'NONE',  ( 43.48864058788180387, 1440.913032444390183, 270.3367086676489635 ) ) ;
#17048 = CARTESIAN_POINT ( 'NONE',  ( -38.61927355701700293, 1444.188087899089851, 137.1592452686400065 ) ) ;
#17049 = CARTESIAN_POINT ( 'NONE',  ( -16.49832412793039893, 1414.913057855109855, 208.5959317959809880 ) ) ;
#17050 = CARTESIAN_POINT ( 'NONE',  ( 24.84705735490000222, 1435.864857748740178, 137.4753733619980096 ) ) ;
#17051 = CARTESIAN_POINT ( 'NONE',  ( -9.716620324715218970, 1396.252372248279926, 203.8292857818589994 ) ) ;
#17052 = ORIENTED_EDGE ( 'NONE', *, *, #34365, .T. ) ;
#17053 = CARTESIAN_POINT ( 'NONE',  ( -0.08022770239056420394, 1416.524489948229984, 191.0302681666710214 ) ) ;
#17054 = CARTESIAN_POINT ( 'NONE',  ( -4.781335570289999559, 1409.080028304630105, 230.4240303851980229 ) ) ;
#17055 = ORIENTED_EDGE ( 'NONE', *, *, #45337, .T. ) ;
#17056 = EDGE_LOOP ( 'NONE', ( #15773, #24158, #84611, #26292 ) ) ;
#17057 = DIRECTION ( 'NONE',  ( 0.9980318515193541407, 1.681712440757244397E-31, 0.06270903725022322628 ) ) ;
#17058 = CARTESIAN_POINT ( 'NONE',  ( 7.322103118964429669, 1516.556754281647045, 207.4728157223430571 ) ) ;
#17060 = CARTESIAN_POINT ( 'NONE',  ( -24.41186848150000444, 1440.913060429529878, 212.0284777737979880 ) ) ;
#17059 = DIRECTION ( 'NONE',  ( 0.000000000000000000, 1.000000000000000000, 0.000000000000000000 ) ) ;
#17061 = CARTESIAN_POINT ( 'NONE',  ( -9.033607467220001297, 1447.303979291489895, 212.0883436982290107 ) ) ;
#17062 = CARTESIAN_POINT ( 'NONE',  ( 4.191474726083669999, 1424.969438579149937, 185.2130605783640078 ) ) ;
#17063 = CARTESIAN_POINT ( 'NONE',  ( -35.85007572059999603, 1380.172836988449944, 220.5090016197590046 ) ) ;
#17064 = CARTESIAN_POINT ( 'NONE',  ( -2.508314376045169158, 1421.038292245390949, 185.1991979782232249 ) ) ;
#17065 = CARTESIAN_POINT ( 'NONE',  ( -0.6235920161070117596, 1525.878013734321485, 242.9475333194527877 ) ) ;
#17066 = CARTESIAN_POINT ( 'NONE',  ( -13.32684181309999971, 1469.522592936189994, 191.9925905970989959 ) ) ;
#17067 = CARTESIAN_POINT ( 'NONE',  ( 8.768089064850000725, 1509.161960657329928, 181.7959779642980038 ) ) ;
#17068 = CARTESIAN_POINT ( 'NONE',  ( -113.4000000000000057, 1378.061224848670008, 306.7703178455799957 ) ) ;
#17069 = CARTESIAN_POINT ( 'NONE',  ( 8.796059898609998484, 1362.759824263850078, 207.6218459616989946 ) ) ;
#17070 = CARTESIAN_POINT ( 'NONE',  ( -29.05308884557584648, 1510.038507275123038, 216.5997246920866530 ) ) ;
#17072 = ORIENTED_EDGE ( 'NONE', *, *, #50710, .F. ) ;
#17071 = CARTESIAN_POINT ( 'NONE',  ( -21.53565904410000087, 1506.077647802389947, 209.2113159668039941 ) ) ;
#17073 = ORIENTED_EDGE ( 'NONE', *, *, #10300, .T. ) ;
#17074 = CARTESIAN_POINT ( 'NONE',  ( 11.19147557906589974, 1422.145537183640045, 210.4506353095700035 ) ) ;
#17075 = EDGE_CURVE ( 'NONE', #1945, #53899, #70875, .T. ) ;
#17076 = CIRCLE ( 'NONE', #56452, 2.000000000000003553 ) ;
#17077 = EDGE_CURVE ( 'NONE', #100609, #38471, #79802, .T. ) ;
#17078 = CARTESIAN_POINT ( 'NONE',  ( 7.494335682567689005, 1510.727597960018329, 203.0672645389179252 ) ) ;
#17079 = CARTESIAN_POINT ( 'NONE',  ( -3.148011829640000148, 1473.184271403730008, 270.4279803161980453 ) ) ;
#17080 = CARTESIAN_POINT ( 'NONE',  ( 11.87742785157381320, 1433.145466849493459, 147.6581215103447846 ) ) ;
#17081 = CARTESIAN_POINT ( 'NONE',  ( -128.5457199608194401, 1340.114449826969576, 295.9477014321888646 ) ) ;
#17083 = ADVANCED_FACE ( 'NONE', ( #23880 ), #97161, .T. ) ;
#17082 = CARTESIAN_POINT ( 'NONE',  ( 18.07642520410000131, 1475.513060387329915, 197.7809371531980105 ) ) ;
#17084 = CARTESIAN_POINT ( 'NONE',  ( -8.623386125339999708, 1384.482357225949954, 199.8976969836290039 ) ) ;
#17085 = B_SPLINE_SURFACE_WITH_KNOTS ( 'NONE', 5, 5, ( 
 ( #60236, #52946, #346, #69763, #10366, #60807 ),
 ( #19865, #44539, #1426, #94355, #43435, #17635 ),
 ( #893, #54068, #79250, #87647, #78684, #35016 ),
 ( #28279, #85975, #27180, #96594, #36137, #70321 ),
 ( #103880, #27727, #61914, #103302, #34473, #18204 ),
 ( #95483, #69196, #77586, #18750, #36682, #10933 ) ),
 .UNSPECIFIED., .F., .F., .F.,
 ( 6, 6 ),
 ( 6, 6 ),
 ( 6.379848894300000239, 6.971437020549999808 ),
 ( 0.000000000000000000, 1.455467945630000148 ),
 .UNSPECIFIED. ) ;
#17086 = EDGE_CURVE ( 'NONE', #8026, #57348, #52945, .T. ) ;
#17087 = CARTESIAN_POINT ( 'NONE',  ( -7.487063421429379417, 1517.051703294439903, 208.6815157772669806 ) ) ;
#17088 = CARTESIAN_POINT ( 'NONE',  ( 4.501691961672608322, 1368.956319095223989, 210.6218459616991936 ) ) ;
#17089 = CARTESIAN_POINT ( 'NONE',  ( -8.773114743372520508, 1448.864173605930091, 211.7399132152989978 ) ) ;
#17090 = CARTESIAN_POINT ( 'NONE',  ( -18.77802133838000032, 1408.856599020109797, 267.0889509827300117 ) ) ;
#17091 = CARTESIAN_POINT ( 'NONE',  ( -14.19163021719490025, 1435.224332456559978, 149.3102015397809907 ) ) ;
#17092 = EDGE_LOOP ( 'NONE', ( #110231, #109888, #54375, #91617 ) ) ;
#17093 = CARTESIAN_POINT ( 'NONE',  ( 2.469101154908970308, 1524.816548299036640, 242.3848636420295293 ) ) ;
#17094 = CARTESIAN_POINT ( 'NONE',  ( 13.17178224790000129, 1444.791376412119916, 187.5900384370979737 ) ) ;
#17095 = ORIENTED_EDGE ( 'NONE', *, *, #50748, .T. ) ;
#17096 = ORIENTED_EDGE ( 'NONE', *, *, #74781, .F. ) ;
#17097 = CARTESIAN_POINT ( 'NONE',  ( -5.292751683389999684, 1386.092796132500098, 203.4019327673190105 ) ) ;
#17098 = CARTESIAN_POINT ( 'NONE',  ( -1.121383629864999953, 1517.104192383289956, 213.7476359466970166 ) ) ;
#17099 = CARTESIAN_POINT ( 'NONE',  ( -18.90100382950000224, 1470.475492315429847, 190.2665493832980133 ) ) ;
#17100 = CARTESIAN_POINT ( 'NONE',  ( 9.833393186232900263, 1522.051704408389924, 205.7359371553449989 ) ) ;
#17101 = ORIENTED_EDGE ( 'NONE', *, *, #24948, .F. ) ;
#17102 = CARTESIAN_POINT ( 'NONE',  ( 0.02955819112566610354, 1517.151704408390060, 193.2356110507530218 ) ) ;
#17103 = AXIS2_PLACEMENT_3D ( 'NONE', #46052, #80185, #3500 ) ;
#17104 = EDGE_CURVE ( 'NONE', #14695, #87290, #108720, .T. ) ;
#17105 = CARTESIAN_POINT ( 'NONE',  ( 2.287084270065000258, 1517.068517094990057, 204.1085709707169826 ) ) ;
#17106 = CARTESIAN_POINT ( 'NONE',  ( -28.21332310190000214, 1508.643929351929955, 208.4757879089329720 ) ) ;
#17107 = CARTESIAN_POINT ( 'NONE',  ( -0.7293669130959999913, 1467.886321022529955, 230.1640753799979962 ) ) ;
#17108 = EDGE_CURVE ( 'NONE', #71672, #73345, #110113, .T. ) ;
#17110 = AXIS2_PLACEMENT_3D ( 'NONE', #91809, #7263, #24583 ) ;
#17109 = CARTESIAN_POINT ( 'NONE',  ( -28.43185375333949949, 1384.552470293700026, 204.7838833589590024 ) ) ;
#17111 =( BOUNDED_SURFACE ( )  B_SPLINE_SURFACE ( 3, 2, ( 
 ( #29985, #106694, #12089 ),
 ( #79864, #56311, #90444 ),
 ( #11551, #3174, #88806 ),
 ( #105620, #39507, #63099 ) ),
 .UNSPECIFIED., .F., .F., .F. ) 
 B_SPLINE_SURFACE_WITH_KNOTS ( ( 4, 4 ),
 ( 3, 3 ),
 ( 0.000000000000000000, 0.0002960034161023848936 ),
 ( 0.000000000000000000, 1.000000000000000000 ),
 .UNSPECIFIED. ) 
 GEOMETRIC_REPRESENTATION_ITEM ( )  RATIONAL_B_SPLINE_SURFACE ( (
 ( 1.000000000000000000, 0.8072480644198120059, 1.000000000000000000),
 ( 1.000000000000000000, 0.8072480346917830785, 1.000000000000000000),
 ( 1.000000000000000000, 0.8071723757218312034, 1.000000000000000000),
 ( 1.000000000000000000, 0.8070209408750057545, 1.000000000000000000) ) ) 
 REPRESENTATION_ITEM ( '' )  SURFACE ( )  );
#17112 = CARTESIAN_POINT ( 'NONE',  ( -3.985728878099999761, 1408.516724292330082, 196.0795530488979921 ) ) ;
#17113 = FACE_OUTER_BOUND ( 'NONE', #32435, .T. ) ;
#17115 = ORIENTED_EDGE ( 'NONE', *, *, #96646, .T. ) ;
#17114 = CARTESIAN_POINT ( 'NONE',  ( 31.18497486287775899, 1524.152349020271004, 196.3673245421346394 ) ) ;
#17116 = CARTESIAN_POINT ( 'NONE',  ( -24.86491373321030096, 1430.503315265359788, 209.8722520918030057 ) ) ;
#17117 = CARTESIAN_POINT ( 'NONE',  ( 27.21299276530000100, 1488.689717874130110, 210.5521098509080105 ) ) ;
#17118 = CARTESIAN_POINT ( 'NONE',  ( -68.77278092737650184, 1379.747928288920093, 280.3133413970129482 ) ) ;
#17119 = CARTESIAN_POINT ( 'NONE',  ( 6.832578770827522519, 1420.119835273649869, 222.9246289101963896 ) ) ;
#17120 = CARTESIAN_POINT ( 'NONE',  ( -23.87957571749999985, 1435.331403578989921, 136.9496437524980195 ) ) ;
#17121 = CARTESIAN_POINT ( 'NONE',  ( -2.283570671295000132, 1516.909589401870107, 212.0033943946770023 ) ) ;
#17122 = CARTESIAN_POINT ( 'NONE',  ( -68.72163677839999707, 1379.747817063369894, 280.0443424388590188 ) ) ;
#17123 = CARTESIAN_POINT ( 'NONE',  ( -14.52771248069999999, 1418.016205493429879, 227.0709974350980076 ) ) ;
#17124 = CARTESIAN_POINT ( 'NONE',  ( -12.98226561589999939, 1414.913060387329779, 219.9156672276980089 ) ) ;
#17125 = CARTESIAN_POINT ( 'NONE',  ( 3.253301381255000013, 1516.790374942449944, 207.9863856151469861 ) ) ;
#17126 = VERTEX_POINT ( 'NONE', #93844 ) ;
#17127 = FACE_OUTER_BOUND ( 'NONE', #23319, .T. ) ;
#17128 = CARTESIAN_POINT ( 'NONE',  ( -5.961592730449999600, 1410.297059247229981, 231.5003550203979898 ) ) ;
#17129 = CARTESIAN_POINT ( 'NONE',  ( -3.078458293560000225, 1384.906579013939790, 218.5736861911289850 ) ) ;
#17130 = ORIENTED_EDGE ( 'NONE', *, *, #18307, .T. ) ;
#17131 = CARTESIAN_POINT ( 'NONE',  ( -13.15726396577390034, 1415.954755716080172, 220.1962943805110058 ) ) ;
#17132 = CARTESIAN_POINT ( 'NONE',  ( -9.647687026466609694, 1493.068473758189839, 201.4942496940060153 ) ) ;
#17133 = CARTESIAN_POINT ( 'NONE',  ( 12.17555016557819947, 1435.314517998499923, 151.0473610424109836 ) ) ;
#17134 = EDGE_CURVE ( 'NONE', #51148, #85474, #28812, .T. ) ;
#17135 = CARTESIAN_POINT ( 'NONE',  ( -4.089785825655819274, 1441.278398204691484, 184.5636933043436443 ) ) ;
#17136 = CARTESIAN_POINT ( 'NONE',  ( -25.22529742364680061, 1509.794288727649928, 224.2186411218499984 ) ) ;
#17137 = CARTESIAN_POINT ( 'NONE',  ( -16.48227147120495317, 1525.651286436459031, 236.6829015109164516 ) ) ;
#17138 = CARTESIAN_POINT ( 'NONE',  ( 44.21963038504740240, 1440.913060387359792, 267.5638318536060183 ) ) ;
#17139 = DIRECTION ( 'NONE',  ( 0.4794255386041986200, 0.000000000000000000, 0.8775825618903752012 ) ) ;
#17140 = CARTESIAN_POINT ( 'NONE',  ( 10.10004869885203682, 1423.143362674105219, 137.0999999980979851 ) ) ;
#17142 = CARTESIAN_POINT ( 'NONE',  ( -2.917792487480000307, 1420.757440859130156, 185.9241331037979990 ) ) ;
#17141 = CARTESIAN_POINT ( 'NONE',  ( 6.557909882634999299, 1516.908489800550115, 214.8995913655070069 ) ) ;
#17143 = CARTESIAN_POINT ( 'NONE',  ( -8.869114759610731369, 1385.182896069670051, 218.6736307222820130 ) ) ;
#17144 = CARTESIAN_POINT ( 'NONE',  ( 4.616861508414999093, 1516.666407245520077, 216.8343369232169948 ) ) ;
#17145 = ORIENTED_EDGE ( 'NONE', *, *, #61921, .F. ) ;
#17146 = CARTESIAN_POINT ( 'NONE',  ( -12.78690732010000097, 1416.828044802929981, 195.5394877781979801 ) ) ;
#17147 = CARTESIAN_POINT ( 'NONE',  ( -11.60004869885203682, 1426.170950560207530, 138.0046165345982843 ) ) ;
#17148 = VERTEX_POINT ( 'NONE', #51878 ) ;
#17150 = CARTESIAN_POINT ( 'NONE',  ( 3.444734345749999704, 1421.426336298530032, 184.7111240843979942 ) ) ;
#17149 = ADVANCED_BREP_SHAPE_REPRESENTATION ( '', ( #9778, #21632 ), #28938 ) ;
#17151 = VECTOR ( 'NONE', #28029, 1000.000000000000000 ) ;
#17152 = FACE_OUTER_BOUND ( 'NONE', #3089, .T. ) ;
#17153 = CARTESIAN_POINT ( 'NONE',  ( 2.693001348315085863, 1524.059663615499858, 176.1570368348570241 ) ) ;
#17154 = CARTESIAN_POINT ( 'NONE',  ( 9857.840209716168829, 50.13405481564039690, -1086.115145477200031 ) ) ;
#17155 = CYLINDRICAL_SURFACE ( 'NONE', #12051, 2.000000000000003553 ) ;
#17156 = CARTESIAN_POINT ( 'NONE',  ( -7.220970672452868833, 1508.392792329803569, 219.6893434555957185 ) ) ;
#17157 = CARTESIAN_POINT ( 'NONE',  ( 18.88088134670000073, 1416.274718424630009, 210.4721620632179793 ) ) ;
#17158 = CARTESIAN_POINT ( 'NONE',  ( 10.93233376569999926, 1490.536113732890044, 207.1036721549689901 ) ) ;
#17159 = CARTESIAN_POINT ( 'NONE',  ( -4.926829097150000614, 1435.943783413959864, 150.1744789664979862 ) ) ;
#17160 = CARTESIAN_POINT ( 'NONE',  ( 27.27137807743889653, 1446.453610523900124, 137.2094998867499953 ) ) ;
#17162 = CARTESIAN_POINT ( 'NONE',  ( 4.327051608332269872, 1515.156337024050117, 208.9297172523390032 ) ) ;
#17161 = CARTESIAN_POINT ( 'NONE',  ( -8.629751412190879378, 1419.780543030299896, 195.8880434429399884 ) ) ;
#17163 = CARTESIAN_POINT ( 'NONE',  ( 7.460636164861699449, 1509.035273820331440, 203.0850866401826522 ) ) ;
#17164 = EDGE_LOOP ( 'NONE', ( #15726, #65572, #94800, #45351 ) ) ;
#17165 = CARTESIAN_POINT ( 'NONE',  ( 1.547077000027379912, 1416.702560751770079, 190.2314781873849654 ) ) ;
#17166 = EDGE_CURVE ( 'NONE', #102315, #106368, #76642, .T. ) ;
#17167 = CARTESIAN_POINT ( 'NONE',  ( 2.500000000000000000, 1440.913060387330006, 209.1218459616979999 ) ) ;
#17168 = CARTESIAN_POINT ( 'NONE',  ( -24.41186848580399982, 1440.913060429360030, 212.0284777848129920 ) ) ;
#17169 = FACE_OUTER_BOUND ( 'NONE', #83489, .T. ) ;
#17170 = ADVANCED_FACE ( 'NONE', ( #60277 ), #45312, .F. ) ;
#17171 = CARTESIAN_POINT ( 'NONE',  ( -10.40181139226799978, 1479.469451619749861, 210.4662640014259978 ) ) ;
#17172 = CARTESIAN_POINT ( 'NONE',  ( 28.44964981547635219, 1526.382868172864164, 219.8796466721251477 ) ) ;
#17174 = AXIS2_PLACEMENT_3D ( 'NONE', #44761, #44200, #76682 ) ;
#17173 = CARTESIAN_POINT ( 'NONE',  ( -5.932239102140000497, 1391.913060387289988, 209.1218459572589836 ) ) ;
#17175 = CARTESIAN_POINT ( 'NONE',  ( -14.38096556510000035, 1422.143733531690032, 196.2925564653990023 ) ) ;
#17176 = AXIS2_PLACEMENT_3D ( 'NONE', #66569, #50310, #23955 ) ;
#17177 = CARTESIAN_POINT ( 'NONE',  ( -72.21359640208430619, 1383.783188034720069, 297.1805363241429632 ) ) ;
#17178 = CARTESIAN_POINT ( 'NONE',  ( -10.26338073471560008, 1517.051704408389924, 184.6900425920350131 ) ) ;
#17179 = CARTESIAN_POINT ( 'NONE',  ( -3.347801439296141268, 1518.913060387330006, 242.0893193391992497 ) ) ;
#17180 = CARTESIAN_POINT ( 'NONE',  ( 14.62022923471335467, 1410.806204316170351, 191.5183363024188168 ) ) ;
#17182 = ORIENTED_EDGE ( 'NONE', *, *, #78864, .T. ) ;
#17181 = CARTESIAN_POINT ( 'NONE',  ( 24.34813363090000138, 1509.525084498130127, 194.8613372772980199 ) ) ;
#17183 = CARTESIAN_POINT ( 'NONE',  ( -18.42620122711428365, 1458.925670360632921, 227.7001417621163455 ) ) ;
#17184 = CARTESIAN_POINT ( 'NONE',  ( -47.98273391449999536, 1382.329346158459884, 255.9965235912589492 ) ) ;
#17185 = CARTESIAN_POINT ( 'NONE',  ( -17.63065570870000087, 1409.528736451330133, 222.5595780730980096 ) ) ;
#17186 = ORIENTED_EDGE ( 'NONE', *, *, #15389, .F. ) ;
#17187 = EDGE_LOOP ( 'NONE', ( #91633, #104326, #88489, #74710 ) ) ;
#17188 = CARTESIAN_POINT ( 'NONE',  ( 19.46142334528079942, 1509.259962660840074, 230.2314711598330064 ) ) ;
#17189 = CARTESIAN_POINT ( 'NONE',  ( 18.80464302510000252, 1425.801049065629968, 225.6039134470979945 ) ) ;
#17190 = CARTESIAN_POINT ( 'NONE',  ( 39.30684815028109824, 1440.174742933630114, 136.7448234688500008 ) ) ;
#17192 = CARTESIAN_POINT ( 'NONE',  ( -4.602356253840000022, 1468.583955076089978, 189.7619545879989857 ) ) ;
#17191 = CARTESIAN_POINT ( 'NONE',  ( 18.10327300539999840, 1416.823634022829992, 209.0372315287800120 ) ) ;
#17193 = CARTESIAN_POINT ( 'NONE',  ( -6.264689016930000243, 1463.667333189490137, 201.0440036769589938 ) ) ;
#17194 = CARTESIAN_POINT ( 'NONE',  ( -108.6438184989999911, 1382.182729019579938, 297.8040021080590236 ) ) ;
#17195 = CARTESIAN_POINT ( 'NONE',  ( -2.038847259689231084, 1522.382868172863937, 244.9330574173806951 ) ) ;
#17196 = CARTESIAN_POINT ( 'NONE',  ( 22.75273496409577945, 1523.382868172864164, 183.6728937936772184 ) ) ;
#17197 = EDGE_CURVE ( 'NONE', #35907, #47709, #18929, .T. ) ;
#17198 = CARTESIAN_POINT ( 'NONE',  ( 4.283818917599999665, 1409.998137916430096, 186.1439897097980065 ) ) ;
#17199 = DIRECTION ( 'NONE',  ( -0.7636030817426309181, -3.014599818829910125E-11, -0.6456859403403150122 ) ) ;
#17200 = CARTESIAN_POINT ( 'NONE',  ( 40.27297414431956923, 1443.653306489278748, 137.1208278072323878 ) ) ;
#17201 = CARTESIAN_POINT ( 'NONE',  ( 8.002862298599998425, 1439.449515709130083, 153.7646872756980088 ) ) ;
#17202 = CARTESIAN_POINT ( 'NONE',  ( -3.654169310603359921, 1441.538905863229957, 168.7225120603009714 ) ) ;
#17203 = CARTESIAN_POINT ( 'NONE',  ( -24.63041513499999979, 1451.910759690930036, 137.3284483466979964 ) ) ;
#17204 = CARTESIAN_POINT ( 'NONE',  ( 0.4781507175040000113, 1465.417316753030036, 236.2850646078979935 ) ) ;
#17205 = ORIENTED_EDGE ( 'NONE', *, *, #44367, .T. ) ;
#17206 = EDGE_CURVE ( 'NONE', #93518, #54705, #53543, .T. ) ;
#17207 = CARTESIAN_POINT ( 'NONE',  ( 10.59812014278140069, 1477.523980704680071, 229.9254261715079792 ) ) ;
#17208 = CARTESIAN_POINT ( 'NONE',  ( -44.28498751210000250, 1445.865707094600111, 269.9174198735980212 ) ) ;
#17209 = CARTESIAN_POINT ( 'NONE',  ( -6.232532106187401055, 1407.162969929529936, 197.7132727037109987 ) ) ;
#17210 = CARTESIAN_POINT ( 'NONE',  ( 0.000000000000000000, 1523.409940573003951, 209.1218459616979999 ) ) ;
#17211 = ADVANCED_FACE ( 'NONE', ( #45701 ), #12622, .T. ) ;
#17212 = CARTESIAN_POINT ( 'NONE',  ( 16.40748204129999976, 1468.824047016830036, 189.6837539406980113 ) ) ;
#17213 = B_SPLINE_CURVE_WITH_KNOTS ( 'NONE', 5,
 ( #22045, #53651, #104017, #22593, #21500, #14220, #72501, #29919, #4189, #30477, #90933, #27312, #10515, #106630, #107188 ),
 .UNSPECIFIED., .F., .F.,
 ( 6, 3, 3, 3, 6 ),
 ( 0.000000000000000000, 0.02279422308916183651, 0.2182353784632560800, 0.6091176892316280123, 1.000000000000000000 ),
 .UNSPECIFIED. ) ;
#17214 = CARTESIAN_POINT ( 'NONE',  ( -4.059787370426500287E-09, 1471.846784317870060, 258.6367045587240341 ) ) ;
#17215 = CARTESIAN_POINT ( 'NONE',  ( -12.80491917260000001, 1502.810374455390047, 208.8309748505670029 ) ) ;
#17216 = CARTESIAN_POINT ( 'NONE',  ( -2.003732309335499728, 1420.923232009330150, 193.8159282254100049 ) ) ;
#17217 = CARTESIAN_POINT ( 'NONE',  ( -6.210268667529999398, 1417.485306226330067, 231.9805137463980031 ) ) ;
#17218 = CARTESIAN_POINT ( 'NONE',  ( 0.6561095716360010321, 1477.838425433890052, 198.7002117315989835 ) ) ;
#17219 = CARTESIAN_POINT ( 'NONE',  ( -108.2870185569999961, 1387.477179604599996, 310.5036998792590452 ) ) ;
#17220 = CARTESIAN_POINT ( 'NONE',  ( -0.6623775808828666900, 1485.388627107794946, 181.9464839905526219 ) ) ;
#17221 = CARTESIAN_POINT ( 'NONE',  ( 5.604365146379768348, 1361.139420828405946, 210.6218459616991936 ) ) ;
#17222 = CARTESIAN_POINT ( 'NONE',  ( -46.08889470559520163, 1438.835070612000209, 266.9740849372739717 ) ) ;
#17223 = CARTESIAN_POINT ( 'NONE',  ( 13.56161761879410044, 1508.782329442760101, 233.5620020540920052 ) ) ;
#17224 = FACE_OUTER_BOUND ( 'NONE', #80289, .T. ) ;
#17225 = EDGE_CURVE ( 'NONE', #10311, #106390, #105029, .T. ) ;
#17226 = ORIENTED_EDGE ( 'NONE', *, *, #17075, .F. ) ;
#17227 = CARTESIAN_POINT ( 'NONE',  ( -5.011551406145000165, 1517.080322339569875, 208.3849417611969841 ) ) ;
#17228 = CARTESIAN_POINT ( 'NONE',  ( -2.478759544509999913, 1435.233202498340006, 157.6046889441980170 ) ) ;
#17229 = CARTESIAN_POINT ( 'NONE',  ( 19.26683521067225868, 1456.110280151028292, 225.0772932314519892 ) ) ;
#17230 = CARTESIAN_POINT ( 'NONE',  ( 7.182548959824419654, 1426.565124233989764, 213.0328279948139993 ) ) ;
#17231 = ADVANCED_FACE ( 'NONE', ( #79839 ), #51178, .T. ) ;
#17232 = B_SPLINE_SURFACE_WITH_KNOTS ( 'NONE', 5, 5, ( 
 ( #4200, #3673, #31035, #37801, #29380, #4734 ),
 ( #73058, #98794, #22056, #90381, #13660, #47849 ),
 ( #81983, #5291, #39449, #73622, #107752, #32699 ),
 ( #32147, #33792, #74174, #41658, #66335, #65765 ),
 ( #109965, #100451, #41096, #100989, #33243, #57382 ),
 ( #14230, #24285, #31588, #7496, #66879, #16419 ),
 ( #108303, #93150, #48419, #23734, #40546, #75275 ),
 ( #15326, #75814, #74720, #50612, #99883, #48974 ),
 ( #82562, #42210, #108853, #57922, #90944, #23181 ) ),
 .UNSPECIFIED., .F., .F., .F.,
 ( 6, 3, 6 ),
 ( 6, 6 ),
 ( 0.7655572723410000169, 2.316155491850000026, 3.835724788479999869 ),
 ( 0.000000000000000000, 1.000000000000000000 ),
 .UNSPECIFIED. ) ;
#17233 = B_SPLINE_CURVE_WITH_KNOTS ( 'NONE', 3,
 ( #60050, #85215, #23663, #15248, #24739, #94168, #49440, #25294, #75195, #149, #34270, #83562, #33163, #68452, #6855, #58936, #67352, #102555, #109346, #74641, #25848, #32627, #100904, #48900, #84119, #83027, #24201, #58387 ),
 .UNSPECIFIED., .F., .F.,
 ( 4, 3, 3, 3, 3, 3, 3, 3, 3, 4 ),
 ( -41.05058650750000027, -39.67091674781929811, -38.29124698813869543, -36.91872546091649809, -35.54143844538869956, -34.17184909951799909, -32.80586366775889928, -31.44473546961619803, -30.07247103563280177, -28.72930409989999845 ),
 .UNSPECIFIED. ) ;
#17234 = CARTESIAN_POINT ( 'NONE',  ( -26.79661678085199839, 1451.977403426660203, 134.9984873815419917 ) ) ;
#17235 = ORIENTED_EDGE ( 'NONE', *, *, #65318, .F. ) ;
#17236 = CARTESIAN_POINT ( 'NONE',  ( 8.713969742539999785, 1418.939459092229981, 231.9965623745979713 ) ) ;
#17237 = CARTESIAN_POINT ( 'NONE',  ( -15.28467106619119953, 1512.548660307860018, 222.3969343260469884 ) ) ;
#17238 = EDGE_CURVE ( 'NONE', #102140, #20317, #77943, .T. ) ;
#17239 = CARTESIAN_POINT ( 'NONE',  ( 4.718773895884976532, 1428.060710547474855, 215.9373307104791309 ) ) ;
#17240 = CARTESIAN_POINT ( 'NONE',  ( -15.46685519719999924, 1426.081634757429811, 211.8324972136479971 ) ) ;
#17241 = FACE_OUTER_BOUND ( 'NONE', #45946, .T. ) ;
#17242 = FACE_OUTER_BOUND ( 'NONE', #5544, .T. ) ;
#17243 = EDGE_CURVE ( 'NONE', #22220, #85592, #35606, .T. ) ;
#17244 = CARTESIAN_POINT ( 'NONE',  ( 5426.659192927022559, 54.07981494723836136, 8449.939230966730975 ) ) ;
#17245 = ORIENTED_EDGE ( 'NONE', *, *, #83127, .T. ) ;
#17246 = CARTESIAN_POINT ( 'NONE',  ( -6.545930427259980533, 1410.746461301010186, 269.3398854477759983 ) ) ;
#17247 = CARTESIAN_POINT ( 'NONE',  ( 4.082851105566869698, 1417.107827966569857, 231.9800176705820149 ) ) ;
#17248 = CARTESIAN_POINT ( 'NONE',  ( -2.541329734699477427, 1448.915361678037016, 183.5773954481504688 ) ) ;
#17250 = VERTEX_POINT ( 'NONE', #45144 ) ;
#17249 = CARTESIAN_POINT ( 'NONE',  ( -2.500000000000000000, 1439.595905110280000, 166.5328619750869734 ) ) ;
#17251 = ORIENTED_EDGE ( 'NONE', *, *, #102049, .T. ) ;
#17252 = EDGE_CURVE ( 'NONE', #18109, #30631, #15138, .T. ) ;
#17253 = CARTESIAN_POINT ( 'NONE',  ( -23.15985215759310023, 1409.837679178900089, 209.7045568244390097 ) ) ;
#17254 = CARTESIAN_POINT ( 'NONE',  ( -1.354641933420439814, 1409.895065768689847, 185.6211235086560123 ) ) ;
#17255 = CARTESIAN_POINT ( 'NONE',  ( -99.28159243359999664, 1336.950374720429863, 311.9347671633890400 ) ) ;
#17256 = CARTESIAN_POINT ( 'NONE',  ( -4.743041381730000339, 1427.184332118029943, 133.6118001900980232 ) ) ;
#17257 = EDGE_CURVE ( 'NONE', #23409, #53095, #20495, .T. ) ;
#17258 = CARTESIAN_POINT ( 'NONE',  ( -14.59279134157089963, 1436.244781760590058, 149.8708244536879874 ) ) ;
#17259 = CARTESIAN_POINT ( 'NONE',  ( -17.69728439860000080, 1415.862141658330074, 225.6688577867979859 ) ) ;
#17260 = CARTESIAN_POINT ( 'NONE',  ( 30.02970996041729990, 1467.470256667440026, 268.6852542625180149 ) ) ;
#17261 = CARTESIAN_POINT ( 'NONE',  ( -3.031930836974722876, 1466.806735891728522, 235.0189408935569872 ) ) ;
#17262 = CARTESIAN_POINT ( 'NONE',  ( -3.994937571899999984, 1430.106198350590148, 201.8091617873290033 ) ) ;
#17263 = CARTESIAN_POINT ( 'NONE',  ( -5.786837717054999608, 1517.040132827679827, 205.8646253294070050 ) ) ;
#17264 = EDGE_LOOP ( 'NONE', ( #7761, #27279, #24843, #55709 ) ) ;
#17265 = CARTESIAN_POINT ( 'NONE',  ( -11.90119038212991498, 1433.600011632037877, 150.4754701663967467 ) ) ;
#17266 = CARTESIAN_POINT ( 'NONE',  ( -1.329273608271069884, 1444.363671018100149, 199.1564131946590237 ) ) ;
#17267 = DIRECTION ( 'NONE',  ( 1.387778780781444413E-14, 0.000000000000000000, 1.000000000000000000 ) ) ;
#17268 = ORIENTED_EDGE ( 'NONE', *, *, #85543, .T. ) ;
#17270 = B_SPLINE_CURVE_WITH_KNOTS ( 'NONE', 3,
 ( #9756, #1370, #53445, #61310, #17576, #33849, #87591, #18691, #35512, #85344, #34955, #52888, #60182, #42816, #94870, #78627, #69705, #76977, #8640, #10308, #25429, #60747, #26553, #59625, #827, #61855, #44481, #68040, #87016, #43920, #9219, #10879, #284, #34410, #77526, #43377, #68582, #76409, #86463, #19236 ),
 .UNSPECIFIED., .F., .F.,
 ( 4, 3, 3, 3, 3, 3, 3, 3, 3, 3, 3, 3, 3, 4 ),
 ( -1.460858415939999988, -1.411203178505739952, -1.297247195856390034, -1.181596853130470137, -1.064890566428260188, -0.9466603196382510355, -0.8277066115153159931, -0.7083408824893170364, -0.5889085004284719815, -0.4643442267839680282, -0.3464089112407460203, -0.2295942582252259445, -0.1140863307625139544, 0.000000000000000000 ),
 .UNSPECIFIED. ) ;
#17269 = CARTESIAN_POINT ( 'NONE',  ( 3.961806501186879270, 1508.551704407889929, 204.5769769800630229 ) ) ;
#17271 = CARTESIAN_POINT ( 'NONE',  ( 26.71914925442930056, 1451.974538300859876, 135.0890004682200072 ) ) ;
#17272 = CARTESIAN_POINT ( 'NONE',  ( 2.487935123032368967, 1508.551704413348716, 204.2634855739857187 ) ) ;
#17273 = CARTESIAN_POINT ( 'NONE',  ( 12.19144863275480084, 1501.599284162290132, 212.7637707930009867 ) ) ;
#17274 = CARTESIAN_POINT ( 'NONE',  ( 7.503571368420000276, 1422.857534295030064, 195.6852864414989881 ) ) ;
#17275 = CARTESIAN_POINT ( 'NONE',  ( 18.49178363470000264, 1410.482338634230018, 194.3597946893979724 ) ) ;
#17276 = CARTESIAN_POINT ( 'NONE',  ( -3.394304855489999717, 1495.766742607790093, 197.6817024317990104 ) ) ;
#17277 = CARTESIAN_POINT ( 'NONE',  ( 0.4554814033272580054, 1408.928966148389918, 186.5349708927100210 ) ) ;
#17279 = CARTESIAN_POINT ( 'NONE',  ( -18.12762350887655316, 1423.809303112999032, 225.6003212586901157 ) ) ;
#17278 = CARTESIAN_POINT ( 'NONE',  ( 30.83422926911982032, 1524.871836253796118, 196.5181389497718385 ) ) ;
#17280 = CARTESIAN_POINT ( 'NONE',  ( 15.94345596297699963, 1409.469818137940138, 225.2684692625209948 ) ) ;
#17281 = LINE ( 'NONE', #85604, #10660 ) ;
#17282 = CARTESIAN_POINT ( 'NONE',  ( -12.70027339480000173, 1379.689331990199889, 213.2914259217290009 ) ) ;
#17283 = CARTESIAN_POINT ( 'NONE',  ( 5.755110967747741668, 1418.244149184685966, 233.8060213123679887 ) ) ;
#17284 = ORIENTED_EDGE ( 'NONE', *, *, #35693, .F. ) ;
#17285 = CARTESIAN_POINT ( 'NONE',  ( 12.77667375843740061, 1416.535698381769862, 222.1372311004039943 ) ) ;
#17286 = DIRECTION ( 'NONE',  ( 0.000000000000000000, 1.000000000000000000, 0.000000000000000000 ) ) ;
#17287 = DIRECTION ( 'NONE',  ( -0.1215789942062150408, 0.8574459172214612401, -0.5000050471825780996 ) ) ;
#17288 = CARTESIAN_POINT ( 'NONE',  ( -12.91227934189999971, 1390.899010879880052, 208.3938681258139809 ) ) ;
#17289 = CARTESIAN_POINT ( 'NONE',  ( 8.168301522416200555, 1425.263768431070048, 211.0005860271879783 ) ) ;
#17290 = EDGE_CURVE ( 'NONE', #5392, #49285, #70357, .T. ) ;
#17291 = CARTESIAN_POINT ( 'NONE',  ( -34.62870020261659931, 1450.374171996330006, 136.2315969410039997 ) ) ;
#17292 = CARTESIAN_POINT ( 'NONE',  ( -12.51099982459209947, 1416.825784013739849, 222.1450729932890056 ) ) ;
#17293 = CARTESIAN_POINT ( 'NONE',  ( -28.05448518339999708, 1461.575973621429966, 265.6112251771979800 ) ) ;
#17294 = CARTESIAN_POINT ( 'NONE',  ( -8.934489778684168826, 1384.314414410530162, 218.6338716263649928 ) ) ;
#17295 = CARTESIAN_POINT ( 'NONE',  ( 11.26092790689999923, 1433.522411100119825, 151.5416666487980137 ) ) ;
#17296 = CARTESIAN_POINT ( 'NONE',  ( 28.02005515429999960, 1444.132107003350029, 248.0989693021979861 ) ) ;
#17297 = CONICAL_SURFACE ( 'NONE', #85493, 24.00000000000002132, 0.3430239404209998177 ) ;
#17298 = CARTESIAN_POINT ( 'NONE',  ( -9.854800274776160052, 1461.491539507700054, 209.0809694339070006 ) ) ;
#17299 = CARTESIAN_POINT ( 'NONE',  ( -14.06005930971490159, 1420.585608153310204, 196.0549662394890049 ) ) ;
#17300 = CARTESIAN_POINT ( 'NONE',  ( 8.091109713897852274, 1420.444008331189934, 195.3478219760000059 ) ) ;
#17301 = CARTESIAN_POINT ( 'NONE',  ( 4.575282349084649702, 1466.769470911500093, 218.0850143904499987 ) ) ;
#17302 = EDGE_CURVE ( 'NONE', #68662, #1545, #2923, .T. ) ;
#17303 = DIRECTION ( 'NONE',  ( -5.980589973904019347E-17, 1.000000000000000000, -1.736889445713099699E-16 ) ) ;
#17304 = LINE ( 'NONE', #76147, #73573 ) ;
#17305 = CARTESIAN_POINT ( 'NONE',  ( 2.145405888939999617, 1466.621345377330044, 234.3697071566979844 ) ) ;
#17306 = CARTESIAN_POINT ( 'NONE',  ( 19.53984293219999913, 1410.902666560329862, 220.8234250620979822 ) ) ;
#17307 = CIRCLE ( 'NONE', #6563, 1.999999999999995559 ) ;
#17308 = FACE_OUTER_BOUND ( 'NONE', #85713, .T. ) ;
#17309 = CARTESIAN_POINT ( 'NONE',  ( -40.51263900100065030, 1439.427257612305539, 135.2566761075825923 ) ) ;
#17310 = CARTESIAN_POINT ( 'NONE',  ( -1.842963219479999859, 1515.064792519189950, 204.7923971761390192 ) ) ;
#17311 = CARTESIAN_POINT ( 'NONE',  ( 13.91344329550000047, 1453.313060387329870, 223.0352892565979914 ) ) ;
#17312 = CARTESIAN_POINT ( 'NONE',  ( 24.11200014938239988, 1496.633575606299928, 206.8275456630500173 ) ) ;
#17313 = CARTESIAN_POINT ( 'NONE',  ( -4.998515195425000002, 1516.787536375099990, 213.1617432482970003 ) ) ;
#17315 =( BOUNDED_SURFACE ( )  B_SPLINE_SURFACE ( 3, 2, ( 
 ( #78000, #78559, #44978 ),
 ( #52818, #25918, #36550 ),
 ( #103757, #8577, #19167 ),
 ( #102618, #216, #61782 ),
 ( #76909, #86396, #27058 ),
 ( #62337, #1875, #28147 ),
 ( #42747, #69634, #51151 ),
 ( #17509, #1306, #35446 ),
 ( #10808, #68519, #16949 ),
 ( #95906, #44417, #61244 ),
 ( #9685, #53373, #60116 ),
 ( #94234, #34341, #18618 ),
 ( #86949, #10241, #77458 ),
 ( #36009, #70201, #26480 ) ),
 .UNSPECIFIED., .F., .F., .F. ) 
 B_SPLINE_SURFACE_WITH_KNOTS ( ( 4, 2, 2, 2, 2, 2, 4 ),
 ( 3, 3 ),
 ( 2.252972114424878214E-16, 0.0009440840677147236759, 0.001416126101571972811, 0.001888168135429222055, 0.002360210169286471298, 0.002832252203143720542, 0.003776336270858219029 ),
 ( 0.000000000000000000, 1.000000000000000000 ),
 .UNSPECIFIED. ) 
 GEOMETRIC_REPRESENTATION_ITEM ( )  RATIONAL_B_SPLINE_SURFACE ( (
 ( 1.000000000000000000, 0.8070209408749953184, 1.000000000000000000),
 ( 1.000000000000000000, 0.8215603905291239961, 1.000000000000000000),
 ( 1.000000000000000000, 0.8340988699051420374, 1.000000000000000000),
 ( 1.000000000000000000, 0.8516751610463629829, 1.000000000000000000),
 ( 1.000000000000000000, 0.8573697395147750200, 1.000000000000000000),
 ( 1.000000000000000000, 0.8683586635668578690, 1.000000000000000000),
 ( 1.000000000000000000, 0.8736518481705473071, 1.000000000000000000),
 ( 1.000000000000000000, 0.8840377753033259456, 1.000000000000000000),
 ( 1.000000000000000000, 0.8891294171308693484, 1.000000000000000000),
 ( 1.000000000000000000, 0.8992456600572363845, 1.000000000000000000),
 ( 1.000000000000000000, 0.9042785869256293463, 1.000000000000000000),
 ( 1.000000000000000000, 0.9189749222831727904, 1.000000000000000000),
 ( 1.000000000000000000, 0.9283978182353632702, 1.000000000000000000),
 ( 1.000000000000000000, 0.9376006582765943342, 1.000000000000000000) ) ) 
 REPRESENTATION_ITEM ( '' )  SURFACE ( )  );
#17314 = CARTESIAN_POINT ( 'NONE',  ( -15.08395737488610067, 1420.916320493289959, 206.4749953940769842 ) ) ;
#17316 = CARTESIAN_POINT ( 'NONE',  ( 0.1686318752242309815, 1481.134048488709823, 182.0456757912619992 ) ) ;
#17318 = ORIENTED_EDGE ( 'NONE', *, *, #108128, .F. ) ;
#17317 = CARTESIAN_POINT ( 'NONE',  ( 4.093882882269999968, 1442.069604321789939, 216.9756720149090086 ) ) ;
#17319 = CARTESIAN_POINT ( 'NONE',  ( -27.23063139319997816, 1444.324653571829003, 161.8596747266978753 ) ) ;
#17320 = EDGE_CURVE ( 'NONE', #77609, #43746, #21586, .T. ) ;
#17321 = FACE_OUTER_BOUND ( 'NONE', #80797, .T. ) ;
#17322 = DIRECTION ( 'NONE',  ( 1.755985294532469921E-16, -1.000000000000000000, 1.338183447452831989E-16 ) ) ;
#17323 = CARTESIAN_POINT ( 'NONE',  ( -32.00451504911058720, 1524.843416604514459, 216.1170911566689767 ) ) ;
#17324 = CARTESIAN_POINT ( 'NONE',  ( -7.381443632628819529, 1508.551704407720081, 219.0920119588899979 ) ) ;
#17325 = ORIENTED_EDGE ( 'NONE', *, *, #43617, .T. ) ;
#17326 = CARTESIAN_POINT ( 'NONE',  ( -10.57842363610000014, 1471.306182025889939, 209.0456894757570296 ) ) ;
#17327 = FACE_OUTER_BOUND ( 'NONE', #92989, .T. ) ;
#17328 = CARTESIAN_POINT ( 'NONE',  ( -16.76079633530000024, 1415.087818611729972, 211.7983980607679939 ) ) ;
#17329 = CARTESIAN_POINT ( 'NONE',  ( 6.245177529333449939, 1505.788460192030016, 215.5597741259620079 ) ) ;
#17330 = EDGE_CURVE ( 'NONE', #63715, #33885, #39139, .T. ) ;
#17331 = CARTESIAN_POINT ( 'NONE',  ( -1.839380708780000040, 1507.096886517889970, 221.8368464039990045 ) ) ;
#17332 = CARTESIAN_POINT ( 'NONE',  ( -3.430374836980000008, 1431.708658569990121, 216.7924588047190184 ) ) ;
#17333 = CARTESIAN_POINT ( 'NONE',  ( -10.62349018368750109, 1471.736129748900112, 206.9324528759129862 ) ) ;
#17334 = AXIS2_PLACEMENT_3D ( 'NONE', #9044, #85194, #66781 ) ;
#17335 = CARTESIAN_POINT ( 'NONE',  ( -13.72624666664203552, 1519.551704408389924, 195.8110037932692933 ) ) ;
#17336 = CARTESIAN_POINT ( 'NONE',  ( -11.15738186299999946, 1390.939237837450037, 203.8452286657090156 ) ) ;
#17337 = CARTESIAN_POINT ( 'NONE',  ( -83.83445332652270565, 1385.172051411020220, 287.6040778670190434 ) ) ;
#17338 = CARTESIAN_POINT ( 'NONE',  ( -11.66658784013729999, 1391.913060387289988, 209.7120188154370339 ) ) ;
#17339 = CARTESIAN_POINT ( 'NONE',  ( 11.67851423121779852, 1427.517936626490155, 209.0836788490910010 ) ) ;
#17340 = ORIENTED_EDGE ( 'NONE', *, *, #93708, .F. ) ;
#17341 = CARTESIAN_POINT ( 'NONE',  ( 13.14421740897469704, 1443.086052842850677, 164.8757063741590230 ) ) ;
#17343 = ORIENTED_EDGE ( 'NONE', *, *, #921, .F. ) ;
#17342 = CARTESIAN_POINT ( 'NONE',  ( -107.4477384240240099, 1379.886883745280102, 299.0757736425410371 ) ) ;
#17344 = CARTESIAN_POINT ( 'NONE',  ( 2.500011071270000329, 1474.146030601790017, 219.4741456703989968 ) ) ;
#17345 = CARTESIAN_POINT ( 'NONE',  ( 27.34567353230000109, 1509.867992349329825, 219.5431460416980087 ) ) ;
#17346 = CARTESIAN_POINT ( 'NONE',  ( -7.945335120643528093, 1363.374344492768842, 207.6218459616988241 ) ) ;
#17347 = CARTESIAN_POINT ( 'NONE',  ( -6.022896404259999947, 1495.447110633389912, 199.4947492194089875 ) ) ;
#17348 = EDGE_CURVE ( 'NONE', #45555, #7001, #61913, .T. ) ;
#17349 = CARTESIAN_POINT ( 'NONE',  ( 0.5717981366250000086, 1450.893092756410169, 154.2461502948980012 ) ) ;
#17350 = CARTESIAN_POINT ( 'NONE',  ( -11.60004869885204393, 1427.240389456164394, 134.3215321853161015 ) ) ;
#17351 = CARTESIAN_POINT ( 'NONE',  ( 19.11061305480268402, 1438.203271981198668, 213.0090273355756381 ) ) ;
#17352 = CARTESIAN_POINT ( 'NONE',  ( 2.489939931649999938, 1417.821760099730000, 233.9513212198979772 ) ) ;
#17353 = CARTESIAN_POINT ( 'NONE',  ( 5.094924673369999546, 1446.258997694789969, 201.5711013011589898 ) ) ;
#17354 = CARTESIAN_POINT ( 'NONE',  ( -8.530891852070000780, 1512.492641972989759, 210.8763812180689854 ) ) ;
#17355 = CARTESIAN_POINT ( 'NONE',  ( -8.962252599310001955, 1366.920250605820002, 207.6218459616989946 ) ) ;
#17356 = CARTESIAN_POINT ( 'NONE',  ( -2.416533552610000246, 1456.578277723489919, 199.9325152207989902 ) ) ;
#17357 = EDGE_CURVE ( 'NONE', #44537, #80364, #60609, .T. ) ;
#17358 = CARTESIAN_POINT ( 'NONE',  ( 1.701729820345000199, 1516.969638403840008, 206.2395199527169893 ) ) ;
#17359 = CIRCLE ( 'NONE', #38813, 0.9999999999999986677 ) ;
#17360 = CARTESIAN_POINT ( 'NONE',  ( 4.239021759200000794, 1446.365493823910128, 162.7142476321979814 ) ) ;
#17361 = DIRECTION ( 'NONE',  ( -1.876463901673629690E-05, 8.203947739369057955E-07, 0.9999999998236077658 ) ) ;
#17363 = B_SPLINE_CURVE_WITH_KNOTS ( 'NONE', 5,
 ( #46399, #107918, #63744, #5463, #30101, #97857 ),
 .UNSPECIFIED., .F., .F.,
 ( 6, 6 ),
 ( 0.000000000000000000, 1.000000000000000000 ),
 .UNSPECIFIED. ) ;
#17362 = CARTESIAN_POINT ( 'NONE',  ( 20.14111335559999816, 1472.214279811229972, 269.5303638422980157 ) ) ;
#17365 = ORIENTED_EDGE ( 'NONE', *, *, #68866, .T. ) ;
#17364 = CARTESIAN_POINT ( 'NONE',  ( 2.020666342550000216, 1495.217427720489923, 220.5028442773989923 ) ) ;
#17366 = ADVANCED_FACE ( 'NONE', ( #21543 ), #55755, .T. ) ;
#17367 = LINE ( 'NONE', #618, #92116 ) ;
#17368 = VERTEX_POINT ( 'NONE', #46800 ) ;
#17369 = CARTESIAN_POINT ( 'NONE',  ( -16.25286372485815178, 1514.564622118826492, 223.9142624678142681 ) ) ;
#17370 = CARTESIAN_POINT ( 'NONE',  ( -23.43227205760000231, 1410.913138759029835, 206.1403821866979911 ) ) ;
#17372 = CARTESIAN_POINT ( 'NONE',  ( 17.03258580107809905, 1409.880850962159911, 192.7013530600950162 ) ) ;
#17371 = CARTESIAN_POINT ( 'NONE',  ( -11.01180412374380069, 1426.052342128100008, 99.91299076298089687 ) ) ;
#17373 = CARTESIAN_POINT ( 'NONE',  ( 0.7578857918350010436, 1516.872851364150165, 211.6022732247369902 ) ) ;
#17374 = CARTESIAN_POINT ( 'NONE',  ( 17.96796222303624191, 1509.660108813923898, 185.0969589919148461 ) ) ;
#17375 = CARTESIAN_POINT ( 'NONE',  ( 21.95768443299136052, 1524.412455883367329, 233.6991302426335437 ) ) ;
#17376 = CARTESIAN_POINT ( 'NONE',  ( -20.04379692219999853, 1410.189666917429804, 264.7217003517980061 ) ) ;
#17377 = CARTESIAN_POINT ( 'NONE',  ( 17.24816121598360041, 1509.523746382970103, 233.0580511170819875 ) ) ;
#17378 = CARTESIAN_POINT ( 'NONE',  ( 17.28674646035066687, 1460.161652801043374, 228.5469262299488094 ) ) ;
#17379 = PRODUCT_CONTEXT ( 'NONE', #108540, 'mechanical' ) ;
#17380 = CARTESIAN_POINT ( 'NONE',  ( 3.179309441343999953, 1508.551704408389924, 214.0112856217869819 ) ) ;
#17381 = CARTESIAN_POINT ( 'NONE',  ( -38.91668594174339546, 1439.604252461880151, 136.6912434827079892 ) ) ;
#17382 = VERTEX_POINT ( 'NONE', #80930 ) ;
#17383 = CARTESIAN_POINT ( 'NONE',  ( 12.22548255495519953, 1396.339983646510063, 207.2249384526400036 ) ) ;
#17384 = CARTESIAN_POINT ( 'NONE',  ( 10.49671714463670114, 1460.103773102299783, 206.1611881418880046 ) ) ;
#17385 = EDGE_CURVE ( 'NONE', #110691, #98390, #98054, .T. ) ;
#17386 = CARTESIAN_POINT ( 'NONE',  ( -16.89883965940000365, 1458.595428821529822, 229.9355491509979856 ) ) ;
#17387 = ORIENTED_EDGE ( 'NONE', *, *, #96111, .T. ) ;
#17388 = ORIENTED_EDGE ( 'NONE', *, *, #51368, .F. ) ;
#17389 = AXIS2_PLACEMENT_3D ( 'NONE', #99389, #98299, #22667 ) ;
#17390 = CARTESIAN_POINT ( 'NONE',  ( -2.416798835000000256, 1426.601114010129777, 146.0361887655980127 ) ) ;
#17391 = CARTESIAN_POINT ( 'NONE',  ( 1.010302734856489960E-14, 1421.486528603629949, 147.6332008705779799 ) ) ;
#17392 = CARTESIAN_POINT ( 'NONE',  ( -6.218080811995890578, 1508.050148686579860, 220.4488469885409927 ) ) ;
#17393 = CYLINDRICAL_SURFACE ( 'NONE', #4414, 2.000000000000002220 ) ;
#17394 = ADVANCED_FACE ( 'NONE', ( #5879 ), #72173, .F. ) ;
#17395 = DIRECTION ( 'NONE',  ( -0.6736849260863839728, 0.000000000000000000, 0.7390186874254150995 ) ) ;
#17396 = VECTOR ( 'NONE', #8265, 1000.000000000000000 ) ;
#17397 = CARTESIAN_POINT ( 'NONE',  ( -14.52593930399999955, 1470.476261423729966, 229.9537273268980186 ) ) ;
#17398 = CARTESIAN_POINT ( 'NONE',  ( 1.949295068010844068, 1516.541277319971186, 216.3661146437771947 ) ) ;
#17399 = CARTESIAN_POINT ( 'NONE',  ( 9.315848094708581328, 1450.961990831169942, 207.9471377613749894 ) ) ;
#17400 = CARTESIAN_POINT ( 'NONE',  ( -10.34436050340000079, 1391.793768386910187, 215.1256036177990154 ) ) ;
#17401 = CARTESIAN_POINT ( 'NONE',  ( -105.5483579447400047, 1384.891159839150077, 296.9529443240709838 ) ) ;
#17402 = ORIENTED_EDGE ( 'NONE', *, *, #100810, .T. ) ;
#17403 = CARTESIAN_POINT ( 'NONE',  ( 0.7386049046750020608, 1517.122674412569950, 202.5597518628069906 ) ) ;
#17404 = CARTESIAN_POINT ( 'NONE',  ( 7.719640903004999721, 1516.939452820819952, 209.1117431028050078 ) ) ;
#17405 = ORIENTED_EDGE ( 'NONE', *, *, #28400, .T. ) ;
#17406 = CARTESIAN_POINT ( 'NONE',  ( 10.79382126600000014, 1414.913060387329779, 222.1041115775979904 ) ) ;
#17407 = CARTESIAN_POINT ( 'NONE',  ( 3.179695852932951095, 1511.827406192486478, 217.0650637690530687 ) ) ;
#17408 = EDGE_LOOP ( 'NONE', ( #61118, #70744, #95378, #98258 ) ) ;
#17409 = CARTESIAN_POINT ( 'NONE',  ( -14.30561690719999923, 1416.274718424630009, 221.5178275245980046 ) ) ;
#17410 = CARTESIAN_POINT ( 'NONE',  ( -12.53517974735311391, 1442.773887286368335, 169.5044317858154272 ) ) ;
#17411 = DIRECTION ( 'NONE',  ( 0.000000000000000000, 1.000000000000000000, 0.000000000000000000 ) ) ;
#17412 = CARTESIAN_POINT ( 'NONE',  ( -7.217719862338501713, 1489.850359190520294, 217.3448569486999133 ) ) ;
#17413 = CARTESIAN_POINT ( 'NONE',  ( -4.627424403969999211, 1421.862729080530244, 185.4837249234980163 ) ) ;
#17414 = CARTESIAN_POINT ( 'NONE',  ( -0.4392564938140909869, 1517.051704408389924, 216.6483608045730023 ) ) ;
#17415 = DIRECTION ( 'NONE',  ( -1.755985294532469921E-16, 1.000000000000000000, -1.338183447452831989E-16 ) ) ;
#17416 = CARTESIAN_POINT ( 'NONE',  ( -10.04683427352762592, 1410.638564451745424, 188.4446185365461872 ) ) ;
#17417 = CARTESIAN_POINT ( 'NONE',  ( -37.65558013879999777, 1379.730903953030065, 220.7433301062589805 ) ) ;
#17418 = CARTESIAN_POINT ( 'NONE',  ( -15.77309112549999881, 1462.582351688929975, 223.0144108837980070 ) ) ;
#17420 = CARTESIAN_POINT ( 'NONE',  ( -15.13342374508840038, 1507.606285602760181, 191.8462590464540085 ) ) ;
#17419 = CARTESIAN_POINT ( 'NONE',  ( 17.31926483839999875, 1459.104205613330123, 228.6771837914980097 ) ) ;
#17421 = CARTESIAN_POINT ( 'NONE',  ( 15.31719370542390024, 1507.616838218729754, 226.2466523219209762 ) ) ;
#17422 = TOROIDAL_SURFACE ( 'NONE', #101432, 7.500000000000000000, 0.2999999999999999889 ) ;
#17423 = CARTESIAN_POINT ( 'NONE',  ( -2.499950770261460065, 1420.115583131989979, 90.95036697406219162 ) ) ;
#17424 = ORIENTED_EDGE ( 'NONE', *, *, #60483, .F. ) ;
#17425 = CARTESIAN_POINT ( 'NONE',  ( 18.03232038437150209, 1424.487826474579833, 224.4511121296560248 ) ) ;
#17426 = CARTESIAN_POINT ( 'NONE',  ( -17.06401309437357483, 1526.329757971584741, 181.0652997614164974 ) ) ;
#17427 = CARTESIAN_POINT ( 'NONE',  ( -2.897197017797513485, 1484.284914968770636, 183.3151737225298916 ) ) ;
#17428 = CARTESIAN_POINT ( 'NONE',  ( -14.35630723490000094, 1415.677402202029953, 213.7176790535390012 ) ) ;
#17430 = ORIENTED_EDGE ( 'NONE', *, *, #18739, .T. ) ;
#17429 = CARTESIAN_POINT ( 'NONE',  ( -11.25861335519799944, 1500.241393668199862, 210.8792608383079994 ) ) ;
#17431 = B_SPLINE_CURVE_WITH_KNOTS ( 'NONE', 5,
 ( #85032, #42487, #76643, #8873, #34642, #26792 ),
 .UNSPECIFIED., .F., .F.,
 ( 6, 6 ),
 ( -2.000000000000000000, 0.000000000000000000 ),
 .UNSPECIFIED. ) ;
#17432 = CARTESIAN_POINT ( 'NONE',  ( -8.371636071799999357, 1384.910415699319856, 199.7750054352590041 ) ) ;
#17433 = CARTESIAN_POINT ( 'NONE',  ( -12.78654151568484210, 1416.818673872114459, 195.1663110372768983 ) ) ;
#17434 = CARTESIAN_POINT ( 'NONE',  ( -11.76003987410000029, 1426.815402127429934, 145.7846991655979991 ) ) ;
#17435 = LINE ( 'NONE', #85770, #7457 ) ;
#17436 = CARTESIAN_POINT ( 'NONE',  ( -4.121463778139999867, 1441.582014689759944, 184.1216907019980340 ) ) ;
#17437 = CARTESIAN_POINT ( 'NONE',  ( 11.86610049529999955, 1432.336025054189804, 149.9824163679980131 ) ) ;
#17438 = CARTESIAN_POINT ( 'NONE',  ( 1.716045945209999868, 1509.007693206030126, 179.5167849949980052 ) ) ;
#17439 = CARTESIAN_POINT ( 'NONE',  ( -15.48184693596499883, 1513.486273623730085, 223.7694329180669968 ) ) ;
#17440 = CARTESIAN_POINT ( 'NONE',  ( 12.37239278490000061, 1410.398668474930219, 228.8262060006979937 ) ) ;
#17442 = CARTESIAN_POINT ( 'NONE',  ( -10.87893655264359971, 1481.987309145149766, 207.2182299508939991 ) ) ;
#17441 = CARTESIAN_POINT ( 'NONE',  ( -23.68957226320000231, 1508.007654220830091, 223.0814278728979900 ) ) ;
#17444 = CARTESIAN_POINT ( 'NONE',  ( -16.17890917207000001, 1459.145060716636181, 230.7168571672029884 ) ) ;
#17443 = AXIS2_PLACEMENT_3D ( 'NONE', #30561, #73124, #54692 ) ;
#17445 = ORIENTED_EDGE ( 'NONE', *, *, #96295, .F. ) ;
#17446 = CARTESIAN_POINT ( 'NONE',  ( 0.7353365397730019515, 1516.995911393979895, 206.2425275143270085 ) ) ;
#17447 = CARTESIAN_POINT ( 'NONE',  ( 18.29857331400000220, 1408.824872542730191, 266.8292035143980456 ) ) ;
#17448 = CARTESIAN_POINT ( 'NONE',  ( 7.512750208045280154, 1509.038615934079871, 214.6352815289239970 ) ) ;
#17449 = CARTESIAN_POINT ( 'NONE',  ( 19.68669136100000117, 1449.730997079720055, 193.0903452006980103 ) ) ;
#17450 = CARTESIAN_POINT ( 'NONE',  ( -0.2075483795266540032, 1507.637022368109911, 237.3602291488149945 ) ) ;
#17451 = CARTESIAN_POINT ( 'NONE',  ( 32.38601978689747796, 1523.530870145309109, 216.1237258104796410 ) ) ;
#17452 = FACE_OUTER_BOUND ( 'NONE', #68604, .T. ) ;
#17453 = DIRECTION ( 'NONE',  ( -0.9057425179572490270, -0.3859240281742280509, 0.1751945651047430164 ) ) ;
#17454 = CARTESIAN_POINT ( 'NONE',  ( -16.24601214319999798, 1417.782919326170031, 204.8291993099989838 ) ) ;
#17455 = CARTESIAN_POINT ( 'NONE',  ( -13.49821838159999920, 1443.540395460420086, 187.3682244081979889 ) ) ;
#17456 = CARTESIAN_POINT ( 'NONE',  ( -19.76034656259999878, 1519.913060387329779, 221.5779544268979748 ) ) ;
#17457 = CARTESIAN_POINT ( 'NONE',  ( -15.84432591830269743, 1419.853212859319910, 210.7451195136700051 ) ) ;
#17458 = CARTESIAN_POINT ( 'NONE',  ( -2.674172889476567061, 1457.854889596452495, 229.5525240896329819 ) ) ;
#17459 = EDGE_LOOP ( 'NONE', ( #40128, #8393, #29023, #107649 ) ) ;
#17460 = CARTESIAN_POINT ( 'NONE',  ( -2.625066807925000134, 1511.873873588870083, 201.5029411752969963 ) ) ;
#17461 = CARTESIAN_POINT ( 'NONE',  ( -14.92043776882830031, 1409.434093555360050, 208.4812704053670132 ) ) ;
#17462 = CIRCLE ( 'NONE', #80082, 1.999994602261522036 ) ;
#17463 = CARTESIAN_POINT ( 'NONE',  ( -12.36537603459249901, 1507.934286694269986, 209.0016465257290008 ) ) ;
#17464 = CARTESIAN_POINT ( 'NONE',  ( 21.54905603439488004, 1524.816548299036867, 234.5808913040066841 ) ) ;
#17465 = CARTESIAN_POINT ( 'NONE',  ( -18.10264220770000065, 1472.346832327329821, 269.5453876878980282 ) ) ;
#17466 = B_SPLINE_CURVE_WITH_KNOTS ( 'NONE', 3,
 ( #58402, #7431, #39938, #74108 ),
 .UNSPECIFIED., .F., .F.,
 ( 4, 4 ),
 ( -21.04897729589999855, -13.79090555186670031 ),
 .UNSPECIFIED. ) ;
#17467 = CARTESIAN_POINT ( 'NONE',  ( -5.696033815719999893, 1448.953839979589929, 210.9996425703789953 ) ) ;
#17468 = CARTESIAN_POINT ( 'NONE',  ( -13.24888725095132358, 1513.564944022936288, 192.3379340659209618 ) ) ;
#17469 = CARTESIAN_POINT ( 'NONE',  ( -24.29629205419795923, 1444.606322822562333, 211.3000715094191264 ) ) ;
#17470 = CARTESIAN_POINT ( 'NONE',  ( -75.79932541657819911, 1384.647805970779928, 300.7287927689640128 ) ) ;
#17471 = CARTESIAN_POINT ( 'NONE',  ( -26.14076515983080284, 1384.961658909369817, 203.7233559922780159 ) ) ;
#17472 = CARTESIAN_POINT ( 'NONE',  ( 18.03020053570940107, 1424.665392966000127, 225.2865191207559690 ) ) ;
#17473 = VECTOR ( 'NONE', #34737, 1000.000000000000000 ) ;
#17474 = CARTESIAN_POINT ( 'NONE',  ( -6.620521211799999861, 1440.451554611820029, 154.8188655977980090 ) ) ;
#17475 = DIRECTION ( 'NONE',  ( 9.404037925578970303E-16, -1.000000000000000000, 2.220446049250000002E-16 ) ) ;
#17476 = CARTESIAN_POINT ( 'NONE',  ( 9.200258835159148774, 1470.370198451841816, 213.4174792157946854 ) ) ;
#17477 = CARTESIAN_POINT ( 'NONE',  ( -0.01912617869007780455, 1347.932019967219958, 212.1218459616989946 ) ) ;
#17478 = CIRCLE ( 'NONE', #80091, 33.13701971169416538 ) ;
#17479 = CARTESIAN_POINT ( 'NONE',  ( -23.27028561550000063, 1410.220846923830095, 206.2737248513280122 ) ) ;
#17480 = DIRECTION ( 'NONE',  ( -0.7414773880254664773, 0.000000000000000000, 0.6709778558543730842 ) ) ;
#17481 = ADVANCED_FACE ( 'NONE', ( #1919 ), #79172, .T. ) ;
#17482 = CARTESIAN_POINT ( 'NONE',  ( 3.813345290629999607, 1485.053057143089973, 219.5629744241990124 ) ) ;
#17483 = CARTESIAN_POINT ( 'NONE',  ( 3.909229062960000167, 1422.563626564619881, 194.1920524380990116 ) ) ;
#17484 = EDGE_CURVE ( 'NONE', #90113, #28026, #80613, .T. ) ;
#17485 = CARTESIAN_POINT ( 'NONE',  ( -12.14468697209110104, 1448.084251977639951, 193.6129773812070027 ) ) ;
#17486 = CARTESIAN_POINT ( 'NONE',  ( 5.232600787119999985, 1437.236778738189969, 228.7402956028990104 ) ) ;
#17487 = CARTESIAN_POINT ( 'NONE',  ( 16.64711273906109668, 1523.843263703802904, 180.4998296529583683 ) ) ;
#17488 = CARTESIAN_POINT ( 'NONE',  ( 19.38665597314309963, 1498.811989926609840, 221.8202338665909963 ) ) ;
#17490 = CARTESIAN_POINT ( 'NONE',  ( -8.872398163489998879, 1383.598668384430084, 200.1252679808089852 ) ) ;
#17489 = CARTESIAN_POINT ( 'NONE',  ( -22.12673812610000112, 1409.685743109030000, 209.8966867356670036 ) ) ;
#17491 = CARTESIAN_POINT ( 'NONE',  ( 11.71754611134989865, 1426.708450837530108, 142.7745908721059891 ) ) ;
#17492 = CARTESIAN_POINT ( 'NONE',  ( 9.820595928116450324, 1435.622055171000056, 209.3846138168819948 ) ) ;
#17493 = CARTESIAN_POINT ( 'NONE',  ( -10.94672739099999959, 1491.935509946189995, 210.5292650763190068 ) ) ;
#17494 = CARTESIAN_POINT ( 'NONE',  ( 8.887962835699010355, 1449.864045084309964, 203.7541360747050021 ) ) ;
#17495 = CARTESIAN_POINT ( 'NONE',  ( -0.02428268839107049909, 1420.196391110329841, 183.9091636877150222 ) ) ;
#17496 = CARTESIAN_POINT ( 'NONE',  ( 5.775236792744999903, 1516.804776704140068, 204.1142572851869943 ) ) ;
#17498 = CARTESIAN_POINT ( 'NONE',  ( -0.9520131522009163128, 1397.942409892914839, 222.1218459635456099 ) ) ;
#17497 = CIRCLE ( 'NONE', #110487, 2.000000000000001776 ) ;
#17499 = CARTESIAN_POINT ( 'NONE',  ( -3.484680539907339281, 1440.761655002041607, 156.7439059081135042 ) ) ;
#17500 = FACE_BOUND ( 'NONE', #20867, .T. ) ;
#17501 = CARTESIAN_POINT ( 'NONE',  ( 1.399923991030000092, 1507.072109554030021, 236.8180446778980013 ) ) ;
#17502 = CARTESIAN_POINT ( 'NONE',  ( 9.603890370815909350, 1503.574939094829915, 216.4415450440779978 ) ) ;
#17503 = CARTESIAN_POINT ( 'NONE',  ( -9.918481311761176755, 1422.650748571832310, 210.6689247654111909 ) ) ;
#17505 = ORIENTED_EDGE ( 'NONE', *, *, #35220, .F. ) ;
#17504 = CARTESIAN_POINT ( 'NONE',  ( -65.39490631584679647, 1379.739707105699836, 275.4685780489909916 ) ) ;
#17506 = EDGE_CURVE ( 'NONE', #55998, #94471, #52665, .T. ) ;
#17507 = ORIENTED_EDGE ( 'NONE', *, *, #54487, .F. ) ;
#17508 = CARTESIAN_POINT ( 'NONE',  ( 11.94196968702019923, 1433.494760352820094, 149.8932996039710019 ) ) ;
#17509 = CARTESIAN_POINT ( 'NONE',  ( 21.66432897272961000, 1525.042412244735260, 184.7096312766485084 ) ) ;
#17510 = ORIENTED_EDGE ( 'NONE', *, *, #110394, .F. ) ;
#17511 = FACE_OUTER_BOUND ( 'NONE', #101726, .T. ) ;
#17512 = CARTESIAN_POINT ( 'NONE',  ( -22.97499040840000006, 1509.490920569430045, 193.4133551238979862 ) ) ;
#17513 = CARTESIAN_POINT ( 'NONE',  ( -7.561556810379999938, 1385.457612210709840, 219.0574708042989869 ) ) ;
#17515 = CARTESIAN_POINT ( 'NONE',  ( 2.368833328420000051, 1427.018531676430030, 133.6118001900980232 ) ) ;
#17514 = CARTESIAN_POINT ( 'NONE',  ( -0.7790504975549988886, 1442.687250042790083, 200.2740176171789983 ) ) ;
#17516 = CARTESIAN_POINT ( 'NONE',  ( 13.05116814624009969, 1498.106535309839956, 232.7503740319400265 ) ) ;
#17517 = CARTESIAN_POINT ( 'NONE',  ( 7.424385365560000061, 1507.634762273629804, 182.7152872762979996 ) ) ;
#17518 = FACE_OUTER_BOUND ( 'NONE', #1057, .T. ) ;
#17519 = CARTESIAN_POINT ( 'NONE',  ( 15.94344812639999631, 1409.469817864229981, 225.2684562213980257 ) ) ;
#17520 = CARTESIAN_POINT ( 'NONE',  ( -6.933879441005000643, 1516.560253536979872, 211.6083207129769903 ) ) ;
#17521 = CARTESIAN_POINT ( 'NONE',  ( 4.809053151022830264, 1396.080996231650033, 199.1914258291379838 ) ) ;
#17522 = CARTESIAN_POINT ( 'NONE',  ( 14.27868134601139971, 1415.948038442740199, 197.0356935349670096 ) ) ;
#17523 = CARTESIAN_POINT ( 'NONE',  ( 11.56039809610000013, 1431.104951558719904, 151.0881388422979796 ) ) ;
#17524 = CARTESIAN_POINT ( 'NONE',  ( 6.470331875434999880, 1513.423632355030122, 201.6536730834770026 ) ) ;
#17525 = ORIENTED_EDGE ( 'NONE', *, *, #28225, .T. ) ;
#17526 = CARTESIAN_POINT ( 'NONE',  ( 13.76767358908210070, 1435.930931524279913, 150.2736258322640026 ) ) ;
#17527 = EDGE_LOOP ( 'NONE', ( #98526, #106148, #61048, #24416 ) ) ;
#17528 = EDGE_LOOP ( 'NONE', ( #48906, #25476, #62641, #75701 ) ) ;
#17529 = CARTESIAN_POINT ( 'NONE',  ( 13.01250632543007235, 1444.867273317868239, 169.4194736224069686 ) ) ;
#17530 = CARTESIAN_POINT ( 'NONE',  ( -1.528923355689999930, 1467.018653446829831, 235.3777442162979980 ) ) ;
#17531 = AXIS2_PLACEMENT_3D ( 'NONE', #98076, #97537, #55008 ) ;
#17532 = CARTESIAN_POINT ( 'NONE',  ( -9.655138005699368975, 1473.799620413477442, 205.6226705925480474 ) ) ;
#17533 = CARTESIAN_POINT ( 'NONE',  ( -6.941727290454999810, 1516.882217593000178, 216.4530290611770056 ) ) ;
#17535 = CARTESIAN_POINT ( 'NONE',  ( -7.887702616237564079, 1512.266405701032454, 212.0598010800264888 ) ) ;
#17534 = B_SPLINE_CURVE_WITH_KNOTS ( 'NONE', 3,
 ( #72577, #47917, #40064, #22677, #30559, #56323, #56877, #74243, #31107, #23248, #13181, #64748, #98860, #31655, #90454, #72052, #98308, #106705, #13732, #48486, #82052, #39517, #108373, #12658, #91007, #81495, #4270, #82625, #65835, #73692, #14297, #57446, #29445, #91573, #14847, #49038, #83174, #6464, #106168, #63644, #97759, #21030, #55234, #21585, #89366, #64186, #46837, #80966, #55792, #38401, #29995 ),
 .UNSPECIFIED., .F., .F.,
 ( 4, 2, 2, 2, 1, 2, 2, 2, 1, 1, 1, 1, 2, 2, 2, 2, 2, 1, 1, 1, 1, 2, 2, 2, 2, 2, 1, 1, 2, 2, 4 ),
 ( 0.000000000000000000, 0.03124999999711828430, 0.06249999999423656860, 0.09374999999135485984, 0.1093749999899146230, 0.1171874999892398156, 0.1249999999885650082, 0.1874999999835806064, 0.2187499999810354201, 0.2343749999797607175, 0.2421874999790658567, 0.2460937499787189953, 0.2480468749786066129, 0.2499999999784942584, 0.3749999999675763807, 0.4374999999621191349, 0.4687499999594437194, 0.4843749999581046795, 0.4921874999573854215, 0.4960937499569785802, 0.4980468749568228715, 0.4990234374567449338, 0.4999999999566671072, 0.6249999999676451035, 0.6874999999731339351, 0.7187499999758150127, 0.7343749999771556070, 0.7421874999778810267, 0.7460937499782968052, 0.7499999999787125837, 1.000000000000000000 ),
 .UNSPECIFIED. ) ;
#17536 = EDGE_CURVE ( 'NONE', #88847, #76760, #43648, .T. ) ;
#17537 = CARTESIAN_POINT ( 'NONE',  ( 12.00800514267580077, 1421.841763435350003, 208.7871892364869950 ) ) ;
#17538 = CARTESIAN_POINT ( 'NONE',  ( -59.08254685325682232, 1379.721614939749088, 259.3076159164612591 ) ) ;
#17539 = CARTESIAN_POINT ( 'NONE',  ( -18.96272001720000233, 1380.296266888389937, 209.6316668868479951 ) ) ;
#17540 = EDGE_CURVE ( 'NONE', #20317, #34885, #69019, .T. ) ;
#17541 = EDGE_LOOP ( 'NONE', ( #64106, #73809, #77456, #15949 ) ) ;
#17542 = CARTESIAN_POINT ( 'NONE',  ( 7.322105067625000352, 1516.572193931679976, 206.2485165713470110 ) ) ;
#17543 = VERTEX_POINT ( 'NONE', #37700 ) ;
#17544 = CARTESIAN_POINT ( 'NONE',  ( 22.79168776688370102, 1440.913060387330006, 230.8904766920060183 ) ) ;
#17545 = CYLINDRICAL_SURFACE ( 'NONE', #49813, 1.999999999999997335 ) ;
#17546 = ORIENTED_EDGE ( 'NONE', *, *, #102850, .F. ) ;
#17547 = CARTESIAN_POINT ( 'NONE',  ( -11.49135376729999969, 1409.816935674130036, 189.2372629410979812 ) ) ;
#17548 = CARTESIAN_POINT ( 'NONE',  ( 7.962346576125000297, 1514.830240247470101, 215.1813356062270088 ) ) ;
#17550 = ORIENTED_EDGE ( 'NONE', *, *, #100780, .F. ) ;
#17549 = CARTESIAN_POINT ( 'NONE',  ( 2.280398975811160245, 1423.485262736610139, 192.6506460990210314 ) ) ;
#17551 = CARTESIAN_POINT ( 'NONE',  ( 24.58510744930000058, 1439.552595424130232, 212.5220241814980113 ) ) ;
#17552 = DIRECTION ( 'NONE',  ( 0.000000000000000000, -0.7071067811865474617, -0.7071067811865474617 ) ) ;
#17554 = CARTESIAN_POINT ( 'NONE',  ( -106.4203974090000031, 1384.309678820099862, 311.2870763412590236 ) ) ;
#17553 = AXIS2_PLACEMENT_3D ( 'NONE', #64310, #46958, #56445 ) ;
#17555 = DIRECTION ( 'NONE',  ( -0.8564730265368828421, -0.5161917810414575758, 0.000000000000000000 ) ) ;
#17556 = CARTESIAN_POINT ( 'NONE',  ( 10.81506866283119983, 1424.921186100899831, 144.1620444812269852 ) ) ;
#17557 = AXIS2_PLACEMENT_3D ( 'NONE', #91880, #67805, #16250 ) ;
#17558 = CARTESIAN_POINT ( 'NONE',  ( 4.618749068485000109, 1516.729202374750002, 215.6716084172169872 ) ) ;
#17559 = CARTESIAN_POINT ( 'NONE',  ( -3.549339293766919923, 1428.611355690149821, 200.4582084220010074 ) ) ;
#17560 = CARTESIAN_POINT ( 'NONE',  ( -21.80461142280000075, 1509.640046815429741, 189.9822974792980119 ) ) ;
#17561 = AXIS2_PLACEMENT_3D ( 'NONE', #79727, #47215, #1926 ) ;
#17562 = CARTESIAN_POINT ( 'NONE',  ( 5.513222314298020343, 1508.611138448550037, 216.4434734792089898 ) ) ;
#17563 = CARTESIAN_POINT ( 'NONE',  ( -6.933616859135000254, 1516.548716157039962, 211.4141532006069895 ) ) ;
#17564 = CARTESIAN_POINT ( 'NONE',  ( -11.84250961054740081, 1482.176269567949930, 208.0354447653020031 ) ) ;
#17565 = CARTESIAN_POINT ( 'NONE',  ( -17.17023220410861128, 1486.131980952480262, 187.8222342393189876 ) ) ;
#17566 = VECTOR ( 'NONE', #28000, 1000.000000000000000 ) ;
#17568 = VERTEX_POINT ( 'NONE', #70793 ) ;
#17567 = CARTESIAN_POINT ( 'NONE',  ( -79.40695482969999830, 1386.732498983730011, 283.0119451973590117 ) ) ;
#17569 = CARTESIAN_POINT ( 'NONE',  ( -69.45076499915620616, 1385.026108280010021, 294.4474613690360343 ) ) ;
#17570 = CARTESIAN_POINT ( 'NONE',  ( 32.03901053310000435, 1451.703008376129901, 250.0966427451979825 ) ) ;
#17571 = CARTESIAN_POINT ( 'NONE',  ( 2.923658500830763174, 1451.704853250206725, 183.8662944852202656 ) ) ;
#17572 = CARTESIAN_POINT ( 'NONE',  ( -11.76598840989999850, 1428.979790717830156, 145.3128034382980047 ) ) ;
#17573 = CARTESIAN_POINT ( 'NONE',  ( -7.229470473417760168, 1509.092253499190065, 236.9801883832320186 ) ) ;
#17574 = CARTESIAN_POINT ( 'NONE',  ( 10.86655197540000017, 1422.901418124660040, 206.8976527062889943 ) ) ;
#17576 = CARTESIAN_POINT ( 'NONE',  ( 17.99263301768839796, 1410.773178293809906, 222.9786793883430107 ) ) ;
#17575 = CARTESIAN_POINT ( 'NONE',  ( 3.448830483803564828, 1518.913060387330006, 243.0842028158767789 ) ) ;
#17577 = CARTESIAN_POINT ( 'NONE',  ( -9.938748489107151585, 1448.437396663140134, 208.6016734837719753 ) ) ;
#17578 = CARTESIAN_POINT ( 'NONE',  ( -107.1059704325560062, 1382.194773922719833, 310.1619100124009947 ) ) ;
#17579 = MECHANICAL_DESIGN_GEOMETRIC_PRESENTATION_REPRESENTATION (  '', ( #24767 ), #105219 ) ;
#17580 = EDGE_LOOP ( 'NONE', ( #53232, #59934, #70429, #16599 ) ) ;
#17581 = CARTESIAN_POINT ( 'NONE',  ( 2.286446325635000054, 1517.042661899400173, 204.4961520670869959 ) ) ;
#17582 = CARTESIAN_POINT ( 'NONE',  ( -10.10644227791819993, 1508.436924462359912, 218.7282801708559816 ) ) ;
#17583 = CARTESIAN_POINT ( 'NONE',  ( 29.19056935439999734, 1509.932417531129886, 206.4260805152879925 ) ) ;
#17584 = B_SPLINE_CURVE_WITH_KNOTS ( 'NONE', 5,
 ( #11378, #45550, #79690, #2995, #37116, #71316 ),
 .UNSPECIFIED., .F., .F.,
 ( 6, 6 ),
 ( -17.01656662094779904, -6.621488669319999687 ),
 .UNSPECIFIED. ) ;
#17585 = B_SPLINE_CURVE_WITH_KNOTS ( 'NONE', 3,
 ( #88229, #12617, #27759, #46796, #28872, #79834, #53538, #11520, #87684, #69794, #45696, #45139, #79280, #3140, #105587, #97168, #30513, #108329, #55750, #90408, #81451, #74741, #108879, #23206, #56277, #89869, #98267, #83128, #4224, #56833, #64148, #40570, #23757, #39475, #49544, #4757, #38901, #6425, #32171, #73083, #107223, #82011, #38356, #13138, #31612, #5875, #15350, #29955, #73645, #13687, #72535, #57406, #65789, #99910, #91531, #82584, #5316, #64702, #98819, #106665, #21538, #14809, #22081, #65242, #47322, #66356, #40018, #48995, #22628, #100475, #57944, #92076, #74197, #47873, #107776, #31061, #99354, #48446, #90967, #14256, #109988, #93707 ),
 .UNSPECIFIED., .F., .F.,
 ( 4, 2, 2, 1, 1, 1, 1, 2, 2, 2, 2, 1, 1, 1, 1, 1, 1, 2, 2, 2, 2, 2, 1, 1, 1, 1, 1, 1, 2, 2, 2, 2, 2, 2, 2, 1, 1, 1, 1, 1, 2, 2, 2, 2, 2, 1, 1, 1, 1, 1, 2, 2, 2, 4 ),
 ( 0.000000000000000000, 0.06249999999689971608, 0.09374999999534959494, 0.1093749999945813761, 0.1171874999941906192, 0.1210937499939952339, 0.1230468749938975065, 0.1240234374938485873, 0.1249999999937996542, 0.1874999999902269010, 0.2187499999884405799, 0.2343749999875474055, 0.2421874999870951839, 0.2460937499868637024, 0.2480468749867425493, 0.2490234374866871769, 0.2495117187366648337, 0.2497558593616537037, 0.2499999999866426015, 0.3124999999868266487, 0.3437499999869187972, 0.3593749999869604861, 0.3671874999869813583, 0.3710937499869957357, 0.3730468749870029521, 0.3740234374870101686, 0.3745117187370138323, 0.3747558593620157197, 0.3748779296745202716, 0.3749999999870247680, 0.4062499999879649049, 0.4374999999889049862, 0.4687499999898450675, 0.4843749999903206871, 0.4921874999905507253, 0.4960937499906657999, 0.4980468749907230319, 0.4990234374907395187, 0.4995117187407349668, 0.4997558593657326909, 0.4998779296782312476, 0.4999999999907298598, 0.6249999999927761118, 0.6874999999937994044, 0.7187499999943091078, 0.7343749999945639040, 0.7421874999946894702, 0.7460937499947539742, 0.7480468749947879470, 0.7490234374948067098, 0.7495117187448160356, 0.7499999999948252505, 0.8749999999974127363, 1.000000000000000000 ),
 .UNSPECIFIED. ) ;
#17586 = CARTESIAN_POINT ( 'NONE',  ( 24.51094252870000290, 1443.736757004859783, 213.5018118478279803 ) ) ;
#17587 = CARTESIAN_POINT ( 'NONE',  ( -4.326992699989999913, 1515.158586642790169, 209.1218459619010162 ) ) ;
#17588 = CARTESIAN_POINT ( 'NONE',  ( 3.550946725939999826, 1467.682858653789935, 218.4445632802489854 ) ) ;
#17589 = CARTESIAN_POINT ( 'NONE',  ( -20.01067139950000140, 1507.877425041529932, 188.9709217985979706 ) ) ;
#17590 = CARTESIAN_POINT ( 'NONE',  ( 28.39357473329010162, 1435.648819368660043, 136.1155384844830110 ) ) ;
#17591 = CARTESIAN_POINT ( 'NONE',  ( 35.47922246755190656, 1450.191545858459904, 136.2330231413669708 ) ) ;
#17592 = CARTESIAN_POINT ( 'NONE',  ( 3.199222159840339634E-15, 1458.117154428349977, 230.2906725803670156 ) ) ;
#17593 = CARTESIAN_POINT ( 'NONE',  ( -109.5445191200000039, 1385.771176860549986, 297.1603890872589773 ) ) ;
#17594 = CARTESIAN_POINT ( 'NONE',  ( 11.65588960887020065, 1480.025413490480105, 210.9188710873860089 ) ) ;
#17595 = CARTESIAN_POINT ( 'NONE',  ( 19.34601893677221440, 1526.333389947990327, 185.2009018889368406 ) ) ;
#17596 = DIRECTION ( 'NONE',  ( -0.5877852522924629231, 0.000000000000000000, 0.8090169943749548898 ) ) ;
#17597 = ORIENTED_EDGE ( 'NONE', *, *, #5075, .F. ) ;
#17598 = CARTESIAN_POINT ( 'NONE',  ( 19.01764264267215410, 1526.373507135059072, 185.3901233886903128 ) ) ;
#17599 = CARTESIAN_POINT ( 'NONE',  ( 3.418717339140886935, 1426.008825658123897, 185.1440916679583211 ) ) ;
#17600 = CARTESIAN_POINT ( 'NONE',  ( -4.487358476232119919, 1509.034524880150002, 212.9235703428400086 ) ) ;
#17601 = DIRECTION ( 'NONE',  ( -0.06436433998257497235, -0.7055452152167080992, -0.7057359145058558214 ) ) ;
#17602 = CARTESIAN_POINT ( 'NONE',  ( -0.4362016210640000113, 1416.994873689529868, 234.1618458712980271 ) ) ;
#17604 = CARTESIAN_POINT ( 'NONE',  ( -1.906499846882070084E-08, 1517.051704408389924, 209.1218459511669892 ) ) ;
#17603 = CARTESIAN_POINT ( 'NONE',  ( 12.67303841979999923, 1500.818571512490053, 210.2049276646989995 ) ) ;
#17605 = CARTESIAN_POINT ( 'NONE',  ( -28.49020455409999997, 1509.161987687429928, 209.1271010973100033 ) ) ;
#17606 = CARTESIAN_POINT ( 'NONE',  ( 7.747154353170000007, 1424.045375182409998, 212.1192621507390186 ) ) ;
#17607 = CARTESIAN_POINT ( 'NONE',  ( -11.58291379525149978, 1384.886121621980010, 218.9039716644460043 ) ) ;
#17608 = CARTESIAN_POINT ( 'NONE',  ( -12.49434536646978700, 1419.335010250987580, 228.5375418321167444 ) ) ;
#17609 = CARTESIAN_POINT ( 'NONE',  ( -21.04449625164730620, 1450.946923703476841, 144.4076044022301062 ) ) ;
#17610 = CARTESIAN_POINT ( 'NONE',  ( -7.113505352310000696, 1482.903954351189896, 201.0855788274590168 ) ) ;
#17611 = CARTESIAN_POINT ( 'NONE',  ( 24.42260775900000169, 1435.425039144950233, 136.9350572207980008 ) ) ;
#17612 = CARTESIAN_POINT ( 'NONE',  ( -8.592347709929391897, 1396.213111781930138, 202.1620628003519755 ) ) ;
#17613 = EDGE_LOOP ( 'NONE', ( #62249, #89302, #78579, #71892 ) ) ;
#17614 = CARTESIAN_POINT ( 'NONE',  ( 5.151097723079999469, 1490.744826430290004, 188.9005472705989916 ) ) ;
#17615 = CARTESIAN_POINT ( 'NONE',  ( 5.001772368710000194, 1443.913060387330006, 150.4106346902979965 ) ) ;
#17616 = ORIENTED_EDGE ( 'NONE', *, *, #51379, .F. ) ;
#17617 = EDGE_LOOP ( 'NONE', ( #4364, #82032, #102768, #3410 ) ) ;
#17618 = CARTESIAN_POINT ( 'NONE',  ( 1.870139295948670011, 1435.444322134060030, 227.4790408562990081 ) ) ;
#17619 = CARTESIAN_POINT ( 'NONE',  ( 7.245172990059893792, 1516.542928138167781, 207.1721856874727905 ) ) ;
#17621 = CARTESIAN_POINT ( 'NONE',  ( -0.2993477608136759782, 1457.076524069930201, 219.7486934169020003 ) ) ;
#17620 = CARTESIAN_POINT ( 'NONE',  ( 11.01624074439999923, 1426.516487655429955, 91.92649746769789942 ) ) ;
#17622 = CARTESIAN_POINT ( 'NONE',  ( -10.98083652350000072, 1433.016921829010016, 151.7694308519979813 ) ) ;
#17623 = CARTESIAN_POINT ( 'NONE',  ( -2.529134858577002376, 1420.903940735018068, 185.4090734218341936 ) ) ;
#17624 = VECTOR ( 'NONE', #102622, 1000.000000000000114 ) ;
#17625 = CARTESIAN_POINT ( 'NONE',  ( 7.342390941769999735, 1424.750470890219958, 212.5422998803489918 ) ) ;
#17626 = CARTESIAN_POINT ( 'NONE',  ( -9.299436816969999242, 1446.922293007090275, 190.6945112479990030 ) ) ;
#17627 = CARTESIAN_POINT ( 'NONE',  ( 7.976840964510000020, 1508.678916850730047, 182.3492935605979994 ) ) ;
#17628 = CARTESIAN_POINT ( 'NONE',  ( 3.451567150219999824, 1449.151155894430076, 184.0761302567979953 ) ) ;
#17629 = AXIS2_PLACEMENT_3D ( 'NONE', #85383, #8678, #108400 ) ;
#17630 = CARTESIAN_POINT ( 'NONE',  ( 9.943976501859779660, 1365.461622992602088, 210.6218459616987957 ) ) ;
#17632 = VERTEX_POINT ( 'NONE', #95402 ) ;
#17631 = CARTESIAN_POINT ( 'NONE',  ( -4.469061752933077614, 1464.606722936262031, 237.1332386249960678 ) ) ;
#17633 = EDGE_LOOP ( 'NONE', ( #88361, #88623, #64220, #48147, #8202 ) ) ;
#17634 = ADVANCED_FACE ( 'NONE', ( #71902 ), #25518, .T. ) ;
#17635 = CARTESIAN_POINT ( 'NONE',  ( -40.26734664479999282, 1444.073158352789960, 137.1206983653979989 ) ) ;
#17636 = CIRCLE ( 'NONE', #48048, 1.999235054590136507 ) ;
#17637 = CARTESIAN_POINT ( 'NONE',  ( 7.544470622717365238, 1510.539524131637791, 203.3949290437643072 ) ) ;
#17638 = CARTESIAN_POINT ( 'NONE',  ( -1.469869910310000138, 1473.882853011830093, 270.2923612834979963 ) ) ;
#17639 = CARTESIAN_POINT ( 'NONE',  ( 8.547640172370703837, 1500.581726597095212, 201.5589322185294634 ) ) ;
#17640 =( BOUNDED_CURVE ( )  B_SPLINE_CURVE ( 3, ( #82791, #22302, #56505, #12827 ),
 .UNSPECIFIED., .F., .F. ) 
 B_SPLINE_CURVE_WITH_KNOTS ( ( 4, 4 ),
 ( 4.712388980384695003, 6.283185307179586232 ),
 .UNSPECIFIED. ) 
 CURVE ( )  GEOMETRIC_REPRESENTATION_ITEM ( )  RATIONAL_B_SPLINE_CURVE ( ( 1.000000000000000000, 0.8047378541243662697, 0.8047378541243662697, 1.000000000000000000 ) ) 
 REPRESENTATION_ITEM ( '' )  );
#17641 = CARTESIAN_POINT ( 'NONE',  ( -2.048334170740000015, 1486.024116770630144, 181.9733265186980020 ) ) ;
#17642 = CARTESIAN_POINT ( 'NONE',  ( -32.00465973459075286, 1524.843178112495480, 202.1266218387728770 ) ) ;
#17643 = CARTESIAN_POINT ( 'NONE',  ( -0.6340257723134260504, 1475.639747297089798, 197.6856915023410011 ) ) ;
#17644 = EDGE_CURVE ( 'NONE', #5861, #20921, #30389, .T. ) ;
#17645 = CARTESIAN_POINT ( 'NONE',  ( 12.27023112330000032, 1416.839692136459917, 223.5796784318309847 ) ) ;
#17646 = PLANE ( 'NONE',  #2025 ) ;
#17647 = CARTESIAN_POINT ( 'NONE',  ( -22.59376922909999763, 1497.713060387329961, 208.1432028049030123 ) ) ;
#17648 = CARTESIAN_POINT ( 'NONE',  ( 8.731474709677369717, 1369.377627139728020, 208.3718459617010978 ) ) ;
#17649 = CARTESIAN_POINT ( 'NONE',  ( 9.029008260723980328, 1407.892909937350169, 198.8844728701529903 ) ) ;
#17650 = CARTESIAN_POINT ( 'NONE',  ( -10.65237148710020065, 1406.670964572119829, 267.4893520522770132 ) ) ;
#17651 = CARTESIAN_POINT ( 'NONE',  ( -14.38141623268059988, 1435.876664363790042, 149.8601871492290059 ) ) ;
#17652 = ORIENTED_EDGE ( 'NONE', *, *, #63323, .T. ) ;
#17653 = CARTESIAN_POINT ( 'NONE',  ( -11.76966145709999978, 1432.350018154589861, 150.8118972717979887 ) ) ;
#17654 = CARTESIAN_POINT ( 'NONE',  ( 13.85488084099999995, 1444.703314923880043, 189.1754263215979961 ) ) ;
#17655 = ORIENTED_EDGE ( 'NONE', *, *, #31489, .T. ) ;
#17656 = ORIENTED_EDGE ( 'NONE', *, *, #44754, .F. ) ;
#17657 = CARTESIAN_POINT ( 'NONE',  ( 4.966635725421030934, 1423.255510328363698, 184.3056371891483138 ) ) ;
#17658 = DIRECTION ( 'NONE',  ( 0.9999994573234139983, 0.000000000000000000, -0.001041802705659123675 ) ) ;
#17659 = CIRCLE ( 'NONE', #80288, 1.999999999999967581 ) ;
#17660 = CARTESIAN_POINT ( 'NONE',  ( 4.039897278065000208, 1516.787536375099990, 214.1203611275269907 ) ) ;
#17661 = CARTESIAN_POINT ( 'NONE',  ( -12.53056552249999989, 1470.463356747030048, 186.5986695887980034 ) ) ;
#17662 = ORIENTED_EDGE ( 'NONE', *, *, #63095, .F. ) ;
#17663 = DIRECTION ( 'NONE',  ( -0.8672669759446636206, 0.000000000000000000, 0.4978433412588729734 ) ) ;
#17664 = CARTESIAN_POINT ( 'NONE',  ( 9.257694918409999474, 1414.913060387329779, 222.9570521072979830 ) ) ;
#17665 = CARTESIAN_POINT ( 'NONE',  ( -1.132949114555000136, 1516.693851263360102, 204.1241276937270186 ) ) ;
#17666 = B_SPLINE_CURVE_WITH_KNOTS ( 'NONE', 5,
 ( #77398, #700, #35387, #93614, #52755, #77940, #94737, #8515, #103121 ),
 .UNSPECIFIED., .F., .F.,
 ( 6, 3, 6 ),
 ( 0.000000000000000000, 0.4999964934256276861, 1.000000000000000000 ),
 .UNSPECIFIED. ) ;
#17667 = CARTESIAN_POINT ( 'NONE',  ( -29.63837353179999923, 1509.975889270829839, 207.4461348473880093 ) ) ;
#17668 = CARTESIAN_POINT ( 'NONE',  ( -4.649632279085039954, 1420.176633138330089, 186.4708453798239987 ) ) ;
#17669 = CARTESIAN_POINT ( 'NONE',  ( -31.92467753469999892, 1384.972130813700005, 206.3032401593790155 ) ) ;
#17670 = CARTESIAN_POINT ( 'NONE',  ( -37.44610523480289999, 1384.575341795339909, 210.6318899809130016 ) ) ;
#17671 = CARTESIAN_POINT ( 'NONE',  ( 2.789446250490000126E-08, 1406.911841291630253, 196.1218459601980157 ) ) ;
#17672 = CARTESIAN_POINT ( 'NONE',  ( 32.28466283162156714, 1512.187213306747481, 219.1752493337713190 ) ) ;
#17674 = EDGE_LOOP ( 'NONE', ( #87517, #86696, #16813, #46362 ) ) ;
#17673 = CARTESIAN_POINT ( 'NONE',  ( -4.058567207959999479, 1447.362832675280060, 184.9425281217980057 ) ) ;
#17675 = CARTESIAN_POINT ( 'NONE',  ( 4.253777714910000007, 1442.471859903390168, 216.9083338397390150 ) ) ;
#17676 = CARTESIAN_POINT ( 'NONE',  ( 26.42702185389999769, 1508.126183422229815, 216.5535634561180132 ) ) ;
#17677 = CARTESIAN_POINT ( 'NONE',  ( 20.23159575734240079, 1487.448372438290107, 225.6309448190939975 ) ) ;
#17678 = CARTESIAN_POINT ( 'NONE',  ( -25.92882744109999749, 1435.924328612949921, 136.6037266722979950 ) ) ;
#17679 = CARTESIAN_POINT ( 'NONE',  ( 1.716392741775000008, 1516.788317650260069, 211.9856338259669997 ) ) ;
#17680 = CARTESIAN_POINT ( 'NONE',  ( -68.57300709150000273, 1379.748249346600005, 279.7358748726589965 ) ) ;
#17681 = CARTESIAN_POINT ( 'NONE',  ( -3.267039729984999585, 1517.012231669750008, 208.3862772893259887 ) ) ;
#17682 = ORIENTED_EDGE ( 'NONE', *, *, #110148, .F. ) ;
#17683 = CARTESIAN_POINT ( 'NONE',  ( 2.500000000000000000, 1438.463317487690119, 157.6994634259980046 ) ) ;
#17684 = LINE ( 'NONE', #86579, #19831 ) ;
#17685 = CARTESIAN_POINT ( 'NONE',  ( -67.03907699609999327, 1384.912355060409936, 292.1878509945590281 ) ) ;
#17686 = VERTEX_POINT ( 'NONE', #73522 ) ;
#17687 = CARTESIAN_POINT ( 'NONE',  ( -10.02788795287149881, 1385.311267560810165, 218.7355560477120093 ) ) ;
#17688 =( GEOMETRIC_REPRESENTATION_CONTEXT ( 3 ) GLOBAL_UNCERTAINTY_ASSIGNED_CONTEXT ( ( #34543 ) ) GLOBAL_UNIT_ASSIGNED_CONTEXT ( ( #96849, #61062, #35829 ) ) REPRESENTATION_CONTEXT ( 'NONE', 'WORKASPACE' ) );
#17689 = CARTESIAN_POINT ( 'NONE',  ( -3.512136796220000523, 1429.445925473590023, 201.4575808623890225 ) ) ;
#17690 = CARTESIAN_POINT ( 'NONE',  ( 12.22638525410440025, 1434.267039502970192, 150.2713860696590018 ) ) ;
#17691 = B_SPLINE_SURFACE_WITH_KNOTS ( 'NONE', 5, 5, ( 
 ( #45067, #27688, #53461, #54030, #87606, #10893, #4152, #78643, #79210 ),
 ( #29330, #62994, #28237, #55667, #89243, #62425, #45622, #12539, #1958 ),
 ( #46172, #88158, #79761, #3068, #46718, #80849, #38279, #97102, #20368 ),
 ( #72462, #98186, #21457, #39942, #41035, #6338, #13608, #38826, #47796 ),
 ( #108798, #30983, #64619, #23679, #32091, #22000, #65158, #73005, #15267 ),
 ( #14174, #49459, #48359, #66820, #89790, #57863, #81932, #56194, #90329 ) ),
 .UNSPECIFIED., .F., .F., .F.,
 ( 6, 6 ),
 ( 6, 3, 6 ),
 ( 9.945329370599239382, 12.20377897060000016 ),
 ( 0.000000000000000000, 1.000000000000000000, 2.000000000000000000 ),
 .UNSPECIFIED. ) ;
#17692 = CARTESIAN_POINT ( 'NONE',  ( 18.08821306226149872, 1459.310247305569874, 227.9716307757270215 ) ) ;
#17693 = CARTESIAN_POINT ( 'NONE',  ( -24.27332534947139919, 1509.087562220649943, 222.4402390272340142 ) ) ;
#17694 = CARTESIAN_POINT ( 'NONE',  ( -2.923521586279999696, 1410.394928897130058, 186.6127580804979971 ) ) ;
#17695 = CARTESIAN_POINT ( 'NONE',  ( 5.009886284249999377, 1430.069699660889910, 217.1776678749689893 ) ) ;
#17696 = CARTESIAN_POINT ( 'NONE',  ( 4.236872543330679974, 1441.473390915530217, 163.4512186758819894 ) ) ;
#17697 = B_SPLINE_CURVE_WITH_KNOTS ( 'NONE', 5,
 ( #105876, #31348, #50384, #59885, #23497, #84512 ),
 .UNSPECIFIED., .F., .F.,
 ( 6, 6 ),
 ( 0.000000000000000000, 0.03026097244042860734 ),
 .UNSPECIFIED. ) ;
#17699 = CARTESIAN_POINT ( 'NONE',  ( -3.969564362200000307, 1421.142701091429899, 186.0775239138980055 ) ) ;
#17698 = CARTESIAN_POINT ( 'NONE',  ( 2.877744946244999991, 1516.723920667490120, 213.7309102736070088 ) ) ;
#17700 = CARTESIAN_POINT ( 'NONE',  ( 20.18532048049999972, 1508.602711282329892, 189.1193814760979990 ) ) ;
#17701 = CARTESIAN_POINT ( 'NONE',  ( 2.485217193935000068, 1516.534320418310244, 216.8308781079170160 ) ) ;
#17702 = ORIENTED_EDGE ( 'NONE', *, *, #49035, .T. ) ;
#17703 = CARTESIAN_POINT ( 'NONE',  ( -12.61566556969999908, 1416.819759739430083, 194.9201884166980108 ) ) ;
#17704 = B_SPLINE_SURFACE_WITH_KNOTS ( 'NONE', 5, 5, ( 
 ( #70246, #86994, #62957, #70796, #62383, #97068 ),
 ( #27104, #1922, #52867, #104909, #19789, #11413 ),
 ( #71905, #78604, #79723, #53990, #97612, #28197 ),
 ( #96509, #54538, #95954, #88672, #88124, #63492 ),
 ( #19214, #20882, #45581, #53417, #3030, #105463 ),
 ( #11950, #106021, #36059, #46131, #29296, #87568 ) ),
 .UNSPECIFIED., .F., .F., .F.,
 ( 6, 6 ),
 ( 6, 6 ),
 ( 14.17748175450000048, 22.88732747950000146 ),
 ( 0.9649189546150001018, 2.000000000000000000 ),
 .UNSPECIFIED. ) ;
#17705 = CARTESIAN_POINT ( 'NONE',  ( 2.472529913803023227, 1523.678648413191695, 242.8674788698241400 ) ) ;
#17706 = ORIENTED_EDGE ( 'NONE', *, *, #12497, .F. ) ;
#17707 = VECTOR ( 'NONE', #23069, 999.9999999999998863 ) ;
#17708 = CARTESIAN_POINT ( 'NONE',  ( 4.132092042950000099, 1421.241915939129967, 185.3693087620980009 ) ) ;
#17709 = CONICAL_SURFACE ( 'NONE', #94631, 1.000000000000007327, 0.7853981633970000820 ) ;
#17710 = SURFACE_SIDE_STYLE ('',( #69276 ) ) ;
#17711 = CARTESIAN_POINT ( 'NONE',  ( 2.410642264446942296, 1525.163527997520532, 176.1170057922971353 ) ) ;
#17712 = FACE_OUTER_BOUND ( 'NONE', #17904, .T. ) ;
#17713 = CYLINDRICAL_SURFACE ( 'NONE', #69293, 2.000000000000003109 ) ;
#17714 = CARTESIAN_POINT ( 'NONE',  ( -3.609215388063503394, 1508.124843871699341, 220.7461715565221994 ) ) ;
#17715 = CARTESIAN_POINT ( 'NONE',  ( 17.54299231450000107, 1415.063410489729904, 210.2814835228880099 ) ) ;
#17716 = CARTESIAN_POINT ( 'NONE',  ( 19.48178958320507093, 1507.796605003039531, 229.4922759112947972 ) ) ;
#17717 = CARTESIAN_POINT ( 'NONE',  ( -8.881784196999999612E-15, 1443.913060387330006, 126.8032249175980155 ) ) ;
#17718 = CARTESIAN_POINT ( 'NONE',  ( 9265.100134287571564, 5182.654794667087117, -1184.579948005114375 ) ) ;
#17719 = CARTESIAN_POINT ( 'NONE',  ( 38.46602011401969889, 1440.913060379879880, 257.0153466912190083 ) ) ;
#17721 = CARTESIAN_POINT ( 'NONE',  ( 4.329448791022380227, 1515.064792310580060, 207.3461553972610147 ) ) ;
#17720 = CARTESIAN_POINT ( 'NONE',  ( -11.47238377808170107, 1419.373738041100069, 197.8436817076510010 ) ) ;
#17722 = CARTESIAN_POINT ( 'NONE',  ( 7.512705394502938283, 1509.036904577181758, 203.3466803227199193 ) ) ;
#17723 = EDGE_LOOP ( 'NONE', ( #22195, #15193, #47535, #62741 ) ) ;
#17724 = CARTESIAN_POINT ( 'NONE',  ( 14.24685689828609902, 1473.184890486440054, 194.3436051322440221 ) ) ;
#17725 = CARTESIAN_POINT ( 'NONE',  ( 25.36184121639999844, 1469.165572951930244, 206.9791411554380147 ) ) ;
#17726 = CARTESIAN_POINT ( 'NONE',  ( -24.41225618889999893, 1441.001746037479961, 212.0330686186080129 ) ) ;
#17727 = CARTESIAN_POINT ( 'NONE',  ( 4.547831559409852176, 1410.447768422028275, 186.2153058587292094 ) ) ;
#17728 = CARTESIAN_POINT ( 'NONE',  ( -10.49919538747700010, 1479.838970662580095, 209.4913417018410087 ) ) ;
#17729 = B_SPLINE_SURFACE_WITH_KNOTS ( 'NONE', 5, 5, ( 
 ( #80071, #20153, #36412, #12305, #28013, #80629 ),
 ( #96328, #96884, #3392, #19606, #53808, #10678 ),
 ( #11235, #2839, #88481, #45935, #38610, #45397 ),
 ( #71155, #37521, #29120, #106916, #63305, #30205 ),
 ( #97425, #3944, #38071, #106375, #29663, #64396 ),
 ( #63848, #97960, #21230, #55440, #89569, #98517 ),
 ( #12859, #72789, #81165, #4480, #21785, #87383 ),
 ( #44845, #78998, #40268, #48695, #83925, #67151 ),
 ( #100713, #39158, #49244, #41386, #48138, #56537 ) ),
 .UNSPECIFIED., .F., .F., .F.,
 ( 6, 3, 6 ),
 ( 6, 6 ),
 ( 3.197141790549999918, 7.200146509529999683, 12.49638257910000050 ),
 ( 0.000000000000000000, 2.000000000000000000 ),
 .UNSPECIFIED. ) ;
#17730 = CARTESIAN_POINT ( 'NONE',  ( -11.82552473729999853, 1507.579552363830089, 183.2239286378979841 ) ) ;
#17731 = CARTESIAN_POINT ( 'NONE',  ( -22.81224805166159797, 1509.788088251490080, 188.7721076916159859 ) ) ;
#17732 = CARTESIAN_POINT ( 'NONE',  ( -4.633397098031169392, 1377.913060387289988, 204.2654103466966831 ) ) ;
#17733 = CARTESIAN_POINT ( 'NONE',  ( 13.10647016826960076, 1414.913527292460003, 198.0560097828689834 ) ) ;
#17734 = CARTESIAN_POINT ( 'NONE',  ( -68.62142813640339511, 1383.786590555389921, 293.1919703512040201 ) ) ;
#17735 = CARTESIAN_POINT ( 'NONE',  ( -107.7365696369350019, 1379.032352522303881, 299.3254846779751119 ) ) ;
#17736 = CARTESIAN_POINT ( 'NONE',  ( -26.87217695997193800, 1508.240762366635636, 212.0141957947051026 ) ) ;
#17737 = CARTESIAN_POINT ( 'NONE',  ( -1.660008066423290130, 1516.550879573519751, 201.4123801776780169 ) ) ;
#17739 = ORIENTED_EDGE ( 'NONE', *, *, #106847, .F. ) ;
#17738 = CARTESIAN_POINT ( 'NONE',  ( 0.000000000000000000, 1450.913060387330006, 187.0476703040980055 ) ) ;
#17740 = CARTESIAN_POINT ( 'NONE',  ( -18.09679206583593469, 1459.548717300706812, 227.9697539532586461 ) ) ;
#17741 = AXIS2_PLACEMENT_3D ( 'NONE', #81668, #40235, #107985 ) ;
#17742 = CARTESIAN_POINT ( 'NONE',  ( -74.89462252569998668, 1381.007359432420117, 297.5740919175589738 ) ) ;
#17743 = CARTESIAN_POINT ( 'NONE',  ( -0.5172272512948579148, 1416.765894075033202, 233.9543648737588626 ) ) ;
#17744 = EDGE_LOOP ( 'NONE', ( #6242, #12513, #77862, #2726, #40777, #12296, #51252, #49927, #75500, #10643, #99614, #33415 ) ) ;
#17745 = EDGE_LOOP ( 'NONE', ( #43209, #48383 ) ) ;
#17746 = CARTESIAN_POINT ( 'NONE',  ( 19.43393205732160212, 1509.529646666910139, 230.8600434984439858 ) ) ;
#17747 = CARTESIAN_POINT ( 'NONE',  ( 20.20959865099491992, 1511.187213306747708, 236.2316688286738611 ) ) ;
#17748 = CARTESIAN_POINT ( 'NONE',  ( 40.22348776513499757, 1442.812490084199908, 137.0237541975089925 ) ) ;
#17750 = CARTESIAN_POINT ( 'NONE',  ( -20.04379992670000377, 1471.636457544530003, 264.7217083835980134 ) ) ;
#17749 = CARTESIAN_POINT ( 'NONE',  ( 9.580271555476294054, 1411.182622053547220, 269.3463862739754404 ) ) ;
#17751 = CARTESIAN_POINT ( 'NONE',  ( 8.638387969371279951, 1437.275665663040172, 209.5904139818730130 ) ) ;
#17752 = CARTESIAN_POINT ( 'NONE',  ( -110.0797703000000070, 1384.336996500939904, 296.9599543076590180 ) ) ;
#17753 = CARTESIAN_POINT ( 'NONE',  ( -11.72537676174745513, 1435.130261367574121, 151.3178099432534225 ) ) ;
#17754 = CARTESIAN_POINT ( 'NONE',  ( -19.85061890739999768, 1484.702845893429867, 190.8243287402979718 ) ) ;
#17755 = CARTESIAN_POINT ( 'NONE',  ( 1.129978713339999885, 1408.952520113529999, 186.6978219804979915 ) ) ;
#17756 = CARTESIAN_POINT ( 'NONE',  ( 0.4136971850115839788, 1486.226569062650242, 197.2199659705369754 ) ) ;
#17757 = CARTESIAN_POINT ( 'NONE',  ( -11.70596046909999899, 1435.783534794500156, 151.4055864423979756 ) ) ;
#17758 = CARTESIAN_POINT ( 'NONE',  ( 11.53918857109999863, 1434.258397247200037, 151.3471602487979908 ) ) ;
#17759 = CARTESIAN_POINT ( 'NONE',  ( -10.08143941300950175, 1423.969704056519731, 204.5062346435900054 ) ) ;
#17760 = CARTESIAN_POINT ( 'NONE',  ( -23.02752199190000226, 1452.108921600530039, 139.9703293178979777 ) ) ;
#17761 = CARTESIAN_POINT ( 'NONE',  ( 1.283858640530000095, 1464.947442259230002, 237.5396736328980296 ) ) ;
#17762 = VERTEX_POINT ( 'NONE', #107655 ) ;
#17763 = CARTESIAN_POINT ( 'NONE',  ( -3.116127822624859878, 1509.034536885679927, 213.6092057278939933 ) ) ;
#17764 = CARTESIAN_POINT ( 'NONE',  ( -4.389948488746259869, 1481.757683799150072, 231.0981567811180071 ) ) ;
#17765 = CARTESIAN_POINT ( 'NONE',  ( -44.93136296710000011, 1440.913060597359845, 269.6838063816980480 ) ) ;
#17766 = CARTESIAN_POINT ( 'NONE',  ( -4.311053961940764623, 1407.085547473677934, 196.6635586998287977 ) ) ;
#17767 = CARTESIAN_POINT ( 'NONE',  ( 17.59268578599999699, 1410.455475235630047, 224.1775087684979724 ) ) ;
#17768 = CARTESIAN_POINT ( 'NONE',  ( -8.773919776719999675, 1470.032071067190145, 190.9916890139989789 ) ) ;
#17769 = VECTOR ( 'NONE', #16649, 1000.000000000000114 ) ;
#17770 = CARTESIAN_POINT ( 'NONE',  ( 2.330134126739547451, 1515.219201591195088, 213.4472514034076767 ) ) ;
#17771 = CARTESIAN_POINT ( 'NONE',  ( 2.927313424399410113, 1410.174542261320084, 231.6044306003970235 ) ) ;
#17773 = EDGE_CURVE ( 'NONE', #64279, #54634, #88930, .T. ) ;
#17772 = CARTESIAN_POINT ( 'NONE',  ( -0.9667867126420001123, 1415.996778984329922, 227.8322076899980004 ) ) ;
#17774 = CARTESIAN_POINT ( 'NONE',  ( -8.587497642409999798, 1419.088922007130122, 232.7581010276980180 ) ) ;
#17775 = CARTESIAN_POINT ( 'NONE',  ( -107.8448688559999908, 1387.924802880550033, 310.1598078892590138 ) ) ;
#17776 =( BOUNDED_CURVE ( )  B_SPLINE_CURVE ( 3, ( #32605, #26389, #67328, #86307 ),
 .UNSPECIFIED., .F., .F. ) 
 B_SPLINE_CURVE_WITH_KNOTS ( ( 4, 4 ),
 ( 1.144704971675025273, 1.570796326799507314 ),
 .UNSPECIFIED. ) 
 CURVE ( )  GEOMETRIC_REPRESENTATION_ITEM ( )  RATIONAL_B_SPLINE_CURVE ( ( 1.000000000000000000, 0.9849276519253457041, 0.9849276519253457041, 1.000000000000000000 ) ) 
 REPRESENTATION_ITEM ( '' )  );
#17777 = CARTESIAN_POINT ( 'NONE',  ( -8.210436200376010518, 1511.433570353809955, 214.6767451177750274 ) ) ;
#17778 = B_SPLINE_CURVE_WITH_KNOTS ( 'NONE', 5,
 ( #95100, #17803, #60975, #35188, #9988, #18366 ),
 .UNSPECIFIED., .F., .F.,
 ( 6, 6 ),
 ( -167.7881597310000075, -30.40382300159998863 ),
 .UNSPECIFIED. ) ;
#17779 = CARTESIAN_POINT ( 'NONE',  ( -2.595397113752544449, 1358.510305191965017, 209.6218459617033432 ) ) ;
#17780 = CARTESIAN_POINT ( 'NONE',  ( -46.00060696795689807, 1439.228690553249862, 266.6786537750060120 ) ) ;
#17781 = CARTESIAN_POINT ( 'NONE',  ( -2.499999999940000439, 1436.903610872740273, 184.2102826205979795 ) ) ;
#17782 = CIRCLE ( 'NONE', #55398, 1.000000000000000888 ) ;
#17783 = CARTESIAN_POINT ( 'NONE',  ( -8.474551757659998685, 1423.809698281529791, 209.1924171156409784 ) ) ;
#17784 = VERTEX_POINT ( 'NONE', #56708 ) ;
#17785 = CARTESIAN_POINT ( 'NONE',  ( -4.612671377915000370, 1516.783665406140017, 209.8782801844560026 ) ) ;
#17786 = CARTESIAN_POINT ( 'NONE',  ( -5.411782914500000707, 1435.306182108309940, 154.6725736572979883 ) ) ;
#17787 = CARTESIAN_POINT ( 'NONE',  ( 19.27955013568295328, 1456.451286679076929, 224.7795789275638185 ) ) ;
#17788 = CARTESIAN_POINT ( 'NONE',  ( 7.494055247967449596, 1426.002717090129863, 212.3343695544420200 ) ) ;
#17789 = AXIS2_PLACEMENT_3D ( 'NONE', #16618, #68199, #50284 ) ;
#17790 = CARTESIAN_POINT ( 'NONE',  ( -26.88878276533139910, 1451.048910818290096, 136.3593413721419836 ) ) ;
#17791 = ORIENTED_EDGE ( 'NONE', *, *, #85108, .T. ) ;
#17792 = CARTESIAN_POINT ( 'NONE',  ( -16.68455607539956986, 1409.595982907923371, 225.3198891662985375 ) ) ;
#17794 = CARTESIAN_POINT ( 'NONE',  ( 15.10313800449999988, 1488.809466529130077, 194.0858732079979916 ) ) ;
#17793 = CARTESIAN_POINT ( 'NONE',  ( -2.708826876440360909, 1524.477587234266366, 176.2952420485788423 ) ) ;
#17795 = CARTESIAN_POINT ( 'NONE',  ( 11.60004869885203682, 1423.462004151896508, 135.7646869108323244 ) ) ;
#17796 = CARTESIAN_POINT ( 'NONE',  ( -12.23669307423070052, 1377.661331666050273, 207.7794331870949804 ) ) ;
#17797 = CARTESIAN_POINT ( 'NONE',  ( -1.571492423569999852, 1455.857433419590052, 215.6548381990889709 ) ) ;
#17798 = CARTESIAN_POINT ( 'NONE',  ( 4.865303301610000908, 1425.588844564269948, 210.1313439721089935 ) ) ;
#17799 = ORIENTED_EDGE ( 'NONE', *, *, #36340, .F. ) ;
#17800 = CARTESIAN_POINT ( 'NONE',  ( -1.200210185686839903, 1410.247648972750085, 269.6150193402980335 ) ) ;
#17801 = CARTESIAN_POINT ( 'NONE',  ( 4.997718238375000510, 1516.693851263360102, 207.9888968556769839 ) ) ;
#17802 = CARTESIAN_POINT ( 'NONE',  ( 10.94784056215000057, 1419.904943497329896, 232.1968281718800142 ) ) ;
#17803 = CARTESIAN_POINT ( 'NONE',  ( -19.99769045190000227, 1488.355546399329796, 191.5584535652979810 ) ) ;
#17805 = ORIENTED_EDGE ( 'NONE', *, *, #80504, .F. ) ;
#17804 = CARTESIAN_POINT ( 'NONE',  ( -2.500000000000000000, 1439.435444884669778, 162.3942738332719955 ) ) ;
#17806 = VERTEX_POINT ( 'NONE', #90843 ) ;
#17807 = CARTESIAN_POINT ( 'NONE',  ( -23.32570769421149848, 1410.008417559419968, 209.9356539553859875 ) ) ;
#17808 = EDGE_CURVE ( 'NONE', #29004, #105413, #107172, .T. ) ;
#17809 = CARTESIAN_POINT ( 'NONE',  ( -0.2759417911574060245, 1410.303294818389986, 185.0234033110549774 ) ) ;
#17810 = CARTESIAN_POINT ( 'NONE',  ( -105.2220349633299890, 1311.832804576489934, 308.6894886186490226 ) ) ;
#17811 = CIRCLE ( 'NONE', #14240, 1.000000000000000000 ) ;
#17812 = DIRECTION ( 'NONE',  ( 0.03489949670250328678, 0.9993908270190956511, 0.000000000000000000 ) ) ;
#17813 = CARTESIAN_POINT ( 'NONE',  ( -18.85961944716780181, 1416.512142023939987, 207.5743260399690087 ) ) ;
#17814 = CARTESIAN_POINT ( 'NONE',  ( -22.08220418359999826, 1420.825048654430020, 216.4967283580180037 ) ) ;
#17815 = CARTESIAN_POINT ( 'NONE',  ( 29.68528746673739960, 1466.931583989530054, 269.3634784496489942 ) ) ;
#17816 = CARTESIAN_POINT ( 'NONE',  ( -11.63765358216780221, 1391.913060387119913, 208.5693770010209960 ) ) ;
#17817 = CARTESIAN_POINT ( 'NONE',  ( -16.87601176900255595, 1421.848452965002934, 226.8668675059429631 ) ) ;
#17818 = CARTESIAN_POINT ( 'NONE',  ( 3.252530615595000452, 1516.827328999679821, 206.2418890071470230 ) ) ;
#17819 = VERTEX_POINT ( 'NONE', #74067 ) ;
#17820 = CARTESIAN_POINT ( 'NONE',  ( 18.94390663599199343, 1457.575929578803880, 226.8085174276290275 ) ) ;
#17821 = CARTESIAN_POINT ( 'NONE',  ( 1.495889316277259962, 1468.096849455099800, 182.8155357973550110 ) ) ;
#17822 = CARTESIAN_POINT ( 'NONE',  ( 22.85539255169999606, 1409.737614192629962, 208.6607040618730196 ) ) ;
#17823 = ORIENTED_EDGE ( 'NONE', *, *, #59405, .F. ) ;
#17824 = CARTESIAN_POINT ( 'NONE',  ( 4.730384163222276506, 1508.603735221688339, 212.6094383991669758 ) ) ;
#17825 = CARTESIAN_POINT ( 'NONE',  ( 26.47933087948679898, 1450.735437991490016, 136.5163285050169861 ) ) ;
#17826 = CARTESIAN_POINT ( 'NONE',  ( -4.963083875006099710, 1508.551704408389924, 211.9655763852440202 ) ) ;
#17827 = CARTESIAN_POINT ( 'NONE',  ( -8.744990863649999113, 1385.315572773260101, 218.5566709142290165 ) ) ;
#17828 = CARTESIAN_POINT ( 'NONE',  ( 7.435908444379999871, 1422.989459805909974, 195.6132688577989711 ) ) ;
#17830 = B_SPLINE_SURFACE_WITH_KNOTS ( 'NONE', 5, 5, ( 
 ( #8094, #34411, #60748, #109474, #41707, #94871 ),
 ( #83705, #24342, #68583, #66934, #34956, #6999 ),
 ( #42262, #7553, #41158, #15927, #102688, #76410 ),
 ( #50128, #25983, #84257, #75867, #110017, #69140 ),
 ( #43378, #33293, #67486, #101589, #17577, #85916 ),
 ( #110564, #68041, #17015, #8641, #42817, #9220 ),
 ( #77527, #20355, #54015, #62407, #88145, #106041 ),
 ( #70266, #86464, #29318, #37179, #19809, #103825 ),
 ( #3053, #1943, #95429, #36623, #54560, #11433 ) ),
 .UNSPECIFIED., .F., .F., .F.,
 ( 6, 3, 6 ),
 ( 6, 6 ),
 ( 3.058261753925569870, 5.256832519259999614, 7.455370546767019491 ),
 ( -0.0004137009344281229587, 2.000000000000000000 ),
 .UNSPECIFIED. ) ;
#17829 = CARTESIAN_POINT ( 'NONE',  ( 17.60733967200000194, 1409.692916845429863, 193.8802571657980138 ) ) ;
#17831 = B_SPLINE_CURVE_WITH_KNOTS ( 'NONE', 3,
 ( #10632, #97380, #71118, #87336, #72214, #5533, #57618, #82234, #107428, #30724, #6079, #38034, #23424 ),
 .UNSPECIFIED., .F., .F.,
 ( 4, 2, 1, 1, 1, 2, 2, 4 ),
 ( 0.000000000000000000, 0.2500000000001524336, 0.3750000000002216560, 0.4375000000002614020, 0.4687500000002742806, 0.4843750000002768341, 0.5000000000002794431, 1.000000000000000000 ),
 .UNSPECIFIED. ) ;
#17832 = CARTESIAN_POINT ( 'NONE',  ( 27.23063139319997816, 1444.324653571829003, 161.8596747266978753 ) ) ;
#17833 = CARTESIAN_POINT ( 'NONE',  ( 2.554988275568651712, 1439.637233825041221, 183.2488012791049812 ) ) ;
#17835 = CARTESIAN_POINT ( 'NONE',  ( -22.38744152929581333, 1431.163389416910832, 216.9216883821636941 ) ) ;
#17834 = CARTESIAN_POINT ( 'NONE',  ( 1.950421698860000053, 1417.553803591129963, 234.0318042942980128 ) ) ;
#17836 = CARTESIAN_POINT ( 'NONE',  ( -16.66231036550740541, 1523.604703353109699, 180.4882076302515372 ) ) ;
#17837 = CARTESIAN_POINT ( 'NONE',  ( -15.87405076837314333, 1420.081557989787143, 210.7260919225635405 ) ) ;
#17838 = CARTESIAN_POINT ( 'NONE',  ( -9.292238542100001553, 1381.405190552079830, 217.5286081215490128 ) ) ;
#17839 = CARTESIAN_POINT ( 'NONE',  ( 16.90742456150000095, 1444.994950788469851, 162.4348202098979925 ) ) ;
#17840 = EDGE_LOOP ( 'NONE', ( #31950, #102446, #19374, #60827 ) ) ;
#17841 = CARTESIAN_POINT ( 'NONE',  ( 11.84669589606929918, 1415.088506334920112, 221.4079050929989876 ) ) ;
#17842 = CARTESIAN_POINT ( 'NONE',  ( 4.926620861452232880, 1485.064373513001783, 218.6596911836547861 ) ) ;
#17843 = CARTESIAN_POINT ( 'NONE',  ( -0.3445723587089969953, 1409.016293610590083, 232.2535758655419897 ) ) ;
#17844 = EDGE_CURVE ( 'NONE', #29094, #71004, #31485, .T. ) ;
#17845 = CARTESIAN_POINT ( 'NONE',  ( -13.27879787639999876, 1390.397743956920067, 206.9666494769190024 ) ) ;
#17846 = EDGE_CURVE ( 'NONE', #22768, #103324, #12374, .T. ) ;
#17847 = CARTESIAN_POINT ( 'NONE',  ( -0.4768852844176069694, 1420.937210074157747, 193.7246766131215452 ) ) ;
#17848 = ADVANCED_FACE ( 'NONE', ( #15221 ), #24173, .T. ) ;
#17849 = DIRECTION ( 'NONE',  ( -0.6736849260863839728, 0.000000000000000000, 0.7390186874254150995 ) ) ;
#17850 = CARTESIAN_POINT ( 'NONE',  ( -26.42714720800000094, 1440.913060387330006, 243.9198229517980110 ) ) ;
#17851 = CIRCLE ( 'NONE', #103729, 17.26401014167801762 ) ;
#17852 = CARTESIAN_POINT ( 'NONE',  ( -21.95218091425238782, 1509.537469399167094, 191.3967133988915919 ) ) ;
#17853 = EDGE_CURVE ( 'NONE', #31153, #83342, #35221, .T. ) ;
#17854 = CARTESIAN_POINT ( 'NONE',  ( 11.88531770350000016, 1433.194006408179803, 149.9681147489979764 ) ) ;
#17855 = CARTESIAN_POINT ( 'NONE',  ( 9.019386504720001696, 1461.887471368730075, 248.0989693021979861 ) ) ;
#17856 = B_SPLINE_SURFACE_WITH_KNOTS ( 'NONE', 5, 5, ( 
 ( #23445, #24535, #16134, #50341, #84466, #1041 ),
 ( #36827, #17781, #36270, #18345, #9417, #104581 ),
 ( #52536, #104022, #18897, #70460, #35163, #53656 ),
 ( #26198, #27876, #94507, #53092, #68799, #43579 ),
 ( #62057, #78270, #102900, #9965, #60386, #71017 ),
 ( #95079, #87801, #77728, #34613, #61498, #87231 ) ),
 .UNSPECIFIED., .F., .F., .F.,
 ( 6, 6 ),
 ( 6, 6 ),
 ( 86.05908199089999755, 105.4335682549999973 ),
 ( 0.000000000000000000, 2.000000000000000000 ),
 .UNSPECIFIED. ) ;
#17858 = EDGE_CURVE ( 'NONE', #100027, #65578, #32417, .T. ) ;
#17857 = CARTESIAN_POINT ( 'NONE',  ( 11.22084002889469900, 1414.913060387399810, 197.6243765041139966 ) ) ;
#17859 = CARTESIAN_POINT ( 'NONE',  ( 20.15123768920399883, 1431.269255322170011, 215.0996795108299864 ) ) ;
#17860 = CIRCLE ( 'NONE', #64433, 1.000000000000000000 ) ;
#17861 = CARTESIAN_POINT ( 'NONE',  ( 10.48742109869949957, 1419.983217468429984, 196.1364727454310071 ) ) ;
#17862 = CARTESIAN_POINT ( 'NONE',  ( -2.596261494520225366, 1525.907212628473644, 177.4701144822246874 ) ) ;
#17863 = EDGE_CURVE ( 'NONE', #53899, #20182, #65740, .T. ) ;
#17864 = CARTESIAN_POINT ( 'NONE',  ( 22.57319362359999815, 1409.701316935530031, 208.7927549349429910 ) ) ;
#17865 = CARTESIAN_POINT ( 'NONE',  ( 10.12919404300857451, 1398.213353175035536, 200.9395953525430230 ) ) ;
#17866 = CARTESIAN_POINT ( 'NONE',  ( -27.81315569556840117, 1509.884315111430169, 222.3141242500419992 ) ) ;
#17867 = CIRCLE ( 'NONE', #1868, 1.999999999999999556 ) ;
#17868 = CARTESIAN_POINT ( 'NONE',  ( -7.982037141949999359, 1424.874072662569915, 210.5243721551090061 ) ) ;
#17869 = CARTESIAN_POINT ( 'NONE',  ( -3.269259737218870310, 1476.740802116999930, 199.2818558394819775 ) ) ;
#17870 = CARTESIAN_POINT ( 'NONE',  ( -8.482731032629999390, 1508.704755829329770, 235.6989776125980143 ) ) ;
#17871 = CARTESIAN_POINT ( 'NONE',  ( -9.506144258141100423, 1383.863471983120007, 218.5502817718870006 ) ) ;
#17872 = CARTESIAN_POINT ( 'NONE',  ( -5.586163095751780716, 1491.245996555280044, 185.8699225654929990 ) ) ;
#17873 = CARTESIAN_POINT ( 'NONE',  ( -6.935457963315000640, 1516.627618683580067, 212.5772239474869991 ) ) ;
#17874 = EDGE_CURVE ( 'NONE', #323, #3290, #97845, .T. ) ;
#17875 = CARTESIAN_POINT ( 'NONE',  ( -20.80698145192160098, 1418.268157419850013, 208.6562635851959726 ) ) ;
#17876 = CARTESIAN_POINT ( 'NONE',  ( 0.1601303935690119862, 1486.188272806359919, 181.8285171723719884 ) ) ;
#17878 = ORIENTED_EDGE ( 'NONE', *, *, #94503, .T. ) ;
#17877 = CARTESIAN_POINT ( 'NONE',  ( 3.919202604670000145, 1440.900018029090006, 218.2279973031590146 ) ) ;
#17879 = FACE_OUTER_BOUND ( 'NONE', #82163, .T. ) ;
#17880 = DIRECTION ( 'NONE',  ( 0.4794255386042031719, 0.000000000000000000, 0.8775825618903726477 ) ) ;
#17881 = CARTESIAN_POINT ( 'NONE',  ( 12.91284616039999911, 1434.774386575559902, 149.6994772678979757 ) ) ;
#17882 = DIRECTION ( 'NONE',  ( 0.000000000000000000, 1.000000000000000000, 0.000000000000000000 ) ) ;
#17883 = CARTESIAN_POINT ( 'NONE',  ( 5.140114172436319961, 1436.845577873409866, 228.7442477189930230 ) ) ;
#17884 = ORIENTED_EDGE ( 'NONE', *, *, #6296, .F. ) ;
#17886 = EDGE_CURVE ( 'NONE', #44597, #1439, #99235, .T. ) ;
#17885 = CARTESIAN_POINT ( 'NONE',  ( -38.64637139473789773, 1443.913060387190171, 137.1864063576500143 ) ) ;
#17887 = CARTESIAN_POINT ( 'NONE',  ( -14.28042675339239942, 1390.367274744259930, 209.8448731692960223 ) ) ;
#17888 = CARTESIAN_POINT ( 'NONE',  ( -13.24264662000000037, 1414.971439108430104, 220.7226513867979918 ) ) ;
#17889 = CARTESIAN_POINT ( 'NONE',  ( 11.58492313561834131, 1426.183940868015270, 138.6952717246431064 ) ) ;
#17890 = EDGE_CURVE ( 'NONE', #108700, #95777, #53878, .T. ) ;
#17891 = CARTESIAN_POINT ( 'NONE',  ( -2.906570293435709385, 1368.295572657563525, 210.3150243549862068 ) ) ;
#17892 = CARTESIAN_POINT ( 'NONE',  ( -1.353902514868472462, 1408.960339704959324, 187.6075962084191531 ) ) ;
#17893 = CARTESIAN_POINT ( 'NONE',  ( 2.833799216370230134, 1466.651268623249734, 236.4511971046459848 ) ) ;
#17894 = B_SPLINE_CURVE_WITH_KNOTS ( 'NONE', 3,
 ( #48324, #90849, #99236, #84100 ),
 .UNSPECIFIED., .F., .F.,
 ( 4, 4 ),
 ( 0.000000000000000000, 1.000000000000000000 ),
 .UNSPECIFIED. ) ;
#17895 = FACE_OUTER_BOUND ( 'NONE', #30668, .T. ) ;
#17896 = CARTESIAN_POINT ( 'NONE',  ( -12.09196955530000039, 1391.856377031290094, 209.7328924207210150 ) ) ;
#17897 = CARTESIAN_POINT ( 'NONE',  ( -80.63838622464560046, 1385.160061434930185, 283.9401284501640248 ) ) ;
#17898 = CARTESIAN_POINT ( 'NONE',  ( -16.72903711220000034, 1412.957917587729980, 191.6790723950980180 ) ) ;
#17899 = CARTESIAN_POINT ( 'NONE',  ( -51.76145802239999938, 1379.744278086280019, 243.7243931585590246 ) ) ;
#17900 = ORIENTED_EDGE ( 'NONE', *, *, #93344, .T. ) ;
#17901 = EDGE_CURVE ( 'NONE', #40999, #97580, #65695, .T. ) ;
#17902 = CARTESIAN_POINT ( 'NONE',  ( -15.76858003950689913, 1409.463696000809932, 225.2883378276359849 ) ) ;
#17904 = EDGE_LOOP ( 'NONE', ( #68917, #109040, #30086, #72378 ) ) ;
#17903 = DIRECTION ( 'NONE',  ( -5.980589973904019347E-17, 1.000000000000000000, -1.736889445713099699E-16 ) ) ;
#17905 = CARTESIAN_POINT ( 'NONE',  ( 7.323840960111850151, 1466.289181860749977, 215.8067017296629899 ) ) ;
#17906 = ORIENTED_EDGE ( 'NONE', *, *, #104887, .T. ) ;
#17907 = CARTESIAN_POINT ( 'NONE',  ( 6.020918722830000291, 1451.049614457190046, 209.7855091624759893 ) ) ;
#17908 = CARTESIAN_POINT ( 'NONE',  ( -7.458416007436354356, 1363.271152069968139, 210.6218459617142003 ) ) ;
#17909 = CARTESIAN_POINT ( 'NONE',  ( -6.173337796650000264, 1494.737438040389861, 198.8902207915990061 ) ) ;
#17910 = AXIS2_PLACEMENT_3D ( 'NONE', #85417, #26626, #18764 ) ;
#17911 = CARTESIAN_POINT ( 'NONE',  ( 41.28234918735198278, 1446.727361558453140, 269.6338958528504008 ) ) ;
#17912 = CARTESIAN_POINT ( 'NONE',  ( -22.75273496409615603, 1512.187213306747481, 183.6728937936775310 ) ) ;
#17913 = CARTESIAN_POINT ( 'NONE',  ( 17.73602759646932370, 1434.477616020383493, 215.8487880863369810 ) ) ;
#17914 = CARTESIAN_POINT ( 'NONE',  ( -5.258175134983901877, 1511.418042823260521, 200.5125726690029637 ) ) ;
#17915 = CARTESIAN_POINT ( 'NONE',  ( -6.916946890995543384, 1516.591588929718000, 212.0217231930357968 ) ) ;
#17916 = CARTESIAN_POINT ( 'NONE',  ( -12.01638156518240130, 1440.881463477919851, 187.8051726210379968 ) ) ;
#17917 = CARTESIAN_POINT ( 'NONE',  ( -5.761781897038445344, 1370.707051359383968, 209.6218459617033432 ) ) ;
#17918 = DIRECTION ( 'NONE',  ( -1.755985294532469921E-16, 1.000000000000000000, -1.338183447452831989E-16 ) ) ;
#17919 = CARTESIAN_POINT ( 'NONE',  ( 3.251888829344999898, 1516.793978928989873, 206.6294022811970024 ) ) ;
#17920 = CARTESIAN_POINT ( 'NONE',  ( 2.710413740429999940, 1447.398501226639837, 159.5173025968979914 ) ) ;
#17921 = CARTESIAN_POINT ( 'NONE',  ( -2.500000000000000000, 1435.233731004240099, 157.5834550647980166 ) ) ;
#17922 = CARTESIAN_POINT ( 'NONE',  ( 14.20165754500000155, 1416.819759739430083, 196.5061803919979866 ) ) ;
#17924 = ORIENTED_EDGE ( 'NONE', *, *, #83873, .T. ) ;
#17923 = CARTESIAN_POINT ( 'NONE',  ( -68.77190087506669158, 1379.747925807530009, 280.3125204381590265 ) ) ;
#17925 = EDGE_CURVE ( 'NONE', #106043, #87765, #48500, .T. ) ;
#17926 = CARTESIAN_POINT ( 'NONE',  ( -33.92723093277399471, 1436.576986543423800, 136.5095885520893546 ) ) ;
#17927 = VERTEX_POINT ( 'NONE', #68986 ) ;
#17928 = CARTESIAN_POINT ( 'NONE',  ( 13.60516184949999996, 1408.134943172929979, 264.8398108144980370 ) ) ;
#17929 = CARTESIAN_POINT ( 'NONE',  ( -24.42679094869999901, 1430.357408120730270, 206.6252289346280122 ) ) ;
#17931 = CARTESIAN_POINT ( 'NONE',  ( 16.36894064783199809, 1409.509743440080001, 192.9694638889519922 ) ) ;
#17930 = CARTESIAN_POINT ( 'NONE',  ( -11.42728233630000112, 1426.866742535030198, 121.9076973341980050 ) ) ;
#17932 = CARTESIAN_POINT ( 'NONE',  ( 6.563595869685000750, 1517.154223579619838, 211.4114704024570131 ) ) ;
#17933 = EDGE_CURVE ( 'NONE', #66318, #60506, #69217, .T. ) ;
#17934 = CARTESIAN_POINT ( 'NONE',  ( 28.92450383220691990, 1510.034133629718781, 217.1252577293115280 ) ) ;
#17935 = CIRCLE ( 'NONE', #32274, 1.999999999999990452 ) ;
#17936 = DIRECTION ( 'NONE',  ( 1.755985294532464991E-16, -1.000000000000000000, 1.338183447452830017E-16 ) ) ;
#17937 = FACE_OUTER_BOUND ( 'NONE', #8058, .T. ) ;
#17938 = CARTESIAN_POINT ( 'NONE',  ( -13.72550927608089921, 1379.647794360040052, 208.3261796023589909 ) ) ;
#17939 = CARTESIAN_POINT ( 'NONE',  ( 2.862715419362055869, 1516.551704408386058, 216.9343088578988841 ) ) ;
#17940 = CARTESIAN_POINT ( 'NONE',  ( 4.672324531150159999, 1508.551704408389924, 212.8263036817449745 ) ) ;
#17941 = CARTESIAN_POINT ( 'NONE',  ( -35.33152177045790410, 1437.220631632869981, 136.5361142770269964 ) ) ;
#17942 = EDGE_LOOP ( 'NONE', ( #6695, #77884, #38620, #29366, #110625 ) ) ;
#17943 = CARTESIAN_POINT ( 'NONE',  ( 9.694919637589999084, 1396.311071599129946, 201.2694852162679808 ) ) ;
#17944 = CARTESIAN_POINT ( 'NONE',  ( 10.44641616108000015, 1460.893522529900110, 207.9938650532610041 ) ) ;
#17945 = CARTESIAN_POINT ( 'NONE',  ( -18.12928259929999797, 1459.009197536229976, 227.9558348735980076 ) ) ;
#17946 = EDGE_LOOP ( 'NONE', ( #63319, #37943, #104856, #88261 ) ) ;
#17947 = VERTEX_POINT ( 'NONE', #70646 ) ;
#17948 = CARTESIAN_POINT ( 'NONE',  ( -29.22959469711409852, 1509.933780326070064, 211.7723416727030212 ) ) ;
#17949 = CARTESIAN_POINT ( 'NONE',  ( -11.73563908010000034, 1425.610159190430068, 144.1657657165980027 ) ) ;
#17950 = EDGE_CURVE ( 'NONE', #29914, #91726, #7026, .T. ) ;
#17951 = VERTEX_POINT ( 'NONE', #37000 ) ;
#17952 = CARTESIAN_POINT ( 'NONE',  ( -14.18795909183540083, 1380.146470109049915, 210.8218107588240002 ) ) ;
#17953 = CARTESIAN_POINT ( 'NONE',  ( -15.31509580213619870, 1508.249370024519976, 209.5650669845969958 ) ) ;
#17954 = CIRCLE ( 'NONE', #23326, 1.000000000000003553 ) ;
#17955 = CARTESIAN_POINT ( 'NONE',  ( -11.87174114537739911, 1432.759493913710003, 149.9813063557689929 ) ) ;
#17956 = CARTESIAN_POINT ( 'NONE',  ( -15.62061836090000000, 1461.188395550129826, 228.5769436422980050 ) ) ;
#17957 = CARTESIAN_POINT ( 'NONE',  ( 6.551899150602929822, 1508.551566291330118, 202.1600032511879874 ) ) ;
#17958 = CARTESIAN_POINT ( 'NONE',  ( 10.56406725279730097, 1452.658225117510028, 209.7434485084090170 ) ) ;
#17959 =( BOUNDED_SURFACE ( )  B_SPLINE_SURFACE ( 3, 2, ( 
 ( #77787, #61011, #86733 ),
 ( #10023, #68307, #16729 ),
 ( #50392, #102415, #44193 ),
 ( #78336, #85060, #76127 ),
 ( #110268, #42515, #33545 ),
 ( #67743, #101852, #25145 ),
 ( #95689, #62678, #96800 ),
 ( #35783, #104080, #62115 ),
 ( #79989, #3861, #87289 ),
 ( #105756, #11146, #88391 ),
 ( #63227, #97332, #3309 ),
 ( #53151, #54801, #69967 ),
 ( #37439, #11679, #71072 ),
 ( #37989, #29041, #10584 ) ),
 .UNSPECIFIED., .F., .F., .T. ) 
 B_SPLINE_SURFACE_WITH_KNOTS ( ( 4, 2, 2, 2, 2, 2, 4 ),
 ( 3, 3 ),
 ( 3.503057219300664826E-16, 0.0009443072508239318524, 0.001416460876235722463, 0.001888614501647513291, 0.002360768127059304118, 0.002832921752471094512, 0.003777229003294676167 ),
 ( 0.000000000000000000, 1.000000000000000000 ),
 .UNSPECIFIED. ) 
 GEOMETRIC_REPRESENTATION_ITEM ( )  RATIONAL_B_SPLINE_SURFACE ( (
 ( 1.000000000000000000, 0.9376006582765973318, 1.000000000000000000),
 ( 1.000000000000000000, 0.9283977714730341502, 1.000000000000000000),
 ( 1.000000000000000000, 0.9189750060488427463, 1.000000000000000000),
 ( 1.000000000000000000, 0.9042792056123200028, 1.000000000000000000),
 ( 1.000000000000000000, 0.8992469033844596726, 1.000000000000000000),
 ( 1.000000000000000000, 0.8891280264680869738, 1.000000000000000000),
 ( 1.000000000000000000, 0.8840337471675274728, 1.000000000000000000),
 ( 1.000000000000000000, 0.8736395124163596204, 1.000000000000000000),
 ( 1.000000000000000000, 0.8683406746556232569, 1.000000000000000000),
 ( 1.000000000000000000, 0.8573361860704289406, 1.000000000000000000),
 ( 1.000000000000000000, 0.8516508399493524228, 1.000000000000000000),
 ( 1.000000000000000000, 0.8340914917071279300, 1.000000000000000000),
 ( 1.000000000000000000, 0.8215597275858022019, 1.000000000000000000),
 ( 1.000000000000000000, 0.8070209408750096403, 1.000000000000000000) ) ) 
 REPRESENTATION_ITEM ( '' )  SURFACE ( )  );
#17960 = CARTESIAN_POINT ( 'NONE',  ( -4.576312612474013441, 1517.051704408389924, 222.3843417993991807 ) ) ;
#17961 = CARTESIAN_POINT ( 'NONE',  ( -94.11669641235350525, 1384.854232109579698, 294.6094501371869683 ) ) ;
#17962 = ORIENTED_EDGE ( 'NONE', *, *, #97292, .T. ) ;
#17963 = CARTESIAN_POINT ( 'NONE',  ( -3.261635970955000019, 1516.613881697390070, 202.1867125516770045 ) ) ;
#17964 = CARTESIAN_POINT ( 'NONE',  ( -2.286472924554999953, 1516.883361325900069, 209.8798303522490016 ) ) ;
#17965 = EDGE_LOOP ( 'NONE', ( #12831, #26970, #14100, #2000, #80889 ) ) ;
#17966 = CARTESIAN_POINT ( 'NONE',  ( 11.81696617721230069, 1429.121889755289885, 148.9598804145299766 ) ) ;
#17967 = EDGE_CURVE ( 'NONE', #93985, #25781, #3131, .T. ) ;
#17968 = CARTESIAN_POINT ( 'NONE',  ( 20.60060554280000034, 1507.884458093629974, 227.6638854010979856 ) ) ;
#17969 = ORIENTED_EDGE ( 'NONE', *, *, #104187, .F. ) ;
#17970 = CARTESIAN_POINT ( 'NONE',  ( 7.709069255566407541, 1423.240024452770740, 139.1418590084687423 ) ) ;
#17971 = CARTESIAN_POINT ( 'NONE',  ( -1.635875587731045355, 1484.273925081808557, 182.6549239315091029 ) ) ;
#17972 = CARTESIAN_POINT ( 'NONE',  ( 7.245928414539999807, 1509.166093783229826, 236.9901212716980012 ) ) ;
#17973 = VECTOR ( 'NONE', #1859, 1000.000000000000000 ) ;
#17974 = CARTESIAN_POINT ( 'NONE',  ( -7.987427797640509475, 1490.123333955630414, 216.6223879589213936 ) ) ;
#17975 = CARTESIAN_POINT ( 'NONE',  ( -5.127859024660000209, 1422.417124035330062, 185.6440635277980107 ) ) ;
#17976 = EDGE_CURVE ( 'NONE', #58087, #10311, #80410, .T. ) ;
#17977 = CARTESIAN_POINT ( 'NONE',  ( 4.259181585509999479, 1408.384021400730035, 270.3898288651980124 ) ) ;
#17978 = CARTESIAN_POINT ( 'NONE',  ( 9.211627749346281036, 1450.348376029699921, 208.8206138348359957 ) ) ;
#17979 = CARTESIAN_POINT ( 'NONE',  ( -12.58738889680580186, 1502.045147876100145, 211.1486701620410145 ) ) ;
#17980 = CARTESIAN_POINT ( 'NONE',  ( 6.983043359149999851, 1493.573093954689966, 217.9908564108290250 ) ) ;
#17981 = CARTESIAN_POINT ( 'NONE',  ( -14.11459548090000027, 1379.710415317729939, 208.2104247299010069 ) ) ;
#17982 = CARTESIAN_POINT ( 'NONE',  ( 23.86274566002959929, 1440.678159878850011, 206.2105284970400021 ) ) ;
#17984 = CARTESIAN_POINT ( 'NONE',  ( 15.50242774170000004, 1471.316885392330050, 194.6525715419979861 ) ) ;
#17983 = CARTESIAN_POINT ( 'NONE',  ( -3.672024168570000136, 1497.313529941189927, 198.4698546893989715 ) ) ;
#17985 = CARTESIAN_POINT ( 'NONE',  ( 31.34137657934009979, 1512.187213306747481, 196.3411265156547358 ) ) ;
#17986 = AXIS2_PLACEMENT_3D ( 'NONE', #84239, #13706, #7538 ) ;
#17987 = CARTESIAN_POINT ( 'NONE',  ( 17.93107151423210155, 1421.416072919849967, 225.1143211638089952 ) ) ;
#17988 = CARTESIAN_POINT ( 'NONE',  ( -4.566658896609312457, 1506.397480193153115, 187.6488660611327361 ) ) ;
#17989 = ORIENTED_EDGE ( 'NONE', *, *, #103560, .T. ) ;
#17990 = CARTESIAN_POINT ( 'NONE',  ( 16.95839603458921729, 1517.034034081944128, 223.2333545903914285 ) ) ;
#17991 = CARTESIAN_POINT ( 'NONE',  ( -4.363122647530000009, 1409.354802298927325, 137.0999999980979851 ) ) ;
#17992 = EDGE_CURVE ( 'NONE', #50150, #32822, #43759, .T. ) ;
#17993 = CARTESIAN_POINT ( 'NONE',  ( -2.913496927302146933, 1484.798880128765177, 183.2196020003875390 ) ) ;
#17994 = CARTESIAN_POINT ( 'NONE',  ( -16.95309613902585255, 1410.872492358897262, 191.9186258755552217 ) ) ;
#17995 =( BOUNDED_CURVE ( )  B_SPLINE_CURVE ( 3, ( #87937, #44276, #18477, #78990 ),
 .UNSPECIFIED., .F., .T. ) 
 B_SPLINE_CURVE_WITH_KNOTS ( ( 4, 4 ),
 ( 5.447131716497384701, 6.315249268837864527 ),
 .UNSPECIFIED. ) 
 CURVE ( )  GEOMETRIC_REPRESENTATION_ITEM ( )  RATIONAL_B_SPLINE_CURVE ( ( 1.000000000000000000, 0.9381775213690333182, 0.9381775213690333182, 1.000000000000000000 ) ) 
 REPRESENTATION_ITEM ( '' )  );
#17997 = VERTEX_POINT ( 'NONE', #69539 ) ;
#17996 = CARTESIAN_POINT ( 'NONE',  ( -11.26215388574009957, 1500.310609260709953, 210.9023932557140029 ) ) ;
#17998 = CARTESIAN_POINT ( 'NONE',  ( -9.094910632070000389, 1384.931050598290085, 199.9427863282390092 ) ) ;
#17999 = AXIS2_PLACEMENT_3D ( 'NONE', #45694, #4223, #80378 ) ;
#18000 = DIRECTION ( 'NONE',  ( 1.755985294532469921E-16, -1.000000000000000000, 1.338183447452831989E-16 ) ) ;
#18001 = EDGE_CURVE ( 'NONE', #54902, #24288, #85754, .T. ) ;
#18002 = CARTESIAN_POINT ( 'NONE',  ( -11.25881761529999991, 1429.196009723030102, 150.7919537440980093 ) ) ;
#18003 = CARTESIAN_POINT ( 'NONE',  ( 20.08180131570000171, 1474.154670883989866, 211.0997262866790152 ) ) ;
#18004 = CARTESIAN_POINT ( 'NONE',  ( -10.83132596424780125, 1461.840861733669954, 211.0446618225340103 ) ) ;
#18005 = CARTESIAN_POINT ( 'NONE',  ( -18.22821675530000007, 1443.229620277490085, 204.5519556382290034 ) ) ;
#18006 = B_SPLINE_CURVE_WITH_KNOTS ( 'NONE', 3,
 ( #12292, #19025, #53228, #28559, #44831, #62757, #36400 ),
 .UNSPECIFIED., .F., .F.,
 ( 4, 3, 4 ),
 ( -157.7844419379999863, -101.5361819250880018, -30.93609007885059725 ),
 .UNSPECIFIED. ) ;
#18007 = CYLINDRICAL_SURFACE ( 'NONE', #96758, 1.000000000000000888 ) ;
#18008 = CARTESIAN_POINT ( 'NONE',  ( -16.89844956606500048, 1513.192861445620110, 222.1868582675669757 ) ) ;
#18009 = CARTESIAN_POINT ( 'NONE',  ( 14.34346040870000216, 1410.403127989829954, 227.8390325281980040 ) ) ;
#18010 = EDGE_CURVE ( 'NONE', #92059, #60698, #56019, .T. ) ;
#18011 = CARTESIAN_POINT ( 'NONE',  ( -10.51573792566800059, 1480.737017572810146, 208.3487723898410025 ) ) ;
#18012 = CARTESIAN_POINT ( 'NONE',  ( -16.17783063698000134, 1459.145687810399977, 230.7168772285679950 ) ) ;
#18013 = CARTESIAN_POINT ( 'NONE',  ( 1.118353215965000036, 1516.977201124959947, 206.6281488911770055 ) ) ;
#18014 = CARTESIAN_POINT ( 'NONE',  ( 30.19617742020000151, 1414.287258031230067, 267.1521104148980044 ) ) ;
#18015 = CARTESIAN_POINT ( 'NONE',  ( 7.012921545624998920, 1508.551704408389924, 214.6352815241970120 ) ) ;
#18016 = CARTESIAN_POINT ( 'NONE',  ( 22.93100030269999934, 1430.293864573130122, 203.3539861534579813 ) ) ;
#18017 = EDGE_CURVE ( 'NONE', #14033, #90411, #23081, .T. ) ;
#18018 = EDGE_CURVE ( 'NONE', #69179, #16271, #12341, .T. ) ;
#18019 = CARTESIAN_POINT ( 'NONE',  ( -20.92707481170000250, 1427.944386893930186, 220.6468670353979746 ) ) ;
#18020 = CARTESIAN_POINT ( 'NONE',  ( 18.42577555256999844, 1424.509265906519886, 223.4215472205989954 ) ) ;
#18021 = DIRECTION ( 'NONE',  ( 0.000000000000000000, 0.000000000000000000, 1.000000000000000000 ) ) ;
#18022 = DIRECTION ( 'NONE',  ( -0.02578658883684968942, 0.9994800766169525952, 0.01935531663212984241 ) ) ;
#18023 = CARTESIAN_POINT ( 'NONE',  ( -6.972733166630000312, 1409.156553594930301, 196.2309095765980089 ) ) ;
#18024 = CARTESIAN_POINT ( 'NONE',  ( -18.89907699009999931, 1416.828040557830036, 207.5749716938179859 ) ) ;
#18025 = CARTESIAN_POINT ( 'NONE',  ( -13.44162146400000069, 1443.167077655089997, 187.7002249684979915 ) ) ;
#18026 = CARTESIAN_POINT ( 'NONE',  ( -3.578645720892979831, 1485.309967107140210, 197.7694655723200015 ) ) ;
#18027 = B_SPLINE_SURFACE_WITH_KNOTS ( 'NONE', 5, 5, ( 
 ( #50410, #7823, #104099, #86192, #1661, #79463, #10039, #43649, #96256 ),
 ( #69982, #94581, #78920, #18969, #104651, #43100, #44770, #44209, #86748 ),
 ( #52059, #17299, #27948, #68874, #78352, #103539, #10598, #52610, #87306 ),
 ( #94035, #69426, #2226, #36342, #102430, #9484, #34684, #35800, #26274 ),
 ( #27389, #70533, #62129, #19531, #53737, #51494, #26843, #61568, #77802 ),
 ( #53164, #2774, #45325, #87874, #95153, #61031, #11164, #68322, #95703 ),
 ( #102976, #25713, #59914, #35239, #85626, #8926, #77260, #1111, #559 ),
 ( #60463, #17859, #18412, #34868, #75239, #42174, #85258, #76325, #16930 ),
 ( #43288, #94211, #102596, #9121, #77436, #34319, #24783, #41623, #92558 ),
 ( #33207, #15828, #25897, #51684, #41062, #17486, #67397, #26458, #69056 ),
 ( #50031, #7461, #93647, #84160, #15292, #110475, #8008, #16383, #60095 ),
 ( #76886, #103157, #75777, #735, #102059, #195, #109930, #101495, #24249 ),
 ( #58985, #51131, #92022, #42727, #59535, #85823, #93112, #109389, #58430 ),
 ( #33753, #25341, #32666, #66844, #50580, #84708, #8555, #67950, #68497 ),
 ( #49485, #83608, #6905, #100954, #37079, #28689, #35988, #1853, #2962 ),
 ( #71283, #52797, #19723, #86928, #27033, #87499, #11344, #88605, #94777 ),
 ( #62893, #70176, #104287, #105396, #69612, #97003, #10219, #53924, #44397 ),
 ( #10789, #45516, #11887, #18054, #96444, #103734, #80192, #52249, #36531 ),
 ( #20266, #61222, #35425, #43832, #54467, #27576, #78539, #61761, #79658 ),
 ( #46059, #44959, #3510, #95887, #37634, #71839, #19147, #105957, #9661 ),
 ( #53354, #79107, #60653, #77978, #2414, #70728, #104840, #28128, #86375 ),
 ( #62319, #95336, #1286, #18597, #88059, #55557, #108132, #29235, #38179 ),
 ( #89682, #57216, #31425, #12964, #65052, #13506, #14064, #65607, #22447 ),
 ( #47147, #99165, #107587, #99719, #38722, #46614, #21896, #89138, #81272 ),
 ( #30873, #41902, #80744, #39281, #30324, #76057, #56647, #73456, #82396 ),
 ( #5693, #4589, #48253, #7739, #72897, #91342, #90781, #39837, #107037 ),
 ( #72359, #64513, #21350, #74000, #16122, #23012, #50327, #84453, #63964 ),
 ( #106491, #20813, #81822, #63424, #12424, #4053, #98628, #56094, #97542 ),
 ( #55011, #47694, #29776, #98079, #90221, #5125, #86656, #69335, #25629 ),
 ( #26182, #60937, #27305, #33474, #35151, #8281, #18882, #101783, #86109 ),
 ( #1571, #42445, #84986, #93394, #44123, #51403, #59821, #85535, #18333 ),
 ( #44680, #95066, #10508, #87218, #52524, #60371, #68785, #9951, #35704 ),
 ( #8830, #76603, #69893, #43565, #77172, #25073, #51968, #78258, #43015 ),
 ( #475, #110755, #104008, #61486, #67676, #93941, #95615, #110200, #34046 ),
 ( #17207, #53080, #59276, #34599, #103443, #94492, #16659, #50857, #26748 ),
 ( #102885, #68236, #77716, #102346, #17764, #9403, #1027, #27863, #105127 ),
 ( #80478, #89966, #19445, #88874, #79928, #13240, #72109, #12159, #21089 ),
 ( #55292, #62616, #63700, #55844, #28418, #106762, #46349, #97810, #96733 ),
 ( #11069, #20004, #71006, #3796, #30053, #29507, #37927, #89422, #2692 ),
 ( #45238, #70448, #20540, #106223, #62043, #96169, #3244, #54198, #12712 ),
 ( #37370, #53643, #79376, #87787, #45795, #36816, #21639, #46896, #81020 ),
 ( #36259, #88323, #104568, #105692, #4329, #38459, #11618, #72633, #54744 ),
 ( #78825, #71571, #28975, #64244, #63163, #98366, #97264, #2136, #31708 ),
 ( #101102, #73177, #48538, #23845, #15445, #22732, #99454, #100564, #56382 ),
 ( #39571, #6514, #73744, #13789, #74295, #108984, #75394, #81553, #83224 ),
 ( #66992, #47973, #65894, #5412, #82113, #100011, #92174, #58036, #7067 ),
 ( #107321, #5967, #57496, #56934, #92716, #32269, #58586, #24402, #49636 ),
 ( #40112, #83773, #41223, #23301, #91063, #107868, #109533, #91621, #14347 ),
 ( #14897, #32807, #82676, #47430, #108426, #31156, #4855, #39000, #30616 ),
 ( #64803, #98912, #90514, #40667, #65346, #22184, #49088, #74840, #66451 ),
 ( #894, #94933, #9276, #15992, #76474, #51839, #94357, #18205, #25498 ) ),
 .UNSPECIFIED., .F., .F., .F.,
 ( 6, 3, 3, 3, 3, 3, 3, 3, 3, 3, 3, 3, 3, 3, 3, 3, 6 ),
 ( 6, 3, 6 ),
 ( 0.000000000000000000, 28.69702819429999963, 61.04778752440000034, 93.62768910810000023, 123.7336603250000024, 156.1762685979999787, 187.3272846180000215, 220.4669312460000015, 237.3878297990000021, 254.2938300590000154, 289.2398204710000300, 325.3030936050000150, 360.8626869010000178, 395.8828220460000011, 432.6128460950000090, 468.8934854820000169, 502.1482307969999965 ),
 ( -0.0001008871253083600000, 2.001700839520000219, 3.002551259279999663 ),
 .UNSPECIFIED. ) ;
#18028 = CARTESIAN_POINT ( 'NONE',  ( 4.363122647530000009, 1421.971318475729959, 172.2701767054979882 ) ) ;
#18029 = CARTESIAN_POINT ( 'NONE',  ( -4.771756610380000652, 1496.505580869889855, 219.3152549879989692 ) ) ;
#18030 = EDGE_LOOP ( 'NONE', ( #98688, #14431, #55245, #47364 ) ) ;
#18031 = CARTESIAN_POINT ( 'NONE',  ( -2.838447005044999916, 1511.534866634170157, 201.5062903025470007 ) ) ;
#18032 = CARTESIAN_POINT ( 'NONE',  ( -14.30375442816609954, 1409.412558498570206, 204.8191087406950146 ) ) ;
#18033 = CARTESIAN_POINT ( 'NONE',  ( -11.65744291596249838, 1508.186430388969939, 208.3002178115879985 ) ) ;
#18034 = LINE ( 'NONE', #103138, #65255 ) ;
#18035 = CARTESIAN_POINT ( 'NONE',  ( -18.40068035370000032, 1473.290853966130044, 267.7101340507979899 ) ) ;
#18036 = CARTESIAN_POINT ( 'NONE',  ( 0.1762907655658970119, 1420.387354559859887, 183.3288319911129918 ) ) ;
#18037 = EDGE_CURVE ( 'NONE', #3400, #99658, #62112, .T. ) ;
#18038 = CARTESIAN_POINT ( 'NONE',  ( 18.04484862309950088, 1421.101146633960070, 223.7483925777569880 ) ) ;
#18039 = CARTESIAN_POINT ( 'NONE',  ( -61.29572242790209913, 1384.690799301989955, 283.1176806947750038 ) ) ;
#18040 = CARTESIAN_POINT ( 'NONE',  ( -17.14540223173099776, 1384.945687311829943, 201.0017889155920159 ) ) ;
#18041 = VECTOR ( 'NONE', #35325, 1000.000000000000000 ) ;
#18042 = CARTESIAN_POINT ( 'NONE',  ( -5.238827773017599831, 1374.990239134210015, 214.8178773404370077 ) ) ;
#18043 = CARTESIAN_POINT ( 'NONE',  ( 11.94908641555320017, 1415.673583082879986, 223.2663781018690088 ) ) ;
#18044 = DIRECTION ( 'NONE',  ( 0.9970203751124364633, -0.07713865185920967815, 0.000000000000000000 ) ) ;
#18045 = CARTESIAN_POINT ( 'NONE',  ( -16.50400130224731754, 1525.907212628473644, 236.2546788475584094 ) ) ;
#18046 = CARTESIAN_POINT ( 'NONE',  ( -9.094129269030000629, 1384.954944735329946, 199.9429221374590213 ) ) ;
#18047 = CARTESIAN_POINT ( 'NONE',  ( -23.36195796790000401, 1409.893412594229858, 207.9384553132279905 ) ) ;
#18048 = CIRCLE ( 'NONE', #46713, 1.999999999999999556 ) ;
#18049 = CARTESIAN_POINT ( 'NONE',  ( -113.7188159025760115, 1310.214785017039276, 305.1696626168879902 ) ) ;
#18050 = B_SPLINE_CURVE_WITH_KNOTS ( 'NONE', 3,
 ( #49037, #66395, #56876, #83172, #98859, #22123, #7008, #41166, #108923, #31654, #32215, #73691, #91006, #90453, #14296, #82051, #5916, #6463, #100515, #40612, #23793, #99952, #5357, #92118, #65834, #23247, #49583, #107817, #74783, #66941, #48485, #24349, #58533, #13180, #47368, #81494, #68049, #33858, #86887, #102158 ),
 .UNSPECIFIED., .F., .F.,
 ( 4, 3, 3, 3, 3, 3, 3, 3, 3, 3, 3, 3, 3, 4 ),
 ( -7.530765448250459571, -7.506223803491129942, -7.257045730312249532, -6.983326012374050151, -6.698284398290460295, -6.381132500363879245, -5.928019582097629581, -5.598363948206119822, -5.308105043320740180, -5.156242663369150492, -4.738290659457769394, -4.262467497528719562, -3.657517831626029725, -3.085444082959999612 ),
 .UNSPECIFIED. ) ;
#18051 = FACE_OUTER_BOUND ( 'NONE', #21061, .T. ) ;
#18052 = CARTESIAN_POINT ( 'NONE',  ( 10.43532605497630072, 1480.514957649700136, 207.6513091103709883 ) ) ;
#18053 = CARTESIAN_POINT ( 'NONE',  ( 2.451271202390000070, 1433.447543843880112, 150.3250444719979839 ) ) ;
#18054 = CARTESIAN_POINT ( 'NONE',  ( 18.98377022170240025, 1454.978415555989841, 200.5246066841559696 ) ) ;
#18055 = CARTESIAN_POINT ( 'NONE',  ( 16.48227147120181257, 1525.651286436459941, 181.5607904124787808 ) ) ;
#18056 = CARTESIAN_POINT ( 'NONE',  ( -21.46486174371069922, 1504.440211353449740, 215.6677629390230209 ) ) ;
#18059 = CARTESIAN_POINT ( 'NONE',  ( -9.393822458599998981, 1383.815214525520105, 200.1452963205690025 ) ) ;
#18058 = VECTOR ( 'NONE', #51221, 1000.000000000000000 ) ;
#18057 = LINE ( 'NONE', #55013, #37185 ) ;
#18060 = CARTESIAN_POINT ( 'NONE',  ( -4.992349863779999453, 1391.620913471789891, 203.7504116504090064 ) ) ;
#18061 = CARTESIAN_POINT ( 'NONE',  ( -3.968827103576990201, 1517.151704408390060, 229.5396913781519856 ) ) ;
#18062 = CARTESIAN_POINT ( 'NONE',  ( -10.81618613060000023, 1491.239992459889891, 211.1797723353990079 ) ) ;
#18063 = CARTESIAN_POINT ( 'NONE',  ( 7.173571134148669870, 1448.589511863430062, 201.7444442637240059 ) ) ;
#18064 = CARTESIAN_POINT ( 'NONE',  ( -0.6104152826046118641, 1418.823154379500011, 184.7568847501300127 ) ) ;
#18065 = CIRCLE ( 'NONE', #93200, 2.000000000000002220 ) ;
#18066 = CARTESIAN_POINT ( 'NONE',  ( -3.263521942484999716, 1516.676340709600026, 203.3494421577970002 ) ) ;
#18067 = CARTESIAN_POINT ( 'NONE',  ( -9.382268578863946829, 1398.191384707091629, 218.1279820238655418 ) ) ;
#18068 = CYLINDRICAL_SURFACE ( 'NONE', #3336, 12.50000000000001066 ) ;
#18069 = FACE_BOUND ( 'NONE', #40847, .T. ) ;
#18070 = CARTESIAN_POINT ( 'NONE',  ( 1.913188568150000046, 1508.750155563429871, 237.3579719449979848 ) ) ;
#18071 = CARTESIAN_POINT ( 'NONE',  ( 5.430409578133730264, 1505.407880561079992, 219.8354462761509751 ) ) ;
#18072 = CARTESIAN_POINT ( 'NONE',  ( 38.05425021522230367, 1450.256561828500026, 135.6620645644130150 ) ) ;
#18074 = ORIENTED_EDGE ( 'NONE', *, *, #15389, .T. ) ;
#18073 = CARTESIAN_POINT ( 'NONE',  ( -64.26953522495749382, 1379.737737548759924, 273.6740357258199765 ) ) ;
#18075 = ORIENTED_EDGE ( 'NONE', *, *, #80371, .T. ) ;
#18076 = CARTESIAN_POINT ( 'NONE',  ( 11.82056980545410063, 1433.695608034110137, 150.7613404324029887 ) ) ;
#18077 = CARTESIAN_POINT ( 'NONE',  ( 28.10198114769999833, 1509.875926101730101, 215.6436498675279836 ) ) ;
#18078 = VERTEX_POINT ( 'NONE', #37560 ) ;
#18079 = CARTESIAN_POINT ( 'NONE',  ( -106.5010113160000174, 1379.147773116859980, 307.7477130958589555 ) ) ;
#18080 = CARTESIAN_POINT ( 'NONE',  ( -10.36221610374189872, 1448.183279349199893, 208.6963155564749854 ) ) ;
#18081 = CARTESIAN_POINT ( 'NONE',  ( -4.491293115488388388, 1508.884207226183435, 211.6097811125350177 ) ) ;
#18083 = CARTESIAN_POINT ( 'NONE',  ( 2.329729395510000245, 1427.373795049630189, 123.0297916884979941 ) ) ;
#18082 = CARTESIAN_POINT ( 'NONE',  ( 0.000000000000000000, 1518.913060387330006, 185.4225825198192013 ) ) ;
#18084 = CARTESIAN_POINT ( 'NONE',  ( 17.93739292209999903, 1507.814075490329969, 230.5553894001980098 ) ) ;
#18085 = CIRCLE ( 'NONE', #39520, 2.000000000000001776 ) ;
#18086 = CARTESIAN_POINT ( 'NONE',  ( 3.848404275880000114, 1507.638435329329923, 181.6079968732980205 ) ) ;
#18087 = CARTESIAN_POINT ( 'NONE',  ( 1.939364658240000150, 1467.845018752989972, 219.0547953187090116 ) ) ;
#18088 = CARTESIAN_POINT ( 'NONE',  ( 15.26168084529999902, 1409.446010026229715, 225.6870430949980175 ) ) ;
#18089 = CARTESIAN_POINT ( 'NONE',  ( -5.770883602015000058, 1516.603620185149794, 211.4160555996369908 ) ) ;
#18090 = CARTESIAN_POINT ( 'NONE',  ( 13.98791200557839964, 1415.441076448340027, 197.3320725003540019 ) ) ;
#18092 = AXIS2_PLACEMENT_3D ( 'NONE', #49588, #8653, #17027 ) ;
#18091 = CARTESIAN_POINT ( 'NONE',  ( -9.996465492614740711, 1423.286309259070094, 207.3024158817219984 ) ) ;
#18093 = CARTESIAN_POINT ( 'NONE',  ( 6.557434856144999991, 1513.513616978020082, 201.6636742605270172 ) ) ;
#18094 = ORIENTED_EDGE ( 'NONE', *, *, #30262, .T. ) ;
#18095 = CARTESIAN_POINT ( 'NONE',  ( 13.47042191939980071, 1434.942646400420017, 148.9306420637369968 ) ) ;
#18096 = CARTESIAN_POINT ( 'NONE',  ( -0.8603290292595530131, 1431.922339058240141, 200.7526126593139963 ) ) ;
#18097 = ORIENTED_EDGE ( 'NONE', *, *, #95424, .T. ) ;
#18098 = VERTEX_POINT ( 'NONE', #3980 ) ;
#18099 = CARTESIAN_POINT ( 'NONE',  ( -7.072298227815000615, 1512.974587999920004, 216.2923917488670043 ) ) ;
#18100 = CARTESIAN_POINT ( 'NONE',  ( -1.753158309049999808, 1464.912754134729994, 237.4770670691980001 ) ) ;
#18101 = CARTESIAN_POINT ( 'NONE',  ( -9.972378110560478959, 1407.313660260299912, 200.5612547303060182 ) ) ;
#18102 = CARTESIAN_POINT ( 'NONE',  ( 0.01010282929720150019, 1516.939452820819952, 216.8414868732370167 ) ) ;
#18103 = CARTESIAN_POINT ( 'NONE',  ( 10.52285531690000120, 1461.267078505790096, 209.0122360621460018 ) ) ;
#18104 = AXIS2_PLACEMENT_3D ( 'NONE', #15959, #25466, #68074 ) ;
#18105 = CARTESIAN_POINT ( 'NONE',  ( 12.45034049356619832, 1421.619540909540092, 207.5029415923690124 ) ) ;
#18106 = CARTESIAN_POINT ( 'NONE',  ( 13.04207810306199988, 1409.368499790489750, 192.3005055522939983 ) ) ;
#18107 = CARTESIAN_POINT ( 'NONE',  ( 4.249254207745330802, 1446.470040732190000, 161.2344365711890077 ) ) ;
#18108 = CARTESIAN_POINT ( 'NONE',  ( 8.637056729921679832, 1437.983744640310078, 209.9529184353999938 ) ) ;
#18109 = VERTEX_POINT ( 'NONE', #99091 ) ;
#18110 = CARTESIAN_POINT ( 'NONE',  ( -7.725372170364999569, 1517.158319634930194, 206.2490093095770192 ) ) ;
#18111 = ORIENTED_EDGE ( 'NONE', *, *, #101368, .F. ) ;
#18112 = CARTESIAN_POINT ( 'NONE',  ( 20.92687816970969550, 1440.913060387330006, 221.9350866778629836 ) ) ;
#18113 = EDGE_CURVE ( 'NONE', #78057, #69033, #6605, .T. ) ;
#18114 = CARTESIAN_POINT ( 'NONE',  ( -19.75079221190000212, 1509.023212918529907, 229.8582975788980036 ) ) ;
#18115 = EDGE_LOOP ( 'NONE', ( #59069, #108185 ) ) ;
#18116 = CARTESIAN_POINT ( 'NONE',  ( 26.41530183785989649, 1448.997685820419974, 136.8834598208839850 ) ) ;
#18117 = CARTESIAN_POINT ( 'NONE',  ( -11.05974434320000022, 1410.673379371429974, 188.8342600372980087 ) ) ;
#18118 = CARTESIAN_POINT ( 'NONE',  ( -24.65398899419999879, 1442.417487969639978, 210.7516708981580109 ) ) ;
#18120 = ORIENTED_EDGE ( 'NONE', *, *, #63971, .T. ) ;
#18119 = CARTESIAN_POINT ( 'NONE',  ( -11.27186228789999944, 1414.983771850430003, 195.8113390693980023 ) ) ;
#18121 = CARTESIAN_POINT ( 'NONE',  ( -6.170974612161120199, 1511.326458810320219, 201.5850279059119714 ) ) ;
#18122 = CARTESIAN_POINT ( 'NONE',  ( 0.3382504354559999760, 1405.989871386730101, 266.9611136494980315 ) ) ;
#18123 = CARTESIAN_POINT ( 'NONE',  ( -1.925297170580940076, 1519.551704408389924, 187.5582988486569889 ) ) ;
#18124 = CARTESIAN_POINT ( 'NONE',  ( -5.292247061280000331, 1391.913060387289988, 209.1218459616989946 ) ) ;
#18126 = CARTESIAN_POINT ( 'NONE',  ( -2.011314089155299634, 1484.247616858960100, 182.9841112829520000 ) ) ;
#18125 = CARTESIAN_POINT ( 'NONE',  ( 21.38516915557947584, 1522.906561336852974, 180.3939891059719969 ) ) ;
#18127 = CARTESIAN_POINT ( 'NONE',  ( -2.288357445734999995, 1517.116049120239950, 214.9102823043970147 ) ) ;
#18128 = CARTESIAN_POINT ( 'NONE',  ( -2.681276382835120042, 1429.097449907909777, 200.1427365742090103 ) ) ;
#18129 = CARTESIAN_POINT ( 'NONE',  ( -22.52564151159999639, 1509.699673122230024, 190.3321270483980072 ) ) ;
#18130 = CARTESIAN_POINT ( 'NONE',  ( 29.24528532949999970, 1509.871747146429925, 208.3253336781129974 ) ) ;
#18131 = CARTESIAN_POINT ( 'NONE',  ( 2.299983577604999940, 1516.861367446839949, 211.4044688825970013 ) ) ;
#18132 = CARTESIAN_POINT ( 'NONE',  ( -11.82493131255569985, 1482.231903543040062, 207.8362869629800116 ) ) ;
#18133 = AXIS2_PLACEMENT_3D ( 'NONE', #108180, #31471, #65652 ) ;
#18134 = CARTESIAN_POINT ( 'NONE',  ( 30.25946001110534311, 1524.776010967693537, 221.7839220010320105 ) ) ;
#18136 = ORIENTED_EDGE ( 'NONE', *, *, #54811, .T. ) ;
#18135 = CARTESIAN_POINT ( 'NONE',  ( -79.49029774420000649, 1385.156174356060092, 282.9512253370589860 ) ) ;
#18137 = CARTESIAN_POINT ( 'NONE',  ( 33.60183515679999999, 1443.049082915059898, 248.0844435633979970 ) ) ;
#18138 = EDGE_CURVE ( 'NONE', #21803, #104898, #41730, .T. ) ;
#18139 = CARTESIAN_POINT ( 'NONE',  ( 10.62827625601449988, 1490.977054330010105, 211.9199658921150160 ) ) ;
#18140 = CARTESIAN_POINT ( 'NONE',  ( -29.03287634025529940, 1509.926910769670030, 213.4187435708539908 ) ) ;
#18141 = CARTESIAN_POINT ( 'NONE',  ( -8.482879236748889440, 1508.704785055359935, 235.6989384136039973 ) ) ;
#18142 = EDGE_CURVE ( 'NONE', #68439, #46649, #17697, .T. ) ;
#18143 = CARTESIAN_POINT ( 'NONE',  ( -21.75818116419999981, 1452.902822741230011, 221.5405819497979678 ) ) ;
#18144 = EDGE_CURVE ( 'NONE', #8717, #33774, #88554, .T. ) ;
#18145 = VECTOR ( 'NONE', #100803, 1000.000000000000227 ) ;
#18147 = CARTESIAN_POINT ( 'NONE',  ( 19.02030571170000073, 1456.697257245530182, 226.2527947047979922 ) ) ;
#18146 = CARTESIAN_POINT ( 'NONE',  ( 11.86563475029999992, 1432.300009996690051, 149.9825381228980063 ) ) ;
#18148 = CARTESIAN_POINT ( 'NONE',  ( -8.840129632021261230, 1448.960675403350024, 211.5120822850410036 ) ) ;
#18149 = CARTESIAN_POINT ( 'NONE',  ( -108.3715397873749993, 1382.864756451370113, 310.7319415575520338 ) ) ;
#18150 = VERTEX_POINT ( 'NONE', #75588 ) ;
#18151 = CARTESIAN_POINT ( 'NONE',  ( 7.325541787135000149, 1516.710692850270107, 204.1167749238070144 ) ) ;
#18152 = CARTESIAN_POINT ( 'NONE',  ( 0.3370331515910000020, 1406.265758353229785, 269.2946826180980224 ) ) ;
#18153 = CARTESIAN_POINT ( 'NONE',  ( 27.85007275959999617, 1509.193792694529975, 207.4562351974080059 ) ) ;
#18154 = EDGE_CURVE ( 'NONE', #32551, #1227, #24027, .T. ) ;
#18155 = FACE_OUTER_BOUND ( 'NONE', #105281, .T. ) ;
#18156 = FACE_OUTER_BOUND ( 'NONE', #53531, .T. ) ;
#18157 = CARTESIAN_POINT ( 'NONE',  ( -39.38489486480609969, 1449.784184279609917, 136.1650281365439810 ) ) ;
#18158 = CARTESIAN_POINT ( 'NONE',  ( -1.636741614903409969, 1469.777368438049962, 219.0527109355280118 ) ) ;
#18159 = VECTOR ( 'NONE', #100408, 1000.000000000000000 ) ;
#18160 = CARTESIAN_POINT ( 'NONE',  ( -38.33208885764259577, 1440.913060391839963, 256.8080927262569730 ) ) ;
#18161 = CARTESIAN_POINT ( 'NONE',  ( 35.23055949741119974, 1450.257496671300032, 136.2304356426660092 ) ) ;
#18162 = LINE ( 'NONE', #92667, #46736 ) ;
#18163 = CARTESIAN_POINT ( 'NONE',  ( -109.6343409440000016, 1386.390526388930084, 297.1907160496590450 ) ) ;
#18164 = CARTESIAN_POINT ( 'NONE',  ( 11.13173720219280050, 1480.405744213160006, 211.3599368507180145 ) ) ;
#18165 = CARTESIAN_POINT ( 'NONE',  ( -0.5193063452810020575, 1507.010169186189842, 221.5509792533989923 ) ) ;
#18166 = DIRECTION ( 'NONE',  ( 1.755985294532464991E-16, -1.000000000000000000, 1.338183447452830017E-16 ) ) ;
#18167 = ORIENTED_EDGE ( 'NONE', *, *, #481, .T. ) ;
#18168 = CARTESIAN_POINT ( 'NONE',  ( 2.623518071850000410, 1448.928635941619859, 183.1137651247979932 ) ) ;
#18169 = CARTESIAN_POINT ( 'NONE',  ( 13.19906462199999986, 1434.900406958499843, 146.7591386227980195 ) ) ;
#18170 = CARTESIAN_POINT ( 'NONE',  ( 30.31052258194586102, 1523.604703353109699, 195.7506062427368079 ) ) ;
#18171 = CARTESIAN_POINT ( 'NONE',  ( 16.47530569442600168, 1492.985912492669968, 188.5532949614449763 ) ) ;
#18172 = CARTESIAN_POINT ( 'NONE',  ( -0.2907244602440000603, 1416.115749421129976, 233.5373085857980016 ) ) ;
#18173 = CARTESIAN_POINT ( 'NONE',  ( 12.60564844770000015, 1500.992646453189991, 210.8169608434889994 ) ) ;
#18174 = CARTESIAN_POINT ( 'NONE',  ( -28.13497786889999830, 1508.084884472430076, 209.9324264222260013 ) ) ;
#18175 = EDGE_CURVE ( 'NONE', #3936, #74194, #37778, .T. ) ;
#18176 = CARTESIAN_POINT ( 'NONE',  ( 7.956617570819999763, 1426.823372744059952, 211.7778627466090029 ) ) ;
#18177 = CARTESIAN_POINT ( 'NONE',  ( -16.85280213986460041, 1384.871734412140086, 219.8759916889669910 ) ) ;
#18178 = VECTOR ( 'NONE', #5231, 1000.000000000000000 ) ;
#18179 = CARTESIAN_POINT ( 'NONE',  ( -12.61894528015529282, 1419.411281935211719, 228.4589828776151705 ) ) ;
#18180 = CARTESIAN_POINT ( 'NONE',  ( -17.38235991649999690, 1414.983773854429955, 207.6803066081180020 ) ) ;
#18181 = CARTESIAN_POINT ( 'NONE',  ( -7.932780634030001110, 1482.621353729790144, 201.9116440055690020 ) ) ;
#18182 = CARTESIAN_POINT ( 'NONE',  ( 25.11052302270000069, 1436.446855038549984, 137.6568901633980317 ) ) ;
#18184 = ADVANCED_FACE ( 'NONE', ( #25690 ), #21149, .F. ) ;
#18183 = CARTESIAN_POINT ( 'NONE',  ( -8.417397172205490108, 1396.207002374369949, 201.9581881603329805 ) ) ;
#18185 = ORIENTED_EDGE ( 'NONE', *, *, #96543, .F. ) ;
#18186 = CARTESIAN_POINT ( 'NONE',  ( -17.27480999623900004, 1410.739465257400070, 225.9386244916770181 ) ) ;
#18187 = CARTESIAN_POINT ( 'NONE',  ( -16.71982381703620035, 1484.422990366600288, 222.3758235082320027 ) ) ;
#18188 = ORIENTED_EDGE ( 'NONE', *, *, #110319, .F. ) ;
#18189 = EDGE_LOOP ( 'NONE', ( #24377, #39892 ) ) ;
#18190 = CARTESIAN_POINT ( 'NONE',  ( -2.602924848259999813, 1495.483236843290115, 217.1248042506690297 ) ) ;
#18191 = CARTESIAN_POINT ( 'NONE',  ( 7.179997236714190656, 1516.543639203995554, 206.9492468735227533 ) ) ;
#18193 = CARTESIAN_POINT ( 'NONE',  ( -9.968644151297580080, 1439.097532313579904, 209.3205140116839971 ) ) ;
#18192 = CARTESIAN_POINT ( 'NONE',  ( 10.89837308280000094, 1426.095306331829761, 91.92372727469789595 ) ) ;
#18194 = CARTESIAN_POINT ( 'NONE',  ( 4.152837535936280133, 1424.659374145959873, 185.0051014476340185 ) ) ;
#18195 = CARTESIAN_POINT ( 'NONE',  ( -2.870322881153364758, 1419.668002344334354, 186.1847472751339012 ) ) ;
#18196 = CARTESIAN_POINT ( 'NONE',  ( 7.505459564510000625, 1425.357945906760051, 212.2350828798089992 ) ) ;
#18197 = CARTESIAN_POINT ( 'NONE',  ( 5.076283890730000081, 1469.790178736790040, 187.8425608535989966 ) ) ;
#18198 = CARTESIAN_POINT ( 'NONE',  ( 8.309206006240000164, 1507.619018865230146, 183.0708158541980026 ) ) ;
#18199 = CARTESIAN_POINT ( 'NONE',  ( -113.4000000000000057, 1378.967725634990074, 306.1169302589129870 ) ) ;
#18200 = CARTESIAN_POINT ( 'NONE',  ( 8.778479041704853714, 1365.138727624712828, 210.6218459617142003 ) ) ;
#18202 = ORIENTED_EDGE ( 'NONE', *, *, #78172, .T. ) ;
#18201 = CARTESIAN_POINT ( 'NONE',  ( -11.21032122992201785, 1519.551704408389924, 229.8720270527158220 ) ) ;
#18203 = ORIENTED_EDGE ( 'NONE', *, *, #58995, .T. ) ;
#18204 = CARTESIAN_POINT ( 'NONE',  ( -40.27288003839999675, 1443.726530270089825, 137.1298452635979856 ) ) ;
#18205 = CARTESIAN_POINT ( 'NONE',  ( -21.63026377219999929, 1508.312050283890130, 209.5914177110290098 ) ) ;
#18206 = CARTESIAN_POINT ( 'NONE',  ( -2.920683203049999872E-09, 1474.175172929029941, 270.1377426661979939 ) ) ;
#18207 = CARTESIAN_POINT ( 'NONE',  ( 7.544486580690446864, 1500.279846028723568, 200.5799775095794075 ) ) ;
#18208 = CARTESIAN_POINT ( 'NONE',  ( -1.319906717929999918, 1486.022175928729894, 181.9654110648980065 ) ) ;
#18209 = DIRECTION ( 'NONE',  ( 5.980589973904019347E-17, -1.000000000000000000, 1.736889445713099699E-16 ) ) ;
#18210 = CARTESIAN_POINT ( 'NONE',  ( 1.195572441903639982, 1476.044226966599808, 197.7073300112460004 ) ) ;
#18211 = CARTESIAN_POINT ( 'NONE',  ( 22.33897491209999941, 1410.187224165629914, 206.2328829822479861 ) ) ;
#18212 = CARTESIAN_POINT ( 'NONE',  ( -2.500000000000000000, 1448.769782533650186, 157.0284636696169969 ) ) ;
#18213 = CARTESIAN_POINT ( 'NONE',  ( 6.697942107255492772, 1369.372287355299250, 207.6218459616987673 ) ) ;
#18214 = CARTESIAN_POINT ( 'NONE',  ( 14.75735370008069935, 1409.369483614819956, 204.1261042358389943 ) ) ;
#18215 = CARTESIAN_POINT ( 'NONE',  ( -8.399159049882628736, 1406.308215514319727, 267.5079637899610248 ) ) ;
#18216 = CARTESIAN_POINT ( 'NONE',  ( -13.76076751202730009, 1434.979366489430049, 148.7044419327400249 ) ) ;
#18217 = ORIENTED_EDGE ( 'NONE', *, *, #106899, .F. ) ;
#18218 = CARTESIAN_POINT ( 'NONE',  ( 3.566815704669999754, 1424.381564880729911, 184.5429952954980024 ) ) ;
#18219 = CARTESIAN_POINT ( 'NONE',  ( 13.14468279130000106, 1445.308786585929965, 188.3807251759980090 ) ) ;
#18220 = EDGE_LOOP ( 'NONE', ( #110606, #22465, #89670, #101064, #67710 ) ) ;
#18221 = ORIENTED_EDGE ( 'NONE', *, *, #9979, .T. ) ;
#18222 = CIRCLE ( 'NONE', #7282, 1.000000000000000888 ) ;
#18223 = FACE_OUTER_BOUND ( 'NONE', #80654, .T. ) ;
#18224 = CARTESIAN_POINT ( 'NONE',  ( 9.813910351400000565, 1364.017814053650000, 207.6218459616989946 ) ) ;
#18225 = CARTESIAN_POINT ( 'NONE',  ( -7.711550716115000093, 1516.630499592039996, 213.1573366827869904 ) ) ;
#18226 = CARTESIAN_POINT ( 'NONE',  ( 2.475398936714999998, 1511.813148765560072, 216.7072503566170099 ) ) ;
#18227 = B_SPLINE_CURVE_WITH_KNOTS ( 'NONE', 3,
 ( #90990, #108355, #33286, #7546 ),
 .UNSPECIFIED., .F., .F.,
 ( 4, 4 ),
 ( 0.000000000000000000, 1.000000000000000000 ),
 .UNSPECIFIED. ) ;
#18228 = ORIENTED_EDGE ( 'NONE', *, *, #105425, .F. ) ;
#18229 = CARTESIAN_POINT ( 'NONE',  ( 2.500000000000000000, 1426.966631815929986, 170.4008037693979816 ) ) ;
#18230 = CARTESIAN_POINT ( 'NONE',  ( -105.9862693054190004, 1378.913060387289988, 302.9553208434759881 ) ) ;
#18231 = CARTESIAN_POINT ( 'NONE',  ( 0.7369041709050019318, 1517.080322339569875, 204.1102945640870132 ) ) ;
#18232 = AXIS2_PLACEMENT_3D ( 'NONE', #689, #76832, #95287 ) ;
#18233 = CARTESIAN_POINT ( 'NONE',  ( -28.70528459879999872, 1509.871474410030032, 205.0464017625179736 ) ) ;
#18234 = CARTESIAN_POINT ( 'NONE',  ( -1.330926000679999888, 1457.942373938230048, 229.8940546109979834 ) ) ;
#18235 = CARTESIAN_POINT ( 'NONE',  ( -85.86390051840001547, 1385.060281227220003, 289.6783794304589605 ) ) ;
#18236 = CARTESIAN_POINT ( 'NONE',  ( -62.23286792741850348, 1384.686997364249919, 248.8895857189220067 ) ) ;
#18237 = DIRECTION ( 'NONE',  ( -6.123233995736769734E-17, -1.000000000000000000, -1.124819836996399911E-32 ) ) ;
#18238 = CARTESIAN_POINT ( 'NONE',  ( -12.66869256729999904, 1410.724518653430096, 227.9982876970979930 ) ) ;
#18240 = ORIENTED_EDGE ( 'NONE', *, *, #3551, .F. ) ;
#18239 = CARTESIAN_POINT ( 'NONE',  ( -12.03594993039999927, 1445.662098499869899, 187.0019535905980206 ) ) ;
#18241 = CARTESIAN_POINT ( 'NONE',  ( -26.57998359160610136, 1469.327412759369736, 208.7761463849559789 ) ) ;
#18242 = CARTESIAN_POINT ( 'NONE',  ( 28.02912970369999712, 1508.133041384130138, 210.7019033844679825 ) ) ;
#18243 = CARTESIAN_POINT ( 'NONE',  ( -8.228435909236443635, 1441.487949711303372, 203.2737885189420410 ) ) ;
#18244 = CARTESIAN_POINT ( 'NONE',  ( -25.70525537839999686, 1436.337899435129884, 137.0032570942979930 ) ) ;
#18245 = CARTESIAN_POINT ( 'NONE',  ( 5.787476994515000861, 1517.070197312179971, 211.9915394291670054 ) ) ;
#18246 = VECTOR ( 'NONE', #2620, 1000.000000000000000 ) ;
#18247 = CARTESIAN_POINT ( 'NONE',  ( -68.43569653030000666, 1379.748342192099926, 279.4446506693590209 ) ) ;
#18248 = CARTESIAN_POINT ( 'NONE',  ( -14.16989796110000022, 1420.440730658529901, 227.4201728071980142 ) ) ;
#18249 = CARTESIAN_POINT ( 'NONE',  ( -30.00400320040627378, 1524.843178112495707, 222.2744577634231007 ) ) ;
#18250 = CARTESIAN_POINT ( 'NONE',  ( -11.60004869885203682, 1422.941213646836331, 135.6422426701566053 ) ) ;
#18251 = CARTESIAN_POINT ( 'NONE',  ( -1.135898823814999847, 1516.958737650239982, 208.0022537503870126 ) ) ;
#18252 = VERTEX_POINT ( 'NONE', #64860 ) ;
#18253 = CARTESIAN_POINT ( 'NONE',  ( 2.500000000000000000, 1432.575364831350271, 157.5016493498980026 ) ) ;
#18254 = CARTESIAN_POINT ( 'NONE',  ( -3.088334884859999629, 1412.839240486330027, 232.6088388287980138 ) ) ;
#18255 = CARTESIAN_POINT ( 'NONE',  ( -22.68102785909999852, 1384.991329335610089, 222.0421655005590367 ) ) ;
#18256 = VERTEX_POINT ( 'NONE', #39632 ) ;
#18258 = B_SPLINE_CURVE_WITH_KNOTS ( 'NONE', 3,
 ( #28874, #37276, #64705, #22083, #90410, #71470, #13690, #47875, #105590, #46252 ),
 .UNSPECIFIED., .F., .F.,
 ( 4, 2, 2, 2, 4 ),
 ( 1.301042606982605321E-18, 0.0007406479101618186189, 0.001481295820323635937, 0.002221943730485453471, 0.002962591640647270572 ),
 .UNSPECIFIED. ) ;
#18257 = CARTESIAN_POINT ( 'NONE',  ( -17.87379895800760110, 1385.284389312859957, 220.1513191895170394 ) ) ;
#18259 = DIRECTION ( 'NONE',  ( -3.659266894335750173E-33, -6.123233995736769734E-17, -1.000000000000000000 ) ) ;
#18260 = CARTESIAN_POINT ( 'NONE',  ( 12.44825556113039866, 1434.827193400389888, 150.5385283147030009 ) ) ;
#18261 = EDGE_CURVE ( 'NONE', #82777, #75258, #47782, .T. ) ;
#18262 = CARTESIAN_POINT ( 'NONE',  ( 15.04655486393220087, 1478.705643649750073, 230.8080699388220012 ) ) ;
#18263 = CARTESIAN_POINT ( 'NONE',  ( -23.54197198179479855, 1507.885248531370053, 223.3642489706239758 ) ) ;
#18264 = CYLINDRICAL_SURFACE ( 'NONE', #102975, 8.000000000000000000 ) ;
#18265 = B_SPLINE_CURVE_WITH_KNOTS ( 'NONE', 3,
 ( #4894, #13276, #81589, #71042, #96771, #72143, #28455, #104608, #54774, #20575, #105728, #4366, #21674, #87829, #79961, #55326, #20040, #62649, #53688, #88362, #3834, #2728, #11651, #54236, #106260, #98402, #70489, #105164, #88906, #80517, #19485, #36850, #62084, #12192, #27901, #29013, #37962, #45828, #47468, #63197, #46385, #29547, #63733, #89458, #96210, #11118, #71607, #46933, #38494, #3278, #55880, #97843, #79416, #37408, #21121, #12751, #81051, #72672, #106797, #30087, #90001, #64281, #45278, #73213, #56975, #5450, #23343, #107905, #39610, #57534, #83808, #49676, #109571, #32842, #98947, #108464 ),
 .UNSPECIFIED., .F., .F.,
 ( 4, 2, 2, 2, 1, 1, 1, 1, 2, 2, 2, 1, 1, 2, 2, 2, 2, 2, 2, 1, 1, 1, 1, 1, 1, 2, 2, 2, 2, 2, 1, 1, 1, 1, 1, 2, 2, 2, 2, 2, 1, 2, 2, 2, 2, 2, 4 ),
 ( 0.000000000000000000, 0.007812499999216796637, 0.01171874999882519669, 0.01367187499863343862, 0.01464843749853756219, 0.01513671874849285663, 0.01538085937346737354, 0.01550292968595155113, 0.01556396484219058768, 0.01562499999842962423, 0.02343749999855148508, 0.02734374999860635438, 0.02929687499863947026, 0.03027343749865050657, 0.03124999999866154288, 0.04687499999895392011, 0.05468749999910008097, 0.06249999999924624183, 0.09374999999981868670, 0.1093750000000989486, 0.1171875000002390588, 0.1210937500003148592, 0.1230468750003584633, 0.1240234375003802514, 0.1245117187503911454, 0.1247558593753966549, 0.1250000000004021505, 0.1875000000015698276, 0.2187500000021481705, 0.2343750000024373004, 0.2421875000025818792, 0.2460937500026541547, 0.2480468750026902647, 0.2490234375027044478, 0.2495117187527077784, 0.2497558593777093605, 0.2500000000027109426, 0.3750000000022902791, 0.4375000000020838886, 0.4687500000019808599, 0.4843750000019327873, 0.4921875000019087509, 0.5000000000018847146, 0.6250000000014135360, 0.7500000000009424683, 0.8750000000004711787, 1.000000000000000000 ),
 .UNSPECIFIED. ) ;
#18266 = CARTESIAN_POINT ( 'NONE',  ( -0.4960403072899999821, 1409.436440935729934, 232.9663690048980129 ) ) ;
#18267 = DIRECTION ( 'NONE',  ( -0.000000000000000000, -1.000000000000000000, -0.000000000000000000 ) ) ;
#18269 = CARTESIAN_POINT ( 'NONE',  ( -4.270561097189999877, 1421.938260751330063, 185.0877191730979803 ) ) ;
#18268 = CARTESIAN_POINT ( 'NONE',  ( -5.001338666445000136, 1516.911981270829983, 214.9058546054269812 ) ) ;
#18270 = CARTESIAN_POINT ( 'NONE',  ( 20.07277491569999839, 1508.598349460030022, 188.9934802953980011 ) ) ;
#18271 = CARTESIAN_POINT ( 'NONE',  ( -3.454172653555000139, 1517.122088787240045, 216.8462693643270143 ) ) ;
#18272 = ORIENTED_EDGE ( 'NONE', *, *, #14255, .T. ) ;
#18273 = CARTESIAN_POINT ( 'NONE',  ( -12.57878310069559902, 1415.943166310999914, 196.1339907655800232 ) ) ;
#18274 = CARTESIAN_POINT ( 'NONE',  ( -6.328709615500000218, 1508.913060324029857, 180.8323534384980178 ) ) ;
#18275 = VERTEX_POINT ( 'NONE', #20594 ) ;
#18276 = CARTESIAN_POINT ( 'NONE',  ( 3.238878936319999902, 1420.340958668729854, 185.3443125121980017 ) ) ;
#18277 = EDGE_CURVE ( 'NONE', #64966, #93939, #42408, .T. ) ;
#18278 = CARTESIAN_POINT ( 'NONE',  ( -21.59687142900000012, 1507.523380033690046, 209.4572543540780032 ) ) ;
#18279 = DIRECTION ( 'NONE',  ( 0.000000000000000000, 0.000000000000000000, -1.000000000000000000 ) ) ;
#18280 = CARTESIAN_POINT ( 'NONE',  ( 2.991069600740460466, 1424.175520158889867, 191.4083219421100353 ) ) ;
#18281 = CARTESIAN_POINT ( 'NONE',  ( -29.74902317390499107, 1525.343710797494850, 196.2390521661037894 ) ) ;
#18282 = CARTESIAN_POINT ( 'NONE',  ( -3.035119290295845929, 1377.913060387289988, 210.7799391869605188 ) ) ;
#18283 = CARTESIAN_POINT ( 'NONE',  ( -3.138402261229999990, 1447.047508080440139, 157.7990927532979981 ) ) ;
#18284 = CARTESIAN_POINT ( 'NONE',  ( -18.54535832700000242, 1425.392845097829877, 225.7569259269980080 ) ) ;
#18285 = CARTESIAN_POINT ( 'NONE',  ( -7.344230725084723410, 1458.212826010420713, 215.2418586630906532 ) ) ;
#18286 = EDGE_CURVE ( 'NONE', #30631, #92476, #47100, .T. ) ;
#18287 = FACE_OUTER_BOUND ( 'NONE', #106865, .T. ) ;
#18288 = CARTESIAN_POINT ( 'NONE',  ( 18.16298593710000020, 1438.550562606130143, 191.5625238810979738 ) ) ;
#18290 = CARTESIAN_POINT ( 'NONE',  ( 0.5678390018416790141, 1428.477637517579979, 189.9617647321709910 ) ) ;
#18289 = CARTESIAN_POINT ( 'NONE',  ( -10.92886345369909940, 1418.002833451510014, 197.9448744300869976 ) ) ;
#18291 = CARTESIAN_POINT ( 'NONE',  ( 0.6235920161070115375, 1525.878013734321257, 242.9475333194528446 ) ) ;
#18292 = ORIENTED_EDGE ( 'NONE', *, *, #89334, .T. ) ;
#18293 = CARTESIAN_POINT ( 'NONE',  ( 1.514738106409309948, 1507.606285602550088, 186.2052147526660235 ) ) ;
#18294 = LINE ( 'NONE', #8792, #3281 ) ;
#18295 = CARTESIAN_POINT ( 'NONE',  ( -24.42829869279999855, 1436.527038349410077, 210.7116707911179958 ) ) ;
#18296 = CARTESIAN_POINT ( 'NONE',  ( 7.511829633256015271, 1410.548442039797692, 187.3987484226458946 ) ) ;
#18297 = CARTESIAN_POINT ( 'NONE',  ( 11.83466398084630811, 1519.551704408389924, 190.1848878784103363 ) ) ;
#18298 = DIRECTION ( 'NONE',  ( -1.836970198721029688E-16, -1.000000000000000000, 0.000000000000000000 ) ) ;
#18299 = FACE_OUTER_BOUND ( 'NONE', #67158, .T. ) ;
#18300 = FACE_OUTER_BOUND ( 'NONE', #98414, .T. ) ;
#18301 = CARTESIAN_POINT ( 'NONE',  ( 13.08238251380000072, 1414.913528139129994, 198.0397827309980130 ) ) ;
#18302 = CARTESIAN_POINT ( 'NONE',  ( -95.87000543284069920, 1383.766626252310061, 310.0354134814519966 ) ) ;
#18303 = CARTESIAN_POINT ( 'NONE',  ( 3.588016447739999837, 1452.642150377629832, 153.4169808353979931 ) ) ;
#18305 = CARTESIAN_POINT ( 'NONE',  ( -5.149250441021638203, 1391.888183122331156, 214.5740113081126310 ) ) ;
#18304 =( BOUNDED_CURVE ( )  B_SPLINE_CURVE ( 3, ( #47177, #87535, #70216, #88091 ),
 .UNSPECIFIED., .F., .F. ) 
 B_SPLINE_CURVE_WITH_KNOTS ( ( 4, 4 ),
 ( 4.427184739196824204, 4.808362416880929580 ),
 .UNSPECIFIED. ) 
 CURVE ( )  GEOMETRIC_REPRESENTATION_ITEM ( )  RATIONAL_B_SPLINE_CURVE ( ( 1.000000000000000000, 0.9879285716166186226, 0.9879285716166186226, 1.000000000000000000 ) ) 
 REPRESENTATION_ITEM ( '' )  );
#18307 = EDGE_CURVE ( 'NONE', #43746, #101156, #81772, .T. ) ;
#18306 = CYLINDRICAL_SURFACE ( 'NONE', #83316, 1.999999999999999556 ) ;
#18309 = ORIENTED_EDGE ( 'NONE', *, *, #78222, .T. ) ;
#18308 = CARTESIAN_POINT ( 'NONE',  ( 23.34540950859999953, 1507.878524956530100, 194.4697486434980078 ) ) ;
#18310 = CARTESIAN_POINT ( 'NONE',  ( -1.414439329499999953, 1414.913528139129994, 226.2086894112979962 ) ) ;
#18311 = CARTESIAN_POINT ( 'NONE',  ( -81.27653993580000247, 1383.775959360260003, 304.8043613862590746 ) ) ;
#18312 = CARTESIAN_POINT ( 'NONE',  ( -14.87799178844600156, 1417.019184689190070, 213.1221934129589783 ) ) ;
#18313 = ORIENTED_EDGE ( 'NONE', *, *, #21343, .T. ) ;
#18314 = ORIENTED_EDGE ( 'NONE', *, *, #15321, .F. ) ;
#18315 = CARTESIAN_POINT ( 'NONE',  ( 14.41410989250000085, 1444.046959656890067, 189.7051000925980020 ) ) ;
#18316 = CARTESIAN_POINT ( 'NONE',  ( -0.3821804589910179906, 1506.433683733660018, 187.1424611576989889 ) ) ;
#18317 = DIRECTION ( 'NONE',  ( -1.000000000000000000, 0.000000000000000000, 0.000000000000000000 ) ) ;
#18319 = CARTESIAN_POINT ( 'NONE',  ( -6.248994634959999850, 1472.348783256330080, 259.9484462021979994 ) ) ;
#18318 = CARTESIAN_POINT ( 'NONE',  ( 15.04404422727308344, 1412.425273560396590, 269.3648504014765876 ) ) ;
#18320 = CARTESIAN_POINT ( 'NONE',  ( 9.825411767019899045, 1435.537689025190048, 209.1855920904920083 ) ) ;
#18321 = CARTESIAN_POINT ( 'NONE',  ( -109.8221033779999942, 1384.392514930950028, 297.0589093852589713 ) ) ;
#18322 = CARTESIAN_POINT ( 'NONE',  ( -12.19020004887032727, 1435.566796327880638, 151.0976163169758877 ) ) ;
#18323 = CARTESIAN_POINT ( 'NONE',  ( -19.80101799410000041, 1484.918799879129892, 190.6212978484980169 ) ) ;
#18324 = CARTESIAN_POINT ( 'NONE',  ( 1.122881213689999935, 1410.331791442129997, 185.2157289252980092 ) ) ;
#18325 = CARTESIAN_POINT ( 'NONE',  ( 4.770564261300000553, 1422.188385567129899, 184.2239224491979996 ) ) ;
#18326 = CARTESIAN_POINT ( 'NONE',  ( -10.13504282470000106, 1439.368087670590057, 152.9209922797979857 ) ) ;
#18327 = CARTESIAN_POINT ( 'NONE',  ( -9.190602985553210758, 1449.883023889459992, 209.4828535419830189 ) ) ;
#18328 = CARTESIAN_POINT ( 'NONE',  ( -12.46654139771550085, 1422.643769205189983, 203.9843212440389948 ) ) ;
#18329 = CARTESIAN_POINT ( 'NONE',  ( -3.141354938490000137, 1451.554175194630261, 154.1120778672979839 ) ) ;
#18330 = DIRECTION ( 'NONE',  ( 0.9786619618251657382, 0.000000000000000000, 0.2054769195713180563 ) ) ;
#18331 = ORIENTED_EDGE ( 'NONE', *, *, #26356, .T. ) ;
#18332 = CARTESIAN_POINT ( 'NONE',  ( -15.72751745975079984, 1517.151704408390060, 211.3620530696679793 ) ) ;
#18333 = CARTESIAN_POINT ( 'NONE',  ( 4.667614565920000125, 1472.762121965489769, 187.6119789488990079 ) ) ;
#18334 = CARTESIAN_POINT ( 'NONE',  ( -43.48864995209999762, 1440.913074447990084, 270.3367068800979496 ) ) ;
#18335 = CARTESIAN_POINT ( 'NONE',  ( 2.566893074593609807E-08, 1406.911841303630126, 196.1218459607310081 ) ) ;
#18336 = CARTESIAN_POINT ( 'NONE',  ( 17.98939575750000230, 1410.465183456229852, 222.9682893216979949 ) ) ;
#18337 = CARTESIAN_POINT ( 'NONE',  ( -14.38570825430000077, 1474.169743061429926, 223.8345247943979928 ) ) ;
#18338 = CARTESIAN_POINT ( 'NONE',  ( 0.9766393796380001824, 1453.313060387329870, 188.4686263754979905 ) ) ;
#18339 = CARTESIAN_POINT ( 'NONE',  ( 2.915910696398010149, 1409.692218141939975, 231.4126881937029907 ) ) ;
#18340 = CARTESIAN_POINT ( 'NONE',  ( -1.936437027941079858, 1420.638707705209754, 193.8409875628919963 ) ) ;
#18341 = CARTESIAN_POINT ( 'NONE',  ( -2.995672382979999604, 1416.748940793229849, 233.0563413717979984 ) ) ;
#18342 = CARTESIAN_POINT ( 'NONE',  ( -8.380780172617267709, 1511.478807872990046, 214.6783014743539866 ) ) ;
#18343 = CARTESIAN_POINT ( 'NONE',  ( 0.06326327880447388252, 1358.388637432561609, 209.6218459617033432 ) ) ;
#18344 = CARTESIAN_POINT ( 'NONE',  ( -45.63195895436749794, 1439.443261914909954, 266.1896113851490213 ) ) ;
#18345 = CARTESIAN_POINT ( 'NONE',  ( -3.087032477589999768, 1436.949765671180103, 185.2347600039979909 ) ) ;
#18346 = ORIENTED_EDGE ( 'NONE', *, *, #57013, .F. ) ;
#18347 = CARTESIAN_POINT ( 'NONE',  ( -9.199049879260000395, 1422.949100153850168, 210.5804414222690184 ) ) ;
#18348 = EDGE_LOOP ( 'NONE', ( #19030, #27842, #34218, #70335 ) ) ;
#18349 = CARTESIAN_POINT ( 'NONE',  ( 2.299667965875000331, 1516.965971551240045, 210.2399506998270056 ) ) ;
#18350 = PLANE ( 'NONE',  #16193 ) ;
#18351 = CARTESIAN_POINT ( 'NONE',  ( 1.191524307911311586, 1526.382868172863937, 179.0083900503167911 ) ) ;
#18352 = CARTESIAN_POINT ( 'NONE',  ( 7.526870069911640648, 1425.474419429210002, 212.1962186843350082 ) ) ;
#18353 = CARTESIAN_POINT ( 'NONE',  ( 0.1490614901714290008, 1496.163810114490161, 221.4655199671470029 ) ) ;
#18354 = VERTEX_POINT ( 'NONE', #76530 ) ;
#18355 = CARTESIAN_POINT ( 'NONE',  ( 7.313756596019999279, 1422.662435718929828, 212.8858276506779816 ) ) ;
#18357 = CARTESIAN_POINT ( 'NONE',  ( -15.30900801332620098, 1512.850289816019767, 222.8271770998339889 ) ) ;
#18356 = CARTESIAN_POINT ( 'NONE',  ( -10.93631254607359971, 1492.700895685820115, 207.3057419371699837 ) ) ;
#18358 = CARTESIAN_POINT ( 'NONE',  ( 11.60004869885203682, 1422.586145265931236, 135.5999999980982125 ) ) ;
#18359 = CARTESIAN_POINT ( 'NONE',  ( -11.59119438181595818, 1426.213969660457678, 138.6120005729653144 ) ) ;
#18360 = CARTESIAN_POINT ( 'NONE',  ( 3.696672296620000076, 1460.253338437389857, 228.3281616586990026 ) ) ;
#18361 = CARTESIAN_POINT ( 'NONE',  ( -8.666962939886769135, 1439.175798852059870, 207.1921834104900029 ) ) ;
#18362 = VERTEX_POINT ( 'NONE', #83280 ) ;
#18363 = CARTESIAN_POINT ( 'NONE',  ( -4.332897253567730367, 1408.387299629059953, 270.3897631605610172 ) ) ;
#18364 = CARTESIAN_POINT ( 'NONE',  ( -3.460866208815000178, 1517.020847257979995, 208.3861469975149987 ) ) ;
#18365 = CARTESIAN_POINT ( 'NONE',  ( 10.63881130030000044, 1418.746488869330051, 230.0613383181980112 ) ) ;
#18366 = CARTESIAN_POINT ( 'NONE',  ( -17.60627563539920004, 1410.895669414250051, 194.0661810348550205 ) ) ;
#18368 = VERTEX_POINT ( 'NONE', #101711 ) ;
#18367 = CARTESIAN_POINT ( 'NONE',  ( -5.690168351895294130, 1366.535003315410449, 209.6218459617148824 ) ) ;
#18369 = VERTEX_POINT ( 'NONE', #84917 ) ;
#18370 = CARTESIAN_POINT ( 'NONE',  ( -22.59787312113130042, 1409.702172917540111, 209.4225048435710050 ) ) ;
#18371 = CARTESIAN_POINT ( 'NONE',  ( -4.216177480479998962, 1424.161827809529996, 185.4694233363979947 ) ) ;
#18372 = CARTESIAN_POINT ( 'NONE',  ( 3.683511325231741740, 1425.182533976880450, 185.0553125120289906 ) ) ;
#18373 = CARTESIAN_POINT ( 'NONE',  ( -0.005607894164331979868, 1408.917889387629884, 186.3448695751470154 ) ) ;
#18374 = CARTESIAN_POINT ( 'NONE',  ( -20.53032749330389706, 1436.446110082554924, 144.8592029257055458 ) ) ;
#18375 = CARTESIAN_POINT ( 'NONE',  ( -18.51512065000000007, 1415.857213627029978, 224.3066119029979859 ) ) ;
#18376 = CARTESIAN_POINT ( 'NONE',  ( 36.87367878740020188, 1461.868311835329905, 266.6849271820060494 ) ) ;
#18377 = CARTESIAN_POINT ( 'NONE',  ( -8.890585777435378034, 1465.118968690018619, 232.8711024472996201 ) ) ;
#18378 = CARTESIAN_POINT ( 'NONE',  ( -16.84468799194050703, 1421.803329214568066, 226.8795727158544366 ) ) ;
#18379 = CARTESIAN_POINT ( 'NONE',  ( -2.298369507954999946, 1516.779243033999819, 205.8702346062869992 ) ) ;
#18380 = ORIENTED_EDGE ( 'NONE', *, *, #26320, .F. ) ;
#18381 = CARTESIAN_POINT ( 'NONE',  ( 23.82822416500561502, 1411.105482365838270, 210.7039567702046554 ) ) ;
#18382 = CARTESIAN_POINT ( 'NONE',  ( 1.475113315915349999, 1481.918977469239962, 182.2120507298820087 ) ) ;
#18383 = CARTESIAN_POINT ( 'NONE',  ( 23.86654294979999946, 1410.978130439630149, 208.1633478644210129 ) ) ;
#18384 = VERTEX_POINT ( 'NONE', #6023 ) ;
#18385 = CARTESIAN_POINT ( 'NONE',  ( 2.487923763832299962, 1508.731372606449895, 204.5668970731580032 ) ) ;
#18386 = CARTESIAN_POINT ( 'NONE',  ( 25.88275927131619980, 1451.560184493740053, 136.3203580496130201 ) ) ;
#18387 = CARTESIAN_POINT ( 'NONE',  ( 15.94345596297699963, 1409.469818137940138, 225.2684692625209948 ) ) ;
#18388 = CARTESIAN_POINT ( 'NONE',  ( 12.44780704128189974, 1501.268281525590055, 211.7240718234590133 ) ) ;
#18389 = DIRECTION ( 'NONE',  ( 0.000000000000000000, -1.000000000000000000, 0.000000000000000000 ) ) ;
#18390 = CARTESIAN_POINT ( 'NONE',  ( 16.34466203799999917, 1409.483828562729968, 193.4811910679979974 ) ) ;
#18391 = CARTESIAN_POINT ( 'NONE',  ( 20.77846844200000120, 1444.740067931809790, 176.2781434906979996 ) ) ;
#18392 = CARTESIAN_POINT ( 'NONE',  ( 2.713487254142998850, 1439.656254381911822, 183.6712819054291970 ) ) ;
#18394 = CARTESIAN_POINT ( 'NONE',  ( -14.01707770341873527, 1379.589456901253470, 211.9120362016159049 ) ) ;
#18393 = CARTESIAN_POINT ( 'NONE',  ( -2.714091174029999877E-10, 1417.262443616730025, 235.9145977375980010 ) ) ;
#18395 = CARTESIAN_POINT ( 'NONE',  ( 4.165142600520000293, 1409.058510372029787, 229.9895894434979766 ) ) ;
#18396 = DIRECTION ( 'NONE',  ( 0.000000000000000000, 1.000000000000000000, -6.123233995736769734E-17 ) ) ;
#18397 = CARTESIAN_POINT ( 'NONE',  ( -10.49767883750000053, 1382.256743515189783, 217.7001910593189677 ) ) ;
#18398 = CARTESIAN_POINT ( 'NONE',  ( -1.121383629864999953, 1517.104192383289956, 213.7476359466970166 ) ) ;
#18399 = CARTESIAN_POINT ( 'NONE',  ( 3.097576048983416541, 1369.855992675987409, 207.7442862697458565 ) ) ;
#18400 = EDGE_LOOP ( 'NONE', ( #43331, #38803, #34623, #69213 ) ) ;
#18401 = DIRECTION ( 'NONE',  ( -0.9510565162951518658, 0.000000000000000000, 0.3090169943749526138 ) ) ;
#18402 = CARTESIAN_POINT ( 'NONE',  ( -1.033263135950000189, 1463.032196151989865, 228.8909791214989866 ) ) ;
#18403 = CARTESIAN_POINT ( 'NONE',  ( -0.3209257366447499926, 1408.978166690620128, 232.1464160328119988 ) ) ;
#18404 = CARTESIAN_POINT ( 'NONE',  ( 4.590060377064090424, 1517.051704403100075, 201.3992656192910147 ) ) ;
#18405 = CARTESIAN_POINT ( 'NONE',  ( -0.3700193229654308857, 1420.964624414496029, 193.7214914399045256 ) ) ;
#18406 = CARTESIAN_POINT ( 'NONE',  ( -4.329177920710369776, 1515.075136430330076, 207.6418469693050213 ) ) ;
#18407 = CARTESIAN_POINT ( 'NONE',  ( -24.08292308869999943, 1450.076351704500212, 243.9198229383979992 ) ) ;
#18408 = CARTESIAN_POINT ( 'NONE',  ( -28.27139721233055170, 1526.382868172863937, 198.6830693683576214 ) ) ;
#18409 = CARTESIAN_POINT ( 'NONE',  ( 11.90133581370000115, 1433.308793707279847, 149.9471025605980117 ) ) ;
#18410 = CARTESIAN_POINT ( 'NONE',  ( 9.145222436810001909, 1453.522154064530014, 214.3676144197979738 ) ) ;
#18411 = CARTESIAN_POINT ( 'NONE',  ( 25.26688801316450039, 1440.913060399130018, 217.7010804864050044 ) ) ;
#18412 = CARTESIAN_POINT ( 'NONE',  ( 20.19719966420300139, 1431.660555912299969, 215.0136818726180081 ) ) ;
#18413 = CARTESIAN_POINT ( 'NONE',  ( 10.88623464157270071, 1425.216911896579859, 199.6949144308769917 ) ) ;
#18414 = CARTESIAN_POINT ( 'NONE',  ( 10.62765097360019872, 1462.208136432790070, 211.9187849626219702 ) ) ;
#18415 = CARTESIAN_POINT ( 'NONE',  ( -9.574504100549999563, 1485.990341757929855, 183.6379974207980013 ) ) ;
#18416 = DIRECTION ( 'NONE',  ( 0.000000000000000000, 1.000000000000000000, 0.000000000000000000 ) ) ;
#18417 = CARTESIAN_POINT ( 'NONE',  ( 0.04628635179088989859, 1508.911441867209987, 238.5489216072199952 ) ) ;
#18418 = CARTESIAN_POINT ( 'NONE',  ( 25.41997721730000137, 1449.801887500550038, 211.0416158964779925 ) ) ;
#18419 = CARTESIAN_POINT ( 'NONE',  ( -16.87913774836607672, 1420.004850516591659, 207.9502230898332016 ) ) ;
#18420 = CARTESIAN_POINT ( 'NONE',  ( 25.68555131787286783, 1436.646045936909786, 137.1303311310317952 ) ) ;
#18421 = CARTESIAN_POINT ( 'NONE',  ( -1.842963430059999963, 1515.219201257890063, 204.7964405181290033 ) ) ;
#18422 = CARTESIAN_POINT ( 'NONE',  ( 0.5708672412673110319, 1460.784242060219867, 230.4191149082050174 ) ) ;
#18423 = CARTESIAN_POINT ( 'NONE',  ( 5.009478067315000338, 1516.886345593249871, 213.7343532441369973 ) ) ;
#18424 = CARTESIAN_POINT ( 'NONE',  ( -9.200421138165051360, 1422.937291722789951, 210.7384568321920142 ) ) ;
#18425 = CARTESIAN_POINT ( 'NONE',  ( 0.1639172357618859655, 1483.921440558410040, 181.9259246723260048 ) ) ;
#18427 = ORIENTED_EDGE ( 'NONE', *, *, #55358, .T. ) ;
#18426 = CARTESIAN_POINT ( 'NONE',  ( 3.196982321300000152, 1441.723154499190059, 217.7614377107290125 ) ) ;
#18428 = CARTESIAN_POINT ( 'NONE',  ( -12.53380499169999851, 1445.052233488290085, 169.4755105685979970 ) ) ;
#18429 = CARTESIAN_POINT ( 'NONE',  ( -6.169242136949999455, 1378.878171907740125, 208.5195113185000082 ) ) ;
#18430 = CARTESIAN_POINT ( 'NONE',  ( -28.77730029287999969, 1509.917985857419808, 212.2396942430650029 ) ) ;
#18432 = ORIENTED_EDGE ( 'NONE', *, *, #8351, .F. ) ;
#18431 = CARTESIAN_POINT ( 'NONE',  ( -38.87405678782049989, 1449.786581495279961, 134.0999999981590065 ) ) ;
#18433 = CARTESIAN_POINT ( 'NONE',  ( -2.195050156180049949, 1508.551704408389924, 220.0605044532859722 ) ) ;
#18434 = ORIENTED_EDGE ( 'NONE', *, *, #98027, .T. ) ;
#18435 = CARTESIAN_POINT ( 'NONE',  ( 18.18137293399999876, 1507.546748832030062, 186.5307135875980009 ) ) ;
#18436 = CARTESIAN_POINT ( 'NONE',  ( -12.10181609356209975, 1392.233360485750154, 211.6594669569279858 ) ) ;
#18437 = CARTESIAN_POINT ( 'NONE',  ( -13.95470550870000004, 1415.426952351230057, 221.1148131923979747 ) ) ;
#18438 = EDGE_CURVE ( 'NONE', #73589, #43960, #60330, .T. ) ;
#18439 = CARTESIAN_POINT ( 'NONE',  ( 23.17538675820700789, 1409.994297229576887, 208.1793956993277845 ) ) ;
#18440 = CARTESIAN_POINT ( 'NONE',  ( -3.273236734419999738, 1432.101391978590073, 216.8815162293089713 ) ) ;
#18441 = B_SPLINE_CURVE_WITH_KNOTS ( 'NONE', 3,
 ( #54158, #3755, #19963, #98326, #12676, #38418 ),
 .UNSPECIFIED., .F., .F.,
 ( 4, 2, 4 ),
 ( -1.131363979615304141E-05, 0.001067788114096033690, 0.002146889867988220277 ),
 .UNSPECIFIED. ) ;
#18442 = CARTESIAN_POINT ( 'NONE',  ( 1.842963333050209318, 1515.193466656063265, 213.4479253432561450 ) ) ;
#18443 = CARTESIAN_POINT ( 'NONE',  ( 11.39880752746310044, 1409.311115508779949, 218.7955269592959837 ) ) ;
#18444 = CARTESIAN_POINT ( 'NONE',  ( 10.10004869885234058, 1422.222932908421171, 137.0999999980978430 ) ) ;
#18445 = CARTESIAN_POINT ( 'NONE',  ( -68.28143006493819200, 1385.103599963460056, 262.2692984668489657 ) ) ;
#18446 = CARTESIAN_POINT ( 'NONE',  ( -17.60602154420000076, 1410.887439192729971, 193.4352696968979899 ) ) ;
#18447 = CARTESIAN_POINT ( 'NONE',  ( -62.03809624990000060, 1379.749343316239901, 266.3689138319589915 ) ) ;
#18448 = ORIENTED_EDGE ( 'NONE', *, *, #55531, .T. ) ;
#18449 = CARTESIAN_POINT ( 'NONE',  ( 12.06590886230689996, 1491.397659232809929, 206.8029289098089691 ) ) ;
#18451 = ORIENTED_EDGE ( 'NONE', *, *, #74444, .T. ) ;
#18450 = CARTESIAN_POINT ( 'NONE',  ( 0.000000000000000000, 1412.913060387329779, 209.1218459616989946 ) ) ;
#18452 = CARTESIAN_POINT ( 'NONE',  ( -8.313145311751080513, 1507.316772571419961, 235.1568484389069909 ) ) ;
#18453 = EDGE_LOOP ( 'NONE', ( #24161, #73903, #53390, #13103 ) ) ;
#18454 = B_SPLINE_CURVE_WITH_KNOTS ( 'NONE', 5,
 ( #53177, #53754, #45339, #20101, #54293, #4425 ),
 .UNSPECIFIED., .F., .F.,
 ( 6, 6 ),
 ( 0.000000000000000000, 1.000000000000000000 ),
 .UNSPECIFIED. ) ;
#18455 = CARTESIAN_POINT ( 'NONE',  ( -14.35646903299999799, 1420.584115152450067, 213.7701001417389932 ) ) ;
#18456 = CARTESIAN_POINT ( 'NONE',  ( -9.178315062050000250, 1363.109187794150102, 207.6218459616989946 ) ) ;
#18457 = CARTESIAN_POINT ( 'NONE',  ( -6.072056330729999729, 1495.887419368989868, 199.6590240909889928 ) ) ;
#18458 = B_SPLINE_CURVE_WITH_KNOTS ( 'NONE', 3,
 ( #14839, #66388, #21575, #47359, #40604, #14287, #4259, #74774, #98851, #23786, #90997, #73113, #57975 ),
 .UNSPECIFIED., .F., .F.,
 ( 4, 2, 2, 1, 2, 2, 4 ),
 ( 0.000000000000000000, 0.2500000000000711098, 0.3750000000001102451, 0.4375000000001359468, 0.4687500000001467715, 0.5000000000001576517, 1.000000000000000000 ),
 .UNSPECIFIED. ) ;
#18459 = CARTESIAN_POINT ( 'NONE',  ( 30.19399729140642563, 1462.104126541301866, 269.4728972154693452 ) ) ;
#18460 = CARTESIAN_POINT ( 'NONE',  ( 11.76730872650090021, 1427.477307142819882, 208.8591088289190054 ) ) ;
#18461 = CARTESIAN_POINT ( 'NONE',  ( 17.99196544828748046, 1435.000034824831118, 215.3568569466342240 ) ) ;
#18462 = CARTESIAN_POINT ( 'NONE',  ( 1.534959661399999842, 1416.490978422929857, 232.7302165538980034 ) ) ;
#18463 = CARTESIAN_POINT ( 'NONE',  ( 3.442292827050000170, 1445.232941965290138, 200.8115267138090019 ) ) ;
#18464 = CARTESIAN_POINT ( 'NONE',  ( 0.000000000000000000, 1523.382868172864164, 209.1218459616979999 ) ) ;
#18465 = CARTESIAN_POINT ( 'NONE',  ( -9.765027863526395180, 1368.680785116012430, 208.3718459617010978 ) ) ;
#18466 = CARTESIAN_POINT ( 'NONE',  ( -13.24484260582790185, 1487.711350369650290, 193.0573247253030047 ) ) ;
#18467 = B_SPLINE_CURVE_WITH_KNOTS ( 'NONE', 3,
 ( #63748, #19504, #53138, #104624, #18943, #80537 ),
 .UNSPECIFIED., .F., .F.,
 ( 4, 2, 4 ),
 ( 0.000000000000000000, 0.5000000000000000000, 1.000000000000000000 ),
 .UNSPECIFIED. ) ;
#18468 = CARTESIAN_POINT ( 'NONE',  ( -16.17567356680000046, 1459.146941997929844, 230.7169173512979796 ) ) ;
#18469 = CARTESIAN_POINT ( 'NONE',  ( -1.136814071995000175, 1516.854133554269993, 206.8377924607469822 ) ) ;
#18470 = CARTESIAN_POINT ( 'NONE',  ( -2.225543501807631053, 1525.712835404586031, 176.6707008850455622 ) ) ;
#18471 = DIRECTION ( 'NONE',  ( 0.1041548977914050628, 0.000000000000000000, 0.9945610877497982338 ) ) ;
#18472 = CARTESIAN_POINT ( 'NONE',  ( -3.812371247207599900, 1428.459941768050157, 200.5740418269730014 ) ) ;
#18474 = EDGE_LOOP ( 'NONE', ( #59799, #42744, #70521, #56888, #4222, #94232, #96298, #99219 ) ) ;
#18473 = CARTESIAN_POINT ( 'NONE',  ( -68.75448126042309127, 1379.747879528159956, 280.3343026105569606 ) ) ;
#18475 = CARTESIAN_POINT ( 'NONE',  ( 40.26396420611710170, 1444.186530323160014, 137.1012295353969819 ) ) ;
#18476 = ORIENTED_EDGE ( 'NONE', *, *, #34318, .T. ) ;
#18477 = CARTESIAN_POINT ( 'NONE',  ( 13.29425500587429099, 1516.551188142742603, 192.2497704072501108 ) ) ;
#18478 = EDGE_CURVE ( 'NONE', #46912, #42405, #49698, .T. ) ;
#18479 = CARTESIAN_POINT ( 'NONE',  ( -24.66781776999999920, 1430.359786449429976, 207.5926804364680152 ) ) ;
#18481 = CARTESIAN_POINT ( 'NONE',  ( 17.29966500927950079, 1410.740263436930263, 192.3341061383550255 ) ) ;
#18480 = CARTESIAN_POINT ( 'NONE',  ( -11.50950220968000082, 1425.948128105500018, 135.2567894809000109 ) ) ;
#18482 = EDGE_CURVE ( 'NONE', #36240, #97581, #45726, .T. ) ;
#18483 = CARTESIAN_POINT ( 'NONE',  ( -4.609064341505000328, 1516.723920667490120, 211.9995909164769898 ) ) ;
#18484 = CARTESIAN_POINT ( 'NONE',  ( 28.15304776960663347, 1510.007776421887002, 219.4938112226830640 ) ) ;
#18485 = CARTESIAN_POINT ( 'NONE',  ( -16.36456115631863284, 1519.551704408389924, 220.0929384032941698 ) ) ;
#18486 = CARTESIAN_POINT ( 'NONE',  ( -11.55307676520000015, 1412.346723819529871, 255.2309104534979838 ) ) ;
#18487 = CARTESIAN_POINT ( 'NONE',  ( -12.54333794360629817, 1378.892795628550175, 208.9638137175840029 ) ) ;
#18488 = EDGE_CURVE ( 'NONE', #60010, #75798, #87102, .T. ) ;
#18489 = CARTESIAN_POINT ( 'NONE',  ( 28.37476903720190080, 1508.765197038709857, 209.4266949452929794 ) ) ;
#18490 = EDGE_CURVE ( 'NONE', #76035, #33799, #76390, .T. ) ;
#18491 = CARTESIAN_POINT ( 'NONE',  ( -4.994708980640000462, 1391.711004509789973, 214.5419497225390160 ) ) ;
#18492 = CARTESIAN_POINT ( 'NONE',  ( -23.91153816693510592, 1410.421621729604794, 208.6572396396597355 ) ) ;
#18493 = EDGE_LOOP ( 'NONE', ( #8353, #56267, #23718 ) ) ;
#18494 = CARTESIAN_POINT ( 'NONE',  ( 11.09436156092809966, 1397.627175189450099, 216.7935160369219716 ) ) ;
#18495 = CARTESIAN_POINT ( 'NONE',  ( 10.06105783719169899, 1461.204106559300044, 207.9595875702549961 ) ) ;
#18496 = CARTESIAN_POINT ( 'NONE',  ( -18.04322080909999926, 1457.691026831229919, 229.4369243693979854 ) ) ;
#18497 = EDGE_LOOP ( 'NONE', ( #59028, #23226, #84925 ) ) ;
#18498 = ORIENTED_EDGE ( 'NONE', *, *, #55754, .T. ) ;
#18499 = CARTESIAN_POINT ( 'NONE',  ( 8.793327190495521251, 1451.709117791070184, 212.0827695763929910 ) ) ;
#18500 = CARTESIAN_POINT ( 'NONE',  ( 8.853113012480001487, 1424.852003149989969, 195.9493848808990037 ) ) ;
#18501 = ORIENTED_EDGE ( 'NONE', *, *, #17206, .F. ) ;
#18502 = CARTESIAN_POINT ( 'NONE',  ( -0.3187450556299999960, 1417.474787828929948, 184.6859738898979799 ) ) ;
#18503 = CARTESIAN_POINT ( 'NONE',  ( 10.54091203686897416, 1446.571174882411242, 153.1861154149677589 ) ) ;
#18504 = FACE_OUTER_BOUND ( 'NONE', #38353, .T. ) ;
#18505 = CARTESIAN_POINT ( 'NONE',  ( -0.7274293653769999812, 1461.199170862730170, 235.2852282102980155 ) ) ;
#18506 = CARTESIAN_POINT ( 'NONE',  ( 7.512716716675900130, 1509.034509426269778, 202.9804468418519718 ) ) ;
#18507 = SURFACE_SIDE_STYLE ('',( #27477 ) ) ;
#18508 = CARTESIAN_POINT ( 'NONE',  ( -12.50784581649999971, 1391.398398855719961, 210.4070514663689835 ) ) ;
#18509 = EDGE_CURVE ( 'NONE', #60035, #51052, #71117, .T. ) ;
#18510 = CARTESIAN_POINT ( 'NONE',  ( -87.98792674194200458, 1384.830566764610012, 291.2189899076259394 ) ) ;
#18511 = CARTESIAN_POINT ( 'NONE',  ( -2.292307268505000106, 1516.548716157039962, 202.1882291110970300 ) ) ;
#18512 = CARTESIAN_POINT ( 'NONE',  ( 2.491655725414999800, 1516.977504706749869, 209.8569557413499922 ) ) ;
#18513 = ORIENTED_EDGE ( 'NONE', *, *, #62702, .T. ) ;
#18514 = CARTESIAN_POINT ( 'NONE',  ( 11.85851152176929979, 1431.806602705250043, 149.9566501966939995 ) ) ;
#18515 = DIRECTION ( 'NONE',  ( 0.4090087482554164988, -1.225281874271768203E-16, -0.9125304618754035424 ) ) ;
#18516 = EDGE_LOOP ( 'NONE', ( #31577, #110495, #2934, #76228 ) ) ;
#18517 = CARTESIAN_POINT ( 'NONE',  ( 3.801724495280383476, 1509.034510030706542, 213.6092049197077358 ) ) ;
#18518 = CARTESIAN_POINT ( 'NONE',  ( -6.495308355903510744, 1508.529747571519920, 219.5985094923219947 ) ) ;
#18519 = CARTESIAN_POINT ( 'NONE',  ( 8.897726803999999490, 1507.634723498030098, 234.8284024826979817 ) ) ;
#18520 = EDGE_CURVE ( 'NONE', #16786, #48269, #8426, .T. ) ;
#18521 = CARTESIAN_POINT ( 'NONE',  ( -5.500484314761993510, 1489.299785632448902, 218.6043133970500776 ) ) ;
#18522 = CARTESIAN_POINT ( 'NONE',  ( -5.138143496799999710, 1421.871349575429804, 186.0645463248980036 ) ) ;
#18523 = CARTESIAN_POINT ( 'NONE',  ( 1.454159971469330070, 1408.575797871499844, 270.4288814118980326 ) ) ;
#18524 = DIRECTION ( 'NONE',  ( -0.8775825618903723147, 0.000000000000000000, -0.4794255386042039491 ) ) ;
#18525 = CARTESIAN_POINT ( 'NONE',  ( -6.256968529720000838, 1474.711004521489940, 200.7308274939090040 ) ) ;
#18526 = EDGE_CURVE ( 'NONE', #21788, #73262, #71069, .T. ) ;
#18527 = CARTESIAN_POINT ( 'NONE',  ( -2.280747111621419965, 1421.889025025900082, 193.3469174479820083 ) ) ;
#18528 = CARTESIAN_POINT ( 'NONE',  ( -41.90725927229999570, 1379.698394009460117, 226.1262471626590127 ) ) ;
#18529 = VECTOR ( 'NONE', #71427, 1000.000000000000000 ) ;
#18530 = DIRECTION ( 'NONE',  ( 0.6480245870892075155, -1.644245901462725924E-32, -0.7616194158028418704 ) ) ;
#18532 = CARTESIAN_POINT ( 'NONE',  ( 10.86930439285440109, 1469.920656080350000, 205.9146108117720075 ) ) ;
#18531 = CARTESIAN_POINT ( 'NONE',  ( -21.23742229959999861, 1505.497921528590041, 209.2995344244330056 ) ) ;
#18533 = CARTESIAN_POINT ( 'NONE',  ( 15.41004394052340132, 1507.593738228510119, 226.1372084082059928 ) ) ;
#18534 = CARTESIAN_POINT ( 'NONE',  ( 17.98982283035719831, 1423.319075982959930, 225.1697406702290323 ) ) ;
#18535 = CARTESIAN_POINT ( 'NONE',  ( -7.238531764446769934, 1498.497943084040116, 213.6891861245020152 ) ) ;
#18536 = ORIENTED_EDGE ( 'NONE', *, *, #47348, .F. ) ;
#18537 = CARTESIAN_POINT ( 'NONE',  ( 7.993605777300000598E-15, 1410.951844103529993, 268.3665355202980436 ) ) ;
#18538 = CIRCLE ( 'NONE', #81132, 1.999999999999998890 ) ;
#18539 = DIRECTION ( 'NONE',  ( -5.053215498073659967E-16, -1.000000000000000000, -2.442490654180000246E-15 ) ) ;
#18540 = B_SPLINE_SURFACE_WITH_KNOTS ( 'NONE', 5, 5, ( 
 ( #42510, #77781, #67186, #94014, #15626, #17834, #49832, #43079, #83962 ),
 ( #7804, #51469, #85056, #34112, #59345, #7262, #67739, #8346, #76670 ),
 ( #77239, #68302, #85601, #68850, #102952, #75591, #58775, #92913, #16186 ),
 ( #101287, #41971, #76123, #26253, #101848, #93454, #44186, #11141, #78327 ),
 ( #38383, #90436, #22105, #62109, #82035, #104073, #64730, #19510, #13713 ),
 ( #107246, #29979, #73106, #44748, #56305, #107801, #2204, #10577, #38926 ),
 ( #53715, #47899, #104630, #39499, #52592, #81476, #64171, #70515, #13162 ),
 ( #1639, #45301, #5340, #73674, #95131, #47349, #61005, #69959, #35777 ),
 ( #79441, #30539, #78898, #18949, #98844, #27368, #72559, #106688, #18393 ) ),
 .UNSPECIFIED., .F., .F., .F.,
 ( 6, 3, 6 ),
 ( 6, 3, 6 ),
 ( 19.36767300329999841, 21.57900985360000234, 24.75070551640000005 ),
 ( 0.000000000000000000, 1.000000000000000000, 2.000000000000000000 ),
 .UNSPECIFIED. ) ;
#18541 = DIRECTION ( 'NONE',  ( -0.000000000000000000, -1.000000000000000000, -0.000000000000000000 ) ) ;
#18542 = CARTESIAN_POINT ( 'NONE',  ( 5.597778194180000888, 1506.679269386989972, 219.3685102149989916 ) ) ;
#18543 = CARTESIAN_POINT ( 'NONE',  ( -14.00462132320000030, 1415.677402202029953, 214.2425697179989754 ) ) ;
#18545 = ORIENTED_EDGE ( 'NONE', *, *, #14450, .T. ) ;
#18544 = CARTESIAN_POINT ( 'NONE',  ( -11.25901873334290038, 1500.172003390719965, 210.8567363214919794 ) ) ;
#18546 = CARTESIAN_POINT ( 'NONE',  ( -15.84810074378578726, 1415.892833117942246, 209.7228954066766846 ) ) ;
#18547 = CARTESIAN_POINT ( 'NONE',  ( -24.31663498039999638, 1442.649881727339789, 211.4598683180379908 ) ) ;
#18548 = CARTESIAN_POINT ( 'NONE',  ( -16.31348683090000051, 1416.654170080089898, 208.8366974938609815 ) ) ;
#18549 = CARTESIAN_POINT ( 'NONE',  ( -14.45783243223209880, 1416.839692136300073, 221.3920770721769884 ) ) ;
#18550 = CARTESIAN_POINT ( 'NONE',  ( 27.01381218759999925, 1450.681579806120226, 136.4483250053980044 ) ) ;
#18551 = CARTESIAN_POINT ( 'NONE',  ( 14.10736255014890084, 1509.405700343320177, 234.8174336805699909 ) ) ;
#18552 = VECTOR ( 'NONE', #4486, 1000.000000000000000 ) ;
#18553 = CARTESIAN_POINT ( 'NONE',  ( 13.21074212996050079, 1428.906843343100036, 222.3308662938179907 ) ) ;
#18554 = CARTESIAN_POINT ( 'NONE',  ( -16.64927610386499879, 1512.799725290110018, 221.1696797412670037 ) ) ;
#18555 = CARTESIAN_POINT ( 'NONE',  ( 4.407100737270000401, 1415.074620172329787, 231.6221103901980030 ) ) ;
#18556 = CARTESIAN_POINT ( 'NONE',  ( -11.18808235593009925, 1482.416383379920035, 206.6602392150250296 ) ) ;
#18557 = CARTESIAN_POINT ( 'NONE',  ( -17.03425942710000029, 1460.964640061230057, 228.2738983644979953 ) ) ;
#18558 = CARTESIAN_POINT ( 'NONE',  ( 7.321455873725000174, 1516.545806094630279, 206.6359999332069890 ) ) ;
#18559 = CARTESIAN_POINT ( 'NONE',  ( 26.91412824380000046, 1412.677791826929933, 269.0204588372980083 ) ) ;
#18560 = CARTESIAN_POINT ( 'NONE',  ( 23.94500711619999933, 1436.145502024209918, 139.9316946685979701 ) ) ;
#18561 = CARTESIAN_POINT ( 'NONE',  ( 19.05531048790000170, 1469.162939635429893, 190.6018527114979975 ) ) ;
#18562 = CARTESIAN_POINT ( 'NONE',  ( -23.65757480440000293, 1436.093104310619992, 212.3677326929179969 ) ) ;
#18563 = CARTESIAN_POINT ( 'NONE',  ( -12.29793863238220020, 1378.259112548620124, 208.2596361589930041 ) ) ;
#18564 = DIRECTION ( 'NONE',  ( 0.000000000000000000, 0.000000000000000000, -1.000000000000000000 ) ) ;
#18565 = CARTESIAN_POINT ( 'NONE',  ( -1.740983587059999893, 1450.463600072650024, 182.5789179400979947 ) ) ;
#18566 = CARTESIAN_POINT ( 'NONE',  ( -13.86092847646930082, 1410.765486861110048, 227.1170286572800023 ) ) ;
#18567 = CARTESIAN_POINT ( 'NONE',  ( -15.42622997279999986, 1414.667236775670062, 209.1420281344999808 ) ) ;
#18568 = CARTESIAN_POINT ( 'NONE',  ( -12.65017221549999960, 1441.023539904969994, 188.0792847196979949 ) ) ;
#18569 = DIRECTION ( 'NONE',  ( 0.4794255386042041156, -5.511896626706601104E-17, -0.8775825618903722036 ) ) ;
#18570 = CARTESIAN_POINT ( 'NONE',  ( -31.76432722529999708, 1435.606706419230022, 135.1329931210979964 ) ) ;
#18571 = CARTESIAN_POINT ( 'NONE',  ( 1.914156610164409855, 1431.087920293139859, 199.8421651263110164 ) ) ;
#18572 = ORIENTED_EDGE ( 'NONE', *, *, #43940, .T. ) ;
#18573 = CARTESIAN_POINT ( 'NONE',  ( -2.392017086155000083, 1512.336926113599930, 201.5227265233669982 ) ) ;
#18574 = CARTESIAN_POINT ( 'NONE',  ( -13.02096109902269916, 1409.367762368420017, 201.7918158736540022 ) ) ;
#18575 = EDGE_CURVE ( 'NONE', #758, #85844, #84360, .T. ) ;
#18576 = CARTESIAN_POINT ( 'NONE',  ( -5.468515302949999324, 1438.698907413310053, 154.7381877631979989 ) ) ;
#18577 = CARTESIAN_POINT ( 'NONE',  ( 16.66936639845630097, 1523.382868172864164, 180.4828114240739296 ) ) ;
#18578 = CARTESIAN_POINT ( 'NONE',  ( -37.75040342469999644, 1461.765090176830199, 268.4864265932980061 ) ) ;
#18579 = CARTESIAN_POINT ( 'NONE',  ( -11.60577372236650007, 1481.108615670409790, 211.3960606566309934 ) ) ;
#18580 = DIRECTION ( 'NONE',  ( -1.755985294532469921E-16, 1.000000000000000000, -1.338183447452831989E-16 ) ) ;
#18581 = ADVANCED_FACE ( 'NONE', ( #37170 ), #44474, .F. ) ;
#18582 = CARTESIAN_POINT ( 'NONE',  ( 17.81563488885300117, 1417.676982138360017, 224.3990780826929949 ) ) ;
#18583 = CARTESIAN_POINT ( 'NONE',  ( -70.16143979324509417, 1384.662073857830137, 295.2445469226630053 ) ) ;
#18584 = CARTESIAN_POINT ( 'NONE',  ( -23.72885132301209765, 1384.957336300120005, 202.7962431987409957 ) ) ;
#18585 = DIRECTION ( 'NONE',  ( 0.000000000000000000, 0.000000000000000000, 1.000000000000000000 ) ) ;
#18586 = CARTESIAN_POINT ( 'NONE',  ( 16.73038498189999856, 1415.425582719929707, 215.1584419701680133 ) ) ;
#18587 = CARTESIAN_POINT ( 'NONE',  ( -3.240637488290000423, 1434.541222282480021, 155.4779008716980115 ) ) ;
#18588 = CARTESIAN_POINT ( 'NONE',  ( -4.491820960670080849E-16, 1519.551704408389924, 209.1218459616989946 ) ) ;
#18589 = CARTESIAN_POINT ( 'NONE',  ( 2.175409717514719593E-31, 1397.551704408390151, 209.1218459616989946 ) ) ;
#18590 = CARTESIAN_POINT ( 'NONE',  ( -7.888904176470000529, 1508.843978788529967, 181.1771252059980100 ) ) ;
#18591 = CARTESIAN_POINT ( 'NONE',  ( -23.14291596900000059, 1409.885718316829752, 207.0974899646379868 ) ) ;
#18592 = CARTESIAN_POINT ( 'NONE',  ( 14.44608937009999927, 1416.522662136229883, 196.8582539822980095 ) ) ;
#18593 = CARTESIAN_POINT ( 'NONE',  ( 4.644142782429999450, 1485.095378571789979, 218.9446188854689979 ) ) ;
#18594 = EDGE_CURVE ( 'NONE', #2720, #10258, #17359, .T. ) ;
#18595 = CARTESIAN_POINT ( 'NONE',  ( 5.161277829439999465, 1424.205378812969911, 193.2953232350990049 ) ) ;
#18596 = DIRECTION ( 'NONE',  ( 0.000000000000000000, 0.000000000000000000, 1.000000000000000000 ) ) ;
#18597 = CARTESIAN_POINT ( 'NONE',  ( 0.7745446704201689458, 1461.969662288189966, 230.4743262828090167 ) ) ;
#18598 = CARTESIAN_POINT ( 'NONE',  ( -6.081399352906980305, 1508.610505977480216, 216.4418972120009812 ) ) ;
#18599 = CARTESIAN_POINT ( 'NONE',  ( -9.966728093320000426, 1439.480327435690015, 208.4309914835989730 ) ) ;
#18601 = CARTESIAN_POINT ( 'NONE',  ( -8.179930635319999865, 1384.351711335470100, 199.6861503408189833 ) ) ;
#18600 = CARTESIAN_POINT ( 'NONE',  ( -22.77810859050000047, 1410.208903787329973, 210.9686725571380066 ) ) ;
#18602 = CARTESIAN_POINT ( 'NONE',  ( -0.1059456692259999888, 1414.379792559529960, 233.4365792652980076 ) ) ;
#18603 = CARTESIAN_POINT ( 'NONE',  ( 9.788188108289379130, 1435.901480349360099, 210.0315044652950007 ) ) ;
#18604 = CARTESIAN_POINT ( 'NONE',  ( -10.62155590039999886, 1491.490808487190179, 212.0487326096589982 ) ) ;
#18605 = CARTESIAN_POINT ( 'NONE',  ( -23.43225536839999990, 1425.871618787629814, 211.3010252580280053 ) ) ;
#18606 = AXIS2_PLACEMENT_3D ( 'NONE', #92322, #99611, #75003 ) ;
#18607 = CARTESIAN_POINT ( 'NONE',  ( -1.483050551783430038, 1420.942730047339865, 183.9156232671229816 ) ) ;
#18608 = CARTESIAN_POINT ( 'NONE',  ( 0.7365611785030020675, 1517.066898074209803, 204.4979538714769944 ) ) ;
#18609 = CARTESIAN_POINT ( 'NONE',  ( -7.991989199987382442, 1398.150427817915897, 219.3750528887007647 ) ) ;
#18610 = CARTESIAN_POINT ( 'NONE',  ( -17.38301961261850082, 1485.251990578760115, 188.4777382281349958 ) ) ;
#18611 = CARTESIAN_POINT ( 'NONE',  ( 2.744339645710000219, 1509.008894839529830, 238.2322746441979859 ) ) ;
#18612 = CARTESIAN_POINT ( 'NONE',  ( 7.222610535631719841, 1505.072920045980027, 218.4676445938339953 ) ) ;
#18613 = CARTESIAN_POINT ( 'NONE',  ( 38.88053497846389917, 1448.078305046199830, 136.4777416074680048 ) ) ;
#18615 = ORIENTED_EDGE ( 'NONE', *, *, #65043, .F. ) ;
#18614 = CARTESIAN_POINT ( 'NONE',  ( -63.27222210238460320, 1379.733933836859933, 271.8034403823299954 ) ) ;
#18616 = ORIENTED_EDGE ( 'NONE', *, *, #21255, .F. ) ;
#18617 = CARTESIAN_POINT ( 'NONE',  ( 11.74365990218139899, 1433.750782862119877, 150.9400914570229872 ) ) ;
#18618 = CARTESIAN_POINT ( 'NONE',  ( 20.85167258422537984, 1525.730671215511848, 184.1901402302743236 ) ) ;
#18619 = VERTEX_POINT ( 'NONE', #59748 ) ;
#18620 = DIRECTION ( 'NONE',  ( -0.007750486606685237645, 0.0002706418309149287806, 0.9999699279030140886 ) ) ;
#18621 = EDGE_CURVE ( 'NONE', #106344, #91492, #32204, .T. ) ;
#18622 = CARTESIAN_POINT ( 'NONE',  ( -10.23585214307190050, 1448.784286493050104, 207.3798671416320190 ) ) ;
#18623 = CARTESIAN_POINT ( 'NONE',  ( -7.552662639750000295, 1385.340273189239952, 219.0680905273789847 ) ) ;
#18624 =( BOUNDED_CURVE ( )  B_SPLINE_CURVE ( 3, ( #19700, #1831, #2938, #37057 ),
 .UNSPECIFIED., .F., .F. ) 
 B_SPLINE_CURVE_WITH_KNOTS ( ( 4, 4 ),
 ( 0.9036827175325773398, 1.148836376245267354 ),
 .UNSPECIFIED. ) 
 CURVE ( )  GEOMETRIC_REPRESENTATION_ITEM ( )  RATIONAL_B_SPLINE_CURVE ( ( 1.000000000000000000, 0.9949979080785074093, 0.9949979080785074093, 1.000000000000000000 ) ) 
 REPRESENTATION_ITEM ( '' )  );
#18626 = CARTESIAN_POINT ( 'NONE',  ( 6.629188914260000232, 1428.588785140030041, 91.31218443469779800 ) ) ;
#18625 = CARTESIAN_POINT ( 'NONE',  ( -1.063763185130000011, 1443.513877504690072, 200.1423821450789831 ) ) ;
#18627 = DIRECTION ( 'NONE',  ( 1.755985294532464991E-16, -1.000000000000000000, 1.338183447452830017E-16 ) ) ;
#18628 = ADVANCED_FACE ( 'NONE', ( #29309 ), #63185, .F. ) ;
#18629 = B_SPLINE_CURVE_WITH_KNOTS ( 'NONE', 3,
 ( #96366, #70100, #104213, #36450, #44887, #11808, #71194, #61150, #105316, #53848, #95265, #87985, #52723, #18527, #27500, #61688, #11273, #19077, #79579, #16667, #110207, #69342, #43022, #101791, #103451, #26757, #51975, #101229, #17216, #93949, #16128, #68245, #18340, #77722 ),
 .UNSPECIFIED., .F., .F.,
 ( 4, 3, 3, 3, 3, 3, 3, 3, 3, 3, 3, 4 ),
 ( -1.999999989621509933, -1.903346754608929992, -1.716103420023969983, -1.526665084407200057, -1.336006962675679866, -1.143849630969659970, -0.9512259096668089775, -0.7586077023791939489, -0.5664647939433908874, -0.3759670744414520538, -0.1870530681013899965, 0.000000000000000000 ),
 .UNSPECIFIED. ) ;
#18630 = CARTESIAN_POINT ( 'NONE',  ( 5.636002709010000444, 1488.168530458630130, 183.0004181446979885 ) ) ;
#18631 = CARTESIAN_POINT ( 'NONE',  ( 2.453786550779999853, 1468.127272575889947, 218.8237816726089875 ) ) ;
#18632 = CARTESIAN_POINT ( 'NONE',  ( 15.35953408680000010, 1409.616044574130228, 226.6522495080980093 ) ) ;
#18633 = B_SPLINE_SURFACE_WITH_KNOTS ( 'NONE', 5, 5, ( 
 ( #72987, #4671, #38810, #13591, #107124, #30415, #32071, #72447, #98722 ),
 ( #65692, #56733, #21982, #83563, #6320, #56174, #22533, #48901, #90313 ),
 ( #39926, #47779, #90870, #81914, #74094, #91436, #40468, #14158, #48344 ),
 ( #74643, #66262, #82483, #57847, #91974, #49441, #38262, #2017, #9290 ),
 ( #35033, #17094, #51855, #59703, #18219, #69212, #36153, #78704, #102234 ),
 ( #10382, #9834, #26629, #8719, #77601, #93282, #42336, #34489, #68664 ),
 ( #110640, #94373, #59163, #69779, #51286, #17654, #52964, #18767, #8167 ),
 ( #1441, #52415, #103321, #102764, #85420, #101664, #24953, #87097, #16545 ),
 ( #26060, #85992, #33925, #78138, #60255, #68121, #25511, #93815, #42898 ),
 ( #43453, #77056, #50736, #60825, #363, #907, #94950, #84869, #86541 ),
 ( #44555, #76488, #44003, #35587, #103897, #27196, #61379, #95498, #96048 ),
 ( #36698, #97703, #10952, #105569, #28855, #27741, #19319, #45681, #96611 ),
 ( #81428, #2576, #28295, #4205, #61932, #3678, #19880, #20425, #62491 ),
 ( #37806, #4739, #47304, #70892, #29936, #89849, #89304, #106108, #88212 ),
 ( #53520, #45124, #3126, #37254, #63586, #79266, #63050, #87663, #38337 ) ),
 .UNSPECIFIED., .F., .F., .F.,
 ( 6, 3, 3, 3, 6 ),
 ( 6, 3, 6 ),
 ( 3.366324640010000202, 5.876786115260000720, 8.564366035440000857, 10.59338889530000039, 13.45705438670000120 ),
 ( 0.000000000000000000, 1.000000000000000000, 2.000000000000000000 ),
 .UNSPECIFIED. ) ;
#18634 = CARTESIAN_POINT ( 'NONE',  ( -4.609673279564999504, 1516.754149861460064, 212.3872530880769887 ) ) ;
#18635 = CARTESIAN_POINT ( 'NONE',  ( 36.12226356638380054, 1436.069430018940011, 134.0999999971620014 ) ) ;
#18636 = CARTESIAN_POINT ( 'NONE',  ( -8.007800200046078842, 1425.247483720839909, 205.0429105383470016 ) ) ;
#18637 = CARTESIAN_POINT ( 'NONE',  ( 6.852741806675000547, 1514.298059036119867, 201.1790189594169931 ) ) ;
#18638 = ORIENTED_EDGE ( 'NONE', *, *, #19256, .F. ) ;
#18639 = CARTESIAN_POINT ( 'NONE',  ( 13.85944100054009986, 1434.989460371399900, 148.7312857378809952 ) ) ;
#18640 = DIRECTION ( 'NONE',  ( 0.000000000000000000, 0.000000000000000000, 1.000000000000000000 ) ) ;
#18641 = ORIENTED_EDGE ( 'NONE', *, *, #26073, .F. ) ;
#18642 = ORIENTED_EDGE ( 'NONE', *, *, #68384, .T. ) ;
#18643 = ORIENTED_EDGE ( 'NONE', *, *, #49995, .F. ) ;
#18644 = EDGE_CURVE ( 'NONE', #29004, #57276, #10797, .T. ) ;
#18645 = CARTESIAN_POINT ( 'NONE',  ( -7.263042217704999359, 1512.240414293150025, 215.9313971026869865 ) ) ;
#18646 = CARTESIAN_POINT ( 'NONE',  ( -0.8516783078649999839, 1465.062050906930153, 236.8964322150979740 ) ) ;
#18647 = CARTESIAN_POINT ( 'NONE',  ( -13.31089767776890120, 1503.456584347970193, 208.6977459380580058 ) ) ;
#18648 = CARTESIAN_POINT ( 'NONE',  ( 0.7533001353030019942, 1516.714320817460020, 216.4479181143769893 ) ) ;
#18649 = CARTESIAN_POINT ( 'NONE',  ( 2.767945032447589604, 1466.138307348149965, 198.4326037334419937 ) ) ;
#18650 = ADVANCED_FACE ( 'NONE', ( #14704 ), #97480, .F. ) ;
#18651 = CARTESIAN_POINT ( 'NONE',  ( -18.74243217561350505, 1444.811426355574213, 213.3821054765419376 ) ) ;
#18652 = CARTESIAN_POINT ( 'NONE',  ( -14.17772861730700207, 1379.591530685439920, 207.8208986668599891 ) ) ;
#18653 = CARTESIAN_POINT ( 'NONE',  ( 4.269062038300520001, 1446.683782444980125, 158.1563956602039980 ) ) ;
#18654 = CARTESIAN_POINT ( 'NONE',  ( -0.02849522097719999966, 1508.320473262429914, 237.7718752957979973 ) ) ;
#18655 = VERTEX_POINT ( 'NONE', #4131 ) ;
#18656 = CARTESIAN_POINT ( 'NONE',  ( 1.701729820345000199, 1516.969638403840008, 206.2395199527169893 ) ) ;
#18657 = ORIENTED_EDGE ( 'NONE', *, *, #26072, .T. ) ;
#18658 = CARTESIAN_POINT ( 'NONE',  ( 25.01214927662029908, 1440.913060387330006, 239.1462821668919787 ) ) ;
#18659 = CARTESIAN_POINT ( 'NONE',  ( 11.68483446183100050, 1479.114072787690020, 207.7860290712830249 ) ) ;
#18660 = ORIENTED_EDGE ( 'NONE', *, *, #24897, .F. ) ;
#18661 = CARTESIAN_POINT ( 'NONE',  ( 26.84712632248179887, 1449.046460843219847, 136.7362323706379925 ) ) ;
#18662 = CARTESIAN_POINT ( 'NONE',  ( -13.92641980429999826, 1410.772210879729982, 190.1674550056980024 ) ) ;
#18663 = DIRECTION ( 'NONE',  ( 1.989694733329999956E-13, 6.948167114160000380E-15, -1.000000000000000000 ) ) ;
#18664 = CARTESIAN_POINT ( 'NONE',  ( 2.504416157725709802, 1423.539630124239920, 192.6809389493199660 ) ) ;
#18665 = CARTESIAN_POINT ( 'NONE',  ( -6.265221826568949659, 1511.198033794599951, 201.6740346495409995 ) ) ;
#18666 = CARTESIAN_POINT ( 'NONE',  ( -12.41422776365670799, 1434.346862065572623, 147.3431289795544785 ) ) ;
#18667 = ADVANCED_FACE ( 'NONE', ( #98715 ), #66252, .F. ) ;
#18668 = FACE_OUTER_BOUND ( 'NONE', #39046, .T. ) ;
#18670 = CARTESIAN_POINT ( 'NONE',  ( 13.72624666093210521, 1519.551704408389924, 222.4326881300486889 ) ) ;
#18669 = CARTESIAN_POINT ( 'NONE',  ( 34.18677586421189574, 1501.977400791986611, 219.7932833225211766 ) ) ;
#18671 = B_SPLINE_CURVE_WITH_KNOTS ( 'NONE', 3,
 ( #27412, #78379, #87332, #10628, #95180, #10062, #70011, #11190, #60490, #96282, #44235, #94611, #8954, #43127, #69451, #86216, #26300, #104125, #53765, #95728, #1687, #18992 ),
 .UNSPECIFIED., .F., .F.,
 ( 4, 3, 3, 3, 3, 3, 3, 4 ),
 ( -136.9024435287539916, -136.6634106196869993, -136.4076183642550006, -136.1480203043660140, -135.8861880622630167, -135.6207110178370101, -135.3532902909820166, -135.0843706930000110 ),
 .UNSPECIFIED. ) ;
#18672 = EDGE_CURVE ( 'NONE', #44714, #29814, #90862, .T. ) ;
#18673 = B_SPLINE_SURFACE_WITH_KNOTS ( 'NONE', 4, 5, ( 
 ( #20675, #103748, #76340, #27590, #25357, #17501 ),
 ( #33770, #34882, #27050, #54875, #104301, #34335 ),
 ( #18611, #43846, #18070, #10233, #51698, #44410 ),
 ( #103171, #752, #61775, #67966, #52264, #59550 ),
 ( #1298, #95899, #211, #16944, #8022, #78550 ) ),
 .UNSPECIFIED., .F., .F., .F.,
 ( 5, 5 ),
 ( 6, 6 ),
 ( 4.939581942080000232, 5.112719791149999971 ),
 ( 0.000000000000000000, 2.000000000000000000 ),
 .UNSPECIFIED. ) ;
#18674 = CARTESIAN_POINT ( 'NONE',  ( 6.944231748164999551, 1516.882690742909972, 215.6753703478370028 ) ) ;
#18675 = CARTESIAN_POINT ( 'NONE',  ( -3.434354545275740023, 1428.676800484289970, 200.4110178052179947 ) ) ;
#18676 = CARTESIAN_POINT ( 'NONE',  ( 5.910253135570970429, 1511.600194708689969, 217.7510657911269902 ) ) ;
#18677 = CARTESIAN_POINT ( 'NONE',  ( 29.28654147530000174, 1509.872632245929935, 208.8940174685830016 ) ) ;
#18678 = CARTESIAN_POINT ( 'NONE',  ( 1.136004274065000041, 1516.815173273089840, 211.9874827793370287 ) ) ;
#18679 = CARTESIAN_POINT ( 'NONE',  ( 13.98887932740000117, 1409.902971935330015, 191.4712550325980089 ) ) ;
#18680 = CARTESIAN_POINT ( 'NONE',  ( 30.24977872777046883, 1524.075132568165373, 222.4742436132389685 ) ) ;
#18682 = ORIENTED_EDGE ( 'NONE', *, *, #108224, .F. ) ;
#18681 = CARTESIAN_POINT ( 'NONE',  ( -87.30316128990000379, 1388.086780051900178, 306.8656371684590454 ) ) ;
#18683 = CARTESIAN_POINT ( 'NONE',  ( 26.02371791099999854, 1449.849912737939803, 231.9820475135979905 ) ) ;
#18684 = CARTESIAN_POINT ( 'NONE',  ( 2.886380516782709904, 1451.746737126376729, 183.8547243489458083 ) ) ;
#18685 = CARTESIAN_POINT ( 'NONE',  ( -27.55179926645890021, 1509.875190418580132, 219.2242857432399887 ) ) ;
#18686 = CARTESIAN_POINT ( 'NONE',  ( -2.551512840923239711, 1507.143442698440140, 236.9472663481859911 ) ) ;
#18687 = CARTESIAN_POINT ( 'NONE',  ( -18.55872592980000135, 1457.839997766830038, 227.5285588847980023 ) ) ;
#18688 = CIRCLE ( 'NONE', #95599, 1.999999999999998668 ) ;
#18689 = B_SPLINE_CURVE_WITH_KNOTS ( 'NONE', 3,
 ( #20494, #46308, #80437, #72067, #92674, #42282, #91021, #40627, #59104, #32230, #8116, #110039, #100528, #6476, #7024, #66410, #74797, #108941, #101611, #16495, #5930, #40076, #83187, #76433, #58548, #68062, #108388, #66956, #57999, #102176, #50152, #101066, #33313, #15952, #23807, #84281, #99968, #56890, #67507, #14308, #24896, #92133 ),
 .UNSPECIFIED., .F., .F.,
 ( 4, 2, 2, 2, 2, 2, 1, 1, 1, 1, 1, 2, 2, 2, 2, 2, 1, 1, 1, 2, 2, 2, 2, 2, 4 ),
 ( 0.000000000000000000, 0.06249999999974691078, 0.1249999999994938216, 0.1874999999992407185, 0.2187499999991080746, 0.2343749999990482891, 0.2421874999990115684, 0.2460937499989931943, 0.2480468749989771515, 0.2490234374989692134, 0.2495117187489654109, 0.2497558593739636346, 0.2499999999989618304, 0.3749999999990640820, 0.4374999999991111554, 0.4687499999991348032, 0.4843749999991467381, 0.4921874999991526778, 0.4960937499991557864, 0.4980468749991602828, 0.4999999999991647792, 0.6249999999993736122, 0.7499999999995823341, 0.8749999999997911670, 1.000000000000000000 ),
 .UNSPECIFIED. ) ;
#18691 = CARTESIAN_POINT ( 'NONE',  ( 17.96820147240839916, 1410.603916924019813, 222.9561480445759969 ) ) ;
#18690 = CARTESIAN_POINT ( 'NONE',  ( 10.96878214529999873, 1432.307818762199986, 151.7701606857980039 ) ) ;
#18692 = DIRECTION ( 'NONE',  ( 0.000000000000000000, 0.000000000000000000, 1.000000000000000000 ) ) ;
#18693 = CARTESIAN_POINT ( 'NONE',  ( -109.1074149406630056, 1382.912272179509955, 310.9584811440479939 ) ) ;
#18694 = VERTEX_POINT ( 'NONE', #5211 ) ;
#18695 = CARTESIAN_POINT ( 'NONE',  ( -3.263521942484999716, 1516.676340709600026, 203.3494421577970002 ) ) ;
#18696 = CARTESIAN_POINT ( 'NONE',  ( 0.1067562447540000015, 1406.506670174130022, 269.4986873273979882 ) ) ;
#18697 = CIRCLE ( 'NONE', #81285, 1.999999999999998668 ) ;
#18698 = CARTESIAN_POINT ( 'NONE',  ( 27.94676410629999808, 1509.200065888029940, 207.5540313486380057 ) ) ;
#18699 = AXIS2_PLACEMENT_3D ( 'NONE', #74801, #83189, #14310 ) ;
#18700 = CARTESIAN_POINT ( 'NONE',  ( 6.588862402215439396, 1473.264983703350026, 270.4290835591440327 ) ) ;
#18701 = FACE_OUTER_BOUND ( 'NONE', #110734, .T. ) ;
#18702 = DIRECTION ( 'NONE',  ( -0.6736849260149578855, 0.000000000000000000, 0.7390186874905266823 ) ) ;
#18703 = CARTESIAN_POINT ( 'NONE',  ( 15.58948595390000058, 1452.698291846990060, 196.7507890572990163 ) ) ;
#18704 = CARTESIAN_POINT ( 'NONE',  ( -19.36857742237540236, 1526.335487865669393, 232.9229765951374986 ) ) ;
#18705 = CARTESIAN_POINT ( 'NONE',  ( -26.21059033610000100, 1446.264569515290077, 137.9459526830979996 ) ) ;
#18706 = CARTESIAN_POINT ( 'NONE',  ( 2.424607408659378738, 1449.446473553185797, 154.4675859022806321 ) ) ;
#18707 = CARTESIAN_POINT ( 'NONE',  ( -0.8833778638539989680, 1431.444913390889951, 200.7505307741990350 ) ) ;
#18708 = CARTESIAN_POINT ( 'NONE',  ( 11.22762520574680067, 1480.213122129130170, 210.8215595684870038 ) ) ;
#18709 = B_SPLINE_CURVE_WITH_KNOTS ( 'NONE', 5,
 ( #71075, #29044, #44196, #18402, #10026, #37442 ),
 .UNSPECIFIED., .F., .F.,
 ( 6, 6 ),
 ( 203.4370383600000025, 213.0683255119999728 ),
 .UNSPECIFIED. ) ;
#18710 = CARTESIAN_POINT ( 'NONE',  ( -21.83550407203938448, 1523.678648413191922, 183.2743720722711203 ) ) ;
#18711 = CARTESIAN_POINT ( 'NONE',  ( -19.53786426058999481, 1501.977400791986611, 236.7197124308268030 ) ) ;
#18712 = ORIENTED_EDGE ( 'NONE', *, *, #65604, .F. ) ;
#18713 = DIRECTION ( 'NONE',  ( 9.056288633775531119E-47, -1.000000000000000000, 1.836970198721029688E-16 ) ) ;
#18714 = ADVANCED_FACE ( 'NONE', ( #82476 ), #1450, .F. ) ;
#18715 = CARTESIAN_POINT ( 'NONE',  ( 2.104449570759999943, 1486.697367722790204, 197.3627489980989935 ) ) ;
#18716 = CARTESIAN_POINT ( 'NONE',  ( 8.801276039060120127, 1468.409988194280004, 201.9109974982270046 ) ) ;
#18717 = CARTESIAN_POINT ( 'NONE',  ( -0.3323210813560000254, 1416.988076901430077, 234.1774585115979903 ) ) ;
#18718 = CARTESIAN_POINT ( 'NONE',  ( 11.87757256900000158, 1501.074157048189818, 209.1815870390489920 ) ) ;
#18719 = CARTESIAN_POINT ( 'NONE',  ( -31.69312280309501872, 1525.713797967457140, 196.3032712708389909 ) ) ;
#18720 = CARTESIAN_POINT ( 'NONE',  ( 8.334173048470001177, 1428.385525302790029, 213.5056454938490162 ) ) ;
#18721 = CARTESIAN_POINT ( 'NONE',  ( -20.98450557191650034, 1384.859229475929851, 221.3795081009360217 ) ) ;
#18722 = CARTESIAN_POINT ( 'NONE',  ( -10.25237677790000035, 1481.942191430589901, 205.9184038113290001 ) ) ;
#18723 = CARTESIAN_POINT ( 'NONE',  ( 26.13227424183079961, 1436.228979033299993, 136.7358178123800201 ) ) ;
#18724 = VECTOR ( 'NONE', #93539, 1000.000000000000227 ) ;
#18725 = CARTESIAN_POINT ( 'NONE',  ( -13.42559421921827756, 1443.464041502655164, 169.3656302353889771 ) ) ;
#18726 = ORIENTED_EDGE ( 'NONE', *, *, #79451, .T. ) ;
#18727 = B_SPLINE_CURVE_WITH_KNOTS ( 'NONE', 3,
 ( #46343, #28967, #82106, #72623, #38992, #80472, #55286, #5404, #54738, #97256 ),
 .UNSPECIFIED., .F., .F.,
 ( 4, 2, 2, 2, 4 ),
 ( -0.1172112179306550039, -0.1055921015938769969, -0.09159876550525229699, -0.04939298262307730003, -2.270117807623428519E-08 ),
 .UNSPECIFIED. ) ;
#18728 = ADVANCED_FACE ( 'NONE', ( #85209 ), #28306, .T. ) ;
#18729 = CARTESIAN_POINT ( 'NONE',  ( 30.31940284292408450, 1523.456872492435195, 195.7503880523414352 ) ) ;
#18730 = CARTESIAN_POINT ( 'NONE',  ( 2.461716435160000049, 1435.943783413959864, 150.4083956814980070 ) ) ;
#18731 = ORIENTED_EDGE ( 'NONE', *, *, #96197, .F. ) ;
#18732 = CARTESIAN_POINT ( 'NONE',  ( -12.05448508659999973, 1501.734409279790043, 211.4994548207789649 ) ) ;
#18733 = CARTESIAN_POINT ( 'NONE',  ( -15.08255442401187452, 1416.081365602056167, 205.7412506966217336 ) ) ;
#18734 = AXIS2_PLACEMENT_3D ( 'NONE', #84209, #102108, #34369 ) ;
#18735 = CARTESIAN_POINT ( 'NONE',  ( -9.499897081856666148, 1447.499268979973067, 186.3975894871608432 ) ) ;
#18737 = DIRECTION ( 'NONE',  ( 1.000000000000000000, 3.155441816300000491E-15, -4.343610028670000616E-15 ) ) ;
#18736 = CARTESIAN_POINT ( 'NONE',  ( 9.970730613730001579, 1425.233768695029994, 92.69245245969780456 ) ) ;
#18738 = CARTESIAN_POINT ( 'NONE',  ( -2.584559296679999729, 1450.363170855389853, 190.1601826918989957 ) ) ;
#18739 = EDGE_CURVE ( 'NONE', #80101, #65500, #44328, .T. ) ;
#18740 = CARTESIAN_POINT ( 'NONE',  ( 4.147542412012739987, 1424.336585509140150, 184.6878609135509919 ) ) ;
#18741 = CARTESIAN_POINT ( 'NONE',  ( 4.034908559714999399, 1517.068717944079935, 201.7859449365070077 ) ) ;
#18742 = CARTESIAN_POINT ( 'NONE',  ( 7.536781297509999256, 1425.186457032809813, 212.1414899705590074 ) ) ;
#18743 = CARTESIAN_POINT ( 'NONE',  ( -13.97985296220000073, 1420.196174967039951, 195.9955836506989897 ) ) ;
#18744 = CARTESIAN_POINT ( 'NONE',  ( -5.496430460230245174, 1510.805212306242311, 201.5628357701014011 ) ) ;
#18745 = CARTESIAN_POINT ( 'NONE',  ( -101.7780583737760054, 1379.485289778789820, 304.0159838458559989 ) ) ;
#18746 = CARTESIAN_POINT ( 'NONE',  ( 7.999780308251754235, 1364.916505385960136, 209.6218459617148824 ) ) ;
#18748 = VERTEX_POINT ( 'NONE', #35934 ) ;
#18747 = CARTESIAN_POINT ( 'NONE',  ( -1.450401175619670857, 1465.036285778872980, 237.9109514038669886 ) ) ;
#18749 = ORIENTED_EDGE ( 'NONE', *, *, #52842, .F. ) ;
#18750 = CARTESIAN_POINT ( 'NONE',  ( -41.15112044609999487, 1443.645550130990159, 136.9181562709980255 ) ) ;
#18751 = CARTESIAN_POINT ( 'NONE',  ( 0.8193110093525590720, 1474.780960361229745, 235.8603769791739921 ) ) ;
#18752 = DIRECTION ( 'NONE',  ( -1.987538202299999878E-13, 0.000000000000000000, 1.000000000000000000 ) ) ;
#18753 = CARTESIAN_POINT ( 'NONE',  ( -7.564413999595000604, 1511.011611623900080, 212.4015039894770212 ) ) ;
#18754 = DIRECTION ( 'NONE',  ( 1.755985294532464991E-16, -1.000000000000000000, 1.338183447452830017E-16 ) ) ;
#18755 = CARTESIAN_POINT ( 'NONE',  ( -31.62137330308219063, 1525.231909165050865, 201.5806583896697646 ) ) ;
#18756 = EDGE_CURVE ( 'NONE', #63442, #2433, #45997, .T. ) ;
#18757 = CARTESIAN_POINT ( 'NONE',  ( 10.80134480061129842, 1446.564900598669965, 153.0805715986590201 ) ) ;
#18758 = CARTESIAN_POINT ( 'NONE',  ( -35.06783964556029787, 1451.227222927539970, 135.9148696056909955 ) ) ;
#18759 = CARTESIAN_POINT ( 'NONE',  ( -2.500000000000000000, 1448.271846337009947, 165.0527805226990097 ) ) ;
#18760 = CARTESIAN_POINT ( 'NONE',  ( 5.343479918049999888, 1396.099658817830004, 218.7752541424879951 ) ) ;
#18761 = CARTESIAN_POINT ( 'NONE',  ( 6.845616174217879824, 1409.091719448260164, 195.7806122793810175 ) ) ;
#18762 = CARTESIAN_POINT ( 'NONE',  ( -0.7759870753352450246, 1405.716808862310018, 267.8539888477289992 ) ) ;
#18763 = EDGE_CURVE ( 'NONE', #33528, #5040, #81719, .T. ) ;
#18764 = DIRECTION ( 'NONE',  ( -0.9997613315435491810, 0.000000000000000000, 0.02184673774890954004 ) ) ;
#18765 = VERTEX_POINT ( 'NONE', #36472 ) ;
#18766 = CARTESIAN_POINT ( 'NONE',  ( -113.4000000000000057, 1384.926148861439970, 304.2218459572590064 ) ) ;
#18767 = CARTESIAN_POINT ( 'NONE',  ( 14.11608679399999922, 1444.853469894119826, 189.4447253316980095 ) ) ;
#18768 = ORIENTED_EDGE ( 'NONE', *, *, #35246, .F. ) ;
#18769 = ORIENTED_EDGE ( 'NONE', *, *, #76182, .T. ) ;
#18770 = EDGE_CURVE ( 'NONE', #84181, #31410, #21463, .T. ) ;
#18771 = CARTESIAN_POINT ( 'NONE',  ( -11.60004869885204215, 1426.273944179774844, 138.2686100621498326 ) ) ;
#18772 = DIRECTION ( 'NONE',  ( -1.000000000000000000, 0.000000000000000000, 0.000000000000000000 ) ) ;
#18773 = CARTESIAN_POINT ( 'NONE',  ( 6.559798056295000457, 1516.987478262539980, 213.7368632980669929 ) ) ;
#18774 = CARTESIAN_POINT ( 'NONE',  ( 2.966689972984999812, 1511.639769324940062, 216.8150789852670073 ) ) ;
#18775 = B_SPLINE_CURVE_WITH_KNOTS ( 'NONE', 5,
 ( #90832, #39335, #87685, #62508, #96066, #73508 ),
 .UNSPECIFIED., .F., .F.,
 ( 6, 6 ),
 ( 0.000000000000000000, 1.000000000000000000 ),
 .UNSPECIFIED. ) ;
#18776 = ADVANCED_FACE ( 'NONE', ( #96945 ), #4216, .F. ) ;
#18777 = VERTEX_POINT ( 'NONE', #54950 ) ;
#18778 = CARTESIAN_POINT ( 'NONE',  ( -94.55573068399999670, 1374.531630663889928, 302.1084921616590009 ) ) ;
#18779 = CARTESIAN_POINT ( 'NONE',  ( -106.1739094701860040, 1378.913060387289988, 302.4879143702450506 ) ) ;
#18780 = CARTESIAN_POINT ( 'NONE',  ( -1.711311266675000109, 1516.591755933730155, 203.3510257909670145 ) ) ;
#18781 = CARTESIAN_POINT ( 'NONE',  ( -27.92468909959999834, 1509.154588341429871, 205.8536344554680113 ) ) ;
#18782 = B_SPLINE_SURFACE_WITH_KNOTS ( 'NONE', 5, 5, ( 
 ( #7993, #77417, #722, #69041, #26443, #60638 ),
 ( #104272, #106472, #89118, #63947, #12948, #46041 ),
 ( #88586, #53336, #29757, #79090, #45499, #70161 ),
 ( #95866, #4034, #71819, #2943, #104823, #27560 ),
 ( #105940, #28109, #62874, #87484, #61744, #98060 ),
 ( #89662, #20793, #54995, #38162, #37617, #29218 ) ),
 .UNSPECIFIED., .F., .F., .F.,
 ( 6, 6 ),
 ( 6, 6 ),
 ( 42.64499113449999612, 56.13383365260000346 ),
 ( 0.000000000000000000, 2.000000000000000000 ),
 .UNSPECIFIED. ) ;
#18783 = CARTESIAN_POINT ( 'NONE',  ( -5.551188713984379852, 1510.480349263560129, 201.5713426139130320 ) ) ;
#18784 = CARTESIAN_POINT ( 'NONE',  ( 40.26396420611710170, 1444.186530323160014, 137.1012295353969819 ) ) ;
#18785 = CARTESIAN_POINT ( 'NONE',  ( -62.89508772654340873, 1384.691239647969724, 250.3595330377160337 ) ) ;
#18786 = CARTESIAN_POINT ( 'NONE',  ( 20.50000000000000000, 1443.913060387330006, 169.0968414572980123 ) ) ;
#18787 = CARTESIAN_POINT ( 'NONE',  ( -4.226789392379999732, 1409.996198396630007, 232.1190139888980184 ) ) ;
#18789 = ORIENTED_EDGE ( 'NONE', *, *, #18520, .T. ) ;
#18788 = CARTESIAN_POINT ( 'NONE',  ( -5.757247049150000073, 1446.202579340599868, 184.3601040033979928 ) ) ;
#18790 = EDGE_CURVE ( 'NONE', #103217, #105896, #25176, .T. ) ;
#18791 = CARTESIAN_POINT ( 'NONE',  ( -13.96141271054625399, 1435.007883397890055, 148.7887677015099257 ) ) ;
#18792 = CARTESIAN_POINT ( 'NONE',  ( -1.906499846882070084E-08, 1517.051704408389924, 209.1218459511669892 ) ) ;
#18793 = CARTESIAN_POINT ( 'NONE',  ( 19.15622051997149811, 1456.936057672450261, 224.8950397092459923 ) ) ;
#18794 = CARTESIAN_POINT ( 'NONE',  ( 9.549000552458089430, 1470.075890067440014, 212.3436661921319910 ) ) ;
#18795 = CARTESIAN_POINT ( 'NONE',  ( -24.64665313769999955, 1435.432891414579899, 136.6581518711979868 ) ) ;
#18796 = EDGE_CURVE ( 'NONE', #5392, #38044, #109745, .T. ) ;
#18797 = CARTESIAN_POINT ( 'NONE',  ( 3.267603515704999850, 1516.858171774179937, 212.3749871074670068 ) ) ;
#18798 = CARTESIAN_POINT ( 'NONE',  ( -66.95646680580000520, 1379.743567625210062, 276.4036447723590300 ) ) ;
#18799 = CARTESIAN_POINT ( 'NONE',  ( -12.87561223598270033, 1428.667272998819954, 222.5140706137790119 ) ) ;
#18800 = CARTESIAN_POINT ( 'NONE',  ( 19.64609177186540023, 1476.662525844680204, 214.0395018079669853 ) ) ;
#18802 = CARTESIAN_POINT ( 'NONE',  ( 22.11164323276918608, 1411.043578901620094, 203.7708757951590428 ) ) ;
#18801 = AXIS2_PLACEMENT_3D ( 'NONE', #103083, #17411, #78461 ) ;
#18803 = CARTESIAN_POINT ( 'NONE',  ( -4.623892098755000291, 1517.066898074209803, 208.3852847535989952 ) ) ;
#18804 = ADVANCED_FACE ( 'NONE', ( #72842 ), #98062, .F. ) ;
#18805 = ORIENTED_EDGE ( 'NONE', *, *, #48148, .T. ) ;
#18806 = CARTESIAN_POINT ( 'NONE',  ( 2.500000000000000000, 1437.759198978020095, 157.6719144024980039 ) ) ;
#18807 = CARTESIAN_POINT ( 'NONE',  ( -1.746867988079999989, 1410.306430355730072, 232.8692363036980169 ) ) ;
#18808 = CARTESIAN_POINT ( 'NONE',  ( -59.23393169420000248, 1385.069165163979960, 279.9259648821590645 ) ) ;
#18809 = ORIENTED_EDGE ( 'NONE', *, *, #10421, .T. ) ;
#18810 = CARTESIAN_POINT ( 'NONE',  ( -105.6563836332091597, 1378.913058981198219, 304.0447272458403631 ) ) ;
#18811 = CARTESIAN_POINT ( 'NONE',  ( -3.478767832449999986, 1430.446984450989930, 201.5308695822689913 ) ) ;
#18812 = CARTESIAN_POINT ( 'NONE',  ( 12.11785592040000026, 1434.486425630220083, 150.7184365762979894 ) ) ;
#18813 = CARTESIAN_POINT ( 'NONE',  ( 16.09934221701070101, 1488.408557597590061, 230.7030962951629931 ) ) ;
#18814 = AXIS2_PLACEMENT_3D ( 'NONE', #37126, #80787, #88100 ) ;
#18815 = CARTESIAN_POINT ( 'NONE',  ( -24.09814616333339998, 1444.255785637029931, 212.5772553280679915 ) ) ;
#18816 = LINE ( 'NONE', #45167, #2632 ) ;
#18817 = CARTESIAN_POINT ( 'NONE',  ( 12.03764642179999989, 1426.191797886159975, 202.7989836356990168 ) ) ;
#18818 = CARTESIAN_POINT ( 'NONE',  ( 0.003115715631340339620, 1420.443923427290201, 182.6727572773859833 ) ) ;
#18820 = CARTESIAN_POINT ( 'NONE',  ( -4.463702575220000135, 1420.728434228329888, 186.4092242875980219 ) ) ;
#18819 = CARTESIAN_POINT ( 'NONE',  ( -2.482067898354999969, 1517.099836525840146, 214.9099431973869798 ) ) ;
#18821 = CARTESIAN_POINT ( 'NONE',  ( 19.05944848800000102, 1508.258419250929819, 188.5048453100980055 ) ) ;
#18822 = CARTESIAN_POINT ( 'NONE',  ( -5.778999811904999895, 1516.955859323880077, 216.4549161051170074 ) ) ;
#18823 = EDGE_LOOP ( 'NONE', ( #69631, #90970, #5181, #102016, #20560 ) ) ;
#18824 = CARTESIAN_POINT ( 'NONE',  ( 2.291514297774999598, 1517.194972660189933, 201.3955140066269962 ) ) ;
#18825 = CARTESIAN_POINT ( 'NONE',  ( -4.602356253840000022, 1468.583955076089978, 189.7619545879989857 ) ) ;
#18826 = ORIENTED_EDGE ( 'NONE', *, *, #95281, .T. ) ;
#18827 = CARTESIAN_POINT ( 'NONE',  ( 3.666229469220000148, 1421.722428054930106, 183.6097529654979894 ) ) ;
#18828 = CARTESIAN_POINT ( 'NONE',  ( -13.16517659032116860, 1522.051704408389924, 224.1947148507618408 ) ) ;
#18829 = CARTESIAN_POINT ( 'NONE',  ( 8.467409380977830580, 1511.685461860059831, 203.1348221448780009 ) ) ;
#18830 = CARTESIAN_POINT ( 'NONE',  ( 2.961602933630000045, 1442.729505202489918, 217.4993384840889803 ) ) ;
#18831 = CARTESIAN_POINT ( 'NONE',  ( -0.02955819112566700213, 1522.051704408389924, 225.0080808726450243 ) ) ;
#18832 = CARTESIAN_POINT ( 'NONE',  ( -15.94347048536829803, 1409.469818645040050, 192.9752432267480060 ) ) ;
#18833 = CARTESIAN_POINT ( 'NONE',  ( 17.58950218620000072, 1415.041103189330215, 210.4382088494780021 ) ) ;
#18834 = CARTESIAN_POINT ( 'NONE',  ( -19.04437315719999901, 1425.784752839030034, 226.3805134473980161 ) ) ;
#18835 = CARTESIAN_POINT ( 'NONE',  ( -15.10045379129999965, 1436.261357401330088, 149.5558351856980153 ) ) ;
#18836 = CARTESIAN_POINT ( 'NONE',  ( -3.882745883101669904, 1464.675334460000158, 198.8121422478580200 ) ) ;
#18837 = CARTESIAN_POINT ( 'NONE',  ( 6.391938627041045429, 1508.551704408389924, 216.1347676210409077 ) ) ;
#18839 = CARTESIAN_POINT ( 'NONE',  ( -9.854212473397289784, 1509.383236553660026, 180.6764149878760009 ) ) ;
#18838 = LINE ( 'NONE', #36769, #46563 ) ;
#18840 = CARTESIAN_POINT ( 'NONE',  ( 5.513435558552499671, 1509.038615934029849, 201.6090957240569992 ) ) ;
#18841 = EDGE_LOOP ( 'NONE', ( #46931, #70823, #89777, #17365 ) ) ;
#18842 = CARTESIAN_POINT ( 'NONE',  ( 1.555973022161739827, 1415.219159636500081, 191.2001064328639757 ) ) ;
#18843 = CARTESIAN_POINT ( 'NONE',  ( -4.491284101706960463, 1508.884228866460035, 211.6097700714119867 ) ) ;
#18844 = CARTESIAN_POINT ( 'NONE',  ( -21.12854634993719927, 1507.715432715349834, 209.4790063854959783 ) ) ;
#18845 = CARTESIAN_POINT ( 'NONE',  ( 29.33431687954583111, 1526.382868172863937, 217.1433072912829800 ) ) ;
#18846 = CARTESIAN_POINT ( 'NONE',  ( -3.639483821036900046, 1426.011012282639740, 185.9494021309836569 ) ) ;
#18847 = CARTESIAN_POINT ( 'NONE',  ( 29.55269881708361268, 1525.821544997590536, 221.1141083160992764 ) ) ;
#18848 = CARTESIAN_POINT ( 'NONE',  ( -11.24594776555490050, 1470.381349896640131, 210.9060676379959887 ) ) ;
#18849 = CARTESIAN_POINT ( 'NONE',  ( -9.799324650868589615, 1490.915621052960205, 214.1421080411050184 ) ) ;
#18850 = CARTESIAN_POINT ( 'NONE',  ( -2.515593459366479934, 1448.349639805989909, 188.5842434069749913 ) ) ;
#18851 = CARTESIAN_POINT ( 'NONE',  ( -100.5687700116990015, 1383.763643007270048, 310.7088986134360198 ) ) ;
#18852 = AXIS2_PLACEMENT_3D ( 'NONE', #17747, #18864, #86091 ) ;
#18853 = DIRECTION ( 'NONE',  ( -0.7071067811860475283, 0.000000000000000000, -0.7071067811870476172 ) ) ;
#18854 = CARTESIAN_POINT ( 'NONE',  ( -31.44837959398599736, 1511.187213306747708, 197.3353852117985525 ) ) ;
#18855 = CARTESIAN_POINT ( 'NONE',  ( -2.409189714827860040, 1516.533014244449987, 201.4128479977840129 ) ) ;
#18857 = EDGE_LOOP ( 'NONE', ( #39733, #12445, #28894, #12750 ) ) ;
#18856 = CARTESIAN_POINT ( 'NONE',  ( 10.54727210182790031, 1452.235375780489903, 208.6466202666740060 ) ) ;
#18858 = CARTESIAN_POINT ( 'NONE',  ( 17.25022834990030063, 1507.614846683550240, 193.9485721999670034 ) ) ;
#18859 = CARTESIAN_POINT ( 'NONE',  ( -76.21403627649999635, 1383.779720587099746, 301.0850818666589817 ) ) ;
#18860 = LINE ( 'NONE', #79354, #58647 ) ;
#18861 = VERTEX_POINT ( 'NONE', #17292 ) ;
#18862 = ORIENTED_EDGE ( 'NONE', *, *, #5027, .F. ) ;
#18863 = CARTESIAN_POINT ( 'NONE',  ( 19.72894155641759895, 1509.632479176759944, 231.2927645791820055 ) ) ;
#18864 = DIRECTION ( 'NONE',  ( -0.000000000000000000, -1.000000000000000000, -0.000000000000000000 ) ) ;
#18865 = CARTESIAN_POINT ( 'NONE',  ( 12.93207668273189981, 1442.909017868442334, 169.4317201798534711 ) ) ;
#18867 = CARTESIAN_POINT ( 'NONE',  ( -43.50118975519999509, 1443.586702812149952, 263.8966299882980024 ) ) ;
#18866 = DIRECTION ( 'NONE',  ( -1.836970198721029688E-16, -1.000000000000000000, 0.000000000000000000 ) ) ;
#18868 = CARTESIAN_POINT ( 'NONE',  ( 9.393521813728380465, 1435.928492946419965, 209.6064062774240142 ) ) ;
#18869 = CARTESIAN_POINT ( 'NONE',  ( -108.2394657659999950, 1382.219629552339939, 297.9605983755590159 ) ) ;
#18870 = CARTESIAN_POINT ( 'NONE',  ( 24.90812900910000138, 1507.935970732329906, 197.8880224007980075 ) ) ;
#18871 = DIRECTION ( 'NONE',  ( 0.000000000000000000, 0.000000000000000000, -1.000000000000000000 ) ) ;
#18872 = CARTESIAN_POINT ( 'NONE',  ( 8.355631587939999605, 1410.577119414130038, 187.7490234216979843 ) ) ;
#18873 = LINE ( 'NONE', #45785, #60740 ) ;
#18874 = CARTESIAN_POINT ( 'NONE',  ( -7.765022151240000170, 1439.035228022859883, 153.8379896386979908 ) ) ;
#18875 = CARTESIAN_POINT ( 'NONE',  ( 10.92774547339999991, 1436.036448765360092, 151.9134061906980264 ) ) ;
#18876 = CARTESIAN_POINT ( 'NONE',  ( -16.43158050010680071, 1420.644938884899830, 203.2808245233400157 ) ) ;
#18877 = CARTESIAN_POINT ( 'NONE',  ( -8.983165774390000635, 1452.599361326030248, 151.2716590506979912 ) ) ;
#18878 = CARTESIAN_POINT ( 'NONE',  ( 4.873735476160000246, 1472.089320948289924, 218.0431589096889695 ) ) ;
#18879 = ORIENTED_EDGE ( 'NONE', *, *, #101526, .T. ) ;
#18880 = CARTESIAN_POINT ( 'NONE',  ( -2.487921644133310295, 1508.551704408389924, 214.1089243590330113 ) ) ;
#18881 = AXIS2_PLACEMENT_3D ( 'NONE', #35569, #110077, #69764 ) ;
#18882 = CARTESIAN_POINT ( 'NONE',  ( -3.160253207629999839, 1471.445056511090115, 187.3830100966989960 ) ) ;
#18883 = CARTESIAN_POINT ( 'NONE',  ( -40.67651829279999731, 1454.550461609130025, 270.1403828920980459 ) ) ;
#18884 = LINE ( 'NONE', #53082, #80265 ) ;
#18885 = CARTESIAN_POINT ( 'NONE',  ( 17.57263885140000070, 1409.691669004730102, 222.6387591511980020 ) ) ;
#18886 = CARTESIAN_POINT ( 'NONE',  ( -14.60169229409999936, 1463.277005629129917, 223.3429056284980163 ) ) ;
#18887 = ADVANCED_FACE ( 'NONE', ( #66658 ), #110280, .F. ) ;
#18888 = CARTESIAN_POINT ( 'NONE',  ( -110.0634901748029932, 1384.899971912700039, 296.9512050915229793 ) ) ;
#18889 = EDGE_CURVE ( 'NONE', #36972, #45161, #69727, .T. ) ;
#18890 = CARTESIAN_POINT ( 'NONE',  ( 2.925549591967640417, 1409.954410087670112, 231.5402738976679871 ) ) ;
#18891 = CARTESIAN_POINT ( 'NONE',  ( -15.12003195112066933, 1517.051704408389924, 218.5174026476448432 ) ) ;
#18892 = CARTESIAN_POINT ( 'NONE',  ( -4.619855912889999416, 1417.833749415829971, 234.7627619328980018 ) ) ;
#18893 = TOROIDAL_SURFACE ( 'NONE', #83252, 2.000000000000000000, 1.000000000000000000 ) ;
#18894 = CARTESIAN_POINT ( 'NONE',  ( -1.311131513420452421, 1484.544387571488642, 182.3338937980581420 ) ) ;
#18895 = CARTESIAN_POINT ( 'NONE',  ( -2.509563559622638884, 1359.307229891140196, 210.6218459617030021 ) ) ;
#18896 = CARTESIAN_POINT ( 'NONE',  ( -45.24356817553269394, 1434.454005103070131, 268.5215513401200269 ) ) ;
#18897 = CARTESIAN_POINT ( 'NONE',  ( -2.694874838370000081, 1434.191529021039969, 184.8910710316980044 ) ) ;
#18898 = ORIENTED_EDGE ( 'NONE', *, *, #3187, .F. ) ;
#18899 = DIRECTION ( 'NONE',  ( 1.000000000000000000, 0.000000000000000000, 0.000000000000000000 ) ) ;
#18900 = VERTEX_POINT ( 'NONE', #23514 ) ;
#18901 = CARTESIAN_POINT ( 'NONE',  ( -2.284053509485000077, 1516.854133554269993, 210.2586600040969813 ) ) ;
#18902 = CARTESIAN_POINT ( 'NONE',  ( -7.012921583638330070, 1508.551704408389924, 203.6084103760139783 ) ) ;
#18903 = CARTESIAN_POINT ( 'NONE',  ( -17.61781123130856486, 1419.766076753951438, 206.8127147925555960 ) ) ;
#18904 = CARTESIAN_POINT ( 'NONE',  ( 7.069913306463050162, 1426.666554464499995, 213.2414280066960259 ) ) ;
#18905 = CARTESIAN_POINT ( 'NONE',  ( 1.724603976620079804, 1495.787172650469984, 221.3394264603180090 ) ) ;
#18906 = ORIENTED_EDGE ( 'NONE', *, *, #22964, .T. ) ;
#18907 = CARTESIAN_POINT ( 'NONE',  ( 24.33278372090000019, 1437.669624983799849, 213.0855618553079864 ) ) ;
#18909 = CARTESIAN_POINT ( 'NONE',  ( 14.69112492350000032, 1470.808655613429892, 194.6682620091980027 ) ) ;
#18908 = DIRECTION ( 'NONE',  ( 0.4978433412588676998, 0.000000000000000000, -0.8672669759446663962 ) ) ;
#18910 = CARTESIAN_POINT ( 'NONE',  ( 2.251015183664099695, 1487.021489544721135, 219.7028229865901494 ) ) ;
#18911 = DIRECTION ( 'NONE',  ( -1.755985294532469921E-16, 1.000000000000000000, -1.338183447452831989E-16 ) ) ;
#18912 = CARTESIAN_POINT ( 'NONE',  ( 5.346297422500000174, 1473.360741859489963, 218.2967445439789742 ) ) ;
#18913 = CARTESIAN_POINT ( 'NONE',  ( -8.312969881423960317, 1439.013910285169914, 206.4662266169680152 ) ) ;
#18914 = ORIENTED_EDGE ( 'NONE', *, *, #69366, .F. ) ;
#18915 = CARTESIAN_POINT ( 'NONE',  ( -28.49266032979539887, 1415.418434190969947, 270.1377136304399755 ) ) ;
#18916 = CARTESIAN_POINT ( 'NONE',  ( 3.253301381255000013, 1516.790374942449944, 207.9863856151469861 ) ) ;
#18917 = CARTESIAN_POINT ( 'NONE',  ( 8.821431567077510749, 1419.123291530620008, 231.9106426862639978 ) ) ;
#18918 = DIRECTION ( 'NONE',  ( 0.000000000000000000, 0.000000000000000000, 1.000000000000000000 ) ) ;
#18920 = ORIENTED_EDGE ( 'NONE', *, *, #80622, .T. ) ;
#18919 = CARTESIAN_POINT ( 'NONE',  ( -7.706043838548156444, 1365.524518540627469, 208.3718459617061285 ) ) ;
#18921 = ORIENTED_EDGE ( 'NONE', *, *, #14581, .T. ) ;
#18922 = CARTESIAN_POINT ( 'NONE',  ( 13.74310390781900004, 1517.051704408389924, 217.0905615615409943 ) ) ;
#18923 = CARTESIAN_POINT ( 'NONE',  ( -0.5926620228766540377, 1409.870422386290102, 185.1089675646719854 ) ) ;
#18924 = CARTESIAN_POINT ( 'NONE',  ( 3.712429952897377650, 1424.143221639157218, 183.8426287002268964 ) ) ;
#18925 = CARTESIAN_POINT ( 'NONE',  ( -0.02711300940577089993, 1409.107386744810128, 185.7397112177479812 ) ) ;
#18926 = EDGE_CURVE ( 'NONE', #52986, #40123, #57707, .T. ) ;
#18927 = CARTESIAN_POINT ( 'NONE',  ( -20.51079079204400202, 1491.138387813179861, 192.7050494188490006 ) ) ;
#18928 = CARTESIAN_POINT ( 'NONE',  ( -22.98680169079999658, 1425.805257318429994, 213.5345393129279898 ) ) ;
#18929 = CIRCLE ( 'NONE', #99422, 1.999999999999998668 ) ;
#18930 = CARTESIAN_POINT ( 'NONE',  ( 28.46682226171239805, 1468.433058268769855, 268.7218470584510328 ) ) ;
#18931 = CIRCLE ( 'NONE', #31416, 1.999999999999999556 ) ;
#18932 = CARTESIAN_POINT ( 'NONE',  ( -4.819546534003323224, 1466.444145834148230, 234.4964832952103677 ) ) ;
#18933 = CARTESIAN_POINT ( 'NONE',  ( -17.36107116584603105, 1422.621875767651090, 226.5805576276689521 ) ) ;
#18934 = CARTESIAN_POINT ( 'NONE',  ( -2.492443689034999910, 1516.793978928989873, 205.8699571027569846 ) ) ;
#18935 = ADVANCED_FACE ( 'NONE', ( #75050 ), #15102, .F. ) ;
#18936 = VERTEX_POINT ( 'NONE', #16199 ) ;
#18937 = CARTESIAN_POINT ( 'NONE',  ( 31.43069643840505734, 1526.748660780343471, 216.5579808171732736 ) ) ;
#18938 = CARTESIAN_POINT ( 'NONE',  ( 1.511551524885510034, 1460.417055334569795, 183.1515410192469915 ) ) ;
#18939 = CARTESIAN_POINT ( 'NONE',  ( 23.81211169210000378, 1410.396487169730108, 208.4716996890240068 ) ) ;
#18940 = ORIENTED_EDGE ( 'NONE', *, *, #24005, .F. ) ;
#18941 = DIRECTION ( 'NONE',  ( 5.980589973904019347E-17, -1.000000000000000000, 1.736889445713099699E-16 ) ) ;
#18942 = CARTESIAN_POINT ( 'NONE',  ( 24.38835192978790189, 1452.061422661730148, 136.1897709901290057 ) ) ;
#18943 = CARTESIAN_POINT ( 'NONE',  ( 11.08292358395013721, 1424.905641017491462, 138.1229852948969494 ) ) ;
#18944 = CARTESIAN_POINT ( 'NONE',  ( 12.27050434115719924, 1501.509400875670053, 212.4841319041250074 ) ) ;
#18945 = CARTESIAN_POINT ( 'NONE',  ( -13.85129689699811451, 1390.139984326732701, 212.7740231941627655 ) ) ;
#18946 = CARTESIAN_POINT ( 'NONE',  ( 18.50440636980000164, 1410.921881894329772, 194.3442019313980040 ) ) ;
#18947 = CARTESIAN_POINT ( 'NONE',  ( -3.674412922749999755, 1496.836503961589870, 198.4902213705989880 ) ) ;
#18948 = CARTESIAN_POINT ( 'NONE',  ( 2.898851852405722962, 1439.669638370619850, 183.9687869958605404 ) ) ;
#18950 = CARTESIAN_POINT ( 'NONE',  ( -20.51844432163499832, 1427.241484048884786, 221.4774438843884639 ) ) ;
#18949 = CARTESIAN_POINT ( 'NONE',  ( -0.02483722075589999898, 1416.432140559029904, 233.7186305100979951 ) ) ;
#18951 = CARTESIAN_POINT ( 'NONE',  ( 0.3619638413112999387, 1452.022047269289942, 183.1176328467209942 ) ) ;
#18952 = CARTESIAN_POINT ( 'NONE',  ( -0.002537736600710310125, 1508.960873149719873, 179.4060637200210238 ) ) ;
#18953 = CARTESIAN_POINT ( 'NONE',  ( 8.915638207339146248, 1427.583583160426770, 192.9091311759471523 ) ) ;
#18954 = CARTESIAN_POINT ( 'NONE',  ( 2.295485501044999932, 1516.651306816259876, 214.1175719399469983 ) ) ;
#18955 = CARTESIAN_POINT ( 'NONE',  ( 27.31124572860469968, 1446.324645400339932, 137.1901751446029891 ) ) ;
#18956 = ORIENTED_EDGE ( 'NONE', *, *, #75470, .F. ) ;
#18957 = DIRECTION ( 'NONE',  ( 0.01484500364209119690, 0.5669078173028199163, -0.8236474686100957454 ) ) ;
#18958 = CARTESIAN_POINT ( 'NONE',  ( 22.41686883764669602, 1524.667648926078300, 236.2663900491572235 ) ) ;
#18959 = CARTESIAN_POINT ( 'NONE',  ( -0.4878771540074440249, 1409.607344574789977, 232.9569252667809849 ) ) ;
#18960 = CARTESIAN_POINT ( 'NONE',  ( 9816.840209715130186, 50.13405481578730161, 1424.308828391600173 ) ) ;
#18961 =( BOUNDED_CURVE ( )  B_SPLINE_CURVE ( 3, ( #32126, #66311, #100428, #61090 ),
 .UNSPECIFIED., .F., .F. ) 
 B_SPLINE_CURVE_WITH_KNOTS ( ( 4, 4 ),
 ( 4.246412475983603940, 5.177358128112214963 ),
 .UNSPECIFIED. ) 
 CURVE ( )  GEOMETRIC_REPRESENTATION_ITEM ( )  RATIONAL_B_SPLINE_CURVE ( ( 1.000000000000000000, 0.9290729598085936125, 0.9290729598085936125, 1.000000000000000000 ) ) 
 REPRESENTATION_ITEM ( '' )  );
#18962 = CARTESIAN_POINT ( 'NONE',  ( 0.8472549444895222104, 1421.277937719025203, 193.7387945151137387 ) ) ;
#18963 = CARTESIAN_POINT ( 'NONE',  ( -4.329068131567179734, 1515.079329108559932, 207.7116314705500315 ) ) ;
#18964 = CARTESIAN_POINT ( 'NONE',  ( 1.043609643150000005E-14, 1456.909266842430043, 224.8635561844979804 ) ) ;
#18965 = CARTESIAN_POINT ( 'NONE',  ( 36.73763096499994418, 1461.736697325623254, 266.4403429611982119 ) ) ;
#18966 = CARTESIAN_POINT ( 'NONE',  ( -12.31816045095820122, 1378.322797730630100, 209.5997611854560034 ) ) ;
#18967 = CARTESIAN_POINT ( 'NONE',  ( 13.84930592310000108, 1450.388901282120059, 209.1218459616979999 ) ) ;
#18968 = CARTESIAN_POINT ( 'NONE',  ( -9.659452839195818541, 1460.929932477109787, 210.9155389501709976 ) ) ;
#18969 = CARTESIAN_POINT ( 'NONE',  ( -17.00466766660930062, 1420.052239869899950, 201.4977556186619836 ) ) ;
#18970 = CARTESIAN_POINT ( 'NONE',  ( 30.90487439922556945, 1525.907212628473644, 201.8101144455177689 ) ) ;
#18971 = CARTESIAN_POINT ( 'NONE',  ( 9.580287517196040881, 1463.259152023979823, 211.7413480895340001 ) ) ;
#18972 = DIRECTION ( 'NONE',  ( 0.000000000000000000, 1.000000000000000000, 0.000000000000000000 ) ) ;
#18973 = CARTESIAN_POINT ( 'NONE',  ( 8.235306720422707727, 1398.157613047823361, 199.0622384067150108 ) ) ;
#18974 = CARTESIAN_POINT ( 'NONE',  ( 0.04570590800825859862, 1508.911464302090053, 238.4015887634199942 ) ) ;
#18975 = CARTESIAN_POINT ( 'NONE',  ( 22.70805115470000146, 1469.235391016429958, 220.6124962964979943 ) ) ;
#18976 = CARTESIAN_POINT ( 'NONE',  ( -15.75193611358070456, 1420.305119455802014, 210.1813702474818228 ) ) ;
#18977 = CARTESIAN_POINT ( 'NONE',  ( -36.93911630280124569, 1436.285477273010429, 135.0345624054817790 ) ) ;
#18978 = CARTESIAN_POINT ( 'NONE',  ( -33.18021480408270207, 1383.837964353870120, 231.4654556182339888 ) ) ;
#18979 = CARTESIAN_POINT ( 'NONE',  ( 18.46110513727499836, 1471.786120601949960, 195.2229452025129888 ) ) ;
#18980 = CARTESIAN_POINT ( 'NONE',  ( -4.997573825325000385, 1516.742629295279812, 212.5803724681170195 ) ) ;
#18981 = CARTESIAN_POINT ( 'NONE',  ( -2201.413669186790685, 11221.53578756870047, 1941.356037698088358 ) ) ;
#18982 = CARTESIAN_POINT ( 'NONE',  ( 9.132990796547860057, 1451.136122370250177, 210.6042708154840000 ) ) ;
#18984 = ORIENTED_EDGE ( 'NONE', *, *, #72053, .F. ) ;
#18983 = CARTESIAN_POINT ( 'NONE',  ( 3.391831335510000045, 1441.614882265790129, 217.6841840411589999 ) ) ;
#18985 = CARTESIAN_POINT ( 'NONE',  ( -1.121465818060000119, 1416.819759814730105, 228.0845569899979921 ) ) ;
#18986 = CARTESIAN_POINT ( 'NONE',  ( -3.078458355069999985, 1384.494027187519805, 199.6978503428690033 ) ) ;
#18987 = CARTESIAN_POINT ( 'NONE',  ( -27.33784579440922613, 1509.867718998758846, 219.6686939752406147 ) ) ;
#18989 = ORIENTED_EDGE ( 'NONE', *, *, #57733, .F. ) ;
#18988 = CARTESIAN_POINT ( 'NONE',  ( -34.34692909063059574, 1451.701922534410187, 134.0999999981429767 ) ) ;
#18990 = CARTESIAN_POINT ( 'NONE',  ( -4.098986974010339956, 1508.551704408389924, 219.8451935736590031 ) ) ;
#18991 = ORIENTED_EDGE ( 'NONE', *, *, #25313, .F. ) ;
#18992 = CARTESIAN_POINT ( 'NONE',  ( -14.53473304376390018, 1379.710786975620067, 208.2794084638009906 ) ) ;
#18993 = CARTESIAN_POINT ( 'NONE',  ( -16.02395347670000447, 1414.971262582530017, 214.1105671929480252 ) ) ;
#18994 = FACE_OUTER_BOUND ( 'NONE', #20016, .T. ) ;
#18995 = DIRECTION ( 'NONE',  ( -0.0003696129300649848913, 0.001489947244085779296, -0.9999988217210517005 ) ) ;
#18996 = CARTESIAN_POINT ( 'NONE',  ( -4.993214567250789493, 1391.653935164599716, 214.7089805434449943 ) ) ;
#18997 = CARTESIAN_POINT ( 'NONE',  ( -10.67674005382819935, 1471.688487720359944, 206.9114804947679715 ) ) ;
#18998 = CARTESIAN_POINT ( 'NONE',  ( 13.92362594963720035, 1409.399284119610229, 203.7196187947509998 ) ) ;
#18999 = CARTESIAN_POINT ( 'NONE',  ( -12.32169104970000006, 1391.303891397440111, 206.9552536725390155 ) ) ;
#19000 = CARTESIAN_POINT ( 'NONE',  ( -89.80898548959270045, 1385.192144560830002, 292.4574326567000639 ) ) ;
#19001 = CARTESIAN_POINT ( 'NONE',  ( -17.83186546889999846, 1421.470479459229864, 192.3242510227980233 ) ) ;
#19002 = CARTESIAN_POINT ( 'NONE',  ( -66.55629426049999608, 1379.749035308849898, 275.7365325667589673 ) ) ;
#19003 = ORIENTED_EDGE ( 'NONE', *, *, #72271, .F. ) ;
#19004 = CARTESIAN_POINT ( 'NONE',  ( 10.83651939265710062, 1490.169899907720037, 207.5021329017099845 ) ) ;
#19006 = ORIENTED_EDGE ( 'NONE', *, *, #53892, .F. ) ;
#19005 = CARTESIAN_POINT ( 'NONE',  ( -1.023515647982950139, 1438.105133628250087, 227.6662252542259921 ) ) ;
#19007 = CARTESIAN_POINT ( 'NONE',  ( 8.729347899703789437, 1465.224243514420095, 213.7259074896789741 ) ) ;
#19008 = ORIENTED_EDGE ( 'NONE', *, *, #14869, .F. ) ;
#19009 = CARTESIAN_POINT ( 'NONE',  ( 25.61065848249999988, 1508.555233516829958, 218.7406679075980094 ) ) ;
#19010 = CARTESIAN_POINT ( 'NONE',  ( 1.748848150589999983, 1360.440694539920059, 207.6218459616989946 ) ) ;
#19011 = CARTESIAN_POINT ( 'NONE',  ( -11.97796580090000162, 1433.627075391659901, 150.2895221116980053 ) ) ;
#19012 = CARTESIAN_POINT ( 'NONE',  ( 29.43805146511517279, 1509.956782691962644, 212.2118635277215901 ) ) ;
#19013 = DIRECTION ( 'NONE',  ( 0.7074300732573276518, 0.02470400251971152997, -0.7063514732133275853 ) ) ;
#19014 = CARTESIAN_POINT ( 'NONE',  ( -27.93158978740000009, 1508.017348977630036, 210.2982006691480024 ) ) ;
#19015 = CARTESIAN_POINT ( 'NONE',  ( 31.81424859195960408, 1524.964230758883104, 201.5864201284566093 ) ) ;
#19016 = CARTESIAN_POINT ( 'NONE',  ( 3.601841467080000303, 1444.840595811589992, 200.9001250664390170 ) ) ;
#19017 = CARTESIAN_POINT ( 'NONE',  ( -0.5328017128810000891, 1467.450758361530006, 182.6307715436979890 ) ) ;
#19018 = CARTESIAN_POINT ( 'NONE',  ( -4.955698549128424446, 1370.907435100005841, 209.6218459617033432 ) ) ;
#19019 = DIRECTION ( 'NONE',  ( 0.000000000000000000, 0.000000000000000000, -1.000000000000000000 ) ) ;
#19020 = B_SPLINE_CURVE_WITH_KNOTS ( 'NONE', 3,
 ( #82819, #7227, #5011, #22889, #64944, #15588 ),
 .UNSPECIFIED., .F., .F.,
 ( 4, 2, 4 ),
 ( 1.358608016385320016E-06, 0.01184128846600049877, 0.02355710845665270198 ),
 .UNSPECIFIED. ) ;
#19021 = CARTESIAN_POINT ( 'NONE',  ( 2.500000000000000000, 1448.210448409899982, 182.3842139592889851 ) ) ;
#19022 = CARTESIAN_POINT ( 'NONE',  ( -2.881548462575000080, 1516.909589401870107, 206.8382752989369919 ) ) ;
#19023 = CARTESIAN_POINT ( 'NONE',  ( -12.99004886546730120, 1434.775507592019949, 149.1620289331810056 ) ) ;
#19024 = CARTESIAN_POINT ( 'NONE',  ( -2.500000000000000000, 1432.593627935599898, 157.5021872924980073 ) ) ;
#19025 = CARTESIAN_POINT ( 'NONE',  ( -0.3657622740145609619, 1430.070695917230069, 190.4861624611909861 ) ) ;
#19027 = ORIENTED_EDGE ( 'NONE', *, *, #55436, .T. ) ;
#19026 = CARTESIAN_POINT ( 'NONE',  ( -3.237583812329999589, 1495.897743034890027, 219.8603346627990049 ) ) ;
#19028 = VECTOR ( 'NONE', #19737, 1000.000000000000000 ) ;
#19029 = DIRECTION ( 'NONE',  ( 1.000000000000000000, 0.000000000000000000, -0.000000000000000000 ) ) ;
#19030 = ORIENTED_EDGE ( 'NONE', *, *, #19541, .T. ) ;
#19031 = EDGE_CURVE ( 'NONE', #38120, #61362, #49677, .T. ) ;
#19032 = CARTESIAN_POINT ( 'NONE',  ( 39.02581916309999599, 1422.344273220830019, 266.4771548496979676 ) ) ;
#19033 = CARTESIAN_POINT ( 'NONE',  ( -25.92853884490000027, 1469.242862528429896, 205.7879372785779992 ) ) ;
#19035 = CARTESIAN_POINT ( 'NONE',  ( 16.44149578104170217, 1409.512336796159843, 193.0768534555940050 ) ) ;
#19034 = CARTESIAN_POINT ( 'NONE',  ( -10.03650023711350059, 1425.202651915989918, 96.73419986872309551 ) ) ;
#19036 = CARTESIAN_POINT ( 'NONE',  ( -0.7353365779029981120, 1516.995911393979895, 212.0011643880069698 ) ) ;
#19037 = CARTESIAN_POINT ( 'NONE',  ( -20.50343491230000126, 1453.154616238729886, 208.2124688364239944 ) ) ;
#19038 = CARTESIAN_POINT ( 'NONE',  ( -30.53571888280000124, 1438.952188671489921, 240.1260121775979997 ) ) ;
#19039 = CARTESIAN_POINT ( 'NONE',  ( -12.79475420062619939, 1379.177177335730221, 208.7218844242719911 ) ) ;
#19040 = CARTESIAN_POINT ( 'NONE',  ( 28.30911832997569988, 1508.554176139660058, 209.4091768886380294 ) ) ;
#19041 = EDGE_CURVE ( 'NONE', #59250, #36202, #54904, .T. ) ;
#19042 = CARTESIAN_POINT ( 'NONE',  ( 3.262929297844129994, 1508.551704408389924, 213.9871752814069907 ) ) ;
#19043 = CARTESIAN_POINT ( 'NONE',  ( 30.80316601989999725, 1450.549250348119813, 136.3368496048979921 ) ) ;
#19044 = EDGE_LOOP ( 'NONE', ( #29142, #88899, #101538, #84657 ) ) ;
#19045 = CARTESIAN_POINT ( 'NONE',  ( 9.185964335410000459, 1396.233841330429868, 201.6855590868979675 ) ) ;
#19046 = CARTESIAN_POINT ( 'NONE',  ( 9.591489393450858714, 1462.438986607349989, 207.3792329919180020 ) ) ;
#19047 = CARTESIAN_POINT ( 'NONE',  ( -17.47006112300000069, 1460.511276975630153, 228.2420954910980129 ) ) ;
#19048 = EDGE_LOOP ( 'NONE', ( #25127, #64280, #110526, #103040 ) ) ;
#19049 = ORIENTED_EDGE ( 'NONE', *, *, #84679, .T. ) ;
#19050 = CARTESIAN_POINT ( 'NONE',  ( 9.699673965497980888, 1453.359162548709946, 212.1674369800300042 ) ) ;
#19051 = CARTESIAN_POINT ( 'NONE',  ( 8.472418160909999330, 1423.407106218679928, 196.2202384860989923 ) ) ;
#19052 = ORIENTED_EDGE ( 'NONE', *, *, #26725, .T. ) ;
#19053 = CARTESIAN_POINT ( 'NONE',  ( -0.3142596228660000102, 1415.641189163630088, 184.7630716501980146 ) ) ;
#19054 = CARTESIAN_POINT ( 'NONE',  ( 8.950554794200915154, 1446.632273707716877, 153.7528715246174329 ) ) ;
#19055 = CARTESIAN_POINT ( 'NONE',  ( -0.1822331536658439999, 1415.403647183765997, 233.4419826045449611 ) ) ;
#19056 = CARTESIAN_POINT ( 'NONE',  ( -7.167074599660000267, 1461.188551261529938, 233.4299114769979724 ) ) ;
#19057 = DIRECTION ( 'NONE',  ( -0.9995237720558002303, 0.03085820952913055637, 3.241389442709986064E-08 ) ) ;
#19058 = CARTESIAN_POINT ( 'NONE',  ( 9.723778708192279296, 1452.046992748000093, 209.3441726741959883 ) ) ;
#19059 = CARTESIAN_POINT ( 'NONE',  ( 6.483588104269999874, 1462.707724100489941, 208.1814389384059893 ) ) ;
#19060 = CARTESIAN_POINT ( 'NONE',  ( 14.23687710369999948, 1463.789345363929897, 224.3885670368980243 ) ) ;
#19061 = ORIENTED_EDGE ( 'NONE', *, *, #10390, .F. ) ;
#19062 = CARTESIAN_POINT ( 'NONE',  ( 7.328049280255000575, 1516.809497469189864, 202.5664528150769854 ) ) ;
#19063 = CARTESIAN_POINT ( 'NONE',  ( 2.299667965875000331, 1516.965971551240045, 210.2399506998270056 ) ) ;
#19064 = ORIENTED_EDGE ( 'NONE', *, *, #51675, .T. ) ;
#19065 = CARTESIAN_POINT ( 'NONE',  ( 11.82848250736780038, 1429.808088084610063, 149.3741360895739660 ) ) ;
#19066 = B_SPLINE_CURVE_WITH_KNOTS ( 'NONE', 3,
 ( #50998, #41495, #103024, #68368, #77306, #8416 ),
 .UNSPECIFIED., .F., .F.,
 ( 4, 2, 4 ),
 ( -0.1558933150621664987, -0.07794925273348111971, -6.503526063517117706E-07 ),
 .UNSPECIFIED. ) ;
#19067 = CARTESIAN_POINT ( 'NONE',  ( 13.11038924667559336, 1444.793296087265162, 187.1321005147183882 ) ) ;
#19068 = EDGE_LOOP ( 'NONE', ( #21012, #11244, #59704 ) ) ;
#19069 = CARTESIAN_POINT ( 'NONE',  ( -15.62937150226415994, 1506.527232289704898, 193.5520135464122973 ) ) ;
#19070 = CARTESIAN_POINT ( 'NONE',  ( -13.51702042466202158, 1443.913060387330461, 169.3754641244113373 ) ) ;
#19071 = CARTESIAN_POINT ( 'NONE',  ( 2.883855425570000186, 1507.998768052829973, 236.1595088610979758 ) ) ;
#19072 = CARTESIAN_POINT ( 'NONE',  ( -10.13006551440279956, 1470.128316028900144, 213.2258428534270251 ) ) ;
#19073 = CARTESIAN_POINT ( 'NONE',  ( -5.638178009059999773, 1424.929087014930019, 186.4582126495980106 ) ) ;
#19074 = CARTESIAN_POINT ( 'NONE',  ( 0.9815367246191329942, 1408.241645913789853, 270.3924816116769989 ) ) ;
#19075 = CARTESIAN_POINT ( 'NONE',  ( -5.599233173528683771, 1387.285800435509827, 209.1218459616989946 ) ) ;
#19076 = CARTESIAN_POINT ( 'NONE',  ( -12.52558728303339919, 1501.938162216189994, 211.4646196275029979 ) ) ;
#19077 = CARTESIAN_POINT ( 'NONE',  ( -2.206411215550580174, 1421.659913175079964, 193.5263021252320073 ) ) ;
#19078 = CARTESIAN_POINT ( 'NONE',  ( -32.57298063980000080, 1379.681802635260055, 216.0596865545890068 ) ) ;
#19079 = CARTESIAN_POINT ( 'NONE',  ( 9.475903704820970219, 1425.358992633405023, 195.5313119463182829 ) ) ;
#19081 = CARTESIAN_POINT ( 'NONE',  ( -15.72751745975079984, 1517.151704408390060, 211.3620530696679793 ) ) ;
#19080 = CARTESIAN_POINT ( 'NONE',  ( -17.46895492501760216, 1435.758675877850010, 191.0377360153560176 ) ) ;
#19082 = CARTESIAN_POINT ( 'NONE',  ( -68.47067290995560995, 1379.747730938292307, 280.0399411559841951 ) ) ;
#19083 = B_SPLINE_CURVE_WITH_KNOTS ( 'NONE', 3,
 ( #29983, #48474, #40048, #64734, #98848, #74230 ),
 .UNSPECIFIED., .F., .F.,
 ( 4, 2, 4 ),
 ( 0.000000000000000000, 0.1289624413956479976, 0.2573965581621350251 ),
 .UNSPECIFIED. ) ;
#19084 = CARTESIAN_POINT ( 'NONE',  ( -9.946277618806290022, 1439.610876520569946, 208.1166930489989966 ) ) ;
#19085 = CARTESIAN_POINT ( 'NONE',  ( -8.038901823954999415, 1514.330398624140116, 202.2117929003169934 ) ) ;
#19086 = ORIENTED_EDGE ( 'NONE', *, *, #3822, .F. ) ;
#19087 = CARTESIAN_POINT ( 'NONE',  ( 1.199040866600000048E-14, 1420.418457356630142, 243.9198229339980060 ) ) ;
#19088 = CARTESIAN_POINT ( 'NONE',  ( 13.34704934129999998, 1434.912633013909954, 148.9126644935979868 ) ) ;
#19089 = AXIS2_PLACEMENT_3D ( 'NONE', #86222, #10633, #85661 ) ;
#19090 = CARTESIAN_POINT ( 'NONE',  ( -18.19590854886883236, 1522.644714754858114, 180.0410247165304156 ) ) ;
#19091 = CARTESIAN_POINT ( 'NONE',  ( -7.965680540240001051, 1384.926148861439970, 199.4891222871690104 ) ) ;
#19092 = DIRECTION ( 'NONE',  ( -0.1070030146457508768, 0.000000000000000000, -0.9942586961433735881 ) ) ;
#19094 = ORIENTED_EDGE ( 'NONE', *, *, #54225, .F. ) ;
#19093 = CARTESIAN_POINT ( 'NONE',  ( 0.01406703362208180062, 1515.158574431529814, 204.7948529419429917 ) ) ;
#19095 = CARTESIAN_POINT ( 'NONE',  ( -16.62146796077700017, 1418.479381249660037, 203.0020891297729975 ) ) ;
#19096 = CARTESIAN_POINT ( 'NONE',  ( 2.719262146893400038E-32, 1524.051704408389924, 209.1218459616989946 ) ) ;
#19097 = CARTESIAN_POINT ( 'NONE',  ( -2.500574544111449971, 1448.942056179399970, 154.5733147259969940 ) ) ;
#19098 = CARTESIAN_POINT ( 'NONE',  ( -2.182355088989220260, 1429.366333297759866, 200.0022119995389858 ) ) ;
#19099 = CARTESIAN_POINT ( 'NONE',  ( 2.717866887673947129, 1443.364948805944778, 217.6365403981836835 ) ) ;
#19100 = CARTESIAN_POINT ( 'NONE',  ( -7.291666587149999934, 1441.356683820160015, 185.8290540692979960 ) ) ;
#19101 = CARTESIAN_POINT ( 'NONE',  ( 30.96823826980000050, 1510.122676044730042, 207.2974432662780089 ) ) ;
#19102 = CARTESIAN_POINT ( 'NONE',  ( 8.788316489185000080, 1511.741868877540128, 202.8695794779170001 ) ) ;
#19103 = CARTESIAN_POINT ( 'NONE',  ( -7.612906430609999830, 1431.113060387329824, 226.5499313142980213 ) ) ;
#19104 = CARTESIAN_POINT ( 'NONE',  ( 16.51790355380000008, 1415.090637380430053, 226.7996615004980185 ) ) ;
#19105 = CARTESIAN_POINT ( 'NONE',  ( -4.524029051260000323, 1475.733900273690097, 218.4636560311490143 ) ) ;
#19106 = CARTESIAN_POINT ( 'NONE',  ( 543.1695162809550084, 1433.553134552160145, 209.1604895367889867 ) ) ;
#19107 = CARTESIAN_POINT ( 'NONE',  ( 4.995994787574999485, 1516.665179208830068, 206.6322283937570035 ) ) ;
#19108 = CARTESIAN_POINT ( 'NONE',  ( 41.61237968540000054, 1425.046497863630066, 267.7539489489980156 ) ) ;
#19109 = CIRCLE ( 'NONE', #106724, 783.3212999198779016 ) ;
#19110 = CARTESIAN_POINT ( 'NONE',  ( -33.05665451062209570, 1523.390106123591067, 217.3123061710364254 ) ) ;
#19111 = CARTESIAN_POINT ( 'NONE',  ( 15.39963790060000015, 1435.849252446450009, 149.2652977341979863 ) ) ;
#19112 = CARTESIAN_POINT ( 'NONE',  ( 26.00771452189999877, 1488.579595437629905, 206.3082675595479998 ) ) ;
#19113 = CARTESIAN_POINT ( 'NONE',  ( 20.19282076750571875, 1506.569407721386142, 218.0946391673573999 ) ) ;
#19114 = CARTESIAN_POINT ( 'NONE',  ( -12.31752474539220010, 1377.944612774040024, 209.1221336184720201 ) ) ;
#19116 = EDGE_CURVE ( 'NONE', #10824, #50393, #10201, .T. ) ;
#19115 = CYLINDRICAL_SURFACE ( 'NONE', #69409, 4.000000000000006217 ) ;
#19117 = CARTESIAN_POINT ( 'NONE',  ( -40.27244786589999848, 1443.155312786579998, 137.0624732611979937 ) ) ;
#19118 = CARTESIAN_POINT ( 'NONE',  ( -20.00077709783896296, 1506.539416727680191, 199.7857358250231812 ) ) ;
#19119 = FACE_OUTER_BOUND ( 'NONE', #84798, .T. ) ;
#19120 = CARTESIAN_POINT ( 'NONE',  ( -14.29155582609999975, 1442.454908126789860, 188.8169266407979876 ) ) ;
#19121 = EDGE_CURVE ( 'NONE', #71944, #37474, #3321, .T. ) ;
#19122 = LINE ( 'NONE', #63394, #56925 ) ;
#19123 = EDGE_CURVE ( 'NONE', #90525, #94930, #6805, .T. ) ;
#19124 = CARTESIAN_POINT ( 'NONE',  ( -33.15527080879999744, 1435.815762631380039, 135.9678225143980228 ) ) ;
#19125 = ORIENTED_EDGE ( 'NONE', *, *, #96302, .T. ) ;
#19126 = CARTESIAN_POINT ( 'NONE',  ( -2.234922686965000516, 1512.341036949130057, 201.5226187864570022 ) ) ;
#19127 = CARTESIAN_POINT ( 'NONE',  ( -13.73196314922649819, 1409.392591107120097, 203.2471964003619860 ) ) ;
#19128 = CARTESIAN_POINT ( 'NONE',  ( -5.519888651039999594, 1440.499828209809948, 154.7645161259980000 ) ) ;
#19129 = CARTESIAN_POINT ( 'NONE',  ( 21.38516915557987375, 1524.726013923371056, 237.8497028174237755 ) ) ;
#19130 = CARTESIAN_POINT ( 'NONE',  ( -46.02998506200000151, 1446.027519629539938, 268.4959083590979958 ) ) ;
#19131 = CARTESIAN_POINT ( 'NONE',  ( -13.53916864874639892, 1429.119333790580185, 222.2883575635510169 ) ) ;
#19132 = CARTESIAN_POINT ( 'NONE',  ( 0.2192322612154889994, 1419.698823279740054, 184.2916502271359889 ) ) ;
#19133 = CARTESIAN_POINT ( 'NONE',  ( -72.07271172023830275, 1384.656943536320114, 297.2850582096680228 ) ) ;
#19134 = CARTESIAN_POINT ( 'NONE',  ( -44.54400286966450295, 1385.001782504770063, 217.7620875069719943 ) ) ;
#19135 = CARTESIAN_POINT ( 'NONE',  ( 17.84384396026800346, 1424.152973260369890, 226.0594126201679899 ) ) ;
#19136 = CARTESIAN_POINT ( 'NONE',  ( 20.86062014670000409, 1508.959785424030088, 227.7205171458979862 ) ) ;
#19137 = CARTESIAN_POINT ( 'NONE',  ( 14.71289468370000009, 1474.176701919529933, 223.5077687996979989 ) ) ;
#19138 = CARTESIAN_POINT ( 'NONE',  ( -19.53786426058999481, 1512.187213306747481, 237.7197124308268030 ) ) ;
#19139 = CARTESIAN_POINT ( 'NONE',  ( 4.327507230410000183, 1515.138937518789817, 208.4081006986280045 ) ) ;
#19140 = CARTESIAN_POINT ( 'NONE',  ( -8.604576571519999106, 1384.925122429579915, 199.8686409562490098 ) ) ;
#19141 = DIRECTION ( 'NONE',  ( 0.003573437736329575058, 0.9999913661844080925, 0.002120872317184724874 ) ) ;
#19142 = CARTESIAN_POINT ( 'NONE',  ( 16.09868664480000078, 1415.425582719929707, 201.5601952599979825 ) ) ;
#19143 = CARTESIAN_POINT ( 'NONE',  ( 11.21638122688047190, 1413.913060387330006, 209.8266014933971064 ) ) ;
#19144 = CARTESIAN_POINT ( 'NONE',  ( 3.327063897169999507, 1422.406709332250102, 194.0529592594990049 ) ) ;
#19145 = CARTESIAN_POINT ( 'NONE',  ( 23.41884693540000129, 1409.895416813330030, 210.0743532913309934 ) ) ;
#19146 = CARTESIAN_POINT ( 'NONE',  ( -106.9772147180469943, 1391.913060387289988, 306.6383769938329920 ) ) ;
#19147 = CARTESIAN_POINT ( 'NONE',  ( 19.08743583839999758, 1460.091080419490027, 220.2973930160990221 ) ) ;
#19148 = CARTESIAN_POINT ( 'NONE',  ( -5.359938512223240359, 1422.303815611070149, 145.5146526691499673 ) ) ;
#19150 = CARTESIAN_POINT ( 'NONE',  ( -8.395462917950000659, 1384.396045361419965, 199.8129348554689955 ) ) ;
#19149 = LINE ( 'NONE', #46061, #47885 ) ;
#19151 = CARTESIAN_POINT ( 'NONE',  ( -5.156154518200000147, 1391.908488942590111, 203.6345722630290140 ) ) ;
#19152 = CARTESIAN_POINT ( 'NONE',  ( 0.000000000000000000, 1523.382868172864164, 209.1218459616979999 ) ) ;
#19153 = CARTESIAN_POINT ( 'NONE',  ( -11.63492915560000007, 1490.028483917189988, 211.0527168509590012 ) ) ;
#19154 = CARTESIAN_POINT ( 'NONE',  ( 2.986193535308999891, 1369.126893976419979, 209.1220808601199792 ) ) ;
#19155 = AXIS2_PLACEMENT_3D ( 'NONE', #14572, #73401, #107539 ) ;
#19156 = CARTESIAN_POINT ( 'NONE',  ( -9.692061980449999226, 1363.802329763670059, 210.6218459616991936 ) ) ;
#19157 = CARTESIAN_POINT ( 'NONE',  ( -6.947377821305000367, 1517.009964551830080, 204.5062011277169916 ) ) ;
#19158 = CARTESIAN_POINT ( 'NONE',  ( -15.52565719226596741, 1421.385870312634552, 199.5589395028577542 ) ) ;
#19159 = CARTESIAN_POINT ( 'NONE',  ( -14.11689929294730028, 1484.918870904669802, 186.6450022189229969 ) ) ;
#19160 = PRESENTATION_STYLE_ASSIGNMENT (( #85841 ) ) ;
#19161 = CARTESIAN_POINT ( 'NONE',  ( -14.46094609940118758, 1420.539308687509902, 213.8039270598953863 ) ) ;
#19164 = ORIENTED_EDGE ( 'NONE', *, *, #14562, .F. ) ;
#19163 = CARTESIAN_POINT ( 'NONE',  ( -62.71435643260001314, 1379.746901600850151, 270.6043089134589650 ) ) ;
#19162 = CONICAL_SURFACE ( 'NONE', #81755, 1.000000000000007327, 0.7853981633970000820 ) ;
#19165 = ORIENTED_EDGE ( 'NONE', *, *, #19541, .F. ) ;
#19166 = CARTESIAN_POINT ( 'NONE',  ( 11.94269759412389931, 1433.497490334299755, 149.9951721422179958 ) ) ;
#19167 = CARTESIAN_POINT ( 'NONE',  ( 21.75647715750188738, 1524.201816949777594, 183.4206492032029416 ) ) ;
#19168 = ORIENTED_EDGE ( 'NONE', *, *, #10427, .T. ) ;
#19169 = CARTESIAN_POINT ( 'NONE',  ( -2.354624258718260421, 1456.603527532422959, 199.9289168914013715 ) ) ;
#19170 = CARTESIAN_POINT ( 'NONE',  ( 10.92766316470000021, 1501.618322990889965, 205.6861136852989773 ) ) ;
#19172 = CARTESIAN_POINT ( 'NONE',  ( 11.59417695439999996, 1428.981093279630159, 133.6118001900980232 ) ) ;
#19171 = DIRECTION ( 'NONE',  ( -0.9991156138703695122, 0.000000000000000000, 0.04204747460234692369 ) ) ;
#19173 = CARTESIAN_POINT ( 'NONE',  ( 11.98890328080000067, 1442.756953654919926, 147.5994355510979688 ) ) ;
#19174 = CARTESIAN_POINT ( 'NONE',  ( -24.07333629580420009, 1452.056479083659951, 137.0861003737580006 ) ) ;
#19175 = CARTESIAN_POINT ( 'NONE',  ( -0.2202020877210009997, 1467.752737336390055, 219.8452965410990032 ) ) ;
#19176 = CARTESIAN_POINT ( 'NONE',  ( 16.40118808329999922, 1409.652464304430168, 226.0181115163979939 ) ) ;
#19177 = EDGE_CURVE ( 'NONE', #93667, #85148, #86937, .T. ) ;
#19178 = SURFACE_STYLE_FILL_AREA ( #70212 ) ;
#19179 = CARTESIAN_POINT ( 'NONE',  ( 5.786837678925000006, 1517.040132827679827, 212.3790665729270017 ) ) ;
#19180 = CARTESIAN_POINT ( 'NONE',  ( 13.64809019993819916, 1415.124054205840139, 197.6749129713249999 ) ) ;
#19181 = LINE ( 'NONE', #1319, #73331 ) ;
#19182 = DIRECTION ( 'NONE',  ( -0.03489951250832355745, 0.9993908264671441666, -5.513386024302311512E-10 ) ) ;
#19183 = ORIENTED_EDGE ( 'NONE', *, *, #66731, .T. ) ;
#19184 = CARTESIAN_POINT ( 'NONE',  ( 14.24850174863960106, 1435.298499589599942, 149.3936294197170014 ) ) ;
#19185 = CARTESIAN_POINT ( 'NONE',  ( 1.110979151289160027, 1432.780184589570126, 200.7448731778110016 ) ) ;
#19186 = ORIENTED_EDGE ( 'NONE', *, *, #59143, .T. ) ;
#19187 = ORIENTED_EDGE ( 'NONE', *, *, #21439, .T. ) ;
#19188 = ORIENTED_EDGE ( 'NONE', *, *, #63496, .F. ) ;
#19189 = CARTESIAN_POINT ( 'NONE',  ( -8.371228039894999640, 1512.069761553110084, 215.5056669251370067 ) ) ;
#19190 = CARTESIAN_POINT ( 'NONE',  ( -0.5359129219849999570, 1465.001496343030112, 237.3400905133979961 ) ) ;
#19191 = CARTESIAN_POINT ( 'NONE',  ( 7.885142363431777213, 1451.393272216873129, 152.9790937285441714 ) ) ;
#19192 = AXIS2_PLACEMENT_3D ( 'NONE', #5633, #106435, #55497 ) ;
#19193 = CARTESIAN_POINT ( 'NONE',  ( -3.744257397248767383, 1509.032015221108395, 204.8809009245644859 ) ) ;
#19194 = CARTESIAN_POINT ( 'NONE',  ( 10.96046450149999885, 1461.176790603689824, 209.3104301672979943 ) ) ;
#19195 = B_SPLINE_CURVE_WITH_KNOTS ( 'NONE', 3,
 ( #15303, #10091, #41634, #1719, #44265, #18466, #50589, #95205, #74697, #108829 ),
 .UNSPECIFIED., .F., .F.,
 ( 4, 2, 2, 2, 4 ),
 ( -2.293181918888250070, -1.719760621652620003, -1.147337202555609892, -0.5730822307304319629, 0.000000000000000000 ),
 .UNSPECIFIED. ) ;
#19196 = CARTESIAN_POINT ( 'NONE',  ( -16.68699431115342335, 1449.695428686811283, 220.1589770093310676 ) ) ;
#19197 = CARTESIAN_POINT ( 'NONE',  ( -41.28229943905566302, 1379.658502791898627, 225.0653720194143546 ) ) ;
#19198 = CARTESIAN_POINT ( 'NONE',  ( 2.360870863690000210, 1465.193912104189849, 199.3990268566589918 ) ) ;
#19199 = CARTESIAN_POINT ( 'NONE',  ( 8.632911994995870586, 1437.313349126720141, 208.5977050715380017 ) ) ;
#19200 = ORIENTED_EDGE ( 'NONE', *, *, #71307, .T. ) ;
#19201 = CARTESIAN_POINT ( 'NONE',  ( 4.995725969715000048, 1516.651306816259876, 206.8263604310569690 ) ) ;
#19202 = ORIENTED_EDGE ( 'NONE', *, *, #92766, .F. ) ;
#19203 = CARTESIAN_POINT ( 'NONE',  ( 28.38347306510890178, 1440.913060387330006, 248.5147831249649926 ) ) ;
#19204 = CARTESIAN_POINT ( 'NONE',  ( -19.49656203970000234, 1509.532970918229921, 187.1097474216979890 ) ) ;
#19205 = ORIENTED_EDGE ( 'NONE', *, *, #20010, .F. ) ;
#19206 = CARTESIAN_POINT ( 'NONE',  ( 26.18878121679949800, 1448.069869514440143, 137.2982896685190042 ) ) ;
#19207 = CARTESIAN_POINT ( 'NONE',  ( -14.04658979979999955, 1410.336061500830056, 190.2513870978979753 ) ) ;
#19208 = CARTESIAN_POINT ( 'NONE',  ( -29.09816620510556362, 1379.626347181600977, 217.7851320636372918 ) ) ;
#19209 = CARTESIAN_POINT ( 'NONE',  ( -24.36525012050000072, 1441.101273928379896, 211.6948751338080115 ) ) ;
#19210 = FACE_OUTER_BOUND ( 'NONE', #22478, .T. ) ;
#19211 = DIRECTION ( 'NONE',  ( 0.8090169943749465631, 0.000000000000000000, -0.5877852522924742473 ) ) ;
#19212 = FACE_OUTER_BOUND ( 'NONE', #1337, .T. ) ;
#19213 = CARTESIAN_POINT ( 'NONE',  ( -11.87905392670000104, 1433.311775745339901, 149.9804763677979906 ) ) ;
#19215 = EDGE_CURVE ( 'NONE', #9928, #99690, #67463, .T. ) ;
#19214 = CARTESIAN_POINT ( 'NONE',  ( -6.255913365080000510, 1508.980388112989885, 219.5104367483990018 ) ) ;
#19217 = CARTESIAN_POINT ( 'NONE',  ( 5.521731335039999244, 1437.871055919089940, 209.1877786888699973 ) ) ;
#19216 = CARTESIAN_POINT ( 'NONE',  ( 2.902343019699999971, 1466.632250434329762, 234.1422827139980143 ) ) ;
#19218 = AXIS2_PLACEMENT_3D ( 'NONE', #15937, #32218, #66398 ) ;
#19219 = CARTESIAN_POINT ( 'NONE',  ( -1.121950782074999875, 1517.123342927159911, 214.1352753262870010 ) ) ;
#19220 = CARTESIAN_POINT ( 'NONE',  ( 1.600144450079999947, 1468.978733938389951, 216.2351156805190158 ) ) ;
#19221 = LINE ( 'NONE', #55085, #98253 ) ;
#19222 = CARTESIAN_POINT ( 'NONE',  ( 30.87183381296008022, 1524.816846803860926, 221.7488379675505143 ) ) ;
#19223 = CARTESIAN_POINT ( 'NONE',  ( -4.027697264044999947, 1516.766397346390022, 212.0005392193770035 ) ) ;
#19224 = CARTESIAN_POINT ( 'NONE',  ( -18.89028803260000089, 1434.820761660239896, 209.2076715186949798 ) ) ;
#19225 = CARTESIAN_POINT ( 'NONE',  ( -18.14293122912915734, 1486.179943799410239, 188.5917708767873933 ) ) ;
#19227 = EDGE_LOOP ( 'NONE', ( #3222, #85696 ) ) ;
#19226 = CARTESIAN_POINT ( 'NONE',  ( -81.17886098919998972, 1384.990453609069846, 304.9592558327589700 ) ) ;
#19228 = CARTESIAN_POINT ( 'NONE',  ( -17.26793975759867550, 1525.730671948510917, 236.6572836587323536 ) ) ;
#19229 = CARTESIAN_POINT ( 'NONE',  ( 26.01655159059999889, 1446.111954671009926, 225.7845402501980061 ) ) ;
#19230 = CARTESIAN_POINT ( 'NONE',  ( -18.92249268369999982, 1456.941604937630018, 229.2980728310979828 ) ) ;
#19231 = CARTESIAN_POINT ( 'NONE',  ( -29.11400471147480218, 1509.929743834820101, 212.8719597320529999 ) ) ;
#19232 = CARTESIAN_POINT ( 'NONE',  ( -6.887159582019999782, 1508.131488034229960, 235.9161536093979805 ) ) ;
#19233 = CARTESIAN_POINT ( 'NONE',  ( -22.76393692040000261, 1450.407194713350009, 220.5314342330980253 ) ) ;
#19234 = CIRCLE ( 'NONE', #28216, 1.999999999999998668 ) ;
#19236 = CARTESIAN_POINT ( 'NONE',  ( 16.87240902346729854, 1409.502257893559772, 222.1138755377239988 ) ) ;
#19235 = CARTESIAN_POINT ( 'NONE',  ( -21.10174429543511110, 1411.010612129340643, 200.2662915755269637 ) ) ;
#19237 = CARTESIAN_POINT ( 'NONE',  ( -0.2282788349709999887, 1452.819461535030086, 189.4800008897979922 ) ) ;
#19238 = CARTESIAN_POINT ( 'NONE',  ( -104.3125648498219817, 1379.920782886319785, 305.5271631452329757 ) ) ;
#19239 = ORIENTED_EDGE ( 'NONE', *, *, #49642, .T. ) ;
#19240 = CARTESIAN_POINT ( 'NONE',  ( -2.489617576474999705, 1516.665179208830068, 204.1258511445269903 ) ) ;
#19241 = CARTESIAN_POINT ( 'NONE',  ( 1.740066313259999932E-09, 1405.749477561730146, 267.5371647992980115 ) ) ;
#19242 = CARTESIAN_POINT ( 'NONE',  ( 4.730384172586849623, 1508.603735228350843, 211.6097810847320204 ) ) ;
#19243 = AXIS2_PLACEMENT_3D ( 'NONE', #100957, #40513, #74691 ) ;
#19244 = CIRCLE ( 'NONE', #101571, 2.000000000000003109 ) ;
#19245 = EDGE_CURVE ( 'NONE', #37608, #50173, #82973, .T. ) ;
#19246 = CARTESIAN_POINT ( 'NONE',  ( 40.26004082231700210, 1457.179229772390045, 269.7776957246979919 ) ) ;
#19247 = EDGE_CURVE ( 'NONE', #46346, #74400, #37446, .T. ) ;
#19248 = CARTESIAN_POINT ( 'NONE',  ( 2.478372249629999580, 1438.462791060409927, 157.7210847686980060 ) ) ;
#19249 = CARTESIAN_POINT ( 'NONE',  ( -28.03239352689999819, 1444.711964596309826, 137.4439080254979899 ) ) ;
#19250 = EDGE_CURVE ( 'NONE', #12028, #29708, #22255, .T. ) ;
#19251 = CARTESIAN_POINT ( 'NONE',  ( -39.40535375317039524, 1440.913060398519974, 258.4323147971229560 ) ) ;
#19252 = CARTESIAN_POINT ( 'NONE',  ( 36.67521471636259633, 1449.719261606250029, 136.2722729094319902 ) ) ;
#19253 = B_SPLINE_CURVE_WITH_KNOTS ( 'NONE', 3,
 ( #10156, #37008, #78473, #71201, #35924, #79043, #28615, #61694, #19084, #87426, #44893, #36457, #62817, #70656, #96931, #104772, #28056, #20198, #62247, #30805, #72831, #89064, #30248, #38655, #108060, #22377, #13995, #56577, #47081, #90709, #81205, #63352, #6155, #48181, #107516, #80674, #64442, #82320, #89611, #72289 ),
 .UNSPECIFIED., .F., .F.,
 ( 4, 3, 3, 3, 3, 3, 3, 3, 3, 3, 3, 3, 3, 4 ),
 ( -7.339220616559999577, -7.191616119070119773, -6.955040122091289412, -6.699117395807109965, -6.422619652672629798, -6.106550893931229851, -5.718306387288239812, -5.419628814236969738, -5.176305405323340381, -4.933732890374959545, -4.561789723725830470, -4.129459730253979721, -3.452867597008769884, -3.013389252340000546 ),
 .UNSPECIFIED. ) ;
#19254 = CARTESIAN_POINT ( 'NONE',  ( 31.34137657934008558, 1501.977400791986611, 196.3411265156547358 ) ) ;
#19255 = CARTESIAN_POINT ( 'NONE',  ( 1.914156564180000020, 1431.087920464090075, 199.8421651513589836 ) ) ;
#19256 = EDGE_CURVE ( 'NONE', #24484, #30213, #63766, .T. ) ;
#19257 = CARTESIAN_POINT ( 'NONE',  ( -31.41104781486828301, 1512.187213306747481, 202.3296363711539527 ) ) ;
#19258 = ADVANCED_FACE ( 'NONE', ( #71644 ), #10165, .T. ) ;
#19259 = CARTESIAN_POINT ( 'NONE',  ( 3.123423494469999895, 1507.140718701690048, 220.4075764222990017 ) ) ;
#19260 = FACE_OUTER_BOUND ( 'NONE', #51168, .T. ) ;
#19261 = EDGE_LOOP ( 'NONE', ( #6601, #104143, #26137, #39871 ) ) ;
#19262 = CARTESIAN_POINT ( 'NONE',  ( -3.813082683120000433E-15, 1426.500992774829911, 146.0666368882980066 ) ) ;
#19263 = ADVANCED_FACE ( 'NONE', ( #83298 ), #17155, .F. ) ;
#19264 = CARTESIAN_POINT ( 'NONE',  ( -1.290300528639490629, 1450.731663515321770, 181.8236001353477036 ) ) ;
#19265 = CARTESIAN_POINT ( 'NONE',  ( 3.152706770380329537, 1465.853101953990063, 199.3412496788349983 ) ) ;
#19266 = CARTESIAN_POINT ( 'NONE',  ( -1.334703446960000095, 1476.095835883030077, 267.8533186384979672 ) ) ;
#19268 = CIRCLE ( 'NONE', #22856, 8.104319688360000384 ) ;
#19267 = CARTESIAN_POINT ( 'NONE',  ( 4.822497006680000808, 1500.099429524390189, 201.8516542630590038 ) ) ;
#19269 = LINE ( 'NONE', #70847, #44144 ) ;
#19270 = CARTESIAN_POINT ( 'NONE',  ( -3.841073510662149637, 1448.295370182304396, 185.0282369137797218 ) ) ;
#19271 = CARTESIAN_POINT ( 'NONE',  ( -15.94115646620460147, 1384.874344242760117, 219.6433026291970236 ) ) ;
#19272 = CARTESIAN_POINT ( 'NONE',  ( -18.06884258770000073, 1415.263254653229978, 207.6880149420679800 ) ) ;
#19273 = CYLINDRICAL_SURFACE ( 'NONE', #68066, 0.9999999999999988898 ) ;
#19274 = CARTESIAN_POINT ( 'NONE',  ( 26.16433611993790009, 1436.692690809629994, 136.8774806592069808 ) ) ;
#19275 =( BOUNDED_CURVE ( )  B_SPLINE_CURVE ( 3, ( #3265, #19471, #20026, #36837 ),
 .UNSPECIFIED., .F., .F. ) 
 B_SPLINE_CURVE_WITH_KNOTS ( ( 4, 4 ),
 ( 1.009476837204658084, 2.132115841021330116 ),
 .UNSPECIFIED. ) 
 CURVE ( )  GEOMETRIC_REPRESENTATION_ITEM ( )  RATIONAL_B_SPLINE_CURVE ( ( 1.000000000000000000, 0.8977023149622460618, 0.8977023149622460618, 1.000000000000000000 ) ) 
 REPRESENTATION_ITEM ( '' )  );
#19276 = CARTESIAN_POINT ( 'NONE',  ( -10.63692245770969969, 1396.284509905209916, 206.0546994452240028 ) ) ;
#19277 = EDGE_CURVE ( 'NONE', #53387, #23318, #58996, .T. ) ;
#19278 = B_SPLINE_CURVE_WITH_KNOTS ( 'NONE', 3,
 ( #44740, #27918, #17824, #36310, #77771, #69395 ),
 .UNSPECIFIED., .F., .F.,
 ( 4, 2, 4 ),
 ( 0.000000000000000000, 0.5000000000000000000, 1.000000000000000000 ),
 .UNSPECIFIED. ) ;
#19279 = CARTESIAN_POINT ( 'NONE',  ( -17.06997858521869915, 1410.142247367640039, 225.8741214327440048 ) ) ;
#19280 = CARTESIAN_POINT ( 'NONE',  ( -7.351108641702090551, 1491.337179302150162, 211.7591575584629879 ) ) ;
#19281 = EDGE_LOOP ( 'NONE', ( #57028, #68784, #102726, #37551 ) ) ;
#19282 = CARTESIAN_POINT ( 'NONE',  ( -19.47231853460000295, 1466.701452153789887, 212.9249870548489980 ) ) ;
#19284 = EDGE_CURVE ( 'NONE', #29958, #6066, #58661, .T. ) ;
#19283 = CARTESIAN_POINT ( 'NONE',  ( -13.58798618625510102, 1508.413595127150074, 209.8328882561570197 ) ) ;
#19285 = CARTESIAN_POINT ( 'NONE',  ( -3.229842622735000113, 1517.051704408389924, 217.4817367409870030 ) ) ;
#19287 = CARTESIAN_POINT ( 'NONE',  ( -9.949472290641201866, 1438.963978288880071, 209.6181135091480030 ) ) ;
#19286 = CARTESIAN_POINT ( 'NONE',  ( 10.71319734329999918, 1425.353252437830179, 115.7252223364979926 ) ) ;
#19288 = CARTESIAN_POINT ( 'NONE',  ( 3.879157139540000188, 1451.813806661290073, 190.3284334383990029 ) ) ;
#19289 = ADVANCED_FACE ( 'NONE', ( #7688 ), #74646, .T. ) ;
#19290 = CARTESIAN_POINT ( 'NONE',  ( 4.303869558802829509, 1423.888414498320117, 183.7752672280500121 ) ) ;
#19291 = VECTOR ( 'NONE', #20810, 1000.000000000000000 ) ;
#19292 = CARTESIAN_POINT ( 'NONE',  ( -109.9872068205719984, 1384.854720727420045, 311.4556833561759390 ) ) ;
#19293 = CARTESIAN_POINT ( 'NONE',  ( 7.645128971980000188, 1425.330907912760040, 211.9289184192489870 ) ) ;
#19294 = CARTESIAN_POINT ( 'NONE',  ( -16.61337445550000069, 1463.629612651790012, 220.4655171657990138 ) ) ;
#19295 = FACE_BOUND ( 'NONE', #83749, .T. ) ;
#19296 = FACE_OUTER_BOUND ( 'NONE', #60235, .T. ) ;
#19297 = CARTESIAN_POINT ( 'NONE',  ( 2.594674246779999915, 1449.291015053200226, 183.0785327561979727 ) ) ;
#19298 = EDGE_CURVE ( 'NONE', #56404, #12156, #74374, .T. ) ;
#19299 = CARTESIAN_POINT ( 'NONE',  ( 8.000513322313473452, 1364.896752889035270, 209.6218459617148824 ) ) ;
#19301 = ORIENTED_EDGE ( 'NONE', *, *, #81620, .T. ) ;
#19300 = LINE ( 'NONE', #95480, #1416 ) ;
#19302 = ORIENTED_EDGE ( 'NONE', *, *, #22687, .F. ) ;
#19303 = CARTESIAN_POINT ( 'NONE',  ( -12.65017221549999960, 1441.023539904969994, 188.0792847196979949 ) ) ;
#19304 = CARTESIAN_POINT ( 'NONE',  ( -0.3160898611105850131, 1482.866385869289843, 236.2848248989660078 ) ) ;
#19305 = CARTESIAN_POINT ( 'NONE',  ( -2.316392100889999917, 1473.548945576829965, 270.3918176930980053 ) ) ;
#19306 = CARTESIAN_POINT ( 'NONE',  ( -7.567811406605000180, 1511.141271963170084, 212.1712098993370148 ) ) ;
#19307 = CARTESIAN_POINT ( 'NONE',  ( -120.1712171740600041, 1306.483669372790018, 304.2218459572590064 ) ) ;
#19308 = CARTESIAN_POINT ( 'NONE',  ( -30.90487439922554103, 1525.907212628473644, 201.8101144455182521 ) ) ;
#19309 = CARTESIAN_POINT ( 'NONE',  ( -2.845798587710199890, 1464.349408459529968, 199.2989423254240080 ) ) ;
#19310 = CARTESIAN_POINT ( 'NONE',  ( 12.34231650081810194, 1419.113258958060214, 223.6504151099339879 ) ) ;
#19311 = FILL_AREA_STYLE ('',( #41775 ) ) ;
#19312 = CARTESIAN_POINT ( 'NONE',  ( 35.14729760223570310, 1435.724875811340098, 135.0317109007289957 ) ) ;
#19313 = CARTESIAN_POINT ( 'NONE',  ( 6.451603462551370072, 1396.138355344729916, 218.0852709918889900 ) ) ;
#19314 = CARTESIAN_POINT ( 'NONE',  ( 14.94931177939999856, 1409.376221040630071, 212.2047251789079780 ) ) ;
#19315 = CARTESIAN_POINT ( 'NONE',  ( -0.7754702341989130332, 1405.749502388330029, 267.5370916581230176 ) ) ;
#19316 = CARTESIAN_POINT ( 'NONE',  ( 41.49088685270000099, 1443.869556898650217, 136.5795280473980142 ) ) ;
#19317 = VERTEX_POINT ( 'NONE', #110152 ) ;
#19318 = CARTESIAN_POINT ( 'NONE',  ( -10.96966797059999799, 1432.360037085170234, 151.7701368415980028 ) ) ;
#19319 = CARTESIAN_POINT ( 'NONE',  ( 12.93995891640000018, 1441.798025058569920, 188.7551818563979964 ) ) ;
#19320 = ORIENTED_EDGE ( 'NONE', *, *, #100767, .T. ) ;
#19321 = AXIS2_PLACEMENT_3D ( 'NONE', #48039, #82179, #73242 ) ;
#19322 = ORIENTED_EDGE ( 'NONE', *, *, #80964, .F. ) ;
#19323 = CARTESIAN_POINT ( 'NONE',  ( -4.254366227259999356, 1454.573790426789856, 200.5971711767689953 ) ) ;
#19324 = CARTESIAN_POINT ( 'NONE',  ( 9.925983360900000108, 1364.303202023270160, 207.6218459616989946 ) ) ;
#19325 = AXIS2_PLACEMENT_3D ( 'NONE', #8115, #93758, #76432 ) ;
#19326 = CARTESIAN_POINT ( 'NONE',  ( 4.620008207075000151, 1516.777260590120022, 214.8964555921769772 ) ) ;
#19327 = CARTESIAN_POINT ( 'NONE',  ( 3.049363929105000093, 1511.141271963160079, 216.6896573387070077 ) ) ;
#19328 = ADVANCED_FACE ( 'NONE', ( #33423 ), #33039, .T. ) ;
#19329 = ORIENTED_EDGE ( 'NONE', *, *, #104250, .T. ) ;
#19330 = CARTESIAN_POINT ( 'NONE',  ( 4.464821409069999802, 1422.103166678080015, 206.5928916359989955 ) ) ;
#19331 = CARTESIAN_POINT ( 'NONE',  ( -69.36674278830000162, 1379.746858117810007, 280.1513224085589968 ) ) ;
#19332 = CIRCLE ( 'NONE', #96247, 1.000000000000000888 ) ;
#19333 = EDGE_CURVE ( 'NONE', #7367, #85956, #99018, .T. ) ;
#19334 = CARTESIAN_POINT ( 'NONE',  ( -105.7960290519230000, 1378.913060387289988, 303.9610383217989806 ) ) ;
#19335 = CARTESIAN_POINT ( 'NONE',  ( -4.620008245204999753, 1516.777260590120022, 203.3472363101570011 ) ) ;
#19336 = CARTESIAN_POINT ( 'NONE',  ( -11.84353516585279920, 1489.590656028399962, 212.0913857160410032 ) ) ;
#19337 = CARTESIAN_POINT ( 'NONE',  ( -92.78435512849998190, 1384.849527344140142, 294.1459074807589786 ) ) ;
#19339 = B_SPLINE_CURVE_WITH_KNOTS ( 'NONE', 3,
 ( #34048, #93396, #8832, #16661, #35706, #9405, #68787, #27307, #102887, #67678 ),
 .UNSPECIFIED., .F., .F.,
 ( 4, 2, 2, 2, 4 ),
 ( 2.159480829822040206E-09, 0.05040947966427840321, 0.1104028076245519990, 0.1513866672460139895, 0.2227566989315760138 ),
 .UNSPECIFIED. ) ;
#19338 = LINE ( 'NONE', #35603, #106237 ) ;
#19340 = CARTESIAN_POINT ( 'NONE',  ( -11.42986879550000090, 1410.682064136229883, 228.8161090984979751 ) ) ;
#19342 = ORIENTED_EDGE ( 'NONE', *, *, #7012, .F. ) ;
#19341 = CARTESIAN_POINT ( 'NONE',  ( -4.084527001869999729, 1446.441115836090148, 184.0652579870979935 ) ) ;
#19343 = CARTESIAN_POINT ( 'NONE',  ( -13.80541478530910027, 1434.979604282769969, 148.5370187744020143 ) ) ;
#19344 = CARTESIAN_POINT ( 'NONE',  ( 10.73506988043325627, 1424.972993549859893, 139.1354236083641922 ) ) ;
#19345 = CARTESIAN_POINT ( 'NONE',  ( -3.078458294050000266, 1383.868666969369770, 218.4015365393190109 ) ) ;
#19347 = EDGE_CURVE ( 'NONE', #93985, #437, #105082, .T. ) ;
#19346 = CARTESIAN_POINT ( 'NONE',  ( 16.77792727996295596, 1423.636664231082932, 228.4337725396501355 ) ) ;
#19348 = CARTESIAN_POINT ( 'NONE',  ( -25.74205574149999975, 1436.650732699449918, 137.0790728707980008 ) ) ;
#19349 = VECTOR ( 'NONE', #19457, 1000.000000000000000 ) ;
#19350 = CARTESIAN_POINT ( 'NONE',  ( -4.027051443935000030, 1516.733363207009916, 211.6130343286269806 ) ) ;
#19351 = CARTESIAN_POINT ( 'NONE',  ( -66.36498982899999532, 1379.745690266980091, 275.3119164116589559 ) ) ;
#19352 = CARTESIAN_POINT ( 'NONE',  ( 0.01485783991055205852, 1507.825067223495580, 237.5163643644461899 ) ) ;
#19353 = CARTESIAN_POINT ( 'NONE',  ( 19.38539822485692810, 1495.497225806873075, 199.6821155845800888 ) ) ;
#19354 = CARTESIAN_POINT ( 'NONE',  ( 19.84840157878679534, 1410.966943121492704, 197.0192273420008178 ) ) ;
#19355 = CARTESIAN_POINT ( 'NONE',  ( 2.879318417774999972, 1516.995911393979895, 209.8571825100049750 ) ) ;
#19356 = ORIENTED_EDGE ( 'NONE', *, *, #13091, .T. ) ;
#19357 = CARTESIAN_POINT ( 'NONE',  ( 2.500000000000000000, 1437.040203032260024, 157.6453869839979802 ) ) ;
#19358 = CARTESIAN_POINT ( 'NONE',  ( -1.898512081650000072, 1415.378575369830060, 233.0498031619979997 ) ) ;
#19359 = CARTESIAN_POINT ( 'NONE',  ( -47.37130750840000104, 1384.881166745699829, 256.2794477600589858 ) ) ;
#19360 = ORIENTED_EDGE ( 'NONE', *, *, #26884, .T. ) ;
#19361 = CARTESIAN_POINT ( 'NONE',  ( -10.35521326297049960, 1385.310235430599960, 218.7605991785599997 ) ) ;
#19362 = ADVANCED_FACE ( 'NONE', ( #34545 ), #17713, .F. ) ;
#19363 = CARTESIAN_POINT ( 'NONE',  ( -2.593205515350000212, 1429.616254713290118, 200.8413778689989897 ) ) ;
#19364 = CARTESIAN_POINT ( 'NONE',  ( 17.55481076435209786, 1469.009107921980103, 228.8208540407819669 ) ) ;
#19365 = CARTESIAN_POINT ( 'NONE',  ( -24.92784963018079836, 1509.784682262980141, 224.7537335476830265 ) ) ;
#19366 = EDGE_CURVE ( 'NONE', #38471, #38998, #49624, .T. ) ;
#19367 = CARTESIAN_POINT ( 'NONE',  ( 3.535327660699999708, 1487.160996047289927, 197.6951164054989931 ) ) ;
#19368 = DIRECTION ( 'NONE',  ( -1.755985294532469921E-16, 1.000000000000000000, -1.338183447452831989E-16 ) ) ;
#19369 = CARTESIAN_POINT ( 'NONE',  ( 0.1432641814004909919, 1420.464960711380172, 182.7250166793000119 ) ) ;
#19371 = CARTESIAN_POINT ( 'NONE',  ( -4.117405581809999937, 1420.599289921329955, 186.3488710820979861 ) ) ;
#19370 = CARTESIAN_POINT ( 'NONE',  ( 5.006329581384999727, 1516.755758396839838, 215.6722354023569892 ) ) ;
#19372 = CARTESIAN_POINT ( 'NONE',  ( 19.26331593919999818, 1508.281539294829827, 188.5704572384980224 ) ) ;
#19373 = CARTESIAN_POINT ( 'NONE',  ( 7.000000000000000000, 1418.913060387330006, 172.2701767054979882 ) ) ;
#19374 = ORIENTED_EDGE ( 'NONE', *, *, #86306, .F. ) ;
#19375 = CARTESIAN_POINT ( 'NONE',  ( -11.74432248202560025, 1415.089118586289942, 196.5522872353360242 ) ) ;
#19376 = CARTESIAN_POINT ( 'NONE',  ( -6.106019680640000225, 1485.913060386929828, 181.8019572232980181 ) ) ;
#19377 = VERTEX_POINT ( 'NONE', #95561 ) ;
#19378 = CARTESIAN_POINT ( 'NONE',  ( 4.071927273580000062, 1420.049653579930009, 185.6171871639980111 ) ) ;
#19379 = EDGE_CURVE ( 'NONE', #70030, #63160, #20980, .T. ) ;
#19380 = CARTESIAN_POINT ( 'NONE',  ( 9.978198430534376939, 1435.712339636959996, 152.5066790191562518 ) ) ;
#19381 = CARTESIAN_POINT ( 'NONE',  ( 7.533847528226220724, 1510.598356033829987, 203.2091179615540284 ) ) ;
#19382 = CARTESIAN_POINT ( 'NONE',  ( 2.838547795930000284, 1441.919264588690112, 217.8904307960689835 ) ) ;
#19383 = DIRECTION ( 'NONE',  ( -0.1070030146457249254, 0.000000000000000000, 0.9942586961433763637 ) ) ;
#19384 = CARTESIAN_POINT ( 'NONE',  ( -2178.386296064867111, -8387.357407334289746, 1972.013908154370711 ) ) ;
#19385 = CARTESIAN_POINT ( 'NONE',  ( -3.701619934510000043, 1446.913858801710148, 156.0868339982980046 ) ) ;
#19387 = ADVANCED_FACE ( 'NONE', ( #26127 ), #53587, .F. ) ;
#19386 = FACE_OUTER_BOUND ( 'NONE', #69178, .T. ) ;
#19388 = CARTESIAN_POINT ( 'NONE',  ( -17.44469085659999763, 1435.922852757180181, 147.7537887305979893 ) ) ;
#19389 = CARTESIAN_POINT ( 'NONE',  ( 33.93392841120000014, 1451.575795592029863, 135.5855060888980006 ) ) ;
#19390 = CARTESIAN_POINT ( 'NONE',  ( 16.09124803980000351, 1410.842148622430159, 191.5172216204979918 ) ) ;
#19392 = CARTESIAN_POINT ( 'NONE',  ( -15.69795926999090163, 1522.051704408389924, 195.4758181584410011 ) ) ;
#19391 = CARTESIAN_POINT ( 'NONE',  ( 6.636923444789999849, 1488.278828811890207, 199.0403411110989964 ) ) ;
#19393 = CARTESIAN_POINT ( 'NONE',  ( 10.86679789090769965, 1425.928602444132594, 148.0726311711557628 ) ) ;
#19394 = VERTEX_POINT ( 'NONE', #36210 ) ;
#19395 = CARTESIAN_POINT ( 'NONE',  ( 0.8261703649055629484, 1507.439225835989873, 186.3102742836619825 ) ) ;
#19396 = CARTESIAN_POINT ( 'NONE',  ( 23.44331756030000236, 1430.465020642029913, 206.4626199018280204 ) ) ;
#19397 = EDGE_CURVE ( 'NONE', #22237, #35341, #56200, .T. ) ;
#19398 = CARTESIAN_POINT ( 'NONE',  ( -23.66389183400000107, 1436.227554635920114, 212.2198923620080109 ) ) ;
#19399 = CARTESIAN_POINT ( 'NONE',  ( -4.687677274410000372, 1484.078770814390055, 199.3574548446190136 ) ) ;
#19400 = CIRCLE ( 'NONE', #92703, 26.50000000000001421 ) ;
#19401 = CARTESIAN_POINT ( 'NONE',  ( -18.51267907639999777, 1508.236097876829945, 229.7333076606979887 ) ) ;
#19402 = CARTESIAN_POINT ( 'NONE',  ( -2.444956619880277682, 1524.972613296788722, 242.2723289509666529 ) ) ;
#19403 = CARTESIAN_POINT ( 'NONE',  ( 5.402657594482866976, 1473.518541113343190, 218.3241216679554100 ) ) ;
#19404 = CARTESIAN_POINT ( 'NONE',  ( 28.27139721233034564, 1526.382868172864164, 219.5606225550385204 ) ) ;
#19405 = CARTESIAN_POINT ( 'NONE',  ( -18.94135955378079572, 1509.705011416190018, 185.2601256149999926 ) ) ;
#19406 = VECTOR ( 'NONE', #44843, 1000.000000000000227 ) ;
#19407 = EDGE_CURVE ( 'NONE', #20038, #77300, #65776, .T. ) ;
#19408 = EDGE_CURVE ( 'NONE', #69834, #10158, #24258, .T. ) ;
#19409 = CARTESIAN_POINT ( 'NONE',  ( -8.097225737347908847, 1490.150856172170052, 216.5834626028189973 ) ) ;
#19410 = CARTESIAN_POINT ( 'NONE',  ( 7.755364537188749630, 1459.738773378459882, 228.9106043144229830 ) ) ;
#19411 = CARTESIAN_POINT ( 'NONE',  ( -94.12119808786221142, 1383.767725327359813, 309.6675098620430049 ) ) ;
#19412 = AXIS2_PLACEMENT_3D ( 'NONE', #91274, #6160, #32480 ) ;
#19413 = CARTESIAN_POINT ( 'NONE',  ( -108.7912213487909980, 1383.917108116560030, 311.1258975414110068 ) ) ;
#19414 = DIRECTION ( 'NONE',  ( 0.7071067811865475727, -6.078560574715863648E-17, 0.7071067811865475727 ) ) ;
#19415 = CARTESIAN_POINT ( 'NONE',  ( -1.579129830164079928, 1516.559523801380010, 201.4121538206049706 ) ) ;
#19417 = VERTEX_POINT ( 'NONE', #41170 ) ;
#19416 = DIRECTION ( 'NONE',  ( 0.000000000000000000, 0.000000000000000000, -1.000000000000000000 ) ) ;
#19418 = CARTESIAN_POINT ( 'NONE',  ( -17.75078229062794222, 1460.106445376706233, 228.1476975191470444 ) ) ;
#19419 = CARTESIAN_POINT ( 'NONE',  ( -85.29011547940000071, 1381.870680097800005, 290.3579090523590480 ) ) ;
#19420 = CARTESIAN_POINT ( 'NONE',  ( -14.75654852344869816, 1418.698223271940151, 213.5276923267749964 ) ) ;
#19421 = EDGE_LOOP ( 'NONE', ( #67561, #45683, #51082, #21617 ) ) ;
#19422 = VERTEX_POINT ( 'NONE', #68052 ) ;
#19423 = CARTESIAN_POINT ( 'NONE',  ( 17.36569701797450094, 1415.089948427370018, 209.9483774915429990 ) ) ;
#19424 = CARTESIAN_POINT ( 'NONE',  ( 13.46763530789999841, 1509.145555155530019, 233.8319897144979791 ) ) ;
#19425 = DIRECTION ( 'NONE',  ( -0.7882878497005411100, 0.000000000000000000, 0.6153066438894488899 ) ) ;
#19427 = CARTESIAN_POINT ( 'NONE',  ( -36.92073947260000466, 1453.101237517530080, 259.2254642747980142 ) ) ;
#19426 = CARTESIAN_POINT ( 'NONE',  ( -24.09814616333339998, 1444.255785637029931, 212.5772553280679915 ) ) ;
#19428 = EDGE_CURVE ( 'NONE', #75409, #10270, #29621, .T. ) ;
#19429 = CARTESIAN_POINT ( 'NONE',  ( -4.660842796387490772, 1495.148806942539977, 197.7136934498280141 ) ) ;
#19430 = CARTESIAN_POINT ( 'NONE',  ( -11.21270966080000164, 1433.906859537220043, 151.6012850642980254 ) ) ;
#19431 = CARTESIAN_POINT ( 'NONE',  ( 26.61730932929999938, 1507.998999673229946, 204.1002567748479919 ) ) ;
#19432 = LINE ( 'NONE', #69324, #67491 ) ;
#19433 = AXIS2_PLACEMENT_3D ( 'NONE', #4356, #105718, #63724 ) ;
#19434 = CARTESIAN_POINT ( 'NONE',  ( 8.290629166600000488, 1409.704288481229923, 187.9461355818979769 ) ) ;
#19435 = CARTESIAN_POINT ( 'NONE',  ( 4.234467102410000017, 1420.712403739130195, 185.6414432377980006 ) ) ;
#19437 = ADVANCED_FACE ( 'NONE', ( #22680 ), #108928, .T. ) ;
#19436 = CARTESIAN_POINT ( 'NONE',  ( -11.55343452480000010, 1436.871189028030130, 151.7006538029980049 ) ) ;
#19438 = CARTESIAN_POINT ( 'NONE',  ( 9.548319690719999642, 1438.548742142269930, 152.9855552813980069 ) ) ;
#19439 = CARTESIAN_POINT ( 'NONE',  ( -9.860632074819870141, 1424.099558978640061, 204.5593013001630140 ) ) ;
#19440 = CARTESIAN_POINT ( 'NONE',  ( -12.23489732466240021, 1490.237667237379810, 209.6383001084460034 ) ) ;
#19441 = CARTESIAN_POINT ( 'NONE',  ( -19.18813880309999931, 1465.797355387890093, 204.3301597990889888 ) ) ;
#19442 = ORIENTED_EDGE ( 'NONE', *, *, #49792, .T. ) ;
#19443 = CARTESIAN_POINT ( 'NONE',  ( -2.404122373123565914, 1426.711430350427463, 142.7750368341233695 ) ) ;
#19445 = CARTESIAN_POINT ( 'NONE',  ( -11.93924564462519911, 1481.986046384150086, 228.0814323177490053 ) ) ;
#19444 = B_SPLINE_CURVE_WITH_KNOTS ( 'NONE', 5,
 ( #21039, #10458, #79330, #53594, #46303, #55242, #35656, #96117, #72060 ),
 .UNSPECIFIED., .F., .F.,
 ( 6, 3, 6 ),
 ( 0.000000000000000000, 0.5050532947658213923, 1.000000000000000000 ),
 .UNSPECIFIED. ) ;
#19446 = CARTESIAN_POINT ( 'NONE',  ( -44.29556206470000035, 1444.183390959899953, 270.0939713427979996 ) ) ;
#19447 = CARTESIAN_POINT ( 'NONE',  ( 7.571416212307459759, 1423.019345442000031, 195.7264161909869813 ) ) ;
#19448 = CARTESIAN_POINT ( 'NONE',  ( 17.37499703619999636, 1409.684548388429903, 222.9025586185979932 ) ) ;
#19449 = DIRECTION ( 'NONE',  ( -1.755985294532469921E-16, 1.000000000000000000, -1.338183447452831989E-16 ) ) ;
#19450 = CARTESIAN_POINT ( 'NONE',  ( 4.329177920710189476, 1515.075136430340081, 210.6018449539679978 ) ) ;
#19451 = CARTESIAN_POINT ( 'NONE',  ( 2.909553342395870157, 1409.594673830890088, 231.3464090763989986 ) ) ;
#19452 = CARTESIAN_POINT ( 'NONE',  ( 1.272733413219999887, 1507.906795984730024, 237.1822243490979929 ) ) ;
#19453 = CARTESIAN_POINT ( 'NONE',  ( -8.212003350069998930, 1417.874967654629927, 230.9629104793979764 ) ) ;
#19454 = CARTESIAN_POINT ( 'NONE',  ( -1.268441606857695803, 1484.597036441479304, 182.2979883374861458 ) ) ;
#19455 = CARTESIAN_POINT ( 'NONE',  ( 11.31426556939452510, 1362.616033936885287, 209.6218459617033432 ) ) ;
#19456 = CARTESIAN_POINT ( 'NONE',  ( -45.90003289832019817, 1437.099605401870122, 266.9804752891529915 ) ) ;
#19457 = DIRECTION ( 'NONE',  ( 0.4090087482554252696, 0.000000000000000000, -0.9125304618753996566 ) ) ;
#19458 = ORIENTED_EDGE ( 'NONE', *, *, #59272, .T. ) ;
#19459 = CARTESIAN_POINT ( 'NONE',  ( 26.60254240749708643, 1435.426458660660273, 135.2844112663541694 ) ) ;
#19460 = B_SPLINE_CURVE_WITH_KNOTS ( 'NONE', 5,
 ( #11847, #35953, #10754, #36494, #54430, #79072 ),
 .UNSPECIFIED., .F., .F.,
 ( 6, 6 ),
 ( 330.1233636409999690, 340.1768165719999502 ),
 .UNSPECIFIED. ) ;
#19461 = VERTEX_POINT ( 'NONE', #82628 ) ;
#19462 = CARTESIAN_POINT ( 'NONE',  ( -3.447128498755000159, 1516.778853242349896, 210.2570310142770040 ) ) ;
#19463 = CARTESIAN_POINT ( 'NONE',  ( -9.655463540387350108, 1446.888654090670116, 212.1942763251040276 ) ) ;
#19464 = DIRECTION ( 'NONE',  ( -0.7071067811865475727, 0.000000000000000000, 0.7071067811865475727 ) ) ;
#19465 = CARTESIAN_POINT ( 'NONE',  ( -5.779044620229999651, 1425.409882702530012, 186.4185359615979962 ) ) ;
#19466 = AXIS2_PLACEMENT_3D ( 'NONE', #42241, #85892, #59056 ) ;
#19467 = CARTESIAN_POINT ( 'NONE',  ( -3.566337987641670093, 1497.263210272700235, 220.9985256183890101 ) ) ;
#19468 = B_SPLINE_SURFACE_WITH_KNOTS ( 'NONE', 5, 5, ( 
 ( #54072, #88198, #95486, #27730, #46213, #45112 ),
 ( #80347, #53508, #62477, #105554, #63037, #54617 ),
 ( #2004, #79806, #96597, #79253, #45667, #2562 ),
 ( #38325, #106094, #3111, #10369, #3664, #72504 ),
 ( #46765, #37240, #61918, #37793, #36685, #55165 ),
 ( #71981, #97142, #29372, #97688, #18753, #96035 ),
 ( #52950, #70879, #20961, #89288, #19306, #80895 ),
 ( #106633, #13652, #21503, #92046, #22048, #64113 ),
 ( #82553, #15318, #56245, #5847, #49512, #38871 ),
 ( #23173, #65757, #40537, #98786, #47292, #73614 ),
 ( #100444, #74164, #22596, #83636, #56799, #98234 ),
 ( #90936, #39987, #31580, #48965, #57373, #65209 ) ),
 .UNSPECIFIED., .F., .F., .F.,
 ( 6, 3, 3, 6 ),
 ( 6, 6 ),
 ( 3.672001930560000016, 6.062162762939999894, 7.801458206509999549, 8.912489289850000773 ),
 ( 0.000000000000000000, 1.000000000000000000 ),
 .UNSPECIFIED. ) ;
#19469 = EDGE_LOOP ( 'NONE', ( #63051, #27777, #13595, #35069, #103415 ) ) ;
#19470 = DIRECTION ( 'NONE',  ( -1.000000000000000000, 0.000000000000000000, 0.000000000000000000 ) ) ;
#19472 = FACE_OUTER_BOUND ( 'NONE', #64725, .T. ) ;
#19471 = CARTESIAN_POINT ( 'NONE',  ( 3.497662945300243909, 1505.961916725443189, 220.6749222718410692 ) ) ;
#19473 = CARTESIAN_POINT ( 'NONE',  ( -114.4405920464259765, 1391.913060387289988, 302.5138740040609946 ) ) ;
#19474 = CARTESIAN_POINT ( 'NONE',  ( -18.15878713041950121, 1508.551704422010062, 211.0186658100620036 ) ) ;
#19475 = CARTESIAN_POINT ( 'NONE',  ( 4.873735476160000246, 1472.089320948289924, 218.0431589096889695 ) ) ;
#19476 = CARTESIAN_POINT ( 'NONE',  ( -9.966728652698208180, 1439.480322961800084, 208.4310021967300202 ) ) ;
#19477 = ORIENTED_EDGE ( 'NONE', *, *, #54848, .T. ) ;
#19478 = CARTESIAN_POINT ( 'NONE',  ( -13.53287548934629925, 1409.390853263720146, 270.2591806110339689 ) ) ;
#19479 = CARTESIAN_POINT ( 'NONE',  ( -7.726684725664999753, 1517.208444099459939, 207.9957078235169945 ) ) ;
#19480 = CARTESIAN_POINT ( 'NONE',  ( 3.564372338642340043, 1417.932634516880171, 233.5387638921010023 ) ) ;
#19481 = CARTESIAN_POINT ( 'NONE',  ( 8.721922434858829121, 1435.147675358199876, 206.9711085294910049 ) ) ;
#19483 = VERTEX_POINT ( 'NONE', #50140 ) ;
#19482 = CARTESIAN_POINT ( 'NONE',  ( -7.581703558749627980, 1366.473201395314163, 210.6218459617142003 ) ) ;
#19484 = ORIENTED_EDGE ( 'NONE', *, *, #40616, .F. ) ;
#19485 = CARTESIAN_POINT ( 'NONE',  ( 45.24071116116442681, 1445.446384637186156, 268.9857686712747977 ) ) ;
#19486 = CARTESIAN_POINT ( 'NONE',  ( -1.126170950785350122, 1467.742527459179882, 220.1728790705329857 ) ) ;
#19487 = CARTESIAN_POINT ( 'NONE',  ( -20.61921987750000085, 1486.434067572889944, 211.1039075214289937 ) ) ;
#19488 = CARTESIAN_POINT ( 'NONE',  ( -0.02885268102940060156, 1409.146038359130216, 185.6769965299799878 ) ) ;
#19489 = VECTOR ( 'NONE', #47385, 1000.000000000000000 ) ;
#19490 = AXIS2_PLACEMENT_3D ( 'NONE', #75178, #23647, #91417 ) ;
#19491 = CARTESIAN_POINT ( 'NONE',  ( -21.91250632251765396, 1506.380977040318612, 210.8063876161204462 ) ) ;
#19492 = CARTESIAN_POINT ( 'NONE',  ( -21.02025974500000061, 1430.787304677930024, 220.7233419882979888 ) ) ;
#19493 = AXIS2_PLACEMENT_3D ( 'NONE', #48186, #82867, #21281 ) ;
#19494 = CARTESIAN_POINT ( 'NONE',  ( -0.0001236924928765489894, 1475.983344053139945, 267.2347465760000205 ) ) ;
#19495 = CARTESIAN_POINT ( 'NONE',  ( -11.55918612708340021, 1391.913060387249971, 207.9911993583930325 ) ) ;
#19496 = LINE ( 'NONE', #53129, #671 ) ;
#19497 = CARTESIAN_POINT ( 'NONE',  ( -3.268235758764999943, 1516.890356958860139, 206.2562572478169898 ) ) ;
#19498 = ORIENTED_EDGE ( 'NONE', *, *, #91922, .T. ) ;
#19499 = CARTESIAN_POINT ( 'NONE',  ( 4.229167303610000594, 1436.983388288790138, 227.1518914930990150 ) ) ;
#19500 = CARTESIAN_POINT ( 'NONE',  ( 1.505303296824910042, 1463.321697279820000, 183.0243996004219866 ) ) ;
#19501 = ORIENTED_EDGE ( 'NONE', *, *, #21990, .F. ) ;
#19502 = CARTESIAN_POINT ( 'NONE',  ( -113.4000000000000057, 1375.913060387289988, 304.2218459572590064 ) ) ;
#19503 = CARTESIAN_POINT ( 'NONE',  ( 24.12978840347330234, 1452.070425774049909, 136.4015957713419880 ) ) ;
#19504 = CARTESIAN_POINT ( 'NONE',  ( 11.60004869885209899, 1425.673082948501360, 137.6482176788198615 ) ) ;
#19505 = CARTESIAN_POINT ( 'NONE',  ( -27.45731751820000355, 1390.955273319920252, 213.9131165264389836 ) ) ;
#19506 = CARTESIAN_POINT ( 'NONE',  ( 7.592573332174999301, 1517.051705360460119, 213.6085791126270124 ) ) ;
#19507 = CARTESIAN_POINT ( 'NONE',  ( 17.23433708029999778, 1409.514896698529810, 194.1039298879979924 ) ) ;
#19508 = DIRECTION ( 'NONE',  ( 0.000000000000000000, 1.000000000000000000, 0.000000000000000000 ) ) ;
#19509 = CARTESIAN_POINT ( 'NONE',  ( 17.06941266450000327, 1409.674943318129863, 224.8086569787979840 ) ) ;
#19511 = CARTESIAN_POINT ( 'NONE',  ( -14.02252553536541235, 1379.587897852161632, 211.9004556758163460 ) ) ;
#19510 = CARTESIAN_POINT ( 'NONE',  ( 1.383512846939999985, 1417.442430893029950, 235.2784810073979997 ) ) ;
#19512 = CARTESIAN_POINT ( 'NONE',  ( 0.9375664774988570205, 1452.266183237480163, 183.3265372543810088 ) ) ;
#19513 = AXIS2_PLACEMENT_3D ( 'NONE', #100065, #32850, #83815 ) ;
#19514 = CARTESIAN_POINT ( 'NONE',  ( -11.18262514070000080, 1381.429409390050068, 216.8219888905990160 ) ) ;
#19515 = CARTESIAN_POINT ( 'NONE',  ( -1.705466448594999962, 1517.120861839400050, 214.1360410720469929 ) ) ;
#19516 = CARTESIAN_POINT ( 'NONE',  ( 27.59078576489319801, 1447.301049566279971, 137.0121621487540153 ) ) ;
#19517 = ORIENTED_EDGE ( 'NONE', *, *, #77071, .T. ) ;
#19518 = CARTESIAN_POINT ( 'NONE',  ( 22.03465957474552539, 1501.977400791986611, 182.8300405912328301 ) ) ;
#19519 = CARTESIAN_POINT ( 'NONE',  ( 22.03465957474572079, 1522.382868172863937, 235.4136513321629991 ) ) ;
#19520 = CARTESIAN_POINT ( 'NONE',  ( -7.195479650174489983, 1484.442662870319964, 199.6339812554890045 ) ) ;
#19521 = DIRECTION ( 'NONE',  ( -1.836970198721029688E-16, -1.000000000000000000, 0.000000000000000000 ) ) ;
#19522 = CARTESIAN_POINT ( 'NONE',  ( -37.24878679391060388, 1449.386611531670042, 136.3094430657310170 ) ) ;
#19523 = CARTESIAN_POINT ( 'NONE',  ( -4.326999254989129184, 1515.158336317470003, 209.0580706801189876 ) ) ;
#19524 = CARTESIAN_POINT ( 'NONE',  ( -17.26713005039999871, 1453.798585005629775, 234.3916895853979838 ) ) ;
#19525 = CARTESIAN_POINT ( 'NONE',  ( 32.87679566159992817, 1465.269378838331249, 266.5399014024979465 ) ) ;
#19527 = EDGE_CURVE ( 'NONE', #79125, #108385, #80056, .T. ) ;
#19526 = CARTESIAN_POINT ( 'NONE',  ( -12.31337600513549901, 1378.372828873670187, 209.7376539469879901 ) ) ;
#19528 = CARTESIAN_POINT ( 'NONE',  ( -19.86748946169999996, 1471.981010699629906, 269.5245921433980243 ) ) ;
#19529 = CARTESIAN_POINT ( 'NONE',  ( 25.13768435607400065, 1440.913060398800098, 216.9184046046830190 ) ) ;
#19530 = DIRECTION ( 'NONE',  ( 1.224227143275421080E-16, 0.02617694830808806397, -0.9996573249755517088 ) ) ;
#19531 = CARTESIAN_POINT ( 'NONE',  ( 2.931378713556060056, 1425.355483872539935, 188.8538262268459960 ) ) ;
#19532 = VERTEX_POINT ( 'NONE', #41717 ) ;
#19533 = CYLINDRICAL_SURFACE ( 'NONE', #44817, 2.000000000000001776 ) ;
#19534 = CARTESIAN_POINT ( 'NONE',  ( 21.31355172050000135, 1471.299568759730164, 210.6477759654979991 ) ) ;
#19535 = CARTESIAN_POINT ( 'NONE',  ( -12.27011089310000003, 1486.375363512730246, 184.4446487454979717 ) ) ;
#19536 = B_SPLINE_CURVE_WITH_KNOTS ( 'NONE', 3,
 ( #57045, #27277, #94462, #59793, #9921, #52498, #95037, #70421, #87758, #42985 ),
 .UNSPECIFIED., .F., .F.,
 ( 4, 2, 2, 2, 4 ),
 ( 0.000000000000000000, 0.2500000000000000000, 0.5000000000000000000, 0.7500000000000000000, 1.000000000000000000 ),
 .UNSPECIFIED. ) ;
#19537 = CARTESIAN_POINT ( 'NONE',  ( 3.461063783934097859, 1398.015735858593189, 196.5635239469207249 ) ) ;
#19538 = CARTESIAN_POINT ( 'NONE',  ( 1.726858845490000016, 1482.796399391929981, 235.4332745692979927 ) ) ;
#19539 = AXIS2_PLACEMENT_3D ( 'NONE', #45459, #11291, #105899 ) ;
#19540 = CARTESIAN_POINT ( 'NONE',  ( 25.96988284260000057, 1469.243118069030061, 212.2965549575379782 ) ) ;
#19541 = EDGE_CURVE ( 'NONE', #79144, #100188, #35297, .T. ) ;
#19542 = CARTESIAN_POINT ( 'NONE',  ( -15.99924670575417274, 1420.237028991483839, 209.6647657703803702 ) ) ;
#19543 = CARTESIAN_POINT ( 'NONE',  ( -17.74011923890000020, 1509.475909753130054, 231.2409737833980046 ) ) ;
#19544 = CARTESIAN_POINT ( 'NONE',  ( -20.48566081668520056, 1383.853069179059958, 220.9684220193649935 ) ) ;
#19545 = CARTESIAN_POINT ( 'NONE',  ( -4.987082939647749846, 1508.551704408389924, 205.8487953860969810 ) ) ;
#19546 = CARTESIAN_POINT ( 'NONE',  ( 18.64618896912524448, 1416.835806650408813, 209.6841501312022160 ) ) ;
#19547 = CARTESIAN_POINT ( 'NONE',  ( -28.15442856212169787, 1509.896234822020006, 200.8410265843269826 ) ) ;
#19548 = CARTESIAN_POINT ( 'NONE',  ( 9.078035843596250487, 1451.272942437749862, 210.9408701583590187 ) ) ;
#19550 = ORIENTED_EDGE ( 'NONE', *, *, #21692, .F. ) ;
#19549 = CARTESIAN_POINT ( 'NONE',  ( 5.083972363190000898, 1436.382653089989844, 207.1318876291190350 ) ) ;
#19551 = CARTESIAN_POINT ( 'NONE',  ( -28.46619500829999794, 1445.052233488290085, 168.7181723459979992 ) ) ;
#19552 = AXIS2_PLACEMENT_3D ( 'NONE', #15554, #58154, #92284 ) ;
#19553 = CARTESIAN_POINT ( 'NONE',  ( -3.078458325710000221, 1378.867273990040076, 208.5251302500439863 ) ) ;
#19554 = CARTESIAN_POINT ( 'NONE',  ( -5.457743909444250363, 1440.715679462449998, 154.7912908061040014 ) ) ;
#19556 = EDGE_LOOP ( 'NONE', ( #97666, #32705, #9030, #84849 ) ) ;
#19555 = CARTESIAN_POINT ( 'NONE',  ( -31.97146249857350853, 1524.678872986481565, 216.6705896045354791 ) ) ;
#19557 = CARTESIAN_POINT ( 'NONE',  ( -6.763867816925220211, 1508.551704407960187, 219.2477951563350018 ) ) ;
#19558 = ORIENTED_EDGE ( 'NONE', *, *, #27442, .T. ) ;
#19559 = CARTESIAN_POINT ( 'NONE',  ( 6.501609782144663896, 1517.051704408389924, 217.4228972380528262 ) ) ;
#19560 = CARTESIAN_POINT ( 'NONE',  ( 2.091623246919999790, 1485.160878225490251, 201.4201072810890025 ) ) ;
#19561 = CARTESIAN_POINT ( 'NONE',  ( -8.311471914476035394, 1509.203303456682079, 237.2547473838516794 ) ) ;
#19562 = DIRECTION ( 'NONE',  ( 0.9950083946325752882, 0.09971571435232254310, -0.003882128528443905269 ) ) ;
#19563 = CARTESIAN_POINT ( 'NONE',  ( -2.427501210939999599, 1432.717019920590019, 217.9482129255790142 ) ) ;
#19564 = CARTESIAN_POINT ( 'NONE',  ( -15.05548819430000052, 1420.901177493080013, 212.6278861834389886 ) ) ;
#19565 = CARTESIAN_POINT ( 'NONE',  ( 12.02250444982000133, 1409.332895484829805, 218.0033144737150224 ) ) ;
#19566 = CARTESIAN_POINT ( 'NONE',  ( 5.314807373273278124, 1420.217340012715113, 137.0999999980982125 ) ) ;
#19567 = CARTESIAN_POINT ( 'NONE',  ( -95.92464888116629140, 1385.210119995399964, 295.2644287896150104 ) ) ;
#19569 = ADVANCED_FACE ( 'NONE', ( #60758 ), #26445, .T. ) ;
#19568 = EDGE_CURVE ( 'NONE', #74353, #74738, #22852, .T. ) ;
#19570 = CARTESIAN_POINT ( 'NONE',  ( -17.63667811080000192, 1430.609996739030066, 191.3996239150980045 ) ) ;
#19571 = CARTESIAN_POINT ( 'NONE',  ( -54.25698729759999850, 1379.746222734200046, 249.0120014888590276 ) ) ;
#19572 = ORIENTED_EDGE ( 'NONE', *, *, #79699, .F. ) ;
#19573 = AXIS2_PLACEMENT_3D ( 'NONE', #12097, #72574, #46292 ) ;
#19574 = CARTESIAN_POINT ( 'NONE',  ( 11.84326266240529968, 1491.682748273859943, 208.2990869752020160 ) ) ;
#19576 = ORIENTED_EDGE ( 'NONE', *, *, #58040, .F. ) ;
#19575 = CARTESIAN_POINT ( 'NONE',  ( -4.073851350468440380, 1438.760108550490258, 227.2697485756019944 ) ) ;
#19577 = ORIENTED_EDGE ( 'NONE', *, *, #26368, .T. ) ;
#19578 = ADVANCED_FACE ( 'NONE', ( #1381 ), #31775, .T. ) ;
#19579 = CARTESIAN_POINT ( 'NONE',  ( -11.86597105770560034, 1415.542389211330146, 195.0589158601300142 ) ) ;
#19580 = CARTESIAN_POINT ( 'NONE',  ( -0.7279988002571550210, 1361.403840689056096, 207.6218459616988241 ) ) ;
#19581 = CARTESIAN_POINT ( 'NONE',  ( -11.52394156360000110, 1434.100698262960123, 151.3697489037979835 ) ) ;
#19582 = CARTESIAN_POINT ( 'NONE',  ( 28.36448145873015036, 1509.903571177603226, 216.7772950919570292 ) ) ;
#19583 = CARTESIAN_POINT ( 'NONE',  ( 5.077070885040000370, 1398.064298510030085, 221.1616505512979813 ) ) ;
#19584 = CARTESIAN_POINT ( 'NONE',  ( 32.70814417905861404, 1524.201816949777822, 201.1172774233197913 ) ) ;
#19585 = CARTESIAN_POINT ( 'NONE',  ( -6.039224196466708605, 1516.749004811059876, 213.5695341108769583 ) ) ;
#19586 = CARTESIAN_POINT ( 'NONE',  ( -1.187216277370000128, 1457.285143779230111, 183.3846202966979888 ) ) ;
#19587 = CARTESIAN_POINT ( 'NONE',  ( -10.96801198806809374, 1364.355713703397896, 207.6218459616987673 ) ) ;
#19588 = DIRECTION ( 'NONE',  ( 0.07713599384728243857, -0.9969860201949397593, -0.008301444997534272036 ) ) ;
#19589 = CARTESIAN_POINT ( 'NONE',  ( -7.338753868364999988, 1517.184383877180153, 206.8309596656170015 ) ) ;
#19590 = CARTESIAN_POINT ( 'NONE',  ( -12.99817078242380042, 1434.787734094880079, 149.3751819043959870 ) ) ;
#19591 = B_SPLINE_SURFACE_WITH_KNOTS ( 'NONE', 5, 5, ( 
 ( #44955, #71834, #46606, #2410, #46055, #95881 ),
 ( #80740, #105953, #36527, #96439, #70723, #21345 ),
 ( #4048, #19717, #20809, #96999, #104835, #55007 ),
 ( #38175, #29771, #29231, #72355, #27573, #106486 ),
 ( #28122, #47142, #63960, #105391, #80188, #81268 ),
 ( #28682, #62315, #53920, #98075, #88055, #11339 ),
 ( #2958, #55551, #45512, #20262, #89677, #79653 ),
 ( #37075, #62889, #54462, #88600, #11883, #75107 ),
 ( #109255, #5689, #57211, #65602, #15692, #47690 ) ),
 .UNSPECIFIED., .F., .F., .F.,
 ( 6, 3, 6 ),
 ( 6, 6 ),
 ( 0.7655572723410000169, 2.316155491850000026, 3.835724788489999870 ),
 ( 0.000000000000000000, 1.000000000000000000 ),
 .UNSPECIFIED. ) ;
#19592 = FACE_OUTER_BOUND ( 'NONE', #19632, .T. ) ;
#19593 = DIRECTION ( 'NONE',  ( 0.8775825618903774217, -3.365001152038843908E-31, 0.4794255386041944567 ) ) ;
#19594 = CARTESIAN_POINT ( 'NONE',  ( 2.135980618300000078, 1495.504087388789912, 220.8536851825989800 ) ) ;
#19595 = CARTESIAN_POINT ( 'NONE',  ( -109.1655177890000061, 1384.872414444939977, 297.1329087538589420 ) ) ;
#19596 = ORIENTED_EDGE ( 'NONE', *, *, #63723, .F. ) ;
#19597 = CARTESIAN_POINT ( 'NONE',  ( 14.25478695230000170, 1406.894174824430138, 267.1909361702979595 ) ) ;
#19598 = CARTESIAN_POINT ( 'NONE',  ( -27.21299276520000276, 1488.689717875729912, 207.6915820717080123 ) ) ;
#19599 = B_SPLINE_CURVE_WITH_KNOTS ( 'NONE', 5,
 ( #96194, #2164, #46784, #69359, #53104, #47310, #1051, #17792, #78854, #51992, #86133, #104033 ),
 .UNSPECIFIED., .F., .F.,
 ( 6, 3, 3, 6 ),
 ( 0.000000000000000000, 0.3237431521556269343, 0.7745810507185086902, 1.000000000000000000 ),
 .UNSPECIFIED. ) ;
#19601 = CARTESIAN_POINT ( 'NONE',  ( 3.378657952879999992E-14, 1414.110153932129833, 261.8343058782979824 ) ) ;
#19600 = CARTESIAN_POINT ( 'NONE',  ( -11.02774336400820054, 1426.509921592220053, 92.74671990447460246 ) ) ;
#19602 = CARTESIAN_POINT ( 'NONE',  ( -2.282915221395000138, 1516.876240617270014, 211.6158662526670184 ) ) ;
#19603 = CARTESIAN_POINT ( 'NONE',  ( -21.36149126229999951, 1471.309244717429920, 207.7943419303680344 ) ) ;
#19604 = VECTOR ( 'NONE', #9375, 1000.000000000000000 ) ;
#19605 = CARTESIAN_POINT ( 'NONE',  ( -38.77640472460000609, 1433.500816082299934, 259.1404853845979801 ) ) ;
#19606 = CARTESIAN_POINT ( 'NONE',  ( 2.869680150050000211, 1485.441877061090054, 219.8814458974989918 ) ) ;
#19607 = CARTESIAN_POINT ( 'NONE',  ( 29.75012120190000076, 1509.993914123429931, 209.6841247587719863 ) ) ;
#19608 = CARTESIAN_POINT ( 'NONE',  ( 2.864408029580055803, 1447.807653760355834, 154.7916318795152506 ) ) ;
#19609 = CARTESIAN_POINT ( 'NONE',  ( 33.14188703010000125, 1450.895165025899814, 136.1944683724980223 ) ) ;
#19610 = ORIENTED_EDGE ( 'NONE', *, *, #48922, .F. ) ;
#19611 = CARTESIAN_POINT ( 'NONE',  ( -5.386577890436130112, 1432.378605031630059, 154.6079252277549756 ) ) ;
#19612 = CARTESIAN_POINT ( 'NONE',  ( 13.20762147703265654, 1513.543684532346106, 225.9078262356120774 ) ) ;
#19613 = B_SPLINE_CURVE_WITH_KNOTS ( 'NONE', 5,
 ( #22959, #90731, #108081, #31376, #65558, #54959, #91289, #89087, #48760 ),
 .UNSPECIFIED., .F., .F.,
 ( 6, 3, 6 ),
 ( 0.000000000000000000, 0.5000000000000000000, 1.000000000000000000 ),
 .UNSPECIFIED. ) ;
#19614 = CARTESIAN_POINT ( 'NONE',  ( 38.48250450508500364, 1443.291876352919871, 137.1415221903349959 ) ) ;
#19615 = VERTEX_POINT ( 'NONE', #70275 ) ;
#19616 = EDGE_LOOP ( 'NONE', ( #51925, #38891, #10932, #19517, #25132 ) ) ;
#19617 = CARTESIAN_POINT ( 'NONE',  ( 9.485899553554340002, 1452.846731054919928, 211.4225977852020151 ) ) ;
#19618 = CARTESIAN_POINT ( 'NONE',  ( -2.114480094995805359, 1486.828170616315219, 220.1547108737681526 ) ) ;
#19619 = ORIENTED_EDGE ( 'NONE', *, *, #82518, .F. ) ;
#19620 = CARTESIAN_POINT ( 'NONE',  ( -1.072088845450000161, 1412.065175156030136, 185.2438394658980201 ) ) ;
#19621 = CARTESIAN_POINT ( 'NONE',  ( -6.144022937698749409, 1419.445111502675900, 195.0001984287017081 ) ) ;
#19622 = CARTESIAN_POINT ( 'NONE',  ( -11.87414320589479999, 1432.940728692309904, 149.9807111271900055 ) ) ;
#19623 = CARTESIAN_POINT ( 'NONE',  ( -1.174483211909999936, 1470.486737867530110, 235.5973338944980071 ) ) ;
#19624 = CARTESIAN_POINT ( 'NONE',  ( 6.766140024152450749, 1508.878901399440110, 201.8613017694559915 ) ) ;
#19625 = CARTESIAN_POINT ( 'NONE',  ( 46.27886946470769658, 1440.912966750240003, 267.5894436979959892 ) ) ;
#19626 = CARTESIAN_POINT ( 'NONE',  ( 6.177640194960000386, 1462.009621597289879, 206.9307941614490289 ) ) ;
#19627 = CARTESIAN_POINT ( 'NONE',  ( 0.03533291443150000238, 1420.203121373229806, 183.8975548986979902 ) ) ;
#19628 = VERTEX_POINT ( 'NONE', #85356 ) ;
#19629 =( BOUNDED_CURVE ( )  B_SPLINE_CURVE ( 3, ( #88253, #45722, #3169, #63093 ),
 .UNSPECIFIED., .F., .F. ) 
 B_SPLINE_CURVE_WITH_KNOTS ( ( 4, 4 ),
 ( 4.245054931713185375, 5.179005799894629725 ),
 .UNSPECIFIED. ) 
 CURVE ( )  GEOMETRIC_REPRESENTATION_ITEM ( )  RATIONAL_B_SPLINE_CURVE ( ( 1.000000000000000000, 0.9286226616644226439, 0.9286226616644226439, 1.000000000000000000 ) ) 
 REPRESENTATION_ITEM ( '' )  );
#19630 = CARTESIAN_POINT ( 'NONE',  ( -3.455378015385000001, 1516.627618683580067, 202.1863880069169852 ) ) ;
#19631 = CARTESIAN_POINT ( 'NONE',  ( -1.119592219845000125, 1516.958737650239982, 210.2577447559170025 ) ) ;
#19632 = EDGE_LOOP ( 'NONE', ( #96817, #50831, #31606, #8728 ) ) ;
#19633 = CARTESIAN_POINT ( 'NONE',  ( 11.85901083361419950, 1431.841316764000112, 149.9599341808090003 ) ) ;
#19634 = CARTESIAN_POINT ( 'NONE',  ( 12.78853242329685891, 1444.985736185042470, 186.5280363921234539 ) ) ;
#19635 = EDGE_LOOP ( 'NONE', ( #50974, #52674, #104503, #2254 ) ) ;
#19636 = CARTESIAN_POINT ( 'NONE',  ( -0.9490323356187280179, 1507.925252277985237, 221.0232043774789759 ) ) ;
#19637 = CARTESIAN_POINT ( 'NONE',  ( -6.585747151019099022, 1508.339498974060007, 219.9410548752989882 ) ) ;
#19638 = DIRECTION ( 'NONE',  ( -1.000000000000000000, -5.823966869780000474E-19, 4.137698748469999823E-18 ) ) ;
#19639 = CARTESIAN_POINT ( 'NONE',  ( -9.683432862967901400, 1470.976754966750150, 212.5624612103730158 ) ) ;
#19640 = CARTESIAN_POINT ( 'NONE',  ( 15.79557044279290068, 1452.361466912919923, 147.2817071249239973 ) ) ;
#19641 = AXIS2_PLACEMENT_3D ( 'NONE', #63951, #38708, #56079 ) ;
#19642 = CARTESIAN_POINT ( 'NONE',  ( 2.339366202910509784, 1407.692004809400260, 270.1366117308560320 ) ) ;
#19643 = CARTESIAN_POINT ( 'NONE',  ( -107.7923298369999969, 1386.973993580999831, 297.6574877858589616 ) ) ;
#19644 = CARTESIAN_POINT ( 'NONE',  ( -5.546142131579999912, 1474.984681366790028, 200.2534476738289868 ) ) ;
#19645 = CARTESIAN_POINT ( 'NONE',  ( 11.60004869885203682, 1422.222932908421853, 135.5999999980979851 ) ) ;
#19646 = CARTESIAN_POINT ( 'NONE',  ( -37.91547825339999633, 1379.647889607849947, 220.5156237355589894 ) ) ;
#19647 = FACE_OUTER_BOUND ( 'NONE', #79674, .T. ) ;
#19649 = CARTESIAN_POINT ( 'NONE',  ( 14.35483055539999953, 1416.837177098629809, 196.6648191809980233 ) ) ;
#19648 = CARTESIAN_POINT ( 'NONE',  ( -15.05712110500000023, 1503.430198388489998, 209.1799330422220180 ) ) ;
#19650 = CARTESIAN_POINT ( 'NONE',  ( -19.29595629980909877, 1379.713387097429404, 212.5268654157613355 ) ) ;
#19651 = CARTESIAN_POINT ( 'NONE',  ( 17.66473809693500030, 1412.789316240470043, 224.8635844683609832 ) ) ;
#19652 = CARTESIAN_POINT ( 'NONE',  ( -7.570419153255000033, 1513.830194289050041, 202.8006730981169596 ) ) ;
#19653 = ORIENTED_EDGE ( 'NONE', *, *, #34105, .F. ) ;
#19654 = CARTESIAN_POINT ( 'NONE',  ( 32.79207797800000179, 1428.560640288129889, 262.6648722463980334 ) ) ;
#19655 = AXIS2_PLACEMENT_3D ( 'NONE', #55554, #68924, #92420 ) ;
#19656 = DIRECTION ( 'NONE',  ( -0.7414773880254664773, 0.000000000000000000, 0.6709778558543730842 ) ) ;
#19657 = CARTESIAN_POINT ( 'NONE',  ( -55.97777492769100149, 1385.087189547780099, 273.6896789270770114 ) ) ;
#19658 = CARTESIAN_POINT ( 'NONE',  ( -19.39983987834945012, 1522.861859112239244, 178.9515629540100861 ) ) ;
#19659 = CARTESIAN_POINT ( 'NONE',  ( 3.964328110410000328, 1507.304896082889854, 220.1351224040989791 ) ) ;
#19660 = CARTESIAN_POINT ( 'NONE',  ( -15.04150367899999985, 1415.861021494549959, 212.2455458053489963 ) ) ;
#19662 = EDGE_LOOP ( 'NONE', ( #37097, #66539, #66617, #16543, #9816, #104895, #107372 ) ) ;
#19661 = CARTESIAN_POINT ( 'NONE',  ( -0.9669097429813701128, 1515.111355597239935, 204.7936164732989823 ) ) ;
#19663 = CARTESIAN_POINT ( 'NONE',  ( -15.86313006842250317, 1415.917248183199717, 209.7285344443807276 ) ) ;
#19664 = CARTESIAN_POINT ( 'NONE',  ( -24.81337094160000234, 1443.616293363810200, 210.6361221007779818 ) ) ;
#19665 = CARTESIAN_POINT ( 'NONE',  ( -1.843570366231615631, 1450.382637347590162, 154.3039494713565603 ) ) ;
#19666 = CARTESIAN_POINT ( 'NONE',  ( 1.529355925611250111, 1430.956820494460089, 199.7836114767660263 ) ) ;
#19667 = CARTESIAN_POINT ( 'NONE',  ( 11.95959062223499991, 1513.007288725360013, 225.7330057136669836 ) ) ;
#19668 = CARTESIAN_POINT ( 'NONE',  ( -11.95688248459999947, 1441.464442770860160, 187.7513092272979804 ) ) ;
#19669 = CARTESIAN_POINT ( 'NONE',  ( 6.436778620621919522, 1509.137837650079973, 179.8165091018489932 ) ) ;
#19670 = CARTESIAN_POINT ( 'NONE',  ( -17.17241001986462123, 1518.913060387330006, 238.6251415217917895 ) ) ;
#19671 = CARTESIAN_POINT ( 'NONE',  ( 12.20256845149948610, 1434.091510794637998, 149.6914622690949273 ) ) ;
#19672 = CARTESIAN_POINT ( 'NONE',  ( 11.80820258149999979, 1417.418794541129955, 229.4144358672980104 ) ) ;
#19673 = CARTESIAN_POINT ( 'NONE',  ( 9.875005135842670256, 1469.705720279170237, 211.0604535260579837 ) ) ;
#19674 = CARTESIAN_POINT ( 'NONE',  ( -16.91862346270000117, 1461.030957408330096, 228.2759457765980073 ) ) ;
#19675 = AXIS2_PLACEMENT_3D ( 'NONE', #45189, #96683, #62564 ) ;
#19676 = CARTESIAN_POINT ( 'NONE',  ( -1.717084749545000122, 1516.819260244609950, 206.6456753351970121 ) ) ;
#19677 = CARTESIAN_POINT ( 'NONE',  ( 45.48702313900000149, 1436.948642006169848, 266.1936685609980486 ) ) ;
#19678 = CARTESIAN_POINT ( 'NONE',  ( -18.49972780619999924, 1410.921726043829949, 223.9058259105980255 ) ) ;
#19679 = CARTESIAN_POINT ( 'NONE',  ( -32.77044109517562021, 1525.581535527370534, 219.1629015078874829 ) ) ;
#19680 = CARTESIAN_POINT ( 'NONE',  ( 18.04150427010000257, 1436.361837209869918, 147.3508937178980034 ) ) ;
#19681 = CARTESIAN_POINT ( 'NONE',  ( 26.64435021830000139, 1508.005964801830032, 204.3334252420080190 ) ) ;
#19682 = CARTESIAN_POINT ( 'NONE',  ( 5.374504625227119803, 1429.015749531610027, 154.0247573729420196 ) ) ;
#19683 = ADVANCED_FACE ( 'NONE', ( #77537 ), #28200, .F. ) ;
#19684 = CARTESIAN_POINT ( 'NONE',  ( -14.31803753242949817, 1379.584910753419990, 207.9694682050350139 ) ) ;
#19685 = FACE_OUTER_BOUND ( 'NONE', #30382, .T. ) ;
#19686 = FACE_OUTER_BOUND ( 'NONE', #33473, .T. ) ;
#19687 = CARTESIAN_POINT ( 'NONE',  ( -38.35651281120340172, 1437.646912403469969, 136.3196577860490208 ) ) ;
#19688 = DIRECTION ( 'NONE',  ( -0.001339522651315419892, 0.9999644786255611484, 0.008321488218843280452 ) ) ;
#19689 = CARTESIAN_POINT ( 'NONE',  ( -18.18905553120000107, 1416.520322350429979, 205.1726131530880082 ) ) ;
#19690 = AXIS2_PLACEMENT_3D ( 'NONE', #110486, #70586, #36942 ) ;
#19691 = CARTESIAN_POINT ( 'NONE',  ( -11.98663175510000123, 1441.172953348979945, 187.7782422411980008 ) ) ;
#19692 = EDGE_CURVE ( 'NONE', #967, #80823, #97869, .T. ) ;
#19693 = DIRECTION ( 'NONE',  ( 0.000000000000000000, 0.000000000000000000, -1.000000000000000000 ) ) ;
#19694 = CARTESIAN_POINT ( 'NONE',  ( -33.93529342339999744, 1435.841716433050124, 135.9421945811979811 ) ) ;
#19695 = CARTESIAN_POINT ( 'NONE',  ( 21.02608924029999926, 1456.853724928630072, 225.6706377209980303 ) ) ;
#19696 = VERTEX_POINT ( 'NONE', #44493 ) ;
#19697 = CARTESIAN_POINT ( 'NONE',  ( -2.566007203944999926, 1512.021995456199875, 201.5004268114669799 ) ) ;
#19698 = CARTESIAN_POINT ( 'NONE',  ( -6.394947566795919691, 1409.136376877240082, 222.6614285949029863 ) ) ;
#19699 = CARTESIAN_POINT ( 'NONE',  ( 31.97743984922253446, 1525.878013734321485, 198.0760624713124969 ) ) ;
#19700 = CARTESIAN_POINT ( 'NONE',  ( 17.17760792425680094, 1517.051704368240053, 222.7507317666290305 ) ) ;
#19701 = CARTESIAN_POINT ( 'NONE',  ( 0.000000000000000000, 1512.187213306747481, 209.1218459616979999 ) ) ;
#19702 = CARTESIAN_POINT ( 'NONE',  ( -45.88374573399999434, 1446.003351892490173, 266.4124074795980164 ) ) ;
#19703 = CARTESIAN_POINT ( 'NONE',  ( -13.08223627748380125, 1428.818921846599778, 222.3767532333990005 ) ) ;
#19704 = CYLINDRICAL_SURFACE ( 'NONE', #76343, 1.999999999999999556 ) ;
#19705 = CARTESIAN_POINT ( 'NONE',  ( 20.07149347155292318, 1526.186458717542791, 233.0642689910310139 ) ) ;
#19706 = CARTESIAN_POINT ( 'NONE',  ( -89.21435300837349303, 1384.620659748430171, 308.4344151408140533 ) ) ;
#19707 = CARTESIAN_POINT ( 'NONE',  ( -40.27720933358730093, 1384.990567941889822, 213.1516827062340269 ) ) ;
#19708 = DIRECTION ( 'NONE',  ( 0.000000000000000000, 1.000000000000000000, -0.000000000000000000 ) ) ;
#19709 = CARTESIAN_POINT ( 'NONE',  ( 16.04707966210000336, 1416.518532928429977, 217.6280249965379880 ) ) ;
#19710 = CARTESIAN_POINT ( 'NONE',  ( -11.86590139589999815, 1432.348266868109931, 151.0567667964980103 ) ) ;
#19711 = CARTESIAN_POINT ( 'NONE',  ( -2.253566441613126910E-10, 1426.918876941764893, 137.0999999980980135 ) ) ;
#19712 = DIRECTION ( 'NONE',  ( -1.156023075842281927E-31, 1.000000000000000000, -1.698192320643030073E-16 ) ) ;
#19713 = CARTESIAN_POINT ( 'NONE',  ( -8.156587067910001210, 1384.920246153470089, 199.6468409925089986 ) ) ;
#19714 = CARTESIAN_POINT ( 'NONE',  ( 5.327762952207462099, 1422.321577162126232, 138.7600416031628754 ) ) ;
#19715 = EDGE_CURVE ( 'NONE', #49951, #88894, #66931, .T. ) ;
#19716 = CARTESIAN_POINT ( 'NONE',  ( 15.32781700640000011, 1414.971279908829956, 201.8289935246679931 ) ) ;
#19717 = CARTESIAN_POINT ( 'NONE',  ( -12.39598156289999942, 1416.274718424630009, 194.8162290544979953 ) ) ;
#19718 = TOROIDAL_SURFACE ( 'NONE', #14352, 24.69926344187880929, 1.000000000000000000 ) ;
#19719 = CARTESIAN_POINT ( 'NONE',  ( 0.1559730049430000098, 1467.142443652729980, 235.6419144452979992 ) ) ;
#19720 = CARTESIAN_POINT ( 'NONE',  ( 23.52564803090000112, 1410.656144928030244, 211.7451932072379748 ) ) ;
#19721 = B_SPLINE_SURFACE_WITH_KNOTS ( 'NONE', 4, 5, ( 
 ( #75765, #15277, #57336, #83591, #109913, #64629 ),
 ( #98749, #65169, #6890, #22559, #14184, #91462 ),
 ( #41046, #14740, #76311, #25882, #86914, #18582 ),
 ( #52777, #43816, #18038, #101481, #86359, #67934 ),
 ( #110462, #27016, #93635, #61206, #102584, #94762 ) ),
 .UNSPECIFIED., .F., .F., .F.,
 ( 5, 5 ),
 ( 6, 6 ),
 ( 30.35883180189999919, 49.62971790979390363 ),
 ( -0.001138638393163039862, 2.001138639208579928 ),
 .UNSPECIFIED. ) ;
#19722 = CARTESIAN_POINT ( 'NONE',  ( -12.07610166159999920, 1433.870589910030048, 149.7869025145980117 ) ) ;
#19723 = CARTESIAN_POINT ( 'NONE',  ( -2.711451550492540274, 1449.129774548599926, 188.5718384860999777 ) ) ;
#19724 = CARTESIAN_POINT ( 'NONE',  ( -4.523944140811339665, 1455.378620635879997, 200.8408219016489795 ) ) ;
#19726 = CARTESIAN_POINT ( 'NONE',  ( -11.39873841100000007, 1380.703654181990032, 203.1461614638990056 ) ) ;
#19725 = CARTESIAN_POINT ( 'NONE',  ( -11.86735416189999803, 1432.439689909539993, 150.3969688813980099 ) ) ;
#19727 = CARTESIAN_POINT ( 'NONE',  ( -0.1180586146000000003, 1410.296227586130044, 233.2638028148980140 ) ) ;
#19728 = DIRECTION ( 'NONE',  ( 0.1189347811660100146, -0.4481226533063590312, 0.8860251720028400335 ) ) ;
#19729 = AXIS2_PLACEMENT_3D ( 'NONE', #15709, #109269, #23586 ) ;
#19730 = FACE_OUTER_BOUND ( 'NONE', #74865, .T. ) ;
#19731 = CARTESIAN_POINT ( 'NONE',  ( 20.41258333560000082, 1494.156730172889866, 204.1224707391089908 ) ) ;
#19732 = CARTESIAN_POINT ( 'NONE',  ( 9.774666768839999520, 1462.791335443590015, 210.7173514753790187 ) ) ;
#19733 = CARTESIAN_POINT ( 'NONE',  ( 5.774609621945000271, 1516.777260590120022, 204.5018377250270021 ) ) ;
#19734 = CARTESIAN_POINT ( 'NONE',  ( -19.98479248519999985, 1427.060832424730052, 224.6412401930980138 ) ) ;
#19735 = CARTESIAN_POINT ( 'NONE',  ( -18.69214414528729762, 1485.716420687259870, 189.3114983721589795 ) ) ;
#19736 = CIRCLE ( 'NONE', #37647, 1.999999999999999556 ) ;
#19737 = DIRECTION ( 'NONE',  ( 5.980589973904019347E-17, -1.000000000000000000, 1.736889445713099699E-16 ) ) ;
#19738 = CARTESIAN_POINT ( 'NONE',  ( -12.18049167383413156, 1421.733962334860962, 210.6454646573376692 ) ) ;
#19740 = ORIENTED_EDGE ( 'NONE', *, *, #45419, .F. ) ;
#19739 = CARTESIAN_POINT ( 'NONE',  ( -65.79241599563980003, 1379.740566815069997, 276.1610046520289643 ) ) ;
#19741 = VERTEX_POINT ( 'NONE', #108733 ) ;
#19742 = CARTESIAN_POINT ( 'NONE',  ( 4.329448781177520189, 1515.064792686469900, 207.2788827064790098 ) ) ;
#19743 = VERTEX_POINT ( 'NONE', #34225 ) ;
#19744 = CARTESIAN_POINT ( 'NONE',  ( -105.5263324250000068, 1378.950045411100064, 305.1391035067590565 ) ) ;
#19745 = CARTESIAN_POINT ( 'NONE',  ( 11.82750276210000173, 1499.979357237489921, 206.0369006055389889 ) ) ;
#19747 = CARTESIAN_POINT ( 'NONE',  ( 13.89716773895519886, 1452.853908481549979, 223.9136441993209985 ) ) ;
#19746 = CARTESIAN_POINT ( 'NONE',  ( -15.72888735940112070, 1409.636818260307336, 226.0013290851642580 ) ) ;
#19748 = CARTESIAN_POINT ( 'NONE',  ( 0.000000000000000000, 1523.409940573003951, 185.4225825198192013 ) ) ;
#19749 = CARTESIAN_POINT ( 'NONE',  ( -24.89146661867219734, 1451.594294999959857, 137.4462232438879994 ) ) ;
#19750 = CARTESIAN_POINT ( 'NONE',  ( -106.1387134729239961, 1378.913060388289978, 305.7024349280350179 ) ) ;
#19751 = CARTESIAN_POINT ( 'NONE',  ( 9.199108954039999730, 1410.609401603230026, 230.1463904532980109 ) ) ;
#19752 =( LENGTH_UNIT ( ) NAMED_UNIT ( * ) SI_UNIT ( .MILLI., .METRE. ) );
#19753 = CARTESIAN_POINT ( 'NONE',  ( -6.547556969464999987, 1516.633288330999903, 212.3841106205370011 ) ) ;
#19754 = CARTESIAN_POINT ( 'NONE',  ( 41.66188030070000536, 1443.705283505699754, 134.0999999982089719 ) ) ;
#19755 = CARTESIAN_POINT ( 'NONE',  ( -4.192418968486159692, 1427.449526014519961, 207.6357443616469993 ) ) ;
#19756 = CARTESIAN_POINT ( 'NONE',  ( 9828.720208560080209, 54.28084071072819938, -1083.674256113199817 ) ) ;
#19757 = VERTEX_POINT ( 'NONE', #15199 ) ;
#19758 = CARTESIAN_POINT ( 'NONE',  ( 14.48646706370279880, 1435.954295751229893, 149.8410885043270184 ) ) ;
#19759 = CARTESIAN_POINT ( 'NONE',  ( 1.227353608591539968, 1432.824896673809917, 200.7599812625429934 ) ) ;
#19760 = ORIENTED_EDGE ( 'NONE', *, *, #55052, .T. ) ;
#19761 = ORIENTED_EDGE ( 'NONE', *, *, #60018, .F. ) ;
#19762 = ORIENTED_EDGE ( 'NONE', *, *, #2284, .T. ) ;
#19763 = CARTESIAN_POINT ( 'NONE',  ( -8.232567760474999830, 1512.371207877109782, 215.7807634015769906 ) ) ;
#19764 = CARTESIAN_POINT ( 'NONE',  ( -0.7051069384629999881, 1465.998960783829943, 235.7578936505979925 ) ) ;
#19765 = AXIS2_PLACEMENT_3D ( 'NONE', #81094, #45324, #19530 ) ;
#19766 = CARTESIAN_POINT ( 'NONE',  ( 21.25084690298298895, 1450.939921383146611, 144.1607677896775783 ) ) ;
#19767 = CARTESIAN_POINT ( 'NONE',  ( -8.297791668369999485, 1384.930381111709949, 218.7035399147090118 ) ) ;
#19768 = CARTESIAN_POINT ( 'NONE',  ( 9.698064379080001629, 1462.705242066090022, 208.0596161272490292 ) ) ;
#19769 = CARTESIAN_POINT ( 'NONE',  ( -17.47882303318302277, 1448.297325624284440, 218.1748229397720706 ) ) ;
#19770 = CARTESIAN_POINT ( 'NONE',  ( 13.30361758462239941, 1409.377634028029888, 191.9462312207510308 ) ) ;
#19771 = CARTESIAN_POINT ( 'NONE',  ( 2.846372769239999823, 1466.158655091689980, 198.4435757763990011 ) ) ;
#19772 = CARTESIAN_POINT ( 'NONE',  ( 0.3083299013670000033, 1507.389591484829907, 237.3685675047980226 ) ) ;
#19773 = VERTEX_POINT ( 'NONE', #109838 ) ;
#19774 = CARTESIAN_POINT ( 'NONE',  ( 6.933587655514999781, 1516.542957540330008, 207.4124872689769745 ) ) ;
#19775 = VERTEX_POINT ( 'NONE', #66759 ) ;
#19776 = CARTESIAN_POINT ( 'NONE',  ( 25.13830754042900040, 1440.913060387330006, 239.5563470660360110 ) ) ;
#19777 = TOROIDAL_SURFACE ( 'NONE', #9066, 11.99982860380000105, 0.5000000000000000000 ) ;
#19778 = CARTESIAN_POINT ( 'NONE',  ( 11.75386664412339854, 1479.308097208950130, 208.5149014641469876 ) ) ;
#19779 = ORIENTED_EDGE ( 'NONE', *, *, #20513, .F. ) ;
#19780 = CARTESIAN_POINT ( 'NONE',  ( 25.74039302815520003, 1448.986371477839839, 137.5027126072619978 ) ) ;
#19781 = CARTESIAN_POINT ( 'NONE',  ( -13.86209743629999913, 1409.397135496529927, 191.7555771504979987 ) ) ;
#19782 = CARTESIAN_POINT ( 'NONE',  ( -27.47436269071217296, 1379.622196554404354, 216.6943055741242006 ) ) ;
#19784 = CARTESIAN_POINT ( 'NONE',  ( 19.75641515910000123, 1473.226389329089898, 205.2875698398590316 ) ) ;
#19783 = CARTESIAN_POINT ( 'NONE',  ( -24.41225618889999893, 1441.001746037479961, 212.0330686186080129 ) ) ;
#19785 = CARTESIAN_POINT ( 'NONE',  ( -2.370970874524632510, 1427.002265528473799, 134.0999999980979851 ) ) ;
#19786 = CARTESIAN_POINT ( 'NONE',  ( -2.618314538174938644, 1456.062981335259792, 218.2460851740787575 ) ) ;
#19787 = CARTESIAN_POINT ( 'NONE',  ( -12.02581300470458459, 1433.744446891241296, 147.5729342865741955 ) ) ;
#19788 = CARTESIAN_POINT ( 'NONE',  ( -13.80542637100000114, 1434.979599513729909, 148.5642174889979970 ) ) ;
#19789 = CARTESIAN_POINT ( 'NONE',  ( -3.535195929379999491, 1507.570998153189976, 221.3286709398989842 ) ) ;
#19791 = FACE_OUTER_BOUND ( 'NONE', #63326, .T. ) ;
#19790 = CARTESIAN_POINT ( 'NONE',  ( 9.952255756299999589, 1464.084013546329970, 232.4863585809980009 ) ) ;
#19792 = CARTESIAN_POINT ( 'NONE',  ( -4.033653302454999867, 1517.028034847769959, 215.6825881955670070 ) ) ;
#19793 = CARTESIAN_POINT ( 'NONE',  ( -4.794426340529999386, 1463.608615258990085, 228.2108236244990280 ) ) ;
#19794 = CARTESIAN_POINT ( 'NONE',  ( 5.619917992193439460, 1511.009256124219974, 216.8017735542370019 ) ) ;
#19795 = CARTESIAN_POINT ( 'NONE',  ( 29.03008455810000044, 1509.878129441930014, 207.4556142791579987 ) ) ;
#19796 = CARTESIAN_POINT ( 'NONE',  ( 0.7574259850960020080, 1516.837969789639828, 212.3776558342370038 ) ) ;
#19797 = CARTESIAN_POINT ( 'NONE',  ( 4.329791512777563689, 1515.051704408389924, 213.0376480771570868 ) ) ;
#19798 = DIRECTION ( 'NONE',  ( -0.9510565162951500895, 0.000000000000000000, 0.3090169943749582759 ) ) ;
#19800 = EDGE_LOOP ( 'NONE', ( #33268, #50720, #16616, #22231 ) ) ;
#19799 = CARTESIAN_POINT ( 'NONE',  ( -80.90466521880000528, 1390.617052934750063, 295.5380644611589673 ) ) ;
#19801 = DIRECTION ( 'NONE',  ( 0.000000000000000000, 0.000000000000000000, -1.000000000000000000 ) ) ;
#19802 = CARTESIAN_POINT ( 'NONE',  ( 21.00608537309999946, 1461.014378765330093, 244.4374624723980105 ) ) ;
#19803 = CARTESIAN_POINT ( 'NONE',  ( 30.95751052620453336, 1525.821544997590308, 216.7905424461071959 ) ) ;
#19804 = CARTESIAN_POINT ( 'NONE',  ( -15.22586266600000116, 1415.677402186129939, 207.8856753661189884 ) ) ;
#19805 = CARTESIAN_POINT ( 'NONE',  ( 2.922318616430000127, 1413.151494948330082, 231.7542961375979758 ) ) ;
#19806 = CARTESIAN_POINT ( 'NONE',  ( -19.13038500899999761, 1456.668630468730044, 226.8508188085980066 ) ) ;
#19808 = CARTESIAN_POINT ( 'NONE',  ( 2.500000000000000000, 1427.007219668030075, 156.3926178584979994 ) ) ;
#19807 = CARTESIAN_POINT ( 'NONE',  ( -23.50967715347146125, 1411.094363712649283, 206.3755992539118438 ) ) ;
#19809 = CARTESIAN_POINT ( 'NONE',  ( -9.850334483518770057, 1448.894916128399927, 207.6442625542179883 ) ) ;
#19810 = CARTESIAN_POINT ( 'NONE',  ( -105.2550079177960072, 1380.603825893849944, 307.9159414798160697 ) ) ;
#19811 = EDGE_LOOP ( 'NONE', ( #58670, #36134, #91787, #94910 ) ) ;
#19812 = CARTESIAN_POINT ( 'NONE',  ( 6.549762446985000430, 1516.729202374750002, 204.5030968636170030 ) ) ;
#19813 = CARTESIAN_POINT ( 'NONE',  ( 0.8788299526799999706, 1406.512806268830218, 269.4984184344980349 ) ) ;
#19814 = CARTESIAN_POINT ( 'NONE',  ( -0.7223987349340009745, 1515.137743094390089, 213.4493844692189839 ) ) ;
#19815 = CARTESIAN_POINT ( 'NONE',  ( 19.56475689569279908, 1470.874168187639725, 270.3418681666850034 ) ) ;
#19816 = B_SPLINE_CURVE_WITH_KNOTS ( 'NONE', 3,
 ( #14644, #21915, #30343, #56111, #99741, #72920, #23032, #99187, #108709, #5147, #57234, #23593, #73475, #31443, #29799, #98648, #107608, #90243, #80765, #63987, #13525, #72381, #22466, #91365, #47713, #15177, #81843, #4608, #48830, #32000, #4073, #64534, #6245, #38198, #12983, #39857, #30891 ),
 .UNSPECIFIED., .F., .F.,
 ( 4, 3, 3, 3, 3, 3, 3, 3, 3, 3, 3, 3, 4 ),
 ( -12.49638257910000050, -12.31284761734790045, -11.59982707651139933, -10.84582623330600093, -10.05221012059380037, -9.203745996424679277, -8.197201293281651147, -7.200146307280610003, -6.413310767835159965, -5.453294015972889319, -4.614923386693979168, -3.884091819314949845, -3.197141790549999030 ),
 .UNSPECIFIED. ) ;
#19817 = CARTESIAN_POINT ( 'NONE',  ( 5.500900010980000587, 1439.900099495260065, 154.7565255832979858 ) ) ;
#19818 = CARTESIAN_POINT ( 'NONE',  ( -19.58687656140000399, 1466.791876332389847, 212.2343231219589939 ) ) ;
#19819 = CARTESIAN_POINT ( 'NONE',  ( -42.50114641298220164, 1440.913060410849994, 262.5787053766010217 ) ) ;
#19820 = CARTESIAN_POINT ( 'NONE',  ( -27.28014783120000075, 1449.116319034829985, 136.7094420238979922 ) ) ;
#19821 = CARTESIAN_POINT ( 'NONE',  ( -30.31052258194577931, 1523.604703353109699, 222.4930856806594193 ) ) ;
#19822 = CARTESIAN_POINT ( 'NONE',  ( 33.36586802512172767, 1523.382868172864164, 201.9069332299488906 ) ) ;
#19823 = CARTESIAN_POINT ( 'NONE',  ( 10.71258033046609803, 1462.053283461631736, 211.5459195315542047 ) ) ;
#19824 = CARTESIAN_POINT ( 'NONE',  ( -14.35058941781813324, 1522.051704408389924, 193.9977807835901729 ) ) ;
#19825 = CARTESIAN_POINT ( 'NONE',  ( -18.70878219499999773, 1442.609711808290058, 207.2810541335790049 ) ) ;
#19826 = AXIS2_PLACEMENT_3D ( 'NONE', #88816, #52473, #87160 ) ;
#19827 = ORIENTED_EDGE ( 'NONE', *, *, #74664, .F. ) ;
#19828 = CARTESIAN_POINT ( 'NONE',  ( -40.73184307449999864, 1440.913060387330006, 268.3665355201979992 ) ) ;
#19829 = CARTESIAN_POINT ( 'NONE',  ( 2.589445462300000056, 1486.845472968690046, 197.4512227720990154 ) ) ;
#19830 = CARTESIAN_POINT ( 'NONE',  ( 8.068722499177209073, 1467.590995982949835, 202.7938328808809842 ) ) ;
#19831 = VECTOR ( 'NONE', #9327, 1000.000000000000227 ) ;
#19832 = CARTESIAN_POINT ( 'NONE',  ( -0.3381555172680000276, 1475.759016768630090, 269.0456609237979819 ) ) ;
#19833 = CARTESIAN_POINT ( 'NONE',  ( -29.29916111349999852, 1451.889927077430229, 134.8511816846980196 ) ) ;
#19834 = CARTESIAN_POINT ( 'NONE',  ( -29.22958589629999793, 1509.933780018729749, 211.7723606568879688 ) ) ;
#19835 = CARTESIAN_POINT ( 'NONE',  ( -3.029999059705268394, 1448.271449514276583, 184.4966768164291864 ) ) ;
#19836 = CARTESIAN_POINT ( 'NONE',  ( -12.16775715655800028, 1384.884604198070065, 218.9723175489479843 ) ) ;
#19837 = B_SPLINE_CURVE_WITH_KNOTS ( 'NONE', 5,
 ( #49473, #64080, #14744, #31545, #81945, #23135, #14187, #55681, #48374 ),
 .UNSPECIFIED., .F., .F.,
 ( 6, 3, 6 ),
 ( 0.8631820001114760554, 2.053866005420000196, 3.194080077832680331 ),
 .UNSPECIFIED. ) ;
#19838 = CARTESIAN_POINT ( 'NONE',  ( -17.97556616420000353, 1415.263254644529979, 208.0573017206880024 ) ) ;
#19839 = CARTESIAN_POINT ( 'NONE',  ( -8.826539524659999358, 1481.764331591789869, 203.1249523938089965 ) ) ;
#19840 = CARTESIAN_POINT ( 'NONE',  ( 26.44714126616960215, 1435.441704364029874, 135.5654590955990102 ) ) ;
#19841 = CARTESIAN_POINT ( 'NONE',  ( -3.345866853802129892, 1396.029900632619956, 219.6261091127090310 ) ) ;
#19842 = AXIS2_PLACEMENT_3D ( 'NONE', #35258, #26862, #78371 ) ;
#19843 = CARTESIAN_POINT ( 'NONE',  ( -14.79386498719999921, 1422.246529131229863, 228.4005900637979778 ) ) ;
#19844 = CARTESIAN_POINT ( 'NONE',  ( -16.75463603240659793, 1409.872673125029905, 225.8937886272380240 ) ) ;
#19845 = CARTESIAN_POINT ( 'NONE',  ( 22.39540279318442373, 1509.695125022787124, 227.2040457527074011 ) ) ;
#19846 = ORIENTED_EDGE ( 'NONE', *, *, #89809, .F. ) ;
#19847 = CARTESIAN_POINT ( 'NONE',  ( -11.32856707963236609, 1502.802494384597594, 207.1046524659502381 ) ) ;
#19848 = CARTESIAN_POINT ( 'NONE',  ( 1.881594583719999880, 1409.481719934030025, 231.8401253045980184 ) ) ;
#19849 = CARTESIAN_POINT ( 'NONE',  ( -11.84242364297029937, 1431.324255904990196, 147.6543138676789795 ) ) ;
#19851 = CARTESIAN_POINT ( 'NONE',  ( -14.69977925956500009, 1513.518111364920060, 193.4636334463669982 ) ) ;
#19850 = CARTESIAN_POINT ( 'NONE',  ( 11.48762818220000170, 1426.845523664929942, 126.2888625367979927 ) ) ;
#19852 = LINE ( 'NONE', #56226, #5701 ) ;
#19853 = ADVANCED_FACE ( 'NONE', ( #40970 ), #93022, .F. ) ;
#19854 = B_SPLINE_CURVE_WITH_KNOTS ( 'NONE', 5,
 ( #47291, #97141, #88197, #80346, #87649, #12031, #55164, #63571, #81414, #4726, #38870, #45111 ),
 .UNSPECIFIED., .F., .F.,
 ( 6, 3, 3, 6 ),
 ( 0.000000000000000000, 0.4310012308516226187, 0.8100023263410623953, 1.000000000000000000 ),
 .UNSPECIFIED. ) ;
#19855 = CARTESIAN_POINT ( 'NONE',  ( 6.554151426245000245, 1516.906641539930206, 201.7900338461269882 ) ) ;
#19856 = CARTESIAN_POINT ( 'NONE',  ( 7.681575139199999569, 1426.029983472850063, 211.9426460963890122 ) ) ;
#19857 = FACE_OUTER_BOUND ( 'NONE', #25186, .T. ) ;
#19858 = CARTESIAN_POINT ( 'NONE',  ( 4.080976423390000107, 1507.461518311630016, 181.6612281710979744 ) ) ;
#19859 = CARTESIAN_POINT ( 'NONE',  ( 7.686100004535000529, 1512.192993275409890, 206.4318633740769826 ) ) ;
#19860 = CARTESIAN_POINT ( 'NONE',  ( -62.02946302165940295, 1379.821285026140004, 270.5012637983109585 ) ) ;
#19861 = CARTESIAN_POINT ( 'NONE',  ( 8.448716945488873975, 1365.724340617022563, 210.6218459617142003 ) ) ;
#19863 = ORIENTED_EDGE ( 'NONE', *, *, #75838, .T. ) ;
#19862 = CARTESIAN_POINT ( 'NONE',  ( 7.407831571229999135, 1453.765711829389829, 215.1756217022590079 ) ) ;
#19864 = ORIENTED_EDGE ( 'NONE', *, *, #6520, .T. ) ;
#19865 = CARTESIAN_POINT ( 'NONE',  ( -41.65810620650000828, 1443.954352776429914, 135.6863023723980177 ) ) ;
#19866 = CARTESIAN_POINT ( 'NONE',  ( 0.8514805750585270339, 1499.044650913519945, 236.8919523093149735 ) ) ;
#19867 = CARTESIAN_POINT ( 'NONE',  ( 7.326859461719999800, 1453.313060387329870, 227.7771414719979930 ) ) ;
#19868 = CARTESIAN_POINT ( 'NONE',  ( 5.229023875898142215, 1499.677744264015701, 199.0195098952981425 ) ) ;
#19870 = CARTESIAN_POINT ( 'NONE',  ( -2.773580850399999687, 1486.025199416829764, 182.0239507221979807 ) ) ;
#19869 = CARTESIAN_POINT ( 'NONE',  ( -8.835564857580001430, 1383.775455445409989, 218.4808771233589937 ) ) ;
#19871 = CARTESIAN_POINT ( 'NONE',  ( -31.65139097221453923, 1525.320849883639085, 202.0582317240186399 ) ) ;
#19872 = CARTESIAN_POINT ( 'NONE',  ( -35.15123143180689880, 1451.685553933709798, 134.6826492062959915 ) ) ;
#19873 = CARTESIAN_POINT ( 'NONE',  ( -2.500000000000000000, 1448.396495418279983, 162.2933047224009897 ) ) ;
#19874 = CARTESIAN_POINT ( 'NONE',  ( 8.910237381932139655, 1396.224212735589845, 215.6676506388549797 ) ) ;
#19875 = CARTESIAN_POINT ( 'NONE',  ( 6.242063231577089866, 1407.474368659629818, 197.0547293822570225 ) ) ;
#19876 = CARTESIAN_POINT ( 'NONE',  ( -2.304782706912239743, 1405.786085933429831, 267.5351694450670266 ) ) ;
#19877 = CARTESIAN_POINT ( 'NONE',  ( 3.829620113550000315, 1515.551704408389924, 207.0352977830190184 ) ) ;
#19878 = ORIENTED_EDGE ( 'NONE', *, *, #109794, .F. ) ;
#19879 = CARTESIAN_POINT ( 'NONE',  ( -11.30106291509999927, 1432.291791638479936, 151.5220416229979890 ) ) ;
#19880 = CARTESIAN_POINT ( 'NONE',  ( 12.56537301320000033, 1441.599614738780019, 188.5161398251980245 ) ) ;
#19881 = ORIENTED_EDGE ( 'NONE', *, *, #11225, .T. ) ;
#19882 = ORIENTED_EDGE ( 'NONE', *, *, #103731, .T. ) ;
#19883 = CARTESIAN_POINT ( 'NONE',  ( -3.423043413499999854, 1454.376749419989892, 199.6187636058789963 ) ) ;
#19884 = CARTESIAN_POINT ( 'NONE',  ( -9.657355732020000971, 1366.083296228050131, 207.6218459616989946 ) ) ;
#19885 = CARTESIAN_POINT ( 'NONE',  ( 0.7560907277860019482, 1516.770163853809890, 214.1221759657669850 ) ) ;
#19886 = CARTESIAN_POINT ( 'NONE',  ( 4.538868744795000687, 1511.336728379370243, 217.2220504028269943 ) ) ;
#19887 = MECHANICAL_DESIGN_GEOMETRIC_PRESENTATION_REPRESENTATION (  '', ( #10959 ), #82490 ) ;
#19888 = ORIENTED_EDGE ( 'NONE', *, *, #42848, .F. ) ;
#19889 = CARTESIAN_POINT ( 'NONE',  ( 7.910841848800000520, 1423.398885000399787, 212.8692358303489982 ) ) ;
#19890 = CARTESIAN_POINT ( 'NONE',  ( -85.19634273949999681, 1374.907833766890008, 296.7812697200590151 ) ) ;
#19891 = EDGE_CURVE ( 'NONE', #35843, #97183, #40654, .T. ) ;
#19892 = EDGE_CURVE ( 'NONE', #49664, #42497, #92517, .T. ) ;
#19893 = ADVANCED_FACE ( 'NONE', ( #76235 ), #103330, .T. ) ;
#19894 = CARTESIAN_POINT ( 'NONE',  ( 11.30589650210000130, 1414.913060387329779, 221.8290180415980046 ) ) ;
#19895 = CARTESIAN_POINT ( 'NONE',  ( 7.324914918154999732, 1516.685667699390024, 204.5043554653269950 ) ) ;
#19896 = CARTESIAN_POINT ( 'NONE',  ( -19.08445480129999794, 1440.913060387330006, 209.8212738029720299 ) ) ;
#19897 = EDGE_CURVE ( 'NONE', #35904, #59861, #89724, .T. ) ;
#19899 = EDGE_CURVE ( 'NONE', #63441, #7367, #57616, .T. ) ;
#19898 = CARTESIAN_POINT ( 'NONE',  ( 11.58906603030466620, 1433.009685293574421, 151.1019960182966031 ) ) ;
#19900 = FACE_OUTER_BOUND ( 'NONE', #89504, .T. ) ;
#19901 = CARTESIAN_POINT ( 'NONE',  ( -8.350981080969999581, 1410.576960734530076, 230.4971537514980184 ) ) ;
#19903 = ORIENTED_EDGE ( 'NONE', *, *, #64081, .T. ) ;
#19902 = CARTESIAN_POINT ( 'NONE',  ( -4.115442145179999400, 1447.984267398149996, 185.1172023007979988 ) ) ;
#19904 = CARTESIAN_POINT ( 'NONE',  ( 5.731937518187070424, 1432.353341358199941, 149.9895731140795760 ) ) ;
#19905 = CARTESIAN_POINT ( 'NONE',  ( -25.74005402952169774, 1440.913060490129965, 220.4485507050690103 ) ) ;
#19906 = CARTESIAN_POINT ( 'NONE',  ( -19.17386968219999943, 1384.864972699589771, 220.5237385319589976 ) ) ;
#19907 = DIRECTION ( 'NONE',  ( 0.000000000000000000, 1.000000000000000000, 0.000000000000000000 ) ) ;
#19908 = AXIS2_PLACEMENT_3D ( 'NONE', #39227, #39794, #30276 ) ;
#19909 = CARTESIAN_POINT ( 'NONE',  ( 41.30101714413999048, 1432.598592530589940, 269.8654501280279874 ) ) ;
#19910 = CARTESIAN_POINT ( 'NONE',  ( 3.267291605165000057, 1516.842852731759876, 212.5687880419470162 ) ) ;
#19911 = CARTESIAN_POINT ( 'NONE',  ( -65.90645751559999610, 1379.740571517399758, 274.2408093113589871 ) ) ;
#19912 = CARTESIAN_POINT ( 'NONE',  ( 0.01069039238330171844, 1508.209830008338031, 237.7339634020152914 ) ) ;
#19913 = CARTESIAN_POINT ( 'NONE',  ( 10.61608522903719987, 1426.022631771789975, 194.5346624901540054 ) ) ;
#19914 = CARTESIAN_POINT ( 'NONE',  ( 19.65563895711393982, 1410.960466841314201, 196.5957095808309703 ) ) ;
#19915 = CARTESIAN_POINT ( 'NONE',  ( -2.868112169295000236, 1516.855632454399938, 209.8795095036720113 ) ) ;
#19916 = VERTEX_POINT ( 'NONE', #98322 ) ;
#19917 = CARTESIAN_POINT ( 'NONE',  ( 8.991744574390811096, 1509.227061438039982, 181.2342617849590169 ) ) ;
#19919 = EDGE_CURVE ( 'NONE', #84881, #102658, #58574, .T. ) ;
#19918 = CARTESIAN_POINT ( 'NONE',  ( -0.7927729341670000096, 1417.918636335230076, 233.4281342940980153 ) ) ;
#19920 = CARTESIAN_POINT ( 'NONE',  ( -62.07136965400000150, 1384.687060561920134, 284.7656473558590164 ) ) ;
#19921 = VERTEX_POINT ( 'NONE', #106182 ) ;
#19923 = VECTOR ( 'NONE', #100499, 1000.000000000000114 ) ;
#19922 = CARTESIAN_POINT ( 'NONE',  ( -25.89380455557000005, 1385.251986020480217, 224.3320981585399920 ) ) ;
#19924 = CARTESIAN_POINT ( 'NONE',  ( 18.89959501459999913, 1416.839692131129823, 210.6687137086479993 ) ) ;
#19925 = CARTESIAN_POINT ( 'NONE',  ( 6.264020380922289633, 1478.700514275750038, 234.1616571566459868 ) ) ;
#19926 = EDGE_CURVE ( 'NONE', #89812, #68458, #7987, .T. ) ;
#19927 = AXIS2_PLACEMENT_3D ( 'NONE', #20613, #86742, #96811 ) ;
#19928 = CARTESIAN_POINT ( 'NONE',  ( -20.17493600595490122, 1508.361572245040179, 228.9114206119960215 ) ) ;
#19929 = CARTESIAN_POINT ( 'NONE',  ( -24.89939545272470056, 1440.978110083920001, 210.4300214511639808 ) ) ;
#19930 = ADVANCED_FACE ( 'NONE', ( #4811 ), #99411, .F. ) ;
#19931 = LINE ( 'NONE', #36196, #96677 ) ;
#19932 = DIRECTION ( 'NONE',  ( 0.3255681544571569219, 1.836970198721028948E-16, 0.9455185755993167351 ) ) ;
#19934 = CARTESIAN_POINT ( 'NONE',  ( 10.43360265539999965, 1481.587351803889987, 210.8844954032190060 ) ) ;
#19933 = CARTESIAN_POINT ( 'NONE',  ( -6.551643424905000401, 1516.807958722750072, 214.9033365145770063 ) ) ;
#19935 = CARTESIAN_POINT ( 'NONE',  ( 19.01903744140000185, 1509.560719669929995, 186.9589011645979895 ) ) ;
#19936 = CARTESIAN_POINT ( 'NONE',  ( 10.01009039213920104, 1469.368769691539910, 209.9822530231150211 ) ) ;
#19937 = EDGE_LOOP ( 'NONE', ( #43118, #53004, #55304, #105844 ) ) ;
#19938 = CARTESIAN_POINT ( 'NONE',  ( 4.616899834755000320, 1517.050041317280147, 201.3993091674070115 ) ) ;
#19939 = LINE ( 'NONE', #53020, #105270 ) ;
#19940 = ORIENTED_EDGE ( 'NONE', *, *, #3780, .T. ) ;
#19941 = AXIS2_PLACEMENT_3D ( 'NONE', #103258, #85360, #16488 ) ;
#19942 = CARTESIAN_POINT ( 'NONE',  ( 0.08972463244040000674, 1506.809279360230221, 231.1592509372979976 ) ) ;
#19943 =( BOUNDED_CURVE ( )  B_SPLINE_CURVE ( 3, ( #59787, #9369, #2099, #51364 ),
 .UNSPECIFIED., .F., .F. ) 
 B_SPLINE_CURVE_WITH_KNOTS ( ( 4, 4 ),
 ( 3.148814872228629991, 3.786951980637359938 ),
 .UNSPECIFIED. ) 
 CURVE ( )  GEOMETRIC_REPRESENTATION_ITEM ( )  RATIONAL_B_SPLINE_CURVE ( ( 1.000000000000000000, 0.9663520053108367591, 0.9663520053108367591, 1.000000000000000000 ) ) 
 REPRESENTATION_ITEM ( '' )  );
#19944 = CARTESIAN_POINT ( 'NONE',  ( -21.84020450222076448, 1523.382868172864164, 183.2638850454220858 ) ) ;
#19945 = LINE ( 'NONE', #63108, #107423 ) ;
#19946 = UNCERTAINTY_MEASURE_WITH_UNIT (LENGTH_MEASURE( 1.000000000000000082E-05 ), #22879, 'distance_accuracy_value', 'NONE');
#19947 = CARTESIAN_POINT ( 'NONE',  ( 1.647714509864909749, 1423.871873006899932, 191.2482835822270033 ) ) ;
#19948 = CARTESIAN_POINT ( 'NONE',  ( -29.41145171355100985, 1525.795403621571040, 196.6862065453202320 ) ) ;
#19949 = DIRECTION ( 'NONE',  ( 0.9991156149436395406, 0.000000000000000000, -0.04204744909971582650 ) ) ;
#19950 = CARTESIAN_POINT ( 'NONE',  ( 18.26532265589999682, 1415.628674266529742, 209.8910850646770143 ) ) ;
#19951 = CARTESIAN_POINT ( 'NONE',  ( -18.66276826640000053, 1424.482644047330041, 224.7741685936979934 ) ) ;
#19952 = CARTESIAN_POINT ( 'NONE',  ( -14.94677667230000040, 1435.443163586859782, 149.2760775765979986 ) ) ;
#19953 = CARTESIAN_POINT ( 'NONE',  ( -105.5745406720000119, 1391.578499750080027, 304.2150149938590289 ) ) ;
#19954 = CARTESIAN_POINT ( 'NONE',  ( 16.94262738639999810, 1413.517289013830123, 191.7422180533980054 ) ) ;
#19956 = CARTESIAN_POINT ( 'NONE',  ( -12.18907324829999972, 1509.462877414930063, 181.5959492063950051 ) ) ;
#19955 = CARTESIAN_POINT ( 'NONE',  ( 0.8067250493409530154, 1409.444751007370314, 232.8393309433039917 ) ) ;
#19957 = CARTESIAN_POINT ( 'NONE',  ( 3.115880651068799967, 1508.551704408389924, 219.3718644903320012 ) ) ;
#19958 = VERTEX_POINT ( 'NONE', #3202 ) ;
#19959 = CARTESIAN_POINT ( 'NONE',  ( 1.554318670623859866, 1415.441076448390049, 190.8942697646920124 ) ) ;
#19960 = CARTESIAN_POINT ( 'NONE',  ( 27.59579075839436868, 1509.876726636794046, 217.1913360364012817 ) ) ;
#19961 = CARTESIAN_POINT ( 'NONE',  ( -23.98687813229999932, 1436.754506703620109, 211.2894088040379756 ) ) ;
#19962 = CARTESIAN_POINT ( 'NONE',  ( -2.333997945480000169, 1485.067782868789891, 198.2455608594989940 ) ) ;
#19963 = CARTESIAN_POINT ( 'NONE',  ( 1.682117298743263101, 1526.345556099435953, 239.7639272011427636 ) ) ;
#19964 = CARTESIAN_POINT ( 'NONE',  ( -3.143084115766277886, 1525.137906803777241, 241.5427217869176104 ) ) ;
#19965 = CARTESIAN_POINT ( 'NONE',  ( 11.38620825595340946, 1434.628468754609457, 151.4994770517398308 ) ) ;
#19966 =( GEOMETRIC_REPRESENTATION_CONTEXT ( 3 ) GLOBAL_UNCERTAINTY_ASSIGNED_CONTEXT ( ( #78202 ) ) GLOBAL_UNIT_ASSIGNED_CONTEXT ( ( #35457, #58464, #85289 ) ) REPRESENTATION_CONTEXT ( 'NONE', 'WORKASPACE' ) );
#19967 = DIRECTION ( 'NONE',  ( 0.4978433412588729179, 0.000000000000000000, -0.8672669759446635096 ) ) ;
#19968 = CARTESIAN_POINT ( 'NONE',  ( -22.37852245395630035, 1509.694535611759875, 189.1625215705749952 ) ) ;
#19969 = ADVANCED_BREP_SHAPE_REPRESENTATION ( '', ( #82338, #21632 ), #61094 ) ;
#19970 = CARTESIAN_POINT ( 'NONE',  ( -11.28984392593030073, 1489.194882175770090, 213.7480122154229889 ) ) ;
#19971 = CARTESIAN_POINT ( 'NONE',  ( 16.66443376260370002, 1492.498784242470037, 193.3249348817559792 ) ) ;
#19972 = CARTESIAN_POINT ( 'NONE',  ( -84.55035757104050731, 1383.773842207470125, 306.2764245462699932 ) ) ;
#19973 = DIRECTION ( 'NONE',  ( 0.000000000000000000, 1.000000000000000000, 0.000000000000000000 ) ) ;
#19974 = CARTESIAN_POINT ( 'NONE',  ( -5.070931069364330135, 1391.839164954021044, 214.6451533971127787 ) ) ;
#19975 = CARTESIAN_POINT ( 'NONE',  ( 7.156881364479999341, 1427.109882774780090, 213.1306227488589968 ) ) ;
#19977 = ORIENTED_EDGE ( 'NONE', *, *, #50557, .T. ) ;
#19976 = CARTESIAN_POINT ( 'NONE',  ( 21.00523825079999796, 1507.839072599329711, 190.5229776796980161 ) ) ;
#19978 = CARTESIAN_POINT ( 'NONE',  ( -77.39008541779999462, 1380.628426168399983, 284.5123695392589980 ) ) ;
#19979 = CARTESIAN_POINT ( 'NONE',  ( 20.59987592950000135, 1509.677367935830262, 230.5839143914980127 ) ) ;
#19980 = ORIENTED_EDGE ( 'NONE', *, *, #107486, .T. ) ;
#19981 = ORIENTED_EDGE ( 'NONE', *, *, #53056, .T. ) ;
#19982 = CARTESIAN_POINT ( 'NONE',  ( 31.64580750758049632, 1523.313115944344872, 221.9353285378996361 ) ) ;
#19983 = CARTESIAN_POINT ( 'NONE',  ( 13.36714629989999814, 1508.095002141429859, 233.0794843863980077 ) ) ;
#19984 = CARTESIAN_POINT ( 'NONE',  ( 12.53380499174499896, 1442.773887286369927, 169.4755105688890069 ) ) ;
#19986 = CARTESIAN_POINT ( 'NONE',  ( -28.68962070750000137, 1467.163296334329971, 264.4914082303979512 ) ) ;
#19985 = CARTESIAN_POINT ( 'NONE',  ( 38.89760815976732289, 1429.358032043940739, 269.5912097956908724 ) ) ;
#19987 = CARTESIAN_POINT ( 'NONE',  ( 8.661242571614819141, 1437.508545366829821, 209.0082535151329921 ) ) ;
#19988 = CARTESIAN_POINT ( 'NONE',  ( -11.93097190810000008, 1433.475858514520041, 150.1043676198979995 ) ) ;
#19989 = ADVANCED_FACE ( 'NONE', ( #106719 ), #88831, .F. ) ;
#19990 = AXIS2_PLACEMENT_3D ( 'NONE', #13635, #98216, #80878 ) ;
#19991 = FACE_OUTER_BOUND ( 'NONE', #13561, .T. ) ;
#19992 = CARTESIAN_POINT ( 'NONE',  ( -19.08494480400000270, 1485.680871126130114, 189.6157807285979970 ) ) ;
#19993 = CARTESIAN_POINT ( 'NONE',  ( 9.483367929919999995, 1409.244226892830056, 189.9488811312979806 ) ) ;
#19994 = EDGE_CURVE ( 'NONE', #28393, #66581, #33514, .T. ) ;
#19995 = CARTESIAN_POINT ( 'NONE',  ( 5.213606989689999693, 1421.909598794630028, 185.7541303422979979 ) ) ;
#19996 = CARTESIAN_POINT ( 'NONE',  ( -6.267127244280000120, 1440.453902086580001, 154.5142011235980135 ) ) ;
#19997 = DIRECTION ( 'NONE',  ( 1.755985294532464991E-16, -1.000000000000000000, 1.338183447452830017E-16 ) ) ;
#19998 = CARTESIAN_POINT ( 'NONE',  ( -3.703129828913089838, 1440.893638029549948, 155.9280501976939775 ) ) ;
#19999 = CARTESIAN_POINT ( 'NONE',  ( -15.18192270269999966, 1451.950609855530047, 149.7661401774980163 ) ) ;
#20001 = ORIENTED_EDGE ( 'NONE', *, *, #34948, .F. ) ;
#20000 = DIRECTION ( 'NONE',  ( 0.000000000000000000, 1.000000000000000000, 0.000000000000000000 ) ) ;
#20002 = ORIENTED_EDGE ( 'NONE', *, *, #79699, .T. ) ;
#20003 = CARTESIAN_POINT ( 'NONE',  ( -13.59512409120000065, 1507.703333874389955, 209.3532891412210120 ) ) ;
#20004 = CARTESIAN_POINT ( 'NONE',  ( -21.30923694625010256, 1486.313822144630194, 201.8416180601869883 ) ) ;
#20005 = CARTESIAN_POINT ( 'NONE',  ( -15.38665937919999926, 1471.938829346429884, 270.2482212355980096 ) ) ;
#20006 = CARTESIAN_POINT ( 'NONE',  ( -7.005862043813290743E-15, 1521.551704408389924, 209.1218459616989946 ) ) ;
#20007 = CARTESIAN_POINT ( 'NONE',  ( 11.91388749740000108, 1435.945967586000052, 151.0354243678980026 ) ) ;
#20008 = CARTESIAN_POINT ( 'NONE',  ( -13.94201645220000074, 1463.289818900630053, 223.5921370626980149 ) ) ;
#20009 = AXIS2_PLACEMENT_3D ( 'NONE', #24068, #15654, #14578 ) ;
#20010 = EDGE_CURVE ( 'NONE', #8134, #14979, #55806, .T. ) ;
#20011 = CARTESIAN_POINT ( 'NONE',  ( 4.762729318109999888, 1475.513060387329915, 188.3206495969979812 ) ) ;
#20012 = DIRECTION ( 'NONE',  ( -1.000000000000000000, 0.000000000000000000, 0.000000000000000000 ) ) ;
#20013 = CARTESIAN_POINT ( 'NONE',  ( -1.274375367929762914, 1484.589685195701577, 182.3028901116345253 ) ) ;
#20014 = CARTESIAN_POINT ( 'NONE',  ( 11.27652648530197510, 1362.794758922350184, 208.3718459617010978 ) ) ;
#20015 = CARTESIAN_POINT ( 'NONE',  ( -44.13844595298070317, 1430.668308869690009, 268.2729030389940021 ) ) ;
#20016 = EDGE_LOOP ( 'NONE', ( #2192, #4578, #108481, #85573, #86270 ) ) ;
#20017 = CARTESIAN_POINT ( 'NONE',  ( -8.468559922060000744, 1424.013193781740028, 208.6259767417379862 ) ) ;
#20018 = ORIENTED_EDGE ( 'NONE', *, *, #68636, .F. ) ;
#20019 = CARTESIAN_POINT ( 'NONE',  ( 3.267039691854999983, 1517.012231669750008, 209.8574146130079896 ) ) ;
#20020 = CARTESIAN_POINT ( 'NONE',  ( -7.141639615954698428, 1508.551704408398564, 203.6084103740969624 ) ) ;
#20021 = CARTESIAN_POINT ( 'NONE',  ( -5.000000000000000000, 1391.913060387289988, 209.1218459616989946 ) ) ;
#20022 = CARTESIAN_POINT ( 'NONE',  ( -5.992819232552545117, 1414.913060387329779, 198.1520639380683235 ) ) ;
#20023 = CIRCLE ( 'NONE', #82621, 2.000000000000001776 ) ;
#20024 = CARTESIAN_POINT ( 'NONE',  ( -1.373535289882310106, 1496.574688335899964, 221.4066534229719991 ) ) ;
#20025 = ORIENTED_EDGE ( 'NONE', *, *, #26068, .T. ) ;
#20026 = CARTESIAN_POINT ( 'NONE',  ( 3.552059671762092474, 1506.620152441753362, 220.2439066918655044 ) ) ;
#20027 = EDGE_CURVE ( 'NONE', #82812, #6492, #62185, .T. ) ;
#20028 = AXIS2_PLACEMENT_3D ( 'NONE', #27731, #18754, #85979 ) ;
#20029 = CARTESIAN_POINT ( 'NONE',  ( -2.485217232065000115, 1516.534320418310244, 201.4128137944169907 ) ) ;
#20030 = CARTESIAN_POINT ( 'NONE',  ( 9.269681807320001354, 1471.390733202289994, 213.6611325259989940 ) ) ;
#20031 = CARTESIAN_POINT ( 'NONE',  ( 4.966881213900000702, 1424.596682296960125, 209.0258764887209963 ) ) ;
#20032 = ORIENTED_EDGE ( 'NONE', *, *, #1601, .T. ) ;
#20033 = CARTESIAN_POINT ( 'NONE',  ( -18.55309621579120360, 1413.291055372490064, 269.6533643345190399 ) ) ;
#20034 = CARTESIAN_POINT ( 'NONE',  ( 1.119592181715000079, 1516.958737650239982, 207.9859471464170326 ) ) ;
#20035 = CARTESIAN_POINT ( 'NONE',  ( 3.481980791854309754, 1416.697837385949924, 231.9089666833169758 ) ) ;
#20036 = DIRECTION ( 'NONE',  ( 0.000000000000000000, 0.000000000000000000, -1.000000000000000000 ) ) ;
#20038 = VERTEX_POINT ( 'NONE', #73706 ) ;
#20037 = CARTESIAN_POINT ( 'NONE',  ( -8.339847315937356953, 1365.851959156268776, 210.6218459617142003 ) ) ;
#20039 = EDGE_LOOP ( 'NONE', ( #26630, #34925, #11934, #12808, #92188, #34177, #97302, #75125, #15146, #30926, #90562, #106909 ) ) ;
#20040 = CARTESIAN_POINT ( 'NONE',  ( 45.61322772378891699, 1442.028537087034465, 268.9754013588537873 ) ) ;
#20041 = EDGE_CURVE ( 'NONE', #55773, #97968, #58777, .T. ) ;
#20042 = CARTESIAN_POINT ( 'NONE',  ( 11.36840161329240040, 1471.274902997630079, 210.2009342684919773 ) ) ;
#20043 = DIRECTION ( 'NONE',  ( -0.000000000000000000, -1.000000000000000000, -0.000000000000000000 ) ) ;
#20044 = DIRECTION ( 'NONE',  ( 0.000000000000000000, -1.000000000000000000, 0.000000000000000000 ) ) ;
#20045 = EDGE_CURVE ( 'NONE', #108404, #6840, #110434, .T. ) ;
#20046 = CARTESIAN_POINT ( 'NONE',  ( -0.5697963391879999895, 1450.893162800530263, 181.2886238165980046 ) ) ;
#20047 = CARTESIAN_POINT ( 'NONE',  ( -22.71012388409999971, 1435.763556584229946, 216.7363462006779855 ) ) ;
#20048 = B_SPLINE_CURVE_WITH_KNOTS ( 'NONE', 5,
 ( #93220, #17592, #60194, #94313, #25447, #103257, #60762, #85359, #76992, #94885, #110579, #50676 ),
 .UNSPECIFIED., .F., .F.,
 ( 6, 3, 3, 6 ),
 ( -13.24352795601230071, -6.990622299139999996, 15.67373306499999686, 31.20981123833860238 ),
 .UNSPECIFIED. ) ;
#20049 = CARTESIAN_POINT ( 'NONE',  ( -13.58268883559999907, 1416.851343902430017, 221.9096085507979979 ) ) ;
#20050 = CARTESIAN_POINT ( 'NONE',  ( 11.41983032809999976, 1415.048591094029916, 222.6307558755980267 ) ) ;
#20051 = CARTESIAN_POINT ( 'NONE',  ( 3.931911409020000026, 1448.296755876420093, 184.2998929499980250 ) ) ;
#20052 = CARTESIAN_POINT ( 'NONE',  ( 4.608146781254999880, 1516.677239312369920, 206.8257210811669893 ) ) ;
#20053 = EDGE_LOOP ( 'NONE', ( #42781, #74531, #52598, #61912 ) ) ;
#20054 = CARTESIAN_POINT ( 'NONE',  ( 1.577336110359999877, 1437.553431094789858, 227.6320445992990074 ) ) ;
#20055 = CARTESIAN_POINT ( 'NONE',  ( 1.475476450778450133, 1481.613566490490030, 182.2253701186220098 ) ) ;
#20056 = VERTEX_POINT ( 'NONE', #31119 ) ;
#20057 = CARTESIAN_POINT ( 'NONE',  ( -4.994775864357231754, 1391.713558696120572, 214.4361776424444770 ) ) ;
#20058 = CARTESIAN_POINT ( 'NONE',  ( 26.46213131619590087, 1451.086884292710010, 136.4161995186190097 ) ) ;
#20059 = CARTESIAN_POINT ( 'NONE',  ( 14.19373553490000006, 1416.535385209630022, 196.5182439381979975 ) ) ;
#20060 = CARTESIAN_POINT ( 'NONE',  ( -34.95273570850000056, 1389.711644948749836, 227.7285918695590112 ) ) ;
#20061 = CARTESIAN_POINT ( 'NONE',  ( -10.82432768028174053, 1387.838219566829594, 217.4113394113601316 ) ) ;
#20062 = CARTESIAN_POINT ( 'NONE',  ( 19.69576296570000196, 1409.600851585830014, 200.3825397104079968 ) ) ;
#20063 = CARTESIAN_POINT ( 'NONE',  ( 22.43804736130000066, 1409.696614266430061, 208.0348436616479830 ) ) ;
#20064 = CARTESIAN_POINT ( 'NONE',  ( 2.842270354763221984, 1439.666206437147821, 183.8926537781620141 ) ) ;
#20065 = CARTESIAN_POINT ( 'NONE',  ( -14.05089909369253753, 1379.587328361107211, 211.8228618032813699 ) ) ;
#20066 = EDGE_CURVE ( 'NONE', #9014, #10764, #44109, .T. ) ;
#20067 = CARTESIAN_POINT ( 'NONE',  ( 21.57000220118974454, 1453.624679045193488, 221.0567102288825367 ) ) ;
#20068 = DIRECTION ( 'NONE',  ( -0.2054769195713296304, -0.000000000000000000, 0.9786619618251631847 ) ) ;
#20069 = CARTESIAN_POINT ( 'NONE',  ( 5.782749401605000727, 1516.858301627840092, 214.8983370654769942 ) ) ;
#20070 = EDGE_CURVE ( 'NONE', #50617, #103878, #26418, .T. ) ;
#20071 = CYLINDRICAL_SURFACE ( 'NONE', #96404, 2.000000000000003109 ) ;
#20072 = ORIENTED_EDGE ( 'NONE', *, *, #40161, .T. ) ;
#20073 = LINE ( 'NONE', #97334, #79546 ) ;
#20074 = CARTESIAN_POINT ( 'NONE',  ( -7.851774706560000539, 1482.164398796690193, 201.8541463733390060 ) ) ;
#20075 = CARTESIAN_POINT ( 'NONE',  ( -8.864084639424179457, 1483.950334342079941, 201.1680632549600034 ) ) ;
#20076 = DIRECTION ( 'NONE',  ( -4.654054919228650096E-15, -0.5877852522921409584, 0.8090169943751888137 ) ) ;
#20077 = CARTESIAN_POINT ( 'NONE',  ( -39.91414502121379826, 1445.986949094549800, 136.8025261772779686 ) ) ;
#20078 = B_SPLINE_CURVE_WITH_KNOTS ( 'NONE', 5,
 ( #34721, #96856, #60501, #86782, #10637, #103013 ),
 .UNSPECIFIED., .F., .F.,
 ( 6, 6 ),
 ( 0.000000000000000000, 1.000000000000000000 ),
 .UNSPECIFIED. ) ;
#20079 = CARTESIAN_POINT ( 'NONE',  ( -4.329407853939799544, 1515.066355634550064, 207.4272903080850199 ) ) ;
#20080 = CARTESIAN_POINT ( 'NONE',  ( -19.00000000000000000, 1442.955095612160221, 209.1218459616979999 ) ) ;
#20081 = B_SPLINE_CURVE_WITH_KNOTS ( 'NONE', 3,
 ( #109076, #93897, #59776, #17162, #42402, #77129, #23928, #65985, #57578, #91704, #92255, #14977, #49172, #83304, #15525, #49721, #7153, #16076, #41309, #109615, #26698, #60895, #105077, #51923, #11571, #45748, #17721, #87741 ),
 .UNSPECIFIED., .F., .F.,
 ( 4, 3, 3, 3, 3, 3, 3, 3, 3, 4 ),
 ( 4.991132198511049722, 5.278154230586550533, 5.575591039858229792, 5.870273493069539938, 6.165162712962199976, 6.464350792949150382, 6.767514390904109334, 7.076365246789670493, 7.382407343268770461, 7.657648704760000591 ),
 .UNSPECIFIED. ) ;
#20082 = CARTESIAN_POINT ( 'NONE',  ( -14.16362979129046629, 1415.677402215299935, 203.9764129101965011 ) ) ;
#20083 = CARTESIAN_POINT ( 'NONE',  ( 11.87551015580000069, 1433.043990029219913, 149.9802084965980100 ) ) ;
#20084 = CARTESIAN_POINT ( 'NONE',  ( -2.417977538859999775, 1475.011631035330083, 269.6427107995980350 ) ) ;
#20085 = DIRECTION ( 'NONE',  ( -0.9510565162951518658, 0.000000000000000000, 0.3090169943749528914 ) ) ;
#20086 = DIRECTION ( 'NONE',  ( 0.000000000000000000, 1.000000000000000000, -6.123233995736769734E-17 ) ) ;
#20087 = DIRECTION ( 'NONE',  ( -1.000000000000000000, 1.836970198721029688E-16, 0.000000000000000000 ) ) ;
#20088 = EDGE_LOOP ( 'NONE', ( #88431, #25951, #91521, #85168 ) ) ;
#20089 = DIRECTION ( 'NONE',  ( 1.000000000000000000, 0.000000000000000000, 0.000000000000000000 ) ) ;
#20090 = CARTESIAN_POINT ( 'NONE',  ( 24.69315803756887462, 1435.858927457940808, 137.7793366136709494 ) ) ;
#20091 = B_SPLINE_CURVE_WITH_KNOTS ( 'NONE', 3,
 ( #60915, #35129, #69311, #105101 ),
 .UNSPECIFIED., .F., .F.,
 ( 4, 4 ),
 ( 0.000000000000000000, 0.0002220129587134773411 ),
 .UNSPECIFIED. ) ;
#20092 = CARTESIAN_POINT ( 'NONE',  ( -19.39983987835376666, 1501.977400791986611, 239.2921289694225777 ) ) ;
#20093 = CARTESIAN_POINT ( 'NONE',  ( -1.099350364300000216, 1443.030192123389952, 200.2900125702489902 ) ) ;
#20094 = CARTESIAN_POINT ( 'NONE',  ( 2.623998188089999850, 1507.107345730630186, 235.9745089064979879 ) ) ;
#20095 = CIRCLE ( 'NONE', #50497, 1.999999999999999556 ) ;
#20096 = CARTESIAN_POINT ( 'NONE',  ( 25.10029913760000042, 1449.799429875570013, 212.3150031425680027 ) ) ;
#20097 = CARTESIAN_POINT ( 'NONE',  ( -17.00402905897148287, 1419.970403769237919, 207.7204247156947474 ) ) ;
#20098 = CARTESIAN_POINT ( 'NONE',  ( -10.69913757989999858, 1509.229551463630060, 235.6719099616980202 ) ) ;
#20099 = CARTESIAN_POINT ( 'NONE',  ( -26.82051671160990125, 1383.845951110550004, 224.8659914338689703 ) ) ;
#20100 = CARTESIAN_POINT ( 'NONE',  ( -3.744255892484579906, 1509.032043295170070, 204.8808982972809929 ) ) ;
#20101 = CARTESIAN_POINT ( 'NONE',  ( 1.381905419950689495, 1417.049098607537871, 233.2953553763333616 ) ) ;
#20102 = CARTESIAN_POINT ( 'NONE',  ( 3.829620088064810801, 1515.551704408389696, 205.9132086401118897 ) ) ;
#20103 = CARTESIAN_POINT ( 'NONE',  ( 0.1622922531163999982, 1484.890809331159971, 181.8842724489669820 ) ) ;
#20105 = ORIENTED_EDGE ( 'NONE', *, *, #5277, .F. ) ;
#20104 = CARTESIAN_POINT ( 'NONE',  ( 1.183438229269999864, 1490.130100670090087, 188.1680879737990040 ) ) ;
#20106 = CARTESIAN_POINT ( 'NONE',  ( -0.5624689348119998877, 1416.828044896230040, 227.7677326544980190 ) ) ;
#20107 = CARTESIAN_POINT ( 'NONE',  ( -7.985077194497058883, 1385.602515846550887, 199.5277730303256192 ) ) ;
#20108 = CARTESIAN_POINT ( 'NONE',  ( -3.028500014641959837, 1440.533662533890038, 157.2362906761999852 ) ) ;
#20110 = VERTEX_POINT ( 'NONE', #63122 ) ;
#20109 = CARTESIAN_POINT ( 'NONE',  ( 1.556099495224211315, 1414.941240495253624, 191.9077315098595875 ) ) ;
#20111 = CARTESIAN_POINT ( 'NONE',  ( -6.571754112979030893, 1508.551704408419937, 219.2970873651759973 ) ) ;
#20112 = VERTEX_POINT ( 'NONE', #97223 ) ;
#20113 = B_SPLINE_CURVE_WITH_KNOTS ( 'NONE', 3,
 ( #102962, #76130, #92361, #83969, #52046, #16732, #50395, #84523, #50938, #86182, #102419, #7812, #15633, #41433, #101294, #43638, #25700, #33548, #94022, #77790, #75600, #85063, #41980, #43087, #42519, #51480, #76677, #1099 ),
 .UNSPECIFIED., .F., .F.,
 ( 4, 3, 3, 3, 3, 3, 3, 3, 3, 4 ),
 ( -1.114100599709999972, -0.9686742879261339700, -0.7108175189242720293, -0.4506292099621960201, -0.1893289210266050349, 0.07294244172766051193, 0.3351108158645359492, 0.5965830097836279933, 0.8568147313408711607, 1.114100599709999972 ),
 .UNSPECIFIED. ) ;
#20114 = CARTESIAN_POINT ( 'NONE',  ( -13.02325698038220025, 1389.786154039980147, 214.1047924551970141 ) ) ;
#20115 = CARTESIAN_POINT ( 'NONE',  ( -0.1912754843509990033, 1484.230304989690012, 201.1822192631990163 ) ) ;
#20116 = CARTESIAN_POINT ( 'NONE',  ( -3.917424962222913365, 1509.064125152231099, 238.3939863888493562 ) ) ;
#20117 = LINE ( 'NONE', #27415, #5354 ) ;
#20118 = EDGE_CURVE ( 'NONE', #62647, #19615, #18689, .T. ) ;
#20119 = CARTESIAN_POINT ( 'NONE',  ( 0.8058879247639990639, 1431.535814502990206, 218.5910766056489933 ) ) ;
#20120 = CARTESIAN_POINT ( 'NONE',  ( 20.71993696733170154, 1509.684823427714718, 187.7542232460070579 ) ) ;
#20121 = CARTESIAN_POINT ( 'NONE',  ( 14.13940509691999914, 1409.406819292400087, 213.9383516266399852 ) ) ;
#20122 = B_SPLINE_CURVE_WITH_KNOTS ( 'NONE', 5,
 ( #109482, #74784, #101050, #68050, #102159, #8649, #41715, #17023, #108924 ),
 .UNSPECIFIED., .F., .F.,
 ( 6, 3, 6 ),
 ( 0.000000000000000000, 0.5477639817078383544, 1.000000000000000000 ),
 .UNSPECIFIED. ) ;
#20123 = CARTESIAN_POINT ( 'NONE',  ( 17.80745809460000117, 1457.129128898490080, 217.9030147174489969 ) ) ;
#20124 = CARTESIAN_POINT ( 'NONE',  ( -93.46554775850030694, 1385.203179652859944, 294.3505717766860244 ) ) ;
#20125 = CARTESIAN_POINT ( 'NONE',  ( -10.21500170628049986, 1391.913060387289988, 214.1061961160360170 ) ) ;
#20126 = CARTESIAN_POINT ( 'NONE',  ( -47.55875411400000274, 1379.740588162619815, 235.3895649973590025 ) ) ;
#20127 = CARTESIAN_POINT ( 'NONE',  ( 11.08214705546439838, 1490.840403352589874, 207.9869870122680027 ) ) ;
#20128 = ORIENTED_EDGE ( 'NONE', *, *, #4509, .T. ) ;
#20129 = ORIENTED_EDGE ( 'NONE', *, *, #9071, .F. ) ;
#20130 = CARTESIAN_POINT ( 'NONE',  ( -12.26979726809049964, 1416.828039266780024, 194.6643405733680083 ) ) ;
#20131 = CARTESIAN_POINT ( 'NONE',  ( 1.222757213320049940, 1496.848853757149755, 196.7997600384149735 ) ) ;
#20132 = EDGE_CURVE ( 'NONE', #60994, #23316, #67535, .T. ) ;
#20133 = CARTESIAN_POINT ( 'NONE',  ( 10.93744292050253897, 1470.445254532535955, 269.3493099203677730 ) ) ;
#20134 = CARTESIAN_POINT ( 'NONE',  ( -31.40702543711121209, 1523.611961620354123, 221.9096305968283787 ) ) ;
#20135 = CARTESIAN_POINT ( 'NONE',  ( -0.01233344495960000085, 1396.097901039330281, 221.0480490741980191 ) ) ;
#20136 = CARTESIAN_POINT ( 'NONE',  ( 32.16538354510014130, 1524.524650307243746, 202.1429721374758230 ) ) ;
#20137 = CARTESIAN_POINT ( 'NONE',  ( -19.19787601965154167, 1486.265670089333526, 189.5055532990568850 ) ) ;
#20138 = CARTESIAN_POINT ( 'NONE',  ( -9.936738324538698208, 1364.340818343091769, 210.6218459616991936 ) ) ;
#20139 = CARTESIAN_POINT ( 'NONE',  ( 12.71038982811789886, 1507.471771741610155, 233.3404631503599944 ) ) ;
#20140 = CARTESIAN_POINT ( 'NONE',  ( 7.708770007014999592, 1516.524310051880093, 206.8307984429870032 ) ) ;
#20141 = FACE_OUTER_BOUND ( 'NONE', #22803, .T. ) ;
#20142 = CARTESIAN_POINT ( 'NONE',  ( 0.7130988073230000168, 1416.837309283630020, 190.3247695230979843 ) ) ;
#20143 = CARTESIAN_POINT ( 'NONE',  ( -66.50000000000000000, 1457.239227002485222, 134.0999999980979851 ) ) ;
#20144 = DIRECTION ( 'NONE',  ( -1.577721810442025012E-32, -1.000000000000000000, 6.123233995736769734E-17 ) ) ;
#20145 = CARTESIAN_POINT ( 'NONE',  ( -103.6765714240000023, 1379.937512265609939, 302.8207899414589974 ) ) ;
#20146 = ORIENTED_EDGE ( 'NONE', *, *, #37375, .T. ) ;
#20147 = CARTESIAN_POINT ( 'NONE',  ( 41.56052307400000245, 1440.913060319270016, 261.5689801501980014 ) ) ;
#20148 = CARTESIAN_POINT ( 'NONE',  ( -25.57225985890000075, 1469.240968291730042, 204.5212093847880226 ) ) ;
#20150 = CARTESIAN_POINT ( 'NONE',  ( 2.383381429599379737E-14, 1423.968400963209888, 229.1191372934970047 ) ) ;
#20149 = CARTESIAN_POINT ( 'NONE',  ( -2.548197114149999720, 1502.019144614829884, 181.0685241395979688 ) ) ;
#20151 = CARTESIAN_POINT ( 'NONE',  ( -22.78790659570000088, 1507.631725798030175, 208.3821237218529916 ) ) ;
#20152 = CARTESIAN_POINT ( 'NONE',  ( -34.48978217409999303, 1438.727114829129960, 250.0021841814979950 ) ) ;
#20153 = CARTESIAN_POINT ( 'NONE',  ( 3.445649996519999814, 1486.078850449689980, 219.3336985103989889 ) ) ;
#20154 = ADVANCED_FACE ( 'NONE', ( #84816 ), #14860, .F. ) ;
#20155 = DIRECTION ( 'NONE',  ( -0.8832694813677296475, 0.3761007070153973841, 0.2799701438848439250 ) ) ;
#20156 = CARTESIAN_POINT ( 'NONE',  ( 4.026786250540000722, 1418.591992575429913, 166.2922546441980103 ) ) ;
#20157 = ORIENTED_EDGE ( 'NONE', *, *, #11192, .T. ) ;
#20158 = CARTESIAN_POINT ( 'NONE',  ( -5.374434774777560264, 1429.031894749750109, 154.0908929508950109 ) ) ;
#20159 = CARTESIAN_POINT ( 'NONE',  ( 17.84338787571943996, 1523.382868172864164, 237.8836641337660467 ) ) ;
#20160 = EDGE_CURVE ( 'NONE', #87156, #89942, #60180, .T. ) ;
#20161 = CARTESIAN_POINT ( 'NONE',  ( 8.877295140909998494, 1509.263243838729977, 237.7422070772980192 ) ) ;
#20162 = ORIENTED_EDGE ( 'NONE', *, *, #29523, .F. ) ;
#20163 = ORIENTED_EDGE ( 'NONE', *, *, #75383, .T. ) ;
#20164 = CARTESIAN_POINT ( 'NONE',  ( -10.16547411475398732, 1422.464089038557177, 137.0999999980979851 ) ) ;
#20165 = CARTESIAN_POINT ( 'NONE',  ( -24.09952038931490037, 1410.987018411419967, 208.6999156859300228 ) ) ;
#20166 = EDGE_CURVE ( 'NONE', #88852, #92278, #28023, .T. ) ;
#20167 = ORIENTED_EDGE ( 'NONE', *, *, #97888, .F. ) ;
#20168 = CARTESIAN_POINT ( 'NONE',  ( -1.368191959960000093, 1419.344527984530032, 185.2221190034979941 ) ) ;
#20169 = CARTESIAN_POINT ( 'NONE',  ( 20.12564951288285897, 1511.187213306747708, 237.5287294252014192 ) ) ;
#20170 = LINE ( 'NONE', #37537, #24302 ) ;
#20171 = EDGE_CURVE ( 'NONE', #48999, #76557, #29408, .T. ) ;
#20172 = CARTESIAN_POINT ( 'NONE',  ( -2.880886796239999548, 1470.483478263630104, 235.2207609509979989 ) ) ;
#20173 = DIRECTION ( 'NONE',  ( -1.000000000000000000, 0.000000000000000000, 0.000000000000000000 ) ) ;
#20174 = ORIENTED_EDGE ( 'NONE', *, *, #40406, .T. ) ;
#20175 = CARTESIAN_POINT ( 'NONE',  ( 2.958239116441710781, 1515.068899845850183, 213.4511871929955760 ) ) ;
#20176 = CARTESIAN_POINT ( 'NONE',  ( -108.4621596517139892, 1384.899542035220065, 297.1088480531129790 ) ) ;
#20177 = ORIENTED_EDGE ( 'NONE', *, *, #27586, .F. ) ;
#20178 = CARTESIAN_POINT ( 'NONE',  ( 3.255340926295000159, 1516.962555622980062, 204.4977466407669908 ) ) ;
#20179 = VERTEX_POINT ( 'NONE', #68606 ) ;
#20180 = CARTESIAN_POINT ( 'NONE',  ( 11.85876122931039944, 1431.823958861970141, 149.9583335947500302 ) ) ;
#20181 = CARTESIAN_POINT ( 'NONE',  ( 13.26498293510852200, 1444.636724116999403, 187.4437205532745168 ) ) ;
#20182 = VERTEX_POINT ( 'NONE', #38150 ) ;
#20183 = ORIENTED_EDGE ( 'NONE', *, *, #82984, .T. ) ;
#20184 = CARTESIAN_POINT ( 'NONE',  ( -4.500000000000000000, 1425.929641636930000, 184.1455913746980002 ) ) ;
#20185 = CARTESIAN_POINT ( 'NONE',  ( -5.969756560322280414, 1508.393149768369994, 220.0371670919589917 ) ) ;
#20186 = CARTESIAN_POINT ( 'NONE',  ( -19.62228242832910396, 1409.598285588889894, 200.2165691342799789 ) ) ;
#20187 = CARTESIAN_POINT ( 'NONE',  ( -2.472525557580699918, 1469.963978788679924, 218.9232492272049910 ) ) ;
#20188 = CARTESIAN_POINT ( 'NONE',  ( 18.52343394138449995, 1452.266207820500085, 144.8864230035439959 ) ) ;
#20189 = CARTESIAN_POINT ( 'NONE',  ( 0.9478853872383249390, 1410.244833127959964, 269.6149691266229524 ) ) ;
#20190 = CARTESIAN_POINT ( 'NONE',  ( 2.487935123032369855, 1509.038615930399828, 204.6345961886270004 ) ) ;
#20191 = CARTESIAN_POINT ( 'NONE',  ( -4.958563834310000473, 1476.141796556890085, 200.0452578302089819 ) ) ;
#20192 = CARTESIAN_POINT ( 'NONE',  ( 9.432521049770000943, 1493.684480589789928, 216.5303968640490098 ) ) ;
#20193 = FACE_OUTER_BOUND ( 'NONE', #30907, .T. ) ;
#20194 = CARTESIAN_POINT ( 'NONE',  ( 9.099391957870764713, 1425.123225031011543, 195.6134721344620573 ) ) ;
#20196 = CARTESIAN_POINT ( 'NONE',  ( 15.14114459860000039, 1453.154616238230119, 195.2667548292980086 ) ) ;
#20195 = CARTESIAN_POINT ( 'NONE',  ( -19.27879749369999729, 1504.883251382790149, 209.1742019046360213 ) ) ;
#20197 = CARTESIAN_POINT ( 'NONE',  ( 12.18097209163730099, 1421.739437254449967, 207.4153353150930172 ) ) ;
#20198 = CARTESIAN_POINT ( 'NONE',  ( -9.888015356226818042, 1439.825890703900086, 207.5876242145089918 ) ) ;
#20199 = ADVANCED_FACE ( 'NONE', ( #26573 ), #104274, .T. ) ;
#20200 = CARTESIAN_POINT ( 'NONE',  ( -6.772137629935000014, 1511.702066573619959, 201.9100861211470033 ) ) ;
#20201 = ORIENTED_EDGE ( 'NONE', *, *, #76019, .T. ) ;
#20202 = CARTESIAN_POINT ( 'NONE',  ( 8.881784196999999612E-15, 1412.362567936729874, 265.6112251771979800 ) ) ;
#20203 = CARTESIAN_POINT ( 'NONE',  ( 18.63535449682491674, 1508.532394786521081, 188.3246405780103601 ) ) ;
#20204 = CARTESIAN_POINT ( 'NONE',  ( -70.52515152282619226, 1385.022333344260005, 295.6573805310360399 ) ) ;
#20205 = CARTESIAN_POINT ( 'NONE',  ( -1.784652446394692227, 1450.428767247505903, 182.6692972897738230 ) ) ;
#20206 = CARTESIAN_POINT ( 'NONE',  ( 5.268140179660000477, 1505.035622830590000, 220.7476737412989962 ) ) ;
#20207 = EDGE_CURVE ( 'NONE', #29796, #42338, #47859, .T. ) ;
#20208 = CARTESIAN_POINT ( 'NONE',  ( 30.04560769488690042, 1414.784964249760151, 269.9543914837240095 ) ) ;
#20210 = VERTEX_POINT ( 'NONE', #85649 ) ;
#20209 = CARTESIAN_POINT ( 'NONE',  ( 12.51870136171140047, 1421.160529832679913, 203.4347662715690035 ) ) ;
#20211 = CARTESIAN_POINT ( 'NONE',  ( 17.39559655639999747, 1414.988015881329829, 210.6209832631780046 ) ) ;
#20212 = CARTESIAN_POINT ( 'NONE',  ( -24.28688219629999878, 1442.594724193030061, 211.8376374323679840 ) ) ;
#20213 = CARTESIAN_POINT ( 'NONE',  ( -11.43741207009999883, 1425.481177415629872, 144.1677667564979970 ) ) ;
#20214 = CARTESIAN_POINT ( 'NONE',  ( -6.428033936520000324, 1460.873501223489939, 208.8163193724650171 ) ) ;
#20215 = CARTESIAN_POINT ( 'NONE',  ( 14.20095105293500026, 1513.466724478469814, 225.6507215884670075 ) ) ;
#20216 = CARTESIAN_POINT ( 'NONE',  ( -10.73123306599999971, 1442.518496289960012, 185.8422046897979953 ) ) ;
#20217 = CARTESIAN_POINT ( 'NONE',  ( 19.03563175159720089, 1509.617364368859853, 184.8006368254200140 ) ) ;
#20218 = CARTESIAN_POINT ( 'NONE',  ( 4.619757391858639650, 1458.438437300470241, 200.4827539045400044 ) ) ;
#20219 = DIRECTION ( 'NONE',  ( 0.05752486295818592249, -0.9969860201949396483, -0.05205540968523067469 ) ) ;
#20220 = CARTESIAN_POINT ( 'NONE',  ( 2.906835402620000064, 1412.735488669030019, 231.7379915122980094 ) ) ;
#20221 = CARTESIAN_POINT ( 'NONE',  ( -7.980724843425534232, 1424.839191111710079, 210.5241416197258957 ) ) ;
#20222 = CARTESIAN_POINT ( 'NONE',  ( -16.44430638549999912, 1460.459436675330153, 228.3413476960980120 ) ) ;
#20223 = CARTESIAN_POINT ( 'NONE',  ( -0.01319654689839849966, 1516.941178807709775, 206.8296289214069930 ) ) ;
#20224 = CARTESIAN_POINT ( 'NONE',  ( 35.66139618599999750, 1418.936225598229839, 269.0502396691979925 ) ) ;
#20225 = CARTESIAN_POINT ( 'NONE',  ( -18.29129824860000042, 1410.914753684329753, 224.2736566455979812 ) ) ;
#20226 = CARTESIAN_POINT ( 'NONE',  ( 20.01829564719999865, 1436.428735692270038, 145.4425850063980192 ) ) ;
#20227 = CARTESIAN_POINT ( 'NONE',  ( 24.99297300310000125, 1508.005497761829929, 198.0964541023980132 ) ) ;
#20228 = CARTESIAN_POINT ( 'NONE',  ( -16.87994269677939840, 1410.001063948119963, 192.1186093866529916 ) ) ;
#20229 = CARTESIAN_POINT ( 'NONE',  ( -12.57424790809989901, 1378.934406982339851, 208.2958865634099936 ) ) ;
#20230 = CARTESIAN_POINT ( 'NONE',  ( -17.21795144880000095, 1423.339050169130132, 226.8104169026979946 ) ) ;
#20231 = DIRECTION ( 'NONE',  ( 0.000000000000000000, 0.000000000000000000, -1.000000000000000000 ) ) ;
#20232 = CARTESIAN_POINT ( 'NONE',  ( 5.510910596163090542E-16, 1508.551704408389924, 204.6218459616989946 ) ) ;
#20233 = CARTESIAN_POINT ( 'NONE',  ( -7.689951449758970270, 1408.132615477319860, 198.3001377377659935 ) ) ;
#20234 = CARTESIAN_POINT ( 'NONE',  ( -15.56205866169999830, 1415.965904284230191, 208.3761328791269989 ) ) ;
#20235 = CARTESIAN_POINT ( 'NONE',  ( -17.41472613699927408, 1410.192975592430230, 193.4350317396312562 ) ) ;
#20236 = CARTESIAN_POINT ( 'NONE',  ( -7.543411004532610598, 1384.832500331219762, 219.0864943133630049 ) ) ;
#20237 = CARTESIAN_POINT ( 'NONE',  ( 2.031898713162200387, 1456.477761189839839, 219.5474395429129970 ) ) ;
#20238 = CARTESIAN_POINT ( 'NONE',  ( 18.20258715539999983, 1429.723789929190161, 209.1218459616989946 ) ) ;
#20239 = CARTESIAN_POINT ( 'NONE',  ( 22.86388141640000171, 1443.913060387330006, 134.0999999980979851 ) ) ;
#20240 = ORIENTED_EDGE ( 'NONE', *, *, #81620, .F. ) ;
#20241 = CARTESIAN_POINT ( 'NONE',  ( 5.145831880350000276, 1478.320212272790059, 199.9344042191389974 ) ) ;
#20242 = DIRECTION ( 'NONE',  ( 1.755985294532464991E-16, -1.000000000000000000, 1.338183447452830017E-16 ) ) ;
#20243 = CARTESIAN_POINT ( 'NONE',  ( -16.90742456150000095, 1444.994950788469851, 162.4348202098979925 ) ) ;
#20244 = CARTESIAN_POINT ( 'NONE',  ( 16.70350999062210917, 1433.635998124934986, 217.7474843568018628 ) ) ;
#20245 = CARTESIAN_POINT ( 'NONE',  ( -4.434413035407485992, 1421.449507706801796, 137.6342364636123534 ) ) ;
#20246 = CARTESIAN_POINT ( 'NONE',  ( -31.40725736689999792, 1466.080781296829855, 269.1484934035979677 ) ) ;
#20247 = CARTESIAN_POINT ( 'NONE',  ( -11.77443355029789984, 1481.434860139880129, 210.4630796381239861 ) ) ;
#20248 = CARTESIAN_POINT ( 'NONE',  ( 0.2538829723067779764, 1420.503732877419907, 182.7635795570130028 ) ) ;
#20249 = CARTESIAN_POINT ( 'NONE',  ( 18.66420869458052323, 1526.382868172864164, 232.7837831374276902 ) ) ;
#20250 = CARTESIAN_POINT ( 'NONE',  ( -106.4523221262569876, 1384.588530624839905, 311.2244654649010158 ) ) ;
#20251 = B_SPLINE_SURFACE_WITH_KNOTS ( 'NONE', 5, 1, ( 
 ( #48766, #82892 ),
 ( #74517, #108648 ),
 ( #100251, #15118 ),
 ( #32502, #49308 ),
 ( #83434, #66672 ),
 ( #100776, #16755 ),
 ( #43658, #8377 ),
 ( #67765, #93485 ),
 ( #33030, #101878 ) ),
 .UNSPECIFIED., .F., .F., .F.,
 ( 6, 3, 6 ),
 ( 2, 2 ),
 ( 0.000000000000000000, 3.823641809439999761, 7.629352094750000646 ),
 ( 0.000000000000000000, 14.00000000000000000 ),
 .UNSPECIFIED. ) ;
#20252 = CARTESIAN_POINT ( 'NONE',  ( -35.56235328268290630, 1384.979870847169877, 209.1200667756079952 ) ) ;
#20253 = CARTESIAN_POINT ( 'NONE',  ( -5.186175634954670599, 1375.029200368459897, 214.7946987418769993 ) ) ;
#20254 = CARTESIAN_POINT ( 'NONE',  ( 22.51756452349999904, 1509.699391067530087, 227.9212136326980271 ) ) ;
#20255 = CARTESIAN_POINT ( 'NONE',  ( -9.421550853199999409, 1433.443826258700028, 153.1575888881980063 ) ) ;
#20256 = CARTESIAN_POINT ( 'NONE',  ( -2.470168521978402421, 1523.382868172864164, 175.3649660270905599 ) ) ;
#20258 = EDGE_LOOP ( 'NONE', ( #54509, #88871 ) ) ;
#20257 = CARTESIAN_POINT ( 'NONE',  ( 4.325405444010000267, 1515.219201233190006, 207.2788824862290085 ) ) ;
#20259 = CARTESIAN_POINT ( 'NONE',  ( -5.740872018370000163, 1508.767882438629840, 180.7041383050980130 ) ) ;
#20260 = CARTESIAN_POINT ( 'NONE',  ( 20.98459803409887314, 1517.151704408390060, 216.7582258867871587 ) ) ;
#20261 = CARTESIAN_POINT ( 'NONE',  ( -3.975645313330000707, 1495.715016291389929, 219.5897528044989997 ) ) ;
#20262 = CARTESIAN_POINT ( 'NONE',  ( -11.70751967709999875, 1415.128105756529976, 195.6471422008980028 ) ) ;
#20263 = CARTESIAN_POINT ( 'NONE',  ( -0.6279686910709979530, 1422.602376000430013, 192.9011112487989976 ) ) ;
#20264 = CARTESIAN_POINT ( 'NONE',  ( 22.70034758849999790, 1409.705773992930062, 211.1194685625279988 ) ) ;
#20265 = CARTESIAN_POINT ( 'NONE',  ( -12.24435440740000125, 1434.149509971349971, 149.6614242918979869 ) ) ;
#20266 = CARTESIAN_POINT ( 'NONE',  ( 20.75865026453080020, 1455.056300995470110, 207.3304593591959986 ) ) ;
#20267 = CARTESIAN_POINT ( 'NONE',  ( -5.360263152496679950, 1422.240933723030139, 144.3253770615330041 ) ) ;
#20269 = CARTESIAN_POINT ( 'NONE',  ( -11.97041545340000113, 1377.998423774769890, 206.0180012850990181 ) ) ;
#20268 = CARTESIAN_POINT ( 'NONE',  ( -10.97839346949999850, 1432.873346371779917, 151.7696626658980108 ) ) ;
#20270 = CARTESIAN_POINT ( 'NONE',  ( 1.456985595923120158, 1417.743458194299819, 225.5366272655959676 ) ) ;
#20271 = CARTESIAN_POINT ( 'NONE',  ( -113.4000000000000057, 1378.528619065190014, 293.9108410952590020 ) ) ;
#20272 = DIRECTION ( 'NONE',  ( -1.755985294532469921E-16, 1.000000000000000000, -1.338183447452831989E-16 ) ) ;
#20273 = CARTESIAN_POINT ( 'NONE',  ( 5.151097723079999469, 1490.744826430290004, 188.9005472705989916 ) ) ;
#20274 = CARTESIAN_POINT ( 'NONE',  ( 3.984081752359151185, 1515.551704408386513, 206.7917118350702310 ) ) ;
#20275 = CARTESIAN_POINT ( 'NONE',  ( -3.458526536014999930, 1516.742629295279812, 204.1242721449069961 ) ) ;
#20276 = CARTESIAN_POINT ( 'NONE',  ( 13.37672536222529907, 1507.734881312529978, 233.0720187032129900 ) ) ;
#20277 = CARTESIAN_POINT ( 'NONE',  ( -16.81674069857199783, 1486.117794611840054, 187.5515125930209877 ) ) ;
#20278 = LINE ( 'NONE', #12438, #13674 ) ;
#20279 = CARTESIAN_POINT ( 'NONE',  ( 18.73327636269999985, 1416.067629296030191, 210.6711993623479771 ) ) ;
#20281 = ORIENTED_EDGE ( 'NONE', *, *, #4245, .F. ) ;
#20280 = CARTESIAN_POINT ( 'NONE',  ( -68.38416025601300419, 1379.747023923529923, 279.9629332694450454 ) ) ;
#20282 = EDGE_LOOP ( 'NONE', ( #29544, #20025, #97092, #11790, #66251 ) ) ;
#20283 = CARTESIAN_POINT ( 'NONE',  ( 29.75011777459999962, 1509.993906964230064, 209.6841330031659822 ) ) ;
#20284 = VERTEX_POINT ( 'NONE', #42559 ) ;
#20285 = CARTESIAN_POINT ( 'NONE',  ( 0.9514631971716608350, 1458.039373609033873, 199.6150042018308568 ) ) ;
#20286 = CARTESIAN_POINT ( 'NONE',  ( 1.547463840030000037, 1414.913060387329779, 192.3096136973980208 ) ) ;
#20288 = CARTESIAN_POINT ( 'NONE',  ( 0.4986428671280000446, 1508.154336060129936, 180.7475829099980160 ) ) ;
#20287 = CARTESIAN_POINT ( 'NONE',  ( 15.83156775414370010, 1415.884059795909934, 191.3615640054380265 ) ) ;
#20289 = CARTESIAN_POINT ( 'NONE',  ( 7.500000000000000000, 1391.913060387289988, 209.1218459616989946 ) ) ;
#20290 =( BOUNDED_SURFACE ( )  B_SPLINE_SURFACE ( 3, 2, ( 
 ( #82245, #39696, #86929 ),
 ( #31288, #52798, #99581 ),
 ( #29633, #106885, #63818 ),
 ( #21201, #38580, #73305 ),
 ( #81675, #55410, #89542 ),
 ( #90081, #81137, #72759 ),
 ( #64367, #98489, #21757 ),
 ( #55958, #13365, #4981 ),
 ( #30736, #68237, #16123 ),
 ( #58165, #22864, #109659 ) ),
 .UNSPECIFIED., .F., .F., .F. ) 
 B_SPLINE_SURFACE_WITH_KNOTS ( ( 4, 2, 2, 2, 4 ),
 ( 3, 3 ),
 ( 0.000000000000000000, 0.3926990816987241395, 0.7853981633974482790, 1.178097245096172418, 1.570796326794896558 ),
 ( 0.000000000000000000, 1.000000000000000000 ),
 .UNSPECIFIED. ) 
 GEOMETRIC_REPRESENTATION_ITEM ( )  RATIONAL_B_SPLINE_SURFACE ( (
 ( 1.000000000000000000, 0.7763623250684366095, 1.000000000000000000),
 ( 1.000000000000000000, 0.7763684247028493912, 1.000000000000000000),
 ( 1.000000000000000000, 0.7746454561806210837, 1.000000000000000000),
 ( 1.000000000000000000, 0.7679730451964270621, 1.000000000000000000),
 ( 1.000000000000000000, 0.7630177051946732680, 1.000000000000000000),
 ( 1.000000000000000000, 0.7504512394528241037, 1.000000000000000000),
 ( 1.000000000000000000, 0.7428408967931674489, 1.000000000000000000),
 ( 1.000000000000000000, 0.7259222650905756691, 1.000000000000000000),
 ( 1.000000000000000000, 0.7166207884823141416, 1.000000000000000000),
 ( 1.000000000000000000, 0.7071067811865875408, 1.000000000000000000) ) ) 
 REPRESENTATION_ITEM ( '' )  SURFACE ( )  );
#20291 = B_SPLINE_CURVE_WITH_KNOTS ( 'NONE', 3,
 ( #35974, #37067, #71263, #105384, #28672, #62878, #96989, #20253, #18042, #46044, #80176, #3492, #37620, #94764, #40361, #29222 ),
 .UNSPECIFIED., .F., .F.,
 ( 4, 2, 2, 2, 2, 2, 2, 4 ),
 ( 0.08222331860531204017, 0.08289724164938169770, 0.1008996809443339915, 0.1197691111161940103, 0.1404166416624439973, 0.1523778974832539768, 0.1644143184452410145, 0.1647592702822719968 ),
 .UNSPECIFIED. ) ;
#20292 = CARTESIAN_POINT ( 'NONE',  ( -25.28519595180179991, 1451.584664909089952, 136.7789216481089909 ) ) ;
#20293 = CARTESIAN_POINT ( 'NONE',  ( 4.500000000000000000, 1418.913060387330006, 172.2701767054979882 ) ) ;
#20294 = CARTESIAN_POINT ( 'NONE',  ( 7.055136800019999654, 1409.159431195129855, 229.7764860247980039 ) ) ;
#20296 = EDGE_CURVE ( 'NONE', #8434, #76507, #24560, .T. ) ;
#20295 = CARTESIAN_POINT ( 'NONE',  ( 9.267786286701291232, 1482.653417688600257, 214.8328156518469996 ) ) ;
#20297 = CARTESIAN_POINT ( 'NONE',  ( 3.267291605165000057, 1516.842852731759876, 212.5687880419470162 ) ) ;
#20298 = CARTESIAN_POINT ( 'NONE',  ( 41.21983904255579745, 1446.341078051059867, 134.0999999985669717 ) ) ;
#20299 = DIRECTION ( 'NONE',  ( 0.05752486295818382001, -0.9969860201949398704, 0.05205540968523099388 ) ) ;
#20300 = ORIENTED_EDGE ( 'NONE', *, *, #38384, .F. ) ;
#20301 = CARTESIAN_POINT ( 'NONE',  ( 18.94655811398780187, 1455.761323333709925, 200.3458120453390165 ) ) ;
#20302 = CARTESIAN_POINT ( 'NONE',  ( 17.71193101166619854, 1519.551704408389924, 196.6727161458730109 ) ) ;
#20303 = EDGE_LOOP ( 'NONE', ( #35400, #23184, #16005, #28543 ) ) ;
#20304 = ORIENTED_EDGE ( 'NONE', *, *, #110696, .F. ) ;
#20305 = VERTEX_POINT ( 'NONE', #9504 ) ;
#20306 = VECTOR ( 'NONE', #110786, 999.9999999999998863 ) ;
#20307 = CARTESIAN_POINT ( 'NONE',  ( -7.641097616105000156, 1512.520476835140016, 215.8818590920970166 ) ) ;
#20308 = CARTESIAN_POINT ( 'NONE',  ( 2.409034624560000282, 1511.999350511789999, 211.5308805862590020 ) ) ;
#20309 = CARTESIAN_POINT ( 'NONE',  ( 8.479372880465721352, 1451.373121564088933, 152.7985077061053119 ) ) ;
#20310 = CARTESIAN_POINT ( 'NONE',  ( -7.012921583605000286, 1508.551704408389924, 214.6352815282469919 ) ) ;
#20311 = CARTESIAN_POINT ( 'NONE',  ( -1.950867193502480168, 1465.012299926070227, 198.2909385611760342 ) ) ;
#20312 = CARTESIAN_POINT ( 'NONE',  ( -12.31997106290000055, 1378.116150593050179, 209.3647868251559885 ) ) ;
#20313 = CARTESIAN_POINT ( 'NONE',  ( -68.21293751808869388, 1379.746846629274842, 278.8708533149582536 ) ) ;
#20314 = CARTESIAN_POINT ( 'NONE',  ( 4.282754796476449854, 1446.855225404319981, 156.0904130296160019 ) ) ;
#20315 = EDGE_CURVE ( 'NONE', #60804, #61195, #76711, .T. ) ;
#20316 = CARTESIAN_POINT ( 'NONE',  ( 0.3083741877719999858, 1507.133244740429973, 237.3561682571980214 ) ) ;
#20317 = VERTEX_POINT ( 'NONE', #25735 ) ;
#20318 = CARTESIAN_POINT ( 'NONE',  ( 3.445407533985000104, 1516.764084769670262, 206.8237970085970119 ) ) ;
#20319 = ORIENTED_EDGE ( 'NONE', *, *, #16591, .F. ) ;
#20320 = CARTESIAN_POINT ( 'NONE',  ( 26.37664415071539992, 1440.913060387330006, 243.3089104971339793 ) ) ;
#20321 = CARTESIAN_POINT ( 'NONE',  ( -19.21279374710000099, 1509.245052335930040, 187.4406862720980200 ) ) ;
#20322 = ORIENTED_EDGE ( 'NONE', *, *, #3633, .T. ) ;
#20323 = CARTESIAN_POINT ( 'NONE',  ( -6.725660328943730448, 1508.728103662679814, 201.9181051944200078 ) ) ;
#20324 = EDGE_CURVE ( 'NONE', #33283, #31336, #34705, .T. ) ;
#20325 = CARTESIAN_POINT ( 'NONE',  ( -13.35894093149999939, 1409.546307774629895, 190.4983039755979917 ) ) ;
#20326 = CARTESIAN_POINT ( 'NONE',  ( -42.58097080400749235, 1379.666281498085482, 232.7225854015026698 ) ) ;
#20327 = B_SPLINE_CURVE_WITH_KNOTS ( 'NONE', 3,
 ( #60004, #42634, #94124, #67854 ),
 .UNSPECIFIED., .F., .F.,
 ( 4, 4 ),
 ( 0.6833227323573606293, 1.000000000000000000 ),
 .UNSPECIFIED. ) ;
#20329 = CARTESIAN_POINT ( 'NONE',  ( 14.76103602627950018, 1512.125809830880144, 196.8968599408240152 ) ) ;
#20328 = CARTESIAN_POINT ( 'NONE',  ( -24.40370832145195479, 1440.437192627858167, 212.0119382815727249 ) ) ;
#20330 = CARTESIAN_POINT ( 'NONE',  ( -6.245023087312289611, 1434.989591264769842, 216.5186931948820188 ) ) ;
#20331 = CARTESIAN_POINT ( 'NONE',  ( -6.161099280462069672, 1511.774605969369986, 200.4817672165819999 ) ) ;
#20332 = CARTESIAN_POINT ( 'NONE',  ( -1.676215897828090107, 1450.511945644329899, 182.4451613505460159 ) ) ;
#20333 = CARTESIAN_POINT ( 'NONE',  ( -12.06083241689999852, 1433.903765800100018, 149.9805303096979969 ) ) ;
#20334 = CARTESIAN_POINT ( 'NONE',  ( -11.39446832680910049, 1470.674085605409800, 209.5209557487560232 ) ) ;
#20336 = FACE_OUTER_BOUND ( 'NONE', #47403, .T. ) ;
#20335 = CARTESIAN_POINT ( 'NONE',  ( 6.415419946120000105, 1464.066614333030202, 235.9991510476980068 ) ) ;
#20337 = CARTESIAN_POINT ( 'NONE',  ( -7.716252091104999877, 1516.810037859429940, 216.0641906620670056 ) ) ;
#20338 = CARTESIAN_POINT ( 'NONE',  ( 1.835445324509999976, 1462.582348107689995, 228.7079535844989948 ) ) ;
#20339 = CARTESIAN_POINT ( 'NONE',  ( -2.664535259099599458E-15, 1405.913060387330006, 209.1218459616979999 ) ) ;
#20340 = CARTESIAN_POINT ( 'NONE',  ( 29.52080212560000305, 1509.954550774029940, 207.1882801656479955 ) ) ;
#20341 = CARTESIAN_POINT ( 'NONE',  ( -2.865588722415000067, 1516.890356958860139, 212.3900816908670208 ) ) ;
#20342 = FACE_OUTER_BOUND ( 'NONE', #65945, .T. ) ;
#20343 = EDGE_CURVE ( 'NONE', #28739, #31342, #38887, .T. ) ;
#20344 = CARTESIAN_POINT ( 'NONE',  ( 6.694003047440447496, 1452.460255165136687, 191.0903148363805713 ) ) ;
#20346 = ORIENTED_EDGE ( 'NONE', *, *, #63306, .T. ) ;
#20345 = CARTESIAN_POINT ( 'NONE',  ( -106.7016412910000014, 1389.434639682969873, 300.0422109230589740 ) ) ;
#20347 = CARTESIAN_POINT ( 'NONE',  ( -16.88555894881161379, 1525.556090473946824, 236.5668007256133194 ) ) ;
#20348 = CARTESIAN_POINT ( 'NONE',  ( 31.18244400220000045, 1447.044067090409953, 244.2061907871979827 ) ) ;
#20349 = CARTESIAN_POINT ( 'NONE',  ( 9.658986663755015911, 1483.195444111240022, 213.6764680106677190 ) ) ;
#20350 = CARTESIAN_POINT ( 'NONE',  ( -15.33278908930000028, 1416.031853564230005, 206.6762098088290145 ) ) ;
#20351 = CARTESIAN_POINT ( 'NONE',  ( -32.86802468386297704, 1523.382868172864164, 201.0396662540046577 ) ) ;
#20352 = CARTESIAN_POINT ( 'NONE',  ( 7.406484258469999915, 1423.002001740159812, 195.5970099228989909 ) ) ;
#20354 = CARTESIAN_POINT ( 'NONE',  ( 2.500000000000000000, 1421.615752562629950, 151.7766360386979727 ) ) ;
#20353 = CARTESIAN_POINT ( 'NONE',  ( 11.77480454480000027, 1432.721964424879843, 150.8108404446980160 ) ) ;
#20355 = CARTESIAN_POINT ( 'NONE',  ( -9.173420980859829044, 1449.906862649680079, 208.3877444760569801 ) ) ;
#20356 = CARTESIAN_POINT ( 'NONE',  ( -106.0127463409999962, 1379.506663669829777, 307.3641268108590339 ) ) ;
#20357 = EDGE_LOOP ( 'NONE', ( #35741, #13667, #69220, #73151 ) ) ;
#20358 = CARTESIAN_POINT ( 'NONE',  ( 4.610938211375000151, 1516.815231249920089, 205.0813186281270077 ) ) ;
#20359 = CARTESIAN_POINT ( 'NONE',  ( 1.333623352150000052, 1405.763012363830057, 267.5364538210980072 ) ) ;
#20360 = FACE_OUTER_BOUND ( 'NONE', #104340, .T. ) ;
#20361 = CARTESIAN_POINT ( 'NONE',  ( 31.49563175233199885, 1465.375308357740096, 270.2507308408049767 ) ) ;
#20362 = CARTESIAN_POINT ( 'NONE',  ( 2.478879819430000353, 1433.496472462500151, 157.5502782321979964 ) ) ;
#20363 = LINE ( 'NONE', #107136, #18178 ) ;
#20364 = CARTESIAN_POINT ( 'NONE',  ( -44.78652650876009744, 1440.913060399449932, 265.2360415858299802 ) ) ;
#20365 = CARTESIAN_POINT ( 'NONE',  ( -2.330134127310790060, 1515.064792882719985, 213.4512947379739956 ) ) ;
#20366 = DIRECTION ( 'NONE',  ( 1.755985294532469921E-16, -1.000000000000000000, 1.338183447452831989E-16 ) ) ;
#20367 = CARTESIAN_POINT ( 'NONE',  ( -0.4151546846821903003, 1512.187213306747481, 242.9330574173806951 ) ) ;
#20368 = CARTESIAN_POINT ( 'NONE',  ( 2.500290409796250390, 1448.931711166909963, 154.7923209379179923 ) ) ;
#20369 = CARTESIAN_POINT ( 'NONE',  ( -0.4460277715470020166, 1507.325196322990223, 221.2183930200990289 ) ) ;
#20370 = CARTESIAN_POINT ( 'NONE',  ( -4.327507230410000183, 1515.138937518789817, 209.8355912247540118 ) ) ;
#20371 = ORIENTED_EDGE ( 'NONE', *, *, #11845, .F. ) ;
#20372 = CARTESIAN_POINT ( 'NONE',  ( -28.02005516190000023, 1440.913060387330006, 248.0989693021979861 ) ) ;
#20373 = CIRCLE ( 'NONE', #14932, 1.638701816490922836 ) ;
#20374 = CARTESIAN_POINT ( 'NONE',  ( 9.862537306333429399, 1469.102982438359959, 206.4340962994679956 ) ) ;
#20375 = CARTESIAN_POINT ( 'NONE',  ( -0.1071916394719999999, 1475.561145520229957, 269.2947192205979832 ) ) ;
#20376 = CARTESIAN_POINT ( 'NONE',  ( -4.269401038497079526, 1446.687744141539952, 158.1052691740970033 ) ) ;
#20377 = CARTESIAN_POINT ( 'NONE',  ( -28.31864945599999928, 1509.156311078129875, 210.0890843349349950 ) ) ;
#20378 = CARTESIAN_POINT ( 'NONE',  ( 3.601839739459999912, 1444.840594719589944, 200.9001243581789993 ) ) ;
#20379 = CARTESIAN_POINT ( 'NONE',  ( -23.85220579467060276, 1384.849935670340074, 222.9428685578329805 ) ) ;
#20380 = B_SPLINE_CURVE_WITH_KNOTS ( 'NONE', 5,
 ( #14634, #65062, #56103, #90232, #48820, #22457, #56658, #14075, #48264 ),
 .UNSPECIFIED., .F., .F.,
 ( 6, 3, 6 ),
 ( 0.000000000000000000, 0.5000000000000000000, 1.000000000000000000 ),
 .UNSPECIFIED. ) ;
#20381 = VECTOR ( 'NONE', #91408, 1000.000000000000114 ) ;
#20382 = B_SPLINE_SURFACE_WITH_KNOTS ( 'NONE', 5, 5, ( 
 ( #84134, #94185, #34837, #41599, #49999, #76854 ),
 ( #58952, #60068, #33178, #77403, #15265, #8522 ),
 ( #109899, #51105, #84682, #83579, #7979, #43256 ),
 ( #23677, #85230, #707, #109363, #6877, #41032 ),
 ( #165, #7434, #58404, #42699, #42146, #17454 ),
 ( #102027, #93621, #25311, #16357, #75753, #16900 ),
 ( #51653, #75210, #34287, #57860, #102571, #85792 ),
 ( #76296, #32641, #110447, #100393, #9090, #66818 ),
 ( #100919, #92529, #15797, #67369, #68468, #25865 ),
 ( #101468, #24755, #93084, #50555, #11852, #80153 ),
 ( #1821, #1255, #20234, #35957, #62858, #61190 ),
 ( #95853, #105363, #11313, #88029, #46025, #3474 ),
 ( #79625, #95307, #27000, #103129, #10760, #103700 ),
 ( #28095, #2929, #35395, #87468, #44930, #2382 ),
 ( #18567, #54435, #52762, #53322, #104257, #86898 ) ),
 .UNSPECIFIED., .F., .F., .F.,
 ( 6, 3, 3, 3, 6 ),
 ( 6, 6 ),
 ( 11.25409733830000114, 13.70140831590000019, 16.14871929349999746, 18.76186865460000064, 19.95016257009999805 ),
 ( 0.000000000000000000, 2.000000000000000000 ),
 .UNSPECIFIED. ) ;
#20383 = CARTESIAN_POINT ( 'NONE',  ( -18.78419925920000111, 1416.547221146729953, 208.4031831864560047 ) ) ;
#20384 = DIRECTION ( 'NONE',  ( 0.000000000000000000, 0.000000000000000000, 1.000000000000000000 ) ) ;
#20385 = CARTESIAN_POINT ( 'NONE',  ( 26.45852657916749706, 1436.406839490560060, 136.7425343492149921 ) ) ;
#20386 = CARTESIAN_POINT ( 'NONE',  ( -11.05566370613560068, 1396.299132671179905, 209.7399892603730223 ) ) ;
#20387 = CARTESIAN_POINT ( 'NONE',  ( -3.078888291435469604, 1508.551704408389924, 204.2041707991759836 ) ) ;
#20388 = CARTESIAN_POINT ( 'NONE',  ( -16.09035704788109911, 1409.474929536219861, 225.2671591083089879 ) ) ;
#20389 = CARTESIAN_POINT ( 'NONE',  ( -13.07344736774610183, 1516.551188146160030, 225.7923144865690119 ) ) ;
#20390 = ORIENTED_EDGE ( 'NONE', *, *, #34494, .F. ) ;
#20391 = CARTESIAN_POINT ( 'NONE',  ( -21.33073281829999956, 1509.431426448229786, 190.3502236029979997 ) ) ;
#20392 = CARTESIAN_POINT ( 'NONE',  ( 2.073856897040000202, 1408.985481066030161, 230.8023040625980116 ) ) ;
#20393 = CARTESIAN_POINT ( 'NONE',  ( -11.81707100502839936, 1430.266226932280006, 147.2485954771549928 ) ) ;
#20395 = CARTESIAN_POINT ( 'NONE',  ( -14.21596113916499959, 1513.125294087170005, 193.6610111176670159 ) ) ;
#20394 = CARTESIAN_POINT ( 'NONE',  ( 11.23902904340000042, 1426.879266721829936, 108.0467253156979979 ) ) ;
#20396 = CARTESIAN_POINT ( 'NONE',  ( -4.649632279085039954, 1420.176633138330089, 186.4708453798239987 ) ) ;
#20397 = CARTESIAN_POINT ( 'NONE',  ( 4.222917386638090242, 1423.993296039239794, 184.1168122550120074 ) ) ;
#20398 = CARTESIAN_POINT ( 'NONE',  ( -109.9764103964939892, 1384.522409963689825, 311.4409506053760310 ) ) ;
#20399 = CARTESIAN_POINT ( 'NONE',  ( 7.893069735660001029, 1424.490648431219824, 211.8460496558390105 ) ) ;
#20400 = CARTESIAN_POINT ( 'NONE',  ( -13.90059962640000180, 1502.276548577589892, 227.4029734405989984 ) ) ;
#20401 = CARTESIAN_POINT ( 'NONE',  ( 5.579395061470000527, 1508.557821581529879, 181.5499561553979788 ) ) ;
#20402 = CARTESIAN_POINT ( 'NONE',  ( 7.693233015035000122, 1511.639769324940062, 206.1551559591169962 ) ) ;
#20403 = CARTESIAN_POINT ( 'NONE',  ( -66.65550921930001493, 1376.456288702509937, 281.7771486387589448 ) ) ;
#20404 = CARTESIAN_POINT ( 'NONE',  ( 7.597707828889148196, 1366.463672655298296, 210.6218459617142003 ) ) ;
#20406 = ORIENTED_EDGE ( 'NONE', *, *, #103603, .F. ) ;
#20405 = CARTESIAN_POINT ( 'NONE',  ( 15.68557540059999766, 1410.853897593529837, 191.5168599455980143 ) ) ;
#20407 = ORIENTED_EDGE ( 'NONE', *, *, #22164, .T. ) ;
#20408 = CARTESIAN_POINT ( 'NONE',  ( -12.97256852330023058, 1446.865977941818528, 187.9439244580588024 ) ) ;
#20409 = CARTESIAN_POINT ( 'NONE',  ( 0.09108844601094030768, 1499.038884509760010, 237.0407834095410067 ) ) ;
#20410 = CARTESIAN_POINT ( 'NONE',  ( -20.12564951288246107, 1511.187213306747708, 237.5287294252017603 ) ) ;
#20411 = CARTESIAN_POINT ( 'NONE',  ( -0.7790226144181949808, 1442.687261678630193, 200.2740145696140246 ) ) ;
#20413 = CARTESIAN_POINT ( 'NONE',  ( -1.364118118321220097, 1416.140226195509968, 185.3579479993269672 ) ) ;
#20412 = CARTESIAN_POINT ( 'NONE',  ( -8.489398380670001742, 1383.783001120280005, 218.5304454457089776 ) ) ;
#20414 = CARTESIAN_POINT ( 'NONE',  ( 0.8591459077770000619, 1410.309640869729947, 185.1536886007980058 ) ) ;
#20415 = CARTESIAN_POINT ( 'NONE',  ( 13.15468524849227094, 1428.736268150490105, 222.9360349510320702 ) ) ;
#20416 = CARTESIAN_POINT ( 'NONE',  ( -39.40612923876570051, 1447.975168223910032, 136.4769383534059841 ) ) ;
#20417 =( NAMED_UNIT ( * ) PLANE_ANGLE_UNIT ( ) SI_UNIT ( $, .RADIAN. ) );
#20418 = CARTESIAN_POINT ( 'NONE',  ( -2.500000000000000000, 1448.480947779509961, 160.8719867021480070 ) ) ;
#20419 = CARTESIAN_POINT ( 'NONE',  ( 3.268503196014072465, 1371.061470524529796, 208.3718459617010978 ) ) ;
#20420 = DIRECTION ( 'NONE',  ( 1.000000000000000000, 0.000000000000000000, 0.000000000000000000 ) ) ;
#20421 = CARTESIAN_POINT ( 'NONE',  ( -5.299937475575299928, 1406.728889454019964, 269.4890040361959791 ) ) ;
#20422 = DIRECTION ( 'NONE',  ( 0.4770263929453589236, -0.7067418228232984490, 0.5224574779883445208 ) ) ;
#20423 = ORIENTED_EDGE ( 'NONE', *, *, #77871, .T. ) ;
#20424 = CARTESIAN_POINT ( 'NONE',  ( -16.53175237170781386, 1526.069472839389164, 182.3016483747010739 ) ) ;
#20425 = CARTESIAN_POINT ( 'NONE',  ( 12.62483932640000006, 1441.362374013529916, 188.6153039823980180 ) ) ;
#20426 = ORIENTED_EDGE ( 'NONE', *, *, #81578, .F. ) ;
#20427 = EDGE_LOOP ( 'NONE', ( #1339, #39124, #47589, #105102 ) ) ;
#20428 = DIRECTION ( 'NONE',  ( 0.000000000000000000, 0.000000000000000000, 1.000000000000000000 ) ) ;
#20429 = CARTESIAN_POINT ( 'NONE',  ( -13.46389150100000087, 1461.194501461529853, 230.8146161405980195 ) ) ;
#20430 = CARTESIAN_POINT ( 'NONE',  ( -4.031142389804999837, 1516.929569650079884, 214.1322689334670031 ) ) ;
#20431 = CARTESIAN_POINT ( 'NONE',  ( 3.173602151875000388, 1510.830536680500245, 216.6815192743169973 ) ) ;
#20432 = ORIENTED_EDGE ( 'NONE', *, *, #102671, .T. ) ;
#20433 = CARTESIAN_POINT ( 'NONE',  ( 2.500000000000000000, 1448.416731250589919, 161.9264764492260156 ) ) ;
#20434 = CARTESIAN_POINT ( 'NONE',  ( -85.19634273949999681, 1379.292758746510117, 296.7812697164590077 ) ) ;
#20435 = EDGE_CURVE ( 'NONE', #77300, #38227, #60419, .T. ) ;
#20436 = CARTESIAN_POINT ( 'NONE',  ( 2.857576036340000236, 1416.519106787530063, 226.9547723584980190 ) ) ;
#20437 = CARTESIAN_POINT ( 'NONE',  ( -2.491188396525000126, 1516.733363207009916, 205.0947945262969938 ) ) ;
#20438 = CARTESIAN_POINT ( 'NONE',  ( -28.81649562247343255, 1526.349689584397083, 220.0454131225313574 ) ) ;
#20439 = ADVANCED_FACE ( 'NONE', ( #100790 ), #76163, .F. ) ;
#20440 = CARTESIAN_POINT ( 'NONE',  ( -103.7379217180000097, 1384.886069803950022, 296.9203887490589864 ) ) ;
#20441 = CARTESIAN_POINT ( 'NONE',  ( -4.079938673100000024, 1409.222872079729996, 231.6014056192980206 ) ) ;
#20443 = ORIENTED_EDGE ( 'NONE', *, *, #21057, .F. ) ;
#20442 = CARTESIAN_POINT ( 'NONE',  ( -30.01999557802949070, 1525.848196786131666, 197.1136699524750213 ) ) ;
#20444 = CARTESIAN_POINT ( 'NONE',  ( 32.73687869649999982, 1451.769863600429971, 134.7502305315980209 ) ) ;
#20445 = CARTESIAN_POINT ( 'NONE',  ( 10.88633642001528479, 1425.077222887074640, 139.1358730495393559 ) ) ;
#20446 = AXIS2_PLACEMENT_3D ( 'NONE', #49403, #39338, #4639 ) ;
#20447 = CARTESIAN_POINT ( 'NONE',  ( -8.743385264969999682, 1384.893486076239924, 218.5827849380889916 ) ) ;
#20448 = CARTESIAN_POINT ( 'NONE',  ( -4.227540919128129460, 1441.218328383909920, 201.3833897788859986 ) ) ;
#20449 = CARTESIAN_POINT ( 'NONE',  ( 20.61505026639999727, 1412.093511550830044, 270.3833838262979725 ) ) ;
#20450 = CARTESIAN_POINT ( 'NONE',  ( -2.865588722415000067, 1516.890356958860139, 212.3900816908670208 ) ) ;
#20451 = CARTESIAN_POINT ( 'NONE',  ( -66.97296676889999389, 1379.743459854440061, 276.3954181864590396 ) ) ;
#20452 = VECTOR ( 'NONE', #71560, 1000.000000000000000 ) ;
#20453 = CARTESIAN_POINT ( 'NONE',  ( 0.02024940985663903001, 1507.190131585810150, 237.3571517750307294 ) ) ;
#20454 = CARTESIAN_POINT ( 'NONE',  ( -30.31052258194575444, 1523.604703353109926, 222.4930856806594477 ) ) ;
#20455 = CARTESIAN_POINT ( 'NONE',  ( 20.45512642757772781, 1410.987358542064840, 198.4416328032433512 ) ) ;
#20456 = CARTESIAN_POINT ( 'NONE',  ( 0.7468175155120010400, 1517.006509894990131, 209.1147170949500094 ) ) ;
#20457 = ORIENTED_EDGE ( 'NONE', *, *, #2359, .F. ) ;
#20458 = CARTESIAN_POINT ( 'NONE',  ( 4.315674504236409526, 1420.473761226789975, 185.6540625970839926 ) ) ;
#20459 = CARTESIAN_POINT ( 'NONE',  ( -0.5925149063449999254, 1420.455671712929870, 233.5810819935980192 ) ) ;
#20460 = CARTESIAN_POINT ( 'NONE',  ( -5.513435773845334786, 1508.731359864534170, 201.6768079085695433 ) ) ;
#20461 = VERTEX_POINT ( 'NONE', #58815 ) ;
#20462 = CARTESIAN_POINT ( 'NONE',  ( -37.65727875451359807, 1385.195046747119932, 238.1789081722270112 ) ) ;
#20463 = CARTESIAN_POINT ( 'NONE',  ( -3.071329290860000061, 1430.205168262290044, 201.3670139598289950 ) ) ;
#20464 = CARTESIAN_POINT ( 'NONE',  ( -20.61688129168850026, 1509.299807670030077, 229.2235502797169886 ) ) ;
#20465 = CARTESIAN_POINT ( 'NONE',  ( -106.3976693117229928, 1390.939243848519936, 307.7527733253859878 ) ) ;
#20466 = CARTESIAN_POINT ( 'NONE',  ( 0.08524399098180000800, 1408.910083407030015, 232.2087777920980045 ) ) ;
#20467 = DIRECTION ( 'NONE',  ( -0.9125304618754024322, 0.000000000000000000, -0.4090087482554191078 ) ) ;
#20469 = CARTESIAN_POINT ( 'NONE',  ( -7.960775697985232213, 1384.702683515537956, 199.4917424227981826 ) ) ;
#20468 = CARTESIAN_POINT ( 'NONE',  ( 2.292940169014999974, 1516.565291103010168, 215.6678853655270132 ) ) ;
#20470 = CARTESIAN_POINT ( 'NONE',  ( 19.27290132190000094, 1509.486203139530062, 187.3727875556980109 ) ) ;
#20471 = DIRECTION ( 'NONE',  ( -1.000000000000000000, 0.000000000000000000, 0.000000000000000000 ) ) ;
#20472 = ORIENTED_EDGE ( 'NONE', *, *, #67354, .F. ) ;
#20473 = CARTESIAN_POINT ( 'NONE',  ( -13.01305160751540058, 1416.520646088689773, 196.6194545781839906 ) ) ;
#20474 = CIRCLE ( 'NONE', #54515, 2.000000000000001776 ) ;
#20475 = CARTESIAN_POINT ( 'NONE',  ( -15.85140264816500100, 1511.863761374039996, 220.8632120430669943 ) ) ;
#20476 = EDGE_LOOP ( 'NONE', ( #99427, #23857, #20032, #54371 ) ) ;
#20477 = CARTESIAN_POINT ( 'NONE',  ( -0.2739174590469999893, 1497.001329539429889, 230.9798146536980141 ) ) ;
#20478 = DIRECTION ( 'NONE',  ( 1.000000000000000000, 0.000000000000000000, 0.000000000000000000 ) ) ;
#20479 = DIRECTION ( 'NONE',  ( 0.000000000000000000, 1.000000000000000000, 0.000000000000000000 ) ) ;
#20480 = CIRCLE ( 'NONE', #17110, 262.4356363184970746 ) ;
#20481 = CARTESIAN_POINT ( 'NONE',  ( 0.2640960436329990446, 1443.540049495290077, 218.1738625233489870 ) ) ;
#20482 = CARTESIAN_POINT ( 'NONE',  ( 15.77707647795940638, 1421.138165674653692, 227.5460774834178608 ) ) ;
#20483 = CARTESIAN_POINT ( 'NONE',  ( 6.032762746330000425, 1424.401310572229931, 186.1143022581979949 ) ) ;
#20484 = CARTESIAN_POINT ( 'NONE',  ( -17.73405907629999589, 1423.343206274430031, 226.1884625415979997 ) ) ;
#20485 = CARTESIAN_POINT ( 'NONE',  ( -19.18996605219999907, 1435.312409617389903, 145.3494678388979935 ) ) ;
#20486 = CARTESIAN_POINT ( 'NONE',  ( 33.92643312500000263, 1450.868062273570104, 136.1711485282980050 ) ) ;
#20487 = CARTESIAN_POINT ( 'NONE',  ( 13.40786183173499779, 1517.051704408389924, 218.6219621693470003 ) ) ;
#20489 = CARTESIAN_POINT ( 'NONE',  ( -17.77930361275660331, 1434.665529742419039, 215.4045010112904492 ) ) ;
#20488 = CARTESIAN_POINT ( 'NONE',  ( 0.5924570975656898719, 1409.870418501489894, 233.1347249525960024 ) ) ;
#20490 = CARTESIAN_POINT ( 'NONE',  ( -10.14920533236069922, 1472.521211810800196, 209.9706665395110292 ) ) ;
#20491 = ORIENTED_EDGE ( 'NONE', *, *, #22127, .T. ) ;
#20492 = CARTESIAN_POINT ( 'NONE',  ( -104.4989196679999992, 1379.706513807679812, 303.6605283612590256 ) ) ;
#20493 = DIRECTION ( 'NONE',  ( -0.7074300732097413835, -0.02470400246699151064, -0.7063514732628303205 ) ) ;
#20494 = CARTESIAN_POINT ( 'NONE',  ( -45.63712966311000230, 1440.913059426480004, 268.9747523979869470 ) ) ;
#20495 = B_SPLINE_CURVE_WITH_KNOTS ( 'NONE', 5,
 ( #3699, #36173, #2040, #106131, #62512, #95520, #88783, #37827, #18791, #29404, #63607, #19343 ),
 .UNSPECIFIED., .F., .F.,
 ( 6, 3, 3, 6 ),
 ( 0.000000000000000000, 0.3100030845520760359, 0.7700076031013588507, 1.000000000000000000 ),
 .UNSPECIFIED. ) ;
#20496 = CARTESIAN_POINT ( 'NONE',  ( -11.93337329947367742, 1433.461403735681188, 149.9038200615264600 ) ) ;
#20497 = CARTESIAN_POINT ( 'NONE',  ( -3.652869222000000082, 1484.340012570490217, 198.9077488943989920 ) ) ;
#20498 = CARTESIAN_POINT ( 'NONE',  ( -16.70830179842720042, 1417.149226859160080, 207.3570905742490140 ) ) ;
#20499 = CARTESIAN_POINT ( 'NONE',  ( 0.1595995995380000143, 1486.508831850330125, 181.8147405652979671 ) ) ;
#20500 = CARTESIAN_POINT ( 'NONE',  ( 11.72456630055093996, 1435.127050470847053, 151.3186841771734237 ) ) ;
#20501 = B_SPLINE_SURFACE_WITH_KNOTS ( 'NONE', 5, 5, ( 
 ( #4732, #32528, #85667, #43138, #7321, #33601, #100808, #59954, #67796 ),
 ( #41484, #67250, #23559, #109244, #40916, #50988, #57751, #66700, #24096 ),
 ( #75645, #41, #92410, #49335, #6756, #76179, #42577, #101906, #93513 ),
 ( #25198, #34172, #100279, #58285, #15682, #49887, #84020, #8967, #24636 ),
 ( #58833, #77296, #110328, #102464, #91871, #59401, #109784, #594, #33062 ),
 ( #92970, #101345, #15145, #16785, #83461, #85117, #8405, #16242, #50447 ),
 ( #17339, #84571, #7863, #76728, #68358, #25754, #94070, #51533, #75096 ),
 ( #42030, #34722, #9518, #79503, #70569, #44806, #88447, #28537, #70022 ),
 ( #80042, #53775, #26310, #11737, #52096, #78390, #2266, #94624, #95738 ) ),
 .UNSPECIFIED., .F., .F., .F.,
 ( 6, 3, 6 ),
 ( 6, 3, 6 ),
 ( 3.281786719996299784, 5.680069915599999852, 8.078356001358638849 ),
 ( -0.0002330648786371619999, 1.500000000000000000, 3.000000000000000000 ),
 .UNSPECIFIED. ) ;
#20502 = FACE_OUTER_BOUND ( 'NONE', #51284, .T. ) ;
#20503 = CARTESIAN_POINT ( 'NONE',  ( -3.958649448056769327, 1508.551704408389924, 214.1089243834869933 ) ) ;
#20504 = CARTESIAN_POINT ( 'NONE',  ( -7.652581619519890133, 1489.002915072239830, 217.1598258052599988 ) ) ;
#20505 = CARTESIAN_POINT ( 'NONE',  ( -13.05160936328820043, 1467.538640410949938, 191.8992777555500311 ) ) ;
#20506 = CARTESIAN_POINT ( 'NONE',  ( -76.37423058801520881, 1383.779709834140021, 300.9739160671820173 ) ) ;
#20507 = ADVANCED_FACE ( 'NONE', ( #110310 ), #11329, .T. ) ;
#20508 = CARTESIAN_POINT ( 'NONE',  ( -109.0618172498179916, 1383.544782690639977, 311.0389996180940102 ) ) ;
#20509 = CARTESIAN_POINT ( 'NONE',  ( -0.6353530967299270138, 1516.751726750550233, 201.4071208092509835 ) ) ;
#20511 = EDGE_LOOP ( 'NONE', ( #76229, #82432, #44434, #110269 ) ) ;
#20510 = CARTESIAN_POINT ( 'NONE',  ( -18.70251467970079773, 1443.789633783120053, 211.1888656691189965 ) ) ;
#20512 = CARTESIAN_POINT ( 'NONE',  ( -98.86909676750001097, 1384.870948519250078, 296.2469157437590184 ) ) ;
#20513 = EDGE_CURVE ( 'NONE', #28929, #84627, #70179, .T. ) ;
#20514 = CARTESIAN_POINT ( 'NONE',  ( 12.97811970330590192, 1512.378201925209851, 224.3338094387339936 ) ) ;
#20515 = EDGE_LOOP ( 'NONE', ( #91362, #58291, #84378, #59955 ) ) ;
#20516 = EDGE_LOOP ( 'NONE', ( #50993, #44850, #11403, #41817, #40261 ) ) ;
#20517 = EDGE_CURVE ( 'NONE', #10258, #58764, #80027, .T. ) ;
#20518 = CARTESIAN_POINT ( 'NONE',  ( 24.59711297958679665, 1435.768809675110106, 207.7339403979270003 ) ) ;
#20519 = CARTESIAN_POINT ( 'NONE',  ( -32.86802468386279941, 1512.187213306747481, 217.2040256693919957 ) ) ;
#20520 = CARTESIAN_POINT ( 'NONE',  ( 12.94625993752471338, 1442.917207449076159, 169.4295987738932183 ) ) ;
#20522 = CARTESIAN_POINT ( 'NONE',  ( -33.60183515930000198, 1443.049082916849784, 248.0844435638979917 ) ) ;
#20521 = CARTESIAN_POINT ( 'NONE',  ( 34.96930673469186246, 1424.017833468233675, 269.5310884720407216 ) ) ;
#20523 = TOROIDAL_SURFACE ( 'NONE', #77700, 2.000000000000000000, 1.000000000000000000 ) ;
#20524 = CARTESIAN_POINT ( 'NONE',  ( -19.88118183330000122, 1503.697998832129997, 189.0919093254979941 ) ) ;
#20525 = CARTESIAN_POINT ( 'NONE',  ( -11.22394236169999893, 1433.945146393620007, 151.5926485512979980 ) ) ;
#20526 = CARTESIAN_POINT ( 'NONE',  ( 25.89800611569999944, 1509.146170259929931, 199.8184420921580227 ) ) ;
#20527 = CARTESIAN_POINT ( 'NONE',  ( 11.68656446679660021, 1426.729241074910078, 140.5600695502919848 ) ) ;
#20528 = CARTESIAN_POINT ( 'NONE',  ( 5.846862684000000421, 1409.284248634629876, 187.2876011129980043 ) ) ;
#20529 = CARTESIAN_POINT ( 'NONE',  ( 5.871102057859999945, 1422.424335551330159, 186.1421875806979926 ) ) ;
#20531 = CARTESIAN_POINT ( 'NONE',  ( -0.5084571940651050337, 1515.143473212400067, 213.4492344207059773 ) ) ;
#20530 = TOROIDAL_SURFACE ( 'NONE', #47332, 1.000000000000000000, 1.000000000000000000 ) ;
#20532 = CARTESIAN_POINT ( 'NONE',  ( 11.39903530061180170, 1471.112746094619979, 209.6182361319149834 ) ) ;
#20533 = CARTESIAN_POINT ( 'NONE',  ( -5.113737714138570034, 1477.155299723150165, 219.4578886346909883 ) ) ;
#20534 = AXIS2_PLACEMENT_3D ( 'NONE', #102580, #25322, #84144 ) ;
#20535 = CARTESIAN_POINT ( 'NONE',  ( -6.341639189019999456, 1451.866620239630265, 153.5781910428979984 ) ) ;
#20537 = ORIENTED_EDGE ( 'NONE', *, *, #36883, .T. ) ;
#20536 = CARTESIAN_POINT ( 'NONE',  ( 2.689344590370000176, 1464.716346886629935, 236.9361822375979898 ) ) ;
#20538 = ORIENTED_EDGE ( 'NONE', *, *, #12337, .T. ) ;
#20539 = CARTESIAN_POINT ( 'NONE',  ( -11.86317285837269964, 1432.131441266870070, 149.9785579755850051 ) ) ;
#20540 = CARTESIAN_POINT ( 'NONE',  ( -17.66645871475320106, 1487.819326808810047, 195.0539618811440050 ) ) ;
#20541 = CARTESIAN_POINT ( 'NONE',  ( -20.37632776330000084, 1469.127044835530114, 270.3601821493979855 ) ) ;
#20542 = CARTESIAN_POINT ( 'NONE',  ( -24.02424858472472380, 1435.845097858818235, 211.1058378785815535 ) ) ;
#20543 = CARTESIAN_POINT ( 'NONE',  ( 17.83435814839999978, 1410.458698069130151, 223.1757618168979889 ) ) ;
#20544 = CARTESIAN_POINT ( 'NONE',  ( -11.87563350447849864, 1433.006677213540115, 147.6591432354780125 ) ) ;
#20545 = CARTESIAN_POINT ( 'NONE',  ( 8.010413950200000244, 1453.313060387329870, 190.7496879910979715 ) ) ;
#20546 = CARTESIAN_POINT ( 'NONE',  ( -12.65888505820000098, 1420.995398902329953, 230.4350877688980006 ) ) ;
#20547 = EDGE_CURVE ( 'NONE', #33885, #64548, #68122, .T. ) ;
#20548 = FACE_OUTER_BOUND ( 'NONE', #87581, .T. ) ;
#20549 = CARTESIAN_POINT ( 'NONE',  ( 9.622136349630000751, 1363.684386430210225, 207.6218459616989946 ) ) ;
#20550 = CARTESIAN_POINT ( 'NONE',  ( -45.50346263270189695, 1435.593246726289863, 268.5130472730970155 ) ) ;
#20551 = EDGE_LOOP ( 'NONE', ( #26086, #84484, #53668, #37345, #99065 ) ) ;
#20552 = CARTESIAN_POINT ( 'NONE',  ( -3.546551875093320039, 1504.287448871370088, 181.0979340408339908 ) ) ;
#20553 = VERTEX_POINT ( 'NONE', #78374 ) ;
#20554 = CARTESIAN_POINT ( 'NONE',  ( -2.476450702264999748, 1516.843453247299749, 211.4215022863270121 ) ) ;
#20555 = APPLICATION_CONTEXT ( 'automotive_design' ) ;
#20556 = CARTESIAN_POINT ( 'NONE',  ( -10.56464281290000073, 1472.012291739390093, 204.5722061169090011 ) ) ;
#20557 = CARTESIAN_POINT ( 'NONE',  ( 17.41472478055370132, 1410.192973118622604, 224.8086574190646729 ) ) ;
#20558 = CARTESIAN_POINT ( 'NONE',  ( -14.69625711549999991, 1410.404083825129874, 190.5984733045979738 ) ) ;
#20559 = DIRECTION ( 'NONE',  ( 0.000000000000000000, -1.000000000000000000, 6.123233995736769734E-17 ) ) ;
#20560 = ORIENTED_EDGE ( 'NONE', *, *, #69826, .T. ) ;
#20561 = DIRECTION ( 'NONE',  ( -8.673617379884002932E-16, 0.02617694830786544691, -0.9996573249755575929 ) ) ;
#20562 = VECTOR ( 'NONE', #22221, 1000.000000000000000 ) ;
#20563 = CARTESIAN_POINT ( 'NONE',  ( 4.035536225084999984, 1517.086065052259983, 201.3983658527070020 ) ) ;
#20564 = EDGE_CURVE ( 'NONE', #74353, #54755, #31987, .T. ) ;
#20565 = CARTESIAN_POINT ( 'NONE',  ( 18.46438756856120023, 1509.557851009430124, 186.5303332237980101 ) ) ;
#20567 = VECTOR ( 'NONE', #107059, 1000.000000000000000 ) ;
#20566 = CARTESIAN_POINT ( 'NONE',  ( -8.739857391529799457, 1438.983306933739868, 207.6178224853659913 ) ) ;
#20568 = ORIENTED_EDGE ( 'NONE', *, *, #101731, .F. ) ;
#20569 = CARTESIAN_POINT ( 'NONE',  ( -25.88986846590829671, 1416.384201605210137, 269.9259352108049939 ) ) ;
#20570 = FACE_OUTER_BOUND ( 'NONE', #56993, .T. ) ;
#20571 = CARTESIAN_POINT ( 'NONE',  ( 0.001991242090180000025, 1395.912990851529912, 197.8078701673980220 ) ) ;
#20573 = EDGE_LOOP ( 'NONE', ( #86275, #89176, #55454, #75295 ) ) ;
#20572 = CARTESIAN_POINT ( 'NONE',  ( -9.692061980470359828, 1363.802329763660055, 210.6218459616987957 ) ) ;
#20574 = VERTEX_POINT ( 'NONE', #10623 ) ;
#20575 = CARTESIAN_POINT ( 'NONE',  ( 45.62473919765866981, 1441.709900562783332, 268.9750890229884135 ) ) ;
#20576 = CARTESIAN_POINT ( 'NONE',  ( -1.703340611422059947, 1467.868438609650184, 220.1112480085430150 ) ) ;
#20577 = CARTESIAN_POINT ( 'NONE',  ( 3.689298841057521372, 1424.196346644569076, 183.9704267610078148 ) ) ;
#20578 = CARTESIAN_POINT ( 'NONE',  ( 7.520437383334657611, 1472.270029459488796, 190.3424407131327882 ) ) ;
#20579 = LINE ( 'NONE', #106266, #101944 ) ;
#20580 = CARTESIAN_POINT ( 'NONE',  ( 5.387463376540000404, 1432.539377501929948, 154.6119119043980277 ) ) ;
#20581 = CARTESIAN_POINT ( 'NONE',  ( 10.58535985277509894, 1474.990920022710043, 269.2679215465090010 ) ) ;
#20582 = CARTESIAN_POINT ( 'NONE',  ( 12.18103061950000132, 1415.553739809529816, 223.0375094449979940 ) ) ;
#20583 = CARTESIAN_POINT ( 'NONE',  ( 4.049067852170000315, 1446.316878933369935, 182.9871537193980089 ) ) ;
#20584 =( BOUNDED_CURVE ( )  B_SPLINE_CURVE ( 3, ( #59310, #50355, #41934, #34077 ),
 .UNSPECIFIED., .F., .F. ) 
 B_SPLINE_CURVE_WITH_KNOTS ( ( 4, 4 ),
 ( 1.570796326794965614, 4.212388980384758952 ),
 .UNSPECIFIED. ) 
 CURVE ( )  GEOMETRIC_REPRESENTATION_ITEM ( )  RATIONAL_B_SPLINE_CURVE ( ( 1.000000000000000000, 0.4982693061696819581, 0.4982693061696819581, 1.000000000000000000 ) ) 
 REPRESENTATION_ITEM ( '' )  );
#20585 = CARTESIAN_POINT ( 'NONE',  ( -0.7578858299649979813, 1516.872851364150165, 206.6414186775969881 ) ) ;
#20586 = ORIENTED_EDGE ( 'NONE', *, *, #58975, .T. ) ;
#20587 = DIRECTION ( 'NONE',  ( -5.164946217006259634E-18, 0.000000000000000000, -1.000000000000000000 ) ) ;
#20588 = CARTESIAN_POINT ( 'NONE',  ( -23.83238225862761794, 1446.589712416024213, 213.8438450975477281 ) ) ;
#20589 = ORIENTED_EDGE ( 'NONE', *, *, #90309, .T. ) ;
#20590 = CARTESIAN_POINT ( 'NONE',  ( 10.56643885385577875, 1455.157788284585422, 226.2919240970107353 ) ) ;
#20591 = CARTESIAN_POINT ( 'NONE',  ( 23.99734131323389974, 1452.069796923729882, 137.0529556418699997 ) ) ;
#20592 = CARTESIAN_POINT ( 'NONE',  ( 20.20959865099471031, 1501.977400791986611, 182.0120230947219966 ) ) ;
#20593 = CARTESIAN_POINT ( 'NONE',  ( -2.923521517025829741, 1410.394928878200062, 186.6127595807840009 ) ) ;
#20594 = CARTESIAN_POINT ( 'NONE',  ( -5.389719915088219793, 1440.971386074470047, 154.8246291213590098 ) ) ;
#20595 = CARTESIAN_POINT ( 'NONE',  ( -8.320994297830779374, 1422.937291762959831, 213.3671062650610111 ) ) ;
#20596 = CARTESIAN_POINT ( 'NONE',  ( -3.827327205999999649, 1416.243718512830128, 162.3415388335980083 ) ) ;
#20597 = CARTESIAN_POINT ( 'NONE',  ( 9.674066812699999574, 1488.345346575790018, 203.9346639274390043 ) ) ;
#20598 = FACE_OUTER_BOUND ( 'NONE', #6511, .T. ) ;
#20599 = ADVANCED_FACE ( 'NONE', ( #54843 ), #70344, .T. ) ;
#20600 = CARTESIAN_POINT ( 'NONE',  ( 2.500000000000000000, 1439.615921250379870, 167.6891701647670061 ) ) ;
#20601 = EDGE_CURVE ( 'NONE', #75158, #88376, #11971, .T. ) ;
#20602 = CARTESIAN_POINT ( 'NONE',  ( 0.7553264358530019651, 1516.745833913490060, 214.8974710475970085 ) ) ;
#20603 = DIRECTION ( 'NONE',  ( -0.8200914087126203178, -0.4884709562387607451, 0.2980708074718837475 ) ) ;
#20604 = ORIENTED_EDGE ( 'NONE', *, *, #21307, .F. ) ;
#20605 = LINE ( 'NONE', #19518, #67010 ) ;
#20606 = CARTESIAN_POINT ( 'NONE',  ( 0.08276195847810161044, 1408.915950497909762, 187.0495686484979956 ) ) ;
#20607 = CARTESIAN_POINT ( 'NONE',  ( -13.15726448721240160, 1416.851343896870048, 221.9096085506390068 ) ) ;
#20608 = FACE_OUTER_BOUND ( 'NONE', #83788, .T. ) ;
#20609 = AXIS2_PLACEMENT_3D ( 'NONE', #48639, #13889, #100119 ) ;
#20610 = CARTESIAN_POINT ( 'NONE',  ( -40.20457429252190451, 1444.781942773269975, 137.0004547941439910 ) ) ;
#20611 = CARTESIAN_POINT ( 'NONE',  ( 19.09907639360000076, 1458.161943520289924, 212.8891023046390103 ) ) ;
#20612 = CARTESIAN_POINT ( 'NONE',  ( -0.4151546846821903003, 1522.382868172863937, 173.3106345060153046 ) ) ;
#20613 = CARTESIAN_POINT ( 'NONE',  ( 19.63722818192610120, 1519.551704408389924, 218.2362632616380154 ) ) ;
#20614 = CARTESIAN_POINT ( 'NONE',  ( 11.07166356589999978, 1433.243716658159883, 151.7035676110980091 ) ) ;
#20615 = FACE_OUTER_BOUND ( 'NONE', #89195, .T. ) ;
#20616 = B_SPLINE_SURFACE_WITH_KNOTS ( 'NONE', 5, 5, ( 
 ( #105648, #79336, #46309, #11576, #63123, #2094 ),
 ( #45195, #80438, #70408, #70967, #60900, #52488 ),
 ( #45753, #105083, #86616, #27824, #3753, #37885 ),
 ( #72069, #28371, #35663, #19961, #54156, #18295 ),
 ( #44080, #78219, #28933, #1529, #62004, #103970 ),
 ( #10465, #19398, #53602, #87746, #3204, #82068 ) ),
 .UNSPECIFIED., .F., .F., .F.,
 ( 6, 6 ),
 ( 6, 6 ),
 ( 40.35130054919999765, 45.55451570600000366 ),
 ( 0.000000000000000000, 2.000000000060000005 ),
 .UNSPECIFIED. ) ;
#20617 = CARTESIAN_POINT ( 'NONE',  ( -9.519205059868689034, 1460.476570792010079, 210.7622160576040073 ) ) ;
#20618 = CARTESIAN_POINT ( 'NONE',  ( -109.8982923870000121, 1385.096845541700077, 297.0319097604589729 ) ) ;
#20619 = CYLINDRICAL_SURFACE ( 'NONE', #22383, 10.00000000000000000 ) ;
#20620 = VERTEX_POINT ( 'NONE', #84965 ) ;
#20621 = DIRECTION ( 'NONE',  ( -1.000000000000000000, 0.000000000000000000, 0.000000000000000000 ) ) ;
#20622 = CARTESIAN_POINT ( 'NONE',  ( 16.66231036550724198, 1523.604703353109699, 237.7554842931445478 ) ) ;
#20623 = DIRECTION ( 'NONE',  ( 0.000000000000000000, 1.000000000000000000, 0.000000000000000000 ) ) ;
#20624 = CARTESIAN_POINT ( 'NONE',  ( -2.165176160182525233, 1526.186458717538699, 240.2894009330203744 ) ) ;
#20625 = CARTESIAN_POINT ( 'NONE',  ( 2.362637160190000252, 1507.103770644730048, 236.0496999084980132 ) ) ;
#20626 = EDGE_CURVE ( 'NONE', #15891, #3640, #94868, .T. ) ;
#20627 = CARTESIAN_POINT ( 'NONE',  ( -0.6774325393469999845, 1465.095555782530027, 238.0673157071979915 ) ) ;
#20628 = CARTESIAN_POINT ( 'NONE',  ( -13.71017305750000048, 1507.516664216029994, 232.5217224164979939 ) ) ;
#20629 = CARTESIAN_POINT ( 'NONE',  ( -20.76923605841339793, 1383.852768131139783, 221.0916664262549887 ) ) ;
#20631 = EDGE_CURVE ( 'NONE', #103706, #68962, #48063, .T. ) ;
#20630 = CIRCLE ( 'NONE', #29599, 2.000034594847158065 ) ;
#20632 = CARTESIAN_POINT ( 'NONE',  ( 20.97834595694860127, 1506.096755889989936, 226.0120427145139956 ) ) ;
#20633 = FACE_OUTER_BOUND ( 'NONE', #50596, .T. ) ;
#20634 = CARTESIAN_POINT ( 'NONE',  ( 3.208637255279672473, 1515.551704408389696, 205.2922258088532317 ) ) ;
#20635 = CARTESIAN_POINT ( 'NONE',  ( 2.811694866999999931, 1464.674002741930053, 236.8041412282979934 ) ) ;
#20636 = EDGE_CURVE ( 'NONE', #67105, #4207, #4061, .T. ) ;
#20638 = EDGE_LOOP ( 'NONE', ( #98822, #30640, #40640, #76929, #54409, #57394, #7481, #79123, #57738, #48593 ) ) ;
#20637 = DIRECTION ( 'NONE',  ( 0.000000000000000000, 0.000000000000000000, 1.000000000000000000 ) ) ;
#20639 = CARTESIAN_POINT ( 'NONE',  ( -1.378953279320000114, 1450.758537438610119, 182.6902919710979916 ) ) ;
#20640 = CARTESIAN_POINT ( 'NONE',  ( -8.125464938096873979, 1386.278383885165113, 199.6698962121421914 ) ) ;
#20641 = CARTESIAN_POINT ( 'NONE',  ( -4.958565512799999908, 1476.141795141989860, 200.0452582524689831 ) ) ;
#20643 = ORIENTED_EDGE ( 'NONE', *, *, #89094, .T. ) ;
#20642 = CYLINDRICAL_SURFACE ( 'NONE', #28639, 2.000000000000011102 ) ;
#20644 = CARTESIAN_POINT ( 'NONE',  ( -19.04698019608209947, 1444.155722059970003, 199.5979690564769840 ) ) ;
#20645 = ORIENTED_EDGE ( 'NONE', *, *, #40285, .F. ) ;
#20646 = AXIS2_PLACEMENT_3D ( 'NONE', #53122, #20043, #77758 ) ;
#20647 = CARTESIAN_POINT ( 'NONE',  ( -9.882261837502390733, 1388.398873433800190, 217.1410497004710010 ) ) ;
#20648 = CARTESIAN_POINT ( 'NONE',  ( 12.27023112330000032, 1416.839692136459917, 223.5796784318309847 ) ) ;
#20649 = CARTESIAN_POINT ( 'NONE',  ( 11.87973986201449961, 1433.324300360609868, 147.6568050212700030 ) ) ;
#20651 = EDGE_CURVE ( 'NONE', #91418, #24977, #77411, .T. ) ;
#20650 = CARTESIAN_POINT ( 'NONE',  ( -5.523724626499999957, 1462.904961658189904, 201.0501093365290046 ) ) ;
#20652 = CARTESIAN_POINT ( 'NONE',  ( -2.944617142229999818, 1431.901135818789953, 217.0105143139790016 ) ) ;
#20653 = FACE_OUTER_BOUND ( 'NONE', #106697, .T. ) ;
#20654 = CARTESIAN_POINT ( 'NONE',  ( 14.93347384300719938, 1409.434548785099878, 209.2195559055120100 ) ) ;
#20655 = CARTESIAN_POINT ( 'NONE',  ( 18.02454965899999806, 1424.443906294430008, 224.7645392682979946 ) ) ;
#20656 = CARTESIAN_POINT ( 'NONE',  ( -107.2083758124640127, 1385.238133497090075, 297.0681113654679848 ) ) ;
#20657 = CARTESIAN_POINT ( 'NONE',  ( -18.43186383950000007, 1440.792975980310075, 191.7737155625979995 ) ) ;
#20658 = CARTESIAN_POINT ( 'NONE',  ( 10.96917002130000007, 1432.328099426499875, 151.7701195723979879 ) ) ;
#20659 = EDGE_CURVE ( 'NONE', #18765, #75001, #37159, .T. ) ;
#20660 = CARTESIAN_POINT ( 'NONE',  ( 10.92860598996890076, 1490.384399647580040, 208.1271090416140055 ) ) ;
#20661 = ORIENTED_EDGE ( 'NONE', *, *, #19347, .T. ) ;
#20662 = ORIENTED_EDGE ( 'NONE', *, *, #4271, .F. ) ;
#20664 = EDGE_CURVE ( 'NONE', #13899, #90367, #20091, .T. ) ;
#20663 = CARTESIAN_POINT ( 'NONE',  ( -7.166260544089549711, 1508.551565390810083, 215.1547104977369997 ) ) ;
#20665 = CARTESIAN_POINT ( 'NONE',  ( -12.10884181134970028, 1416.007771869970156, 194.8210225066299870 ) ) ;
#20666 = CARTESIAN_POINT ( 'NONE',  ( 1.559621619610169985, 1496.922908498869901, 196.8322261072790127 ) ) ;
#20667 = CARTESIAN_POINT ( 'NONE',  ( 20.74483292822688441, 1467.449581717848332, 269.3942764596831125 ) ) ;
#20668 = CYLINDRICAL_SURFACE ( 'NONE', #14119, 1.000000000000076383 ) ;
#20669 = CARTESIAN_POINT ( 'NONE',  ( 0.1955981723673640149, 1414.913060387329779, 225.1861338915940109 ) ) ;
#20670 = CARTESIAN_POINT ( 'NONE',  ( 20.76266746499769766, 1464.825020750889962, 209.7053101748109896 ) ) ;
#20671 = EDGE_CURVE ( 'NONE', #21086, #32612, #3203, .T. ) ;
#20672 = CARTESIAN_POINT ( 'NONE',  ( -1.455133652010000000, 1471.168344426330123, 183.0463840045979964 ) ) ;
#20673 = CARTESIAN_POINT ( 'NONE',  ( -11.09819096161026408, 1364.005208992933603, 210.6218459617030021 ) ) ;
#20674 = CARTESIAN_POINT ( 'NONE',  ( -26.57701928479934850, 1436.737487800338386, 136.7979441010809296 ) ) ;
#20675 = CARTESIAN_POINT ( 'NONE',  ( 2.688588257229999723, 1509.006947958130013, 238.2844991894980069 ) ) ;
#20676 = EDGE_CURVE ( 'NONE', #2790, #97980, #62778, .T. ) ;
#20677 = CARTESIAN_POINT ( 'NONE',  ( 6.933587655514999781, 1516.542957540330008, 207.4124872689769745 ) ) ;
#20678 = CARTESIAN_POINT ( 'NONE',  ( 31.32995031131198616, 1523.678648413191695, 221.9013357025044115 ) ) ;
#20679 = CARTESIAN_POINT ( 'NONE',  ( -8.860265397230000062, 1385.060179297459854, 218.6816725719889973 ) ) ;
#20680 = CARTESIAN_POINT ( 'NONE',  ( 16.65035232609999838, 1409.494503502829957, 193.9825473880979985 ) ) ;
#20681 = CARTESIAN_POINT ( 'NONE',  ( -15.72751745975079984, 1517.051704408389924, 211.3620530696679793 ) ) ;
#20682 = DIRECTION ( 'NONE',  ( 0.7074300732946419146, 0.02470400257053509060, -0.7063514731741787900 ) ) ;
#20683 = EDGE_CURVE ( 'NONE', #58053, #18655, #18860, .T. ) ;
#20684 = CARTESIAN_POINT ( 'NONE',  ( 33.13357216314881981, 1523.313115944345327, 200.8872321731301156 ) ) ;
#20685 = AXIS2_PLACEMENT_3D ( 'NONE', #10854, #19211, #2479 ) ;
#20686 = EDGE_LOOP ( 'NONE', ( #105973, #78555, #91656, #4436 ) ) ;
#20687 = CARTESIAN_POINT ( 'NONE',  ( 27.17992431440000090, 1424.801532951130184, 248.2870168903980073 ) ) ;
#20688 = CARTESIAN_POINT ( 'NONE',  ( -26.35247771899999947, 1469.246089667830120, 207.6027827722479913 ) ) ;
#20691 = LINE ( 'NONE', #11763, #75450 ) ;
#20690 = AXIS2_PLACEMENT_3D ( 'NONE', #73884, #89564, #30199 ) ;
#20689 = CARTESIAN_POINT ( 'NONE',  ( -11.09501388980000058, 1426.902722246829853, 97.52861334269789495 ) ) ;
#20692 = CARTESIAN_POINT ( 'NONE',  ( -3.665756888920000289, 1509.051704408389924, 214.1089243971590008 ) ) ;
#20693 = CARTESIAN_POINT ( 'NONE',  ( -29.81189463440000154, 1423.440805878429956, 254.8364553539980193 ) ) ;
#20694 = CARTESIAN_POINT ( 'NONE',  ( 19.82628316702480120, 1509.637547285240089, 231.2121791950689840 ) ) ;
#20695 = CARTESIAN_POINT ( 'NONE',  ( -5.199570078000000706, 1391.913060387289988, 214.4361776263990009 ) ) ;
#20696 = CARTESIAN_POINT ( 'NONE',  ( 31.79025968199999852, 1451.649844149130104, 135.6495218311980011 ) ) ;
#20697 = VERTEX_POINT ( 'NONE', #88300 ) ;
#20698 = CARTESIAN_POINT ( 'NONE',  ( 3.774231707645040235, 1397.713543333530197, 196.1008760955799914 ) ) ;
#20699 = CARTESIAN_POINT ( 'NONE',  ( 12.05347594647225939, 1513.055456493726751, 225.7288246710316173 ) ) ;
#20700 = CARTESIAN_POINT ( 'NONE',  ( 38.60856580501570079, 1443.613625263020140, 137.1750438873210101 ) ) ;
#20701 = ORIENTED_EDGE ( 'NONE', *, *, #6881, .F. ) ;
#20702 = ORIENTED_EDGE ( 'NONE', *, *, #43903, .T. ) ;
#20703 = CARTESIAN_POINT ( 'NONE',  ( 10.55407258484730093, 1452.751878998079974, 209.9968945314950020 ) ) ;
#20704 = CARTESIAN_POINT ( 'NONE',  ( -24.08426373734519998, 1411.115196246010100, 208.6111089511020111 ) ) ;
#20705 = ORIENTED_EDGE ( 'NONE', *, *, #105925, .T. ) ;
#20706 = CARTESIAN_POINT ( 'NONE',  ( -0.3097659845029999692, 1413.830979672630065, 184.8391456572979905 ) ) ;
#20707 = DIRECTION ( 'NONE',  ( -0.02616798426500960631, -0.9993150019883682011, 0.02616798426500980407 ) ) ;
#20708 = CARTESIAN_POINT ( 'NONE',  ( 5.893213018790000035, 1451.599863458789969, 210.6385936290390077 ) ) ;
#20709 = CARTESIAN_POINT ( 'NONE',  ( -0.8321976068670000615, 1470.487602970729995, 235.6631316893979999 ) ) ;
#20710 = ADVANCED_FACE ( 'NONE', ( #27282, #53622 ), #79907, .T. ) ;
#20711 = CARTESIAN_POINT ( 'NONE',  ( 3.252451448209999985, 1444.627347679690047, 200.7572266927390103 ) ) ;
#20712 = ORIENTED_EDGE ( 'NONE', *, *, #80874, .T. ) ;
#20713 = VECTOR ( 'NONE', #84535, 1000.000000000000000 ) ;
#20714 =( NAMED_UNIT ( * ) PLANE_ANGLE_UNIT ( ) SI_UNIT ( $, .RADIAN. ) );
#20715 = CARTESIAN_POINT ( 'NONE',  ( -12.30902781859879980, 1415.426561690370136, 221.5637004564220263 ) ) ;
#20716 = ADVANCED_FACE ( 'NONE', ( #11045 ), #3220, .T. ) ;
#20717 = DIRECTION ( 'NONE',  ( 0.000000000000000000, 0.000000000000000000, 1.000000000000000000 ) ) ;
#20718 = ORIENTED_EDGE ( 'NONE', *, *, #32164, .T. ) ;
#20719 = CARTESIAN_POINT ( 'NONE',  ( 4.999456390405000228, 1516.830644417779922, 204.5005780481670001 ) ) ;
#20720 = ORIENTED_EDGE ( 'NONE', *, *, #84518, .T. ) ;
#20721 = CARTESIAN_POINT ( 'NONE',  ( 11.85926072867510150, 1431.858703157390210, 149.9614524602589825 ) ) ;
#20722 = CARTESIAN_POINT ( 'NONE',  ( 5.441672279850854110, 1511.126521620429685, 216.8250749836011835 ) ) ;
#20723 = VERTEX_POINT ( 'NONE', #28392 ) ;
#20724 = ORIENTED_EDGE ( 'NONE', *, *, #51714, .F. ) ;
#20725 = CARTESIAN_POINT ( 'NONE',  ( 0.4992773797353681764, 1524.841055067849766, 174.1119671515087077 ) ) ;
#20726 = CARTESIAN_POINT ( 'NONE',  ( -2.710244495734679848, 1508.047929154919984, 220.9036545897700137 ) ) ;
#20727 = CARTESIAN_POINT ( 'NONE',  ( 3.862810189448820264, 1497.382634203200041, 197.2226424524940285 ) ) ;
#20728 =( BOUNDED_CURVE ( )  B_SPLINE_CURVE ( 3, ( #2829, #87934, #11223, #80619 ),
 .UNSPECIFIED., .F., .T. ) 
 B_SPLINE_CURVE_WITH_KNOTS ( ( 4, 4 ),
 ( 4.712545041747917551, 6.283338160402144545 ),
 .UNSPECIFIED. ) 
 CURVE ( )  GEOMETRIC_REPRESENTATION_ITEM ( )  RATIONAL_B_SPLINE_CURVE ( ( 1.000000000000000000, 0.8047386102897660098, 0.8047386102897660098, 1.000000000000000000 ) ) 
 REPRESENTATION_ITEM ( '' )  );
#20729 = CARTESIAN_POINT ( 'NONE',  ( -5.795766362228450319, 1469.762611321129953, 217.6224603134940025 ) ) ;
#20730 = CARTESIAN_POINT ( 'NONE',  ( 19.55518754910140089, 1452.230178190589868, 143.7793110295839938 ) ) ;
#20731 = CARTESIAN_POINT ( 'NONE',  ( 9.225579725230000250, 1420.892510935600058, 196.8152382223989889 ) ) ;
#20732 = CARTESIAN_POINT ( 'NONE',  ( 1.106948036398740065, 1475.016812829990158, 220.4877511142580033 ) ) ;
#20733 = CARTESIAN_POINT ( 'NONE',  ( -109.7725577738988108, 1383.360694053928455, 297.1371496055471653 ) ) ;
#20734 = DIRECTION ( 'NONE',  ( 0.000000000000000000, 0.000000000000000000, 1.000000000000000000 ) ) ;
#20735 = CARTESIAN_POINT ( 'NONE',  ( 0.03381540887034163723, 1410.042656433180582, 233.1880969024354897 ) ) ;
#20737 = CARTESIAN_POINT ( 'NONE',  ( 16.83556426100000181, 1507.627022993330229, 193.5811530782980014 ) ) ;
#20736 = CARTESIAN_POINT ( 'NONE',  ( -14.24321357380000030, 1503.441202237889911, 208.7621914785800072 ) ) ;
#20738 = CARTESIAN_POINT ( 'NONE',  ( -68.34593600991827600, 1379.747695174417913, 279.8829065417061202 ) ) ;
#20739 = EDGE_CURVE ( 'NONE', #65067, #45960, #84142, .T. ) ;
#20740 = CARTESIAN_POINT ( 'NONE',  ( -24.71826599937909918, 1509.391144592290175, 222.6450861662429759 ) ) ;
#20741 = CARTESIAN_POINT ( 'NONE',  ( -6.564976431375000310, 1512.035910181030204, 201.6179728287370096 ) ) ;
#20742 = ORIENTED_EDGE ( 'NONE', *, *, #28541, .T. ) ;
#20743 = CARTESIAN_POINT ( 'NONE',  ( 24.08292308420000083, 1431.749769074620190, 243.9198229428980085 ) ) ;
#20744 = CARTESIAN_POINT ( 'NONE',  ( 41.66193277014346563, 1443.744876556161444, 136.1277638562497998 ) ) ;
#20745 = CARTESIAN_POINT ( 'NONE',  ( -105.8331820287869931, 1384.932354072029966, 311.2232221701380581 ) ) ;
#20746 = CARTESIAN_POINT ( 'NONE',  ( 17.78284146230000218, 1432.724246433989947, 213.5810953123289835 ) ) ;
#20747 = CARTESIAN_POINT ( 'NONE',  ( -8.268835750490000081, 1384.932997505379944, 199.7028512843090198 ) ) ;
#20748 = CARTESIAN_POINT ( 'NONE',  ( 0.0001732888907949209931, 1456.398128790439841, 144.1938086916980239 ) ) ;
#20750 = ORIENTED_EDGE ( 'NONE', *, *, #69410, .F. ) ;
#20749 = CARTESIAN_POINT ( 'NONE',  ( -4.155669664704369382, 1439.704322410719897, 185.4969487652249995 ) ) ;
#20751 = CARTESIAN_POINT ( 'NONE',  ( 17.08684344950000167, 1414.913528139129994, 210.5362852913079905 ) ) ;
#20752 = CARTESIAN_POINT ( 'NONE',  ( -24.18145766900000027, 1443.722874644100102, 211.6519070434079879 ) ) ;
#20753 = EDGE_CURVE ( 'NONE', #98801, #89436, #22635, .T. ) ;
#20754 = FACE_OUTER_BOUND ( 'NONE', #19068, .T. ) ;
#20755 = CARTESIAN_POINT ( 'NONE',  ( -2.480175250669919951, 1429.207669930499833, 200.0830571243679969 ) ) ;
#20756 = CARTESIAN_POINT ( 'NONE',  ( -9.295420174100000210, 1442.315068272750068, 184.6978245454979799 ) ) ;
#20757 = CARTESIAN_POINT ( 'NONE',  ( 16.98869690429640045, 1509.546007420790147, 233.7379480452109988 ) ) ;
#20758 = EDGE_CURVE ( 'NONE', #97290, #89473, #78808, .T. ) ;
#20759 = CARTESIAN_POINT ( 'NONE',  ( 8.884591108237419377, 1458.997830223579967, 202.8087305887910077 ) ) ;
#20760 = CARTESIAN_POINT ( 'NONE',  ( -12.29727565780000020, 1497.713060387329961, 227.1658498148980243 ) ) ;
#20761 = CARTESIAN_POINT ( 'NONE',  ( 12.44046721790000021, 1412.739136509929949, 228.9069206073980070 ) ) ;
#20762 = CARTESIAN_POINT ( 'NONE',  ( -5.573872061590000371, 1477.238916206189970, 218.8617125876789942 ) ) ;
#20763 = CARTESIAN_POINT ( 'NONE',  ( -21.61975802670946933, 1524.130440953581001, 234.4879735737366673 ) ) ;
#20764 = CARTESIAN_POINT ( 'NONE',  ( 3.251611325815000342, 1516.779243033999819, 206.8234764622770001 ) ) ;
#20765 = CARTESIAN_POINT ( 'NONE',  ( 46.15243926309999978, 1440.913083839520141, 268.2044236978980507 ) ) ;
#20766 = CARTESIAN_POINT ( 'NONE',  ( -18.27903283859999917, 1410.475184850630058, 224.2578147637979953 ) ) ;
#20767 = CARTESIAN_POINT ( 'NONE',  ( 18.91392684480000241, 1435.157588376100193, 144.3614089622979861 ) ) ;
#20768 = CARTESIAN_POINT ( 'NONE',  ( 19.88385004780000287, 1469.159394736730064, 191.8385097409980062 ) ) ;
#20769 = PRODUCT_DEFINITION_FORMATION_WITH_SPECIFIED_SOURCE ( 'ANY', '', #39314, .NOT_KNOWN. ) ;
#20770 = CARTESIAN_POINT ( 'NONE',  ( -16.64306880943670208, 1409.659795607699834, 192.3834754672400038 ) ) ;
#20771 = CARTESIAN_POINT ( 'NONE',  ( -0.5566428566430000613, 1475.834717975330022, 266.9610393015980208 ) ) ;
#20772 = CARTESIAN_POINT ( 'NONE',  ( -14.33027067026050005, 1416.949084347329972, 203.2389326530310143 ) ) ;
#20773 = CARTESIAN_POINT ( 'NONE',  ( -34.91933993935739977, 1435.878760628219879, 135.9122342505640120 ) ) ;
#20774 = CARTESIAN_POINT ( 'NONE',  ( 0.2141777920064759921, 1455.006893489930007, 183.1673017730030040 ) ) ;
#20775 = CARTESIAN_POINT ( 'NONE',  ( -12.39163543625050146, 1408.824655388370047, 216.1170731771779856 ) ) ;
#20776 = CARTESIAN_POINT ( 'NONE',  ( 8.900418934672700289, 1428.280648177160174, 213.0365380470040009 ) ) ;
#20777 = CARTESIAN_POINT ( 'NONE',  ( -4.290508133339999475, 1515.379316001789903, 208.7552447710999957 ) ) ;
#20778 = EDGE_CURVE ( 'NONE', #72498, #43776, #13934, .T. ) ;
#20779 = CARTESIAN_POINT ( 'NONE',  ( -7.597325770185070049, 1384.051822739160116, 219.0196936294289856 ) ) ;
#20780 = CARTESIAN_POINT ( 'NONE',  ( 11.94161923459999919, 1433.614922939690132, 146.9203179002980164 ) ) ;
#20781 = CARTESIAN_POINT ( 'NONE',  ( -27.23873616999999925, 1436.777316193260049, 136.7688712040979908 ) ) ;
#20782 = DIRECTION ( 'NONE',  ( -0.7414773880254650340, 5.145032927655519758E-15, 0.6709778558543747495 ) ) ;
#20783 = VERTEX_POINT ( 'NONE', #8132 ) ;
#20784 = CARTESIAN_POINT ( 'NONE',  ( 3.029075602040000259, 1477.864648017889749, 199.0898650909989840 ) ) ;
#20785 = CARTESIAN_POINT ( 'NONE',  ( 39.25629876709999877, 1437.713110276969928, 136.4562061956980017 ) ) ;
#20786 = CARTESIAN_POINT ( 'NONE',  ( -17.14873022714438378, 1468.567877217461501, 198.7365958164457993 ) ) ;
#20788 = EDGE_CURVE ( 'NONE', #96593, #81708, #70915, .T. ) ;
#20787 = CARTESIAN_POINT ( 'NONE',  ( -1.598721155459999993E-13, 1416.913060387330006, 219.9105610086979823 ) ) ;
#20789 = CARTESIAN_POINT ( 'NONE',  ( -15.24410741409210068, 1496.414356836550041, 193.0361994402150003 ) ) ;
#20790 = CARTESIAN_POINT ( 'NONE',  ( -31.26311019219999565, 1465.876731228030167, 269.3319192047979982 ) ) ;
#20791 = CARTESIAN_POINT ( 'NONE',  ( -11.69922274234029835, 1481.273184454980083, 210.9363146797530248 ) ) ;
#20792 = CARTESIAN_POINT ( 'NONE',  ( 18.89959452430000297, 1416.839692140529905, 210.6687134580079999 ) ) ;
#20793 = CARTESIAN_POINT ( 'NONE',  ( -28.18475952270000207, 1509.897293877830180, 212.1715675502779845 ) ) ;
#20794 = CARTESIAN_POINT ( 'NONE',  ( -83.70238417473080972, 1384.631100110490024, 306.0393046053840180 ) ) ;
#20795 = CARTESIAN_POINT ( 'NONE',  ( -35.18605615840250067, 1384.979076970040069, 208.8412567272559954 ) ) ;
#20796 = CARTESIAN_POINT ( 'NONE',  ( 17.84054676580419141, 1523.580203803270933, 180.3625987673424618 ) ) ;
#20797 = CARTESIAN_POINT ( 'NONE',  ( -3.660886842309849953, 1508.551704408389924, 204.4275887013349973 ) ) ;
#20798 = CARTESIAN_POINT ( 'NONE',  ( 14.58371298189999976, 1474.172472513229877, 223.7721885321980153 ) ) ;
#20799 = EDGE_CURVE ( 'NONE', #95904, #30629, #90894, .T. ) ;
#20800 = CIRCLE ( 'NONE', #97710, 2.000003390274323500 ) ;
#20801 = B_SPLINE_CURVE_WITH_KNOTS ( 'NONE', 3,
 ( #46305, #28928, #21597, #63118, #88278, #89377 ),
 .UNSPECIFIED., .F., .F.,
 ( 4, 2, 4 ),
 ( -0.03349458847672189682, -0.01726308003882509948, -1.826968507034898437E-10 ),
 .UNSPECIFIED. ) ;
#20802 = CARTESIAN_POINT ( 'NONE',  ( 17.88592295531849885, 1419.953674261470042, 224.4724256833490017 ) ) ;
#20803 = VECTOR ( 'NONE', #29618, 1000.000000000000114 ) ;
#20805 = ORIENTED_EDGE ( 'NONE', *, *, #110602, .T. ) ;
#20804 = CARTESIAN_POINT ( 'NONE',  ( -0.8241248838030009738, 1509.075058821990069, 218.0915817195690067 ) ) ;
#20806 = CARTESIAN_POINT ( 'NONE',  ( -13.70491633070000148, 1508.146349234029913, 184.2330007275980108 ) ) ;
#20807 = DIRECTION ( 'NONE',  ( 0.9125304618753903307, 0.000000000000000000, -0.4090087482554460863 ) ) ;
#20808 = DIRECTION ( 'NONE',  ( -0.9455185755993178454, 0.000000000000000000, 0.3255681544571537578 ) ) ;
#20809 = CARTESIAN_POINT ( 'NONE',  ( -12.54563646380000108, 1416.254459047329874, 194.9661771226980136 ) ) ;
#20810 = DIRECTION ( 'NONE',  ( -1.000000000000000000, 0.000000000000000000, 0.000000000000000000 ) ) ;
#20811 = CARTESIAN_POINT ( 'NONE',  ( 23.89076625480000260, 1410.242936702429915, 209.5801481993979962 ) ) ;
#20812 = CARTESIAN_POINT ( 'NONE',  ( -11.99985923319999870, 1433.681662988860126, 149.8469377335979971 ) ) ;
#20813 = CARTESIAN_POINT ( 'NONE',  ( -18.51202227299100045, 1466.632449115480085, 200.9222626566809993 ) ) ;
#20814 = CARTESIAN_POINT ( 'NONE',  ( -15.52116303490000071, 1422.636867011229924, 228.4575560400980123 ) ) ;
#20816 = CARTESIAN_POINT ( 'NONE',  ( -11.70591916684050027, 1426.716063593939907, 141.9425537506020021 ) ) ;
#20815 = CARTESIAN_POINT ( 'NONE',  ( -11.77285519380000167, 1432.580890241690213, 150.8112885044980089 ) ) ;
#20817 = CARTESIAN_POINT ( 'NONE',  ( -9.448886036450000248, 1383.288095429739997, 218.3547579606889997 ) ) ;
#20818 = CIRCLE ( 'NONE', #72717, 1.000000000000000888 ) ;
#20819 = CARTESIAN_POINT ( 'NONE',  ( -102.2221789262000726, 1377.418846546389204, 293.0440248834591443 ) ) ;
#20820 = CARTESIAN_POINT ( 'NONE',  ( -234.5897387251999930, 11221.53578756869865, 2175.945776423289772 ) ) ;
#20821 = EDGE_CURVE ( 'NONE', #7200, #61381, #85523, .T. ) ;
#20822 = CARTESIAN_POINT ( 'NONE',  ( -28.15442856212169787, 1509.896234822020006, 200.8410265843269826 ) ) ;
#20823 = CARTESIAN_POINT ( 'NONE',  ( 4.501691961669999742, 1368.956319095230128, 210.6218459616991936 ) ) ;
#20824 = B_SPLINE_CURVE_WITH_KNOTS ( 'NONE', 5,
 ( #85525, #1559, #25618, #60925, #93383, #41889, #50847, #1014, #9391 ),
 .UNSPECIFIED., .F., .F.,
 ( 6, 3, 6 ),
 ( 0.000000000000000000, 0.5000000000000000000, 1.000000000000000000 ),
 .UNSPECIFIED. ) ;
#20825 = CARTESIAN_POINT ( 'NONE',  ( 2.867803626105000170, 1516.994127245590107, 204.4971090729170271 ) ) ;
#20826 = CARTESIAN_POINT ( 'NONE',  ( -16.76078030769999927, 1420.494757909599912, 203.1294657649889928 ) ) ;
#20827 = CARTESIAN_POINT ( 'NONE',  ( -16.69587879669180097, 1485.679718023270198, 187.8645734870310093 ) ) ;
#20828 = EDGE_CURVE ( 'NONE', #20993, #96103, #6749, .T. ) ;
#20829 = CARTESIAN_POINT ( 'NONE',  ( -9.148257661150001496, 1423.748799908730007, 207.7944249153989915 ) ) ;
#20830 = CARTESIAN_POINT ( 'NONE',  ( -4.265900750095979355, 1441.170003579950162, 158.5225822146180121 ) ) ;
#20832 = ORIENTED_EDGE ( 'NONE', *, *, #108567, .T. ) ;
#20831 = CARTESIAN_POINT ( 'NONE',  ( -67.58960521306219960, 1379.745587075000003, 278.8661543758199741 ) ) ;
#20833 = ORIENTED_EDGE ( 'NONE', *, *, #83756, .F. ) ;
#20834 = CARTESIAN_POINT ( 'NONE',  ( 29.36446925850000156, 1509.951008955230009, 212.6618214604380057 ) ) ;
#20835 = EDGE_LOOP ( 'NONE', ( #95356, #68801, #77211, #38473, #17226 ) ) ;
#20836 = CARTESIAN_POINT ( 'NONE',  ( -0.8838665694872513967, 1457.292915820307371, 199.6410733348866415 ) ) ;
#20837 = CARTESIAN_POINT ( 'NONE',  ( -109.4845004149999994, 1384.937458541380011, 311.2840473662590171 ) ) ;
#20839 = CARTESIAN_POINT ( 'NONE',  ( 1.476968277879999958, 1508.190462730230138, 180.8898692100979986 ) ) ;
#20838 = FACE_OUTER_BOUND ( 'NONE', #57123, .T. ) ;
#20840 = CARTESIAN_POINT ( 'NONE',  ( 11.88140585900000090, 1433.447543843229823, 147.6490162021979984 ) ) ;
#20841 = CARTESIAN_POINT ( 'NONE',  ( -25.81326821525899717, 1450.788444190880000, 136.8507296241930078 ) ) ;
#20842 = CARTESIAN_POINT ( 'NONE',  ( -1.431441865960000115, 1468.042762720489918, 219.7628109989989866 ) ) ;
#20843 = CARTESIAN_POINT ( 'NONE',  ( 2.760778140020000215, 1409.009468884330090, 230.1977480460979848 ) ) ;
#20844 = CARTESIAN_POINT ( 'NONE',  ( 9.329257343867968899, 1483.543149501509788, 214.5330026594239996 ) ) ;
#20845 = CARTESIAN_POINT ( 'NONE',  ( -1.702406023195000007, 1516.999105586269934, 212.3918307515370145 ) ) ;
#20846 = CARTESIAN_POINT ( 'NONE',  ( 38.86831401555139820, 1437.615293293499690, 134.0999999973729757 ) ) ;
#20847 = DIRECTION ( 'NONE',  ( 0.8090169943747140824, -7.703825410061002683E-33, 0.5877852522927943246 ) ) ;
#20848 = ORIENTED_EDGE ( 'NONE', *, *, #35860, .F. ) ;
#20849 = CARTESIAN_POINT ( 'NONE',  ( -2.515613294380000031, 1448.349718812090032, 188.5842421506989979 ) ) ;
#20850 = CARTESIAN_POINT ( 'NONE',  ( -2.542680546169759914, 1431.030268854349970, 201.1441491798630068 ) ) ;
#20851 = B_SPLINE_CURVE_WITH_KNOTS ( 'NONE', 3,
 ( #40510, #47818, #30457, #6362 ),
 .UNSPECIFIED., .F., .F.,
 ( 4, 4 ),
 ( 0.000000000000000000, 0.0002960034161023850021 ),
 .UNSPECIFIED. ) ;
#20852 = ORIENTED_EDGE ( 'NONE', *, *, #19527, .T. ) ;
#20853 = ORIENTED_EDGE ( 'NONE', *, *, #63909, .T. ) ;
#20854 = EDGE_LOOP ( 'NONE', ( #94608, #17055, #37669, #80401 ) ) ;
#20855 = CARTESIAN_POINT ( 'NONE',  ( -6.787530816394999889, 1514.254015528269974, 216.9772499547270002 ) ) ;
#20856 = CARTESIAN_POINT ( 'NONE',  ( 32.39800393421785429, 1524.816548299036867, 217.0524289663465538 ) ) ;
#20857 = CARTESIAN_POINT ( 'NONE',  ( 11.19501794742983058, 1451.281070894506001, 151.7798007822887882 ) ) ;
#20858 = CARTESIAN_POINT ( 'NONE',  ( 0.000000000000000000, 1420.584111001019892, 209.1218459616989946 ) ) ;
#20859 = CARTESIAN_POINT ( 'NONE',  ( 11.45444494140000025, 1502.281967335889931, 208.2980153205920146 ) ) ;
#20860 = VECTOR ( 'NONE', #24631, 1000.000000000000000 ) ;
#20861 = DIRECTION ( 'NONE',  ( 0.000000000000000000, -1.000000000000000000, 0.000000000000000000 ) ) ;
#20862 = CARTESIAN_POINT ( 'NONE',  ( -67.56224301914092223, 1379.745465240531303, 277.5421263419358411 ) ) ;
#20863 = CARTESIAN_POINT ( 'NONE',  ( -0.6779417998419989821, 1464.763158441590122, 198.8934648891990093 ) ) ;
#20864 = CARTESIAN_POINT ( 'NONE',  ( -0.7373154782470000557, 1497.695374981930172, 231.4735153508979977 ) ) ;
#20865 = DIRECTION ( 'NONE',  ( -0.000000000000000000, -1.000000000000000000, -0.000000000000000000 ) ) ;
#20866 = CARTESIAN_POINT ( 'NONE',  ( -51.61765082585089459, 1384.627073787560221, 227.8738222896710113 ) ) ;
#20867 = EDGE_LOOP ( 'NONE', ( #15329, #45928 ) ) ;
#20868 = CARTESIAN_POINT ( 'NONE',  ( 2.476170596904999854, 1516.819260244609950, 207.4047612206870213 ) ) ;
#20869 = EDGE_LOOP ( 'NONE', ( #44121, #63841, #78174, #7626 ) ) ;
#20870 = CARTESIAN_POINT ( 'NONE',  ( 26.99384459419149707, 1440.913060387330006, 245.0106952250010011 ) ) ;
#20871 = CARTESIAN_POINT ( 'NONE',  ( 11.26937486967429969, 1478.652699849539886, 205.8601904136019982 ) ) ;
#20872 = ORIENTED_EDGE ( 'NONE', *, *, #100073, .F. ) ;
#20873 = DIRECTION ( 'NONE',  ( 1.836970198721029688E-16, 1.000000000000000000, -1.262177448353620010E-31 ) ) ;
#20874 = CARTESIAN_POINT ( 'NONE',  ( -15.94346743280000034, 1409.469818538429990, 192.9752478756980167 ) ) ;
#20875 = CARTESIAN_POINT ( 'NONE',  ( -23.42267282419999930, 1430.824224223030114, 212.0368849767579889 ) ) ;
#20877 = CARTESIAN_POINT ( 'NONE',  ( -1.058602696091491602, 1414.913060387330006, 225.4991512363474726 ) ) ;
#20876 = CARTESIAN_POINT ( 'NONE',  ( -24.67251852870000306, 1441.156518004890131, 210.6924577872079851 ) ) ;
#20878 = CARTESIAN_POINT ( 'NONE',  ( -9.014963715518330645, 1437.210665075589986, 213.0690570958229841 ) ) ;
#20879 = DIRECTION ( 'NONE',  ( 0.9455185755993178454, 0.000000000000000000, -0.3255681544571537578 ) ) ;
#20880 = CARTESIAN_POINT ( 'NONE',  ( -3.567500082150000029, 1508.690877485930059, 180.4371975227980158 ) ) ;
#20881 = CARTESIAN_POINT ( 'NONE',  ( -27.67757344910459949, 1441.322428384430168, 137.2891306214100098 ) ) ;
#20882 = CARTESIAN_POINT ( 'NONE',  ( -6.349044579700000135, 1508.776756645290106, 219.5917579706989784 ) ) ;
#20884 = CARTESIAN_POINT ( 'NONE',  ( -104.1336782687082234, 1379.826409842592739, 304.0106197004701585 ) ) ;
#20883 = CARTESIAN_POINT ( 'NONE',  ( 7.819645599040000228, 1463.567355340829863, 234.8427059997979995 ) ) ;
#20885 = CARTESIAN_POINT ( 'NONE',  ( -3.452917061035000401, 1517.089216728169959, 216.0711116162470091 ) ) ;
#20886 = CYLINDRICAL_SURFACE ( 'NONE', #108790, 2.000000000000002220 ) ;
#20887 = CARTESIAN_POINT ( 'NONE',  ( 6.014475185372909927, 1511.645396655840159, 217.0724277449770057 ) ) ;
#20888 = CARTESIAN_POINT ( 'NONE',  ( 19.30664356132462700, 1442.871878066172258, 213.0659908379712704 ) ) ;
#20889 = CARTESIAN_POINT ( 'NONE',  ( 4.043366220174999803, 1516.951766529250108, 211.9887038632370206 ) ) ;
#20890 = CARTESIAN_POINT ( 'NONE',  ( -19.64184507200000240, 1452.819461536229937, 209.3501247966860035 ) ) ;
#20891 = CARTESIAN_POINT ( 'NONE',  ( 30.00906612072600765, 1525.856065479257722, 221.1186961711726155 ) ) ;
#20893 = ORIENTED_EDGE ( 'NONE', *, *, #22823, .T. ) ;
#20892 = CARTESIAN_POINT ( 'NONE',  ( -106.7752590979999923, 1385.237353006989906, 297.1314966531590471 ) ) ;
#20894 = CARTESIAN_POINT ( 'NONE',  ( -16.62425451295051104, 1524.075000532257263, 237.7045424426785019 ) ) ;
#20895 = CARTESIAN_POINT ( 'NONE',  ( 4.387875208460000565, 1463.596605969929897, 232.0486588174979943 ) ) ;
#20896 = CARTESIAN_POINT ( 'NONE',  ( 8.416897302759883459, 1484.129603243253086, 215.7648255120577687 ) ) ;
#20897 = CARTESIAN_POINT ( 'NONE',  ( -14.87384579849999966, 1416.121162261860036, 204.9838385039689683 ) ) ;
#20898 = CARTESIAN_POINT ( 'NONE',  ( 2.189642700659999885, 1414.529581730530026, 232.0476498270979846 ) ) ;
#20899 = DIRECTION ( 'NONE',  ( -0.009310542140203791062, -0.9999463363072063071, 0.004542940771242790637 ) ) ;
#20901 = CARTESIAN_POINT ( 'NONE',  ( 2.500000000000000000, 1432.320537255040108, 157.4939813259980212 ) ) ;
#20900 = CARTESIAN_POINT ( 'NONE',  ( -24.24300079589999868, 1470.078714870129943, 216.9670906892179971 ) ) ;
#20903 = CARTESIAN_POINT ( 'NONE',  ( -12.26982153759260008, 1378.706398924530049, 210.4710096042489909 ) ) ;
#20902 = VECTOR ( 'NONE', #85070, 1000.000000000000000 ) ;
#20904 = CARTESIAN_POINT ( 'NONE',  ( -106.5015102169999892, 1378.995521017789997, 308.0072629902589938 ) ) ;
#20905 = VERTEX_POINT ( 'NONE', #83202 ) ;
#20906 = CARTESIAN_POINT ( 'NONE',  ( -0.7568987378019988999, 1516.805675336850072, 205.0906771642370074 ) ) ;
#20907 = CARTESIAN_POINT ( 'NONE',  ( 0.7745009778729999850, 1406.071044366729893, 269.0454658058980044 ) ) ;
#20908 = CARTESIAN_POINT ( 'NONE',  ( -0.008119676937300529876, 1515.178500008189985, 213.4483172118689822 ) ) ;
#20909 = CARTESIAN_POINT ( 'NONE',  ( 44.93138632836440394, 1446.458187732969918, 269.6837875076539603 ) ) ;
#20910 = CARTESIAN_POINT ( 'NONE',  ( -7.627639037761098528, 1513.425324099843010, 202.6766267095247258 ) ) ;
#20911 = CARTESIAN_POINT ( 'NONE',  ( 11.60004869885203682, 1422.586092030433520, 135.6000000024070573 ) ) ;
#20912 = EDGE_CURVE ( 'NONE', #49524, #95045, #83934, .T. ) ;
#20913 = CARTESIAN_POINT ( 'NONE',  ( 3.424720300894999792, 1517.051704408389924, 200.5840233334270124 ) ) ;
#20914 = CARTESIAN_POINT ( 'NONE',  ( -1.971747436821430055, 1450.333125910620083, 155.0636771872389943 ) ) ;
#20915 = CARTESIAN_POINT ( 'NONE',  ( 4.219439013950669448, 1441.595895969210005, 182.7715284958480026 ) ) ;
#20916 = ADVANCED_FACE ( 'NONE', ( #28256 ), #96243, .T. ) ;
#20917 = CARTESIAN_POINT ( 'NONE',  ( 10.78159844869479933, 1461.896569297480028, 211.1674770051990038 ) ) ;
#20918 = CIRCLE ( 'NONE', #97893, 1.999999999999967359 ) ;
#20919 = CARTESIAN_POINT ( 'NONE',  ( -13.98791200573939975, 1415.441076448560125, 220.9116194232070143 ) ) ;
#20920 = DIRECTION ( 'NONE',  ( 1.000000000000000000, 0.000000000000000000, 0.000000000000000000 ) ) ;
#20921 = VERTEX_POINT ( 'NONE', #77568 ) ;
#20922 = CARTESIAN_POINT ( 'NONE',  ( -17.87874069189999915, 1415.075539390429867, 265.6112251771979800 ) ) ;
#20923 = CARTESIAN_POINT ( 'NONE',  ( 6.762278413896400053, 1467.457330156850048, 200.6363351971689895 ) ) ;
#20924 = CARTESIAN_POINT ( 'NONE',  ( -0.8893057567669999663, 1476.070256768630088, 267.5368301733980161 ) ) ;
#20925 = CARTESIAN_POINT ( 'NONE',  ( -16.66101146819999812, 1410.867390116229899, 191.7375337716979971 ) ) ;
#20926 = CARTESIAN_POINT ( 'NONE',  ( -12.03841672722804290, 1513.050507398017544, 192.5203960790572069 ) ) ;
#20927 = CARTESIAN_POINT ( 'NONE',  ( 7.000633479060000219, 1424.213547369589833, 212.7272991732289995 ) ) ;
#20928 = CARTESIAN_POINT ( 'NONE',  ( -28.73531012334500190, 1384.833055677890115, 226.7915508562620062 ) ) ;
#20929 = AXIS2_PLACEMENT_3D ( 'NONE', #5536, #30167, #63807 ) ;
#20930 = EDGE_CURVE ( 'NONE', #25738, #63587, #55151, .T. ) ;
#20931 = CARTESIAN_POINT ( 'NONE',  ( 12.29186695254770001, 1491.851815450179856, 208.3259444585769984 ) ) ;
#20932 = DIRECTION ( 'NONE',  ( -0.9455185755993178454, 0.000000000000000000, 0.3255681544571539243 ) ) ;
#20933 = CARTESIAN_POINT ( 'NONE',  ( 7.891777514710270225, 1512.314860025949883, 206.1798159824890035 ) ) ;
#20934 = CARTESIAN_POINT ( 'NONE',  ( -5.043610348250129327, 1396.089187143350046, 218.9331246055930080 ) ) ;
#20935 =( BOUNDED_SURFACE ( )  B_SPLINE_SURFACE ( 3, 2, ( 
 ( #54290, #88416, #45879 ),
 ( #3337, #105783, #63249 ),
 ( #97358, #88955, #46436 ),
 ( #80568, #55377, #91164 ),
 ( #65997, #108517, #31808 ),
 ( #64333, #13884, #106849 ) ),
 .UNSPECIFIED., .F., .F., .F. ) 
 B_SPLINE_SURFACE_WITH_KNOTS ( ( 4, 2, 4 ),
 ( 3, 3 ),
 ( -2.168404344971008868E-17, 0.001312027981647260989, 0.002624055963294543662 ),
 ( 0.000000000000000000, 1.000000000000000000 ),
 .UNSPECIFIED. ) 
 GEOMETRIC_REPRESENTATION_ITEM ( )  RATIONAL_B_SPLINE_SURFACE ( (
 ( 1.000000000000000000, 0.9376006582765930020, 1.000000000000000000),
 ( 1.000000000000000000, 0.9569320108022597582, 1.000000000000000000),
 ( 1.000000000000000000, 0.9725743441618913687, 1.000000000000000000),
 ( 1.000000000000000000, 0.9942095667135614212, 1.000000000000000000),
 ( 1.000000000000000000, 1.000043666450708191, 1.000000000000000000),
 ( 1.000000000000000000, 1.000000000000000000, 1.000000000000000000) ) ) 
 REPRESENTATION_ITEM ( '' )  SURFACE ( )  );
#20936 = CARTESIAN_POINT ( 'NONE',  ( -15.64557667610000102, 1421.345166096630010, 227.1284468425980094 ) ) ;
#20937 = CARTESIAN_POINT ( 'NONE',  ( -45.63153662610000083, 1440.326745910319914, 268.9749020108980062 ) ) ;
#20938 = EDGE_LOOP ( 'NONE', ( #97808, #48348, #76472, #102548 ) ) ;
#20939 = CARTESIAN_POINT ( 'NONE',  ( -4.660393612750000081, 1436.848553822789881, 227.0391165213990234 ) ) ;
#20940 = CARTESIAN_POINT ( 'NONE',  ( -15.58456279011612544, 1415.964423084322789, 207.9695922479936030 ) ) ;
#20941 = CARTESIAN_POINT ( 'NONE',  ( -14.59646112059999901, 1484.617543311429927, 186.9027180520979812 ) ) ;
#20943 = CARTESIAN_POINT ( 'NONE',  ( -11.74940792826499880, 1512.456207068040158, 192.6559229132670055 ) ) ;
#20942 = CARTESIAN_POINT ( 'NONE',  ( 11.51723948480000104, 1426.416094619729847, 128.4916607458980309 ) ) ;
#20944 = CARTESIAN_POINT ( 'NONE',  ( 5.402232622379999017E-16, 1413.913060387330006, 209.1218459616979999 ) ) ;
#20945 = CARTESIAN_POINT ( 'NONE',  ( -12.31045119098629925, 1378.376187953739873, 209.7947064970520046 ) ) ;
#20946 = CARTESIAN_POINT ( 'NONE',  ( -1.708092304294999808, 1516.523379810429788, 201.4131002843170108 ) ) ;
#20947 = CARTESIAN_POINT ( 'NONE',  ( 7.422111136049999836, 1427.425960435760089, 212.9291018486189841 ) ) ;
#20949 = CARTESIAN_POINT ( 'NONE',  ( -4.897375497219999652, 1432.353341358199941, 150.0655110971979980 ) ) ;
#20948 = CIRCLE ( 'NONE', #87073, 31.41749213351482695 ) ;
#20950 = CARTESIAN_POINT ( 'NONE',  ( 15.52404075913500137, 1511.843510977570077, 197.7123968315669913 ) ) ;
#20951 = DIRECTION ( 'NONE',  ( 0.000000000000000000, 1.000000000000000000, 0.000000000000000000 ) ) ;
#20952 = CARTESIAN_POINT ( 'NONE',  ( -42.70274084799289938, 1379.638451954410129, 233.1566849246620166 ) ) ;
#20953 = ADVANCED_FACE ( 'NONE', ( #88176 ), #81082, .F. ) ;
#20954 = CARTESIAN_POINT ( 'NONE',  ( 7.552428968428530176, 1365.649644077722996, 208.3718459617061285 ) ) ;
#20956 = ORIENTED_EDGE ( 'NONE', *, *, #15331, .F. ) ;
#20955 = CARTESIAN_POINT ( 'NONE',  ( -19.25299971689319989, 1379.621289133459868, 212.6578715478160007 ) ) ;
#20957 = ORIENTED_EDGE ( 'NONE', *, *, #90539, .T. ) ;
#20958 = CARTESIAN_POINT ( 'NONE',  ( -5.343479920809999228, 1396.099658817930049, 199.4684377758579785 ) ) ;
#20959 = CARTESIAN_POINT ( 'NONE',  ( -14.33393486070000122, 1409.413612422530150, 192.0174323315980018 ) ) ;
#20960 = CARTESIAN_POINT ( 'NONE',  ( 6.940379574320000522, 1431.113060387329824, 226.8285010592979916 ) ) ;
#20961 = CARTESIAN_POINT ( 'NONE',  ( -7.717016657154999848, 1511.440441732939917, 212.3987529968069907 ) ) ;
#20964 = EDGE_CURVE ( 'NONE', #71433, #54724, #32402, .T. ) ;
#20963 = CARTESIAN_POINT ( 'NONE',  ( -1.366316002913839922, 1417.860790559529960, 185.2850244214669999 ) ) ;
#20962 = CARTESIAN_POINT ( 'NONE',  ( -8.784226513880000198, 1383.880421208059943, 218.5159863009489811 ) ) ;
#20965 = CARTESIAN_POINT ( 'NONE',  ( -31.34137657934026677, 1523.382868172864164, 196.3411265156551906 ) ) ;
#20966 = CARTESIAN_POINT ( 'NONE',  ( -40.24076440061289617, 1444.613910935890090, 137.0282073429019931 ) ) ;
#20967 = PRESENTATION_STYLE_ASSIGNMENT (( #78696 ) ) ;
#20968 = CARTESIAN_POINT ( 'NONE',  ( 37.07887392490540179, 1437.327007662029928, 136.4872220464899897 ) ) ;
#20969 = CARTESIAN_POINT ( 'NONE',  ( 6.014260514953510217, 1396.123082992429772, 218.3773295970819959 ) ) ;
#20970 = CARTESIAN_POINT ( 'NONE',  ( 33.91375829818579746, 1435.681794709440055, 135.0664790576290102 ) ) ;
#20971 = CARTESIAN_POINT ( 'NONE',  ( -1.514297760018489925, 1406.518541415770187, 269.4982389579009805 ) ) ;
#20972 = DIRECTION ( 'NONE',  ( 0.9996573249755574819, 0.02617694830786558916, 0.000000000000000000 ) ) ;
#20973 = ORIENTED_EDGE ( 'NONE', *, *, #89633, .T. ) ;
#20974 = FACE_OUTER_BOUND ( 'NONE', #64827, .T. ) ;
#20975 = FACE_OUTER_BOUND ( 'NONE', #98264, .T. ) ;
#20976 = ORIENTED_EDGE ( 'NONE', *, *, #44595, .T. ) ;
#20977 = EDGE_LOOP ( 'NONE', ( #101128, #48979, #45262, #56260 ) ) ;
#20978 = CARTESIAN_POINT ( 'NONE',  ( 10.93679547204000002, 1490.434980368090010, 209.9321327948960061 ) ) ;
#20979 = CARTESIAN_POINT ( 'NONE',  ( -13.73081170289999875, 1460.732406911229873, 231.6108505850980066 ) ) ;
#20980 = CIRCLE ( 'NONE', #44268, 1.999999999999998668 ) ;
#20981 = CARTESIAN_POINT ( 'NONE',  ( 7.333070134885000257, 1516.955859323880077, 214.9008457440070003 ) ) ;
#20982 = FACE_OUTER_BOUND ( 'NONE', #71323, .T. ) ;
#20983 = EDGE_LOOP ( 'NONE', ( #72684, #32704, #44253, #74385 ) ) ;
#20984 = CARTESIAN_POINT ( 'NONE',  ( -5.947813039672949387, 1509.175827024919954, 179.7301802773710051 ) ) ;
#20985 = CARTESIAN_POINT ( 'NONE',  ( -35.85007572059999603, 1375.172836988449944, 220.5090016197590046 ) ) ;
#20986 = B_SPLINE_CURVE_WITH_KNOTS ( 'NONE', 3,
 ( #92886, #25671, #109699, #59864, #16702, #68827, #76101, #102389, #26229, #85033 ),
 .UNSPECIFIED., .F., .F.,
 ( 4, 3, 3, 4 ),
 ( 0.9035847615492319518, 0.9657249562039529334, 1.011896175524879871, 1.040557828610000124 ),
 .UNSPECIFIED. ) ;
#20987 = CARTESIAN_POINT ( 'NONE',  ( 2.525974529359999998, 1414.913060387329779, 224.9911480561979999 ) ) ;
#20988 = CARTESIAN_POINT ( 'NONE',  ( -5.010423001364999962, 1516.929569650079884, 205.0907035804270038 ) ) ;
#20989 = CARTESIAN_POINT ( 'NONE',  ( -28.25086440149999945, 1508.135696992230123, 208.8579908607459856 ) ) ;
#20990 = DIRECTION ( 'NONE',  ( 0.02616798426500960631, 0.9993150019883683122, 0.02616798426500960631 ) ) ;
#20991 = CARTESIAN_POINT ( 'NONE',  ( -4.934427622899999477, 1409.085374397729993, 230.8376437965980301 ) ) ;
#20993 = VERTEX_POINT ( 'NONE', #71958 ) ;
#20992 = CARTESIAN_POINT ( 'NONE',  ( -11.34090880850000005, 1475.513060387329915, 191.0454207575980092 ) ) ;
#20994 = DIRECTION ( 'NONE',  ( 0.000000000000000000, 0.000000000000000000, -1.000000000000000000 ) ) ;
#20995 = CARTESIAN_POINT ( 'NONE',  ( 1.719367447207400090, 1490.891747713500081, 235.7942165085109991 ) ) ;
#20997 = CARTESIAN_POINT ( 'NONE',  ( 21.63849897582232273, 1519.551704408389924, 202.6852139837732523 ) ) ;
#20996 = CIRCLE ( 'NONE', #62134, 1.000000000000000888 ) ;
#20998 = CARTESIAN_POINT ( 'NONE',  ( 17.04824238339829634, 1423.676546790900147, 228.9394188427949928 ) ) ;
#20999 = CARTESIAN_POINT ( 'NONE',  ( 20.84494148150000115, 1411.509465946430055, 270.2130226657980074 ) ) ;
#21000 = CARTESIAN_POINT ( 'NONE',  ( 6.948321705865000197, 1517.049325831759916, 213.1561268858870051 ) ) ;
#21001 = CARTESIAN_POINT ( 'NONE',  ( -66.57398076899998784, 1379.745927938969999, 275.7277585373589659 ) ) ;
#21002 = CIRCLE ( 'NONE', #63981, 1.000000000000001554 ) ;
#21003 = CARTESIAN_POINT ( 'NONE',  ( 23.61592788680000154, 1410.127845046630227, 208.5598851522910024 ) ) ;
#21004 = CARTESIAN_POINT ( 'NONE',  ( 0.02005075328566424328, 1507.220604446680682, 237.3599021426030049 ) ) ;
#21005 = CARTESIAN_POINT ( 'NONE',  ( 15.42100696471130128, 1427.564330775570170, 199.6300130664099868 ) ) ;
#21006 = CARTESIAN_POINT ( 'NONE',  ( -7.708848719128969407, 1516.527314490149820, 211.2746510465439940 ) ) ;
#21007 = CARTESIAN_POINT ( 'NONE',  ( -7.326072182274999456, 1516.714320817460020, 209.8751461055349807 ) ) ;
#21008 = ORIENTED_EDGE ( 'NONE', *, *, #21892, .F. ) ;
#21009 = CARTESIAN_POINT ( 'NONE',  ( 4.308397161744589532, 1421.939254178800184, 184.0347638950579778 ) ) ;
#21010 = CARTESIAN_POINT ( 'NONE',  ( -1.314354605479999938, 1420.453030399730096, 233.4140791911979989 ) ) ;
#21011 = CARTESIAN_POINT ( 'NONE',  ( -89.65053622680001411, 1384.736506983960226, 308.7475415573589999 ) ) ;
#21012 = ORIENTED_EDGE ( 'NONE', *, *, #1467, .T. ) ;
#21013 = CARTESIAN_POINT ( 'NONE',  ( -30.62646649957819989, 1385.230650423509815, 228.7000830702139922 ) ) ;
#21014 = CARTESIAN_POINT ( 'NONE',  ( -10.81518740880000173, 1424.921099675630103, 144.1705347734979910 ) ) ;
#21015 = CARTESIAN_POINT ( 'NONE',  ( -20.81060428327939960, 1508.370615559120097, 228.0279630968090032 ) ) ;
#21016 = CARTESIAN_POINT ( 'NONE',  ( -106.7386147527374902, 1391.793769404327804, 307.5809084578692705 ) ) ;
#21017 = CARTESIAN_POINT ( 'NONE',  ( 11.46412257490000108, 1426.137423974189915, 205.4576714340990122 ) ) ;
#21018 = CARTESIAN_POINT ( 'NONE',  ( -0.03430450970949740219, 1420.445176861049958, 182.6785821352689823 ) ) ;
#21020 = CARTESIAN_POINT ( 'NONE',  ( -16.54876248606459299, 1416.988855567187784, 207.7154296687141084 ) ) ;
#21019 = CARTESIAN_POINT ( 'NONE',  ( 4.617490466775000080, 1516.685667699390024, 216.4467608883869900 ) ) ;
#21021 = CARTESIAN_POINT ( 'NONE',  ( 18.63787275289999812, 1508.244465050629969, 188.4525138200980052 ) ) ;
#21022 = CARTESIAN_POINT ( 'NONE',  ( -113.3410085367727334, 1379.913060387289988, 301.7225420527167898 ) ) ;
#21023 = VECTOR ( 'NONE', #46255, 1000.000000000000000 ) ;
#21024 = ORIENTED_EDGE ( 'NONE', *, *, #18526, .T. ) ;
#21025 = CARTESIAN_POINT ( 'NONE',  ( -2.872700555325000238, 1516.559109716219837, 201.4121646638069763 ) ) ;
#21026 = DIRECTION ( 'NONE',  ( 9.970439643713600747E-17, 0.7071067811865474617, 0.7071067811865474617 ) ) ;
#21027 = ORIENTED_EDGE ( 'NONE', *, *, #8891, .T. ) ;
#21028 = CARTESIAN_POINT ( 'NONE',  ( -15.90990259576500065, 1512.830284628050094, 220.0820010595669771 ) ) ;
#21029 = CARTESIAN_POINT ( 'NONE',  ( 9.952822627054100479, 1435.746504192841257, 152.5237976836565679 ) ) ;
#21030 = CARTESIAN_POINT ( 'NONE',  ( 8.033566663349164472, 1423.901403140259163, 195.8561929068294774 ) ) ;
#21031 = PRODUCT_DEFINITION_CONTEXT ( 'detailed design', #20555, 'design' ) ;
#21032 = CARTESIAN_POINT ( 'NONE',  ( 2.194612407920000230, 1441.754231285490050, 218.8080856977990152 ) ) ;
#21033 = CARTESIAN_POINT ( 'NONE',  ( 16.42688314034032260, 1421.633920429433374, 227.1747839813914140 ) ) ;
#21034 = CARTESIAN_POINT ( 'NONE',  ( -4.220927954649999592, 1446.217199771449941, 167.4561887392980282 ) ) ;
#21035 = CARTESIAN_POINT ( 'NONE',  ( -20.26420847629999855, 1427.565864917729868, 222.2644582469980037 ) ) ;
#21036 = CARTESIAN_POINT ( 'NONE',  ( -15.23375471800000014, 1435.180443442269961, 148.6429311973979850 ) ) ;
#21037 = CARTESIAN_POINT ( 'NONE',  ( -105.0196130309999916, 1390.463866858269739, 304.1900705858589617 ) ) ;
#21038 = CARTESIAN_POINT ( 'NONE',  ( 16.93884269750000016, 1507.634939773729911, 188.0954309116980028 ) ) ;
#21040 = CARTESIAN_POINT ( 'NONE',  ( -5.599233173528683771, 1387.285800435509827, 209.1218459616989946 ) ) ;
#21039 = CARTESIAN_POINT ( 'NONE',  ( 0.5624690339869999889, 1416.828040475229955, 190.4759594386979984 ) ) ;
#21041 = CARTESIAN_POINT ( 'NONE',  ( -9.808790059567231268, 1472.102509068790141, 211.8008741836299862 ) ) ;
#21042 = VERTEX_POINT ( 'NONE', #20389 ) ;
#21043 = CARTESIAN_POINT ( 'NONE',  ( -19.34729233231120205, 1486.470064436709890, 189.5887045964369975 ) ) ;
#21044 = CARTESIAN_POINT ( 'NONE',  ( -13.22667534600000216, 1508.519311693090003, 216.8816497979790086 ) ) ;
#21046 = CARTESIAN_POINT ( 'NONE',  ( 11.81135191919999983, 1436.410413307749877, 147.6956600043980075 ) ) ;
#21045 = B_SPLINE_CURVE_WITH_KNOTS ( 'NONE', 5,
 ( #81992, #31597, #55734, #12050, #73067, #54636 ),
 .UNSPECIFIED., .F., .F.,
 ( 6, 6 ),
 ( 434.2407011939999961, 439.4753079239999920 ),
 .UNSPECIFIED. ) ;
#21047 = VECTOR ( 'NONE', #6509, 1000.000000000000000 ) ;
#21048 = CARTESIAN_POINT ( 'NONE',  ( -17.27380198137636214, 1525.712835404586031, 236.6835154643348460 ) ) ;
#21049 = CARTESIAN_POINT ( 'NONE',  ( 30.60907494343232571, 1526.073429442291854, 216.5595792582588501 ) ) ;
#21050 = FACE_OUTER_BOUND ( 'NONE', #3545, .T. ) ;
#21051 = CARTESIAN_POINT ( 'NONE',  ( -3.261863598262784603, 1524.739915903631982, 241.7744910610305169 ) ) ;
#21052 = CARTESIAN_POINT ( 'NONE',  ( 20.80119636470000088, 1475.513060387329915, 213.8845752798079900 ) ) ;
#21053 = CARTESIAN_POINT ( 'NONE',  ( -7.315867787722543092, 1516.555258207057705, 210.7873785203714760 ) ) ;
#21054 = CARTESIAN_POINT ( 'NONE',  ( 3.210133688000829988, 1493.596834919620051, 219.7945351484260073 ) ) ;
#21055 = CARTESIAN_POINT ( 'NONE',  ( -5.221941033162339707, 1489.269461032029767, 185.8916498237339852 ) ) ;
#21057 = EDGE_CURVE ( 'NONE', #25318, #47913, #49254, .T. ) ;
#21056 = CARTESIAN_POINT ( 'NONE',  ( -14.55544240679570045, 1415.677402205800036, 205.6845489372280156 ) ) ;
#21058 = CARTESIAN_POINT ( 'NONE',  ( -109.1218884720000091, 1383.638097810560112, 311.0730448896949838 ) ) ;
#21059 = CARTESIAN_POINT ( 'NONE',  ( -6.896890933126118993E-05, 1408.913065613199933, 231.7784170915439859 ) ) ;
#21061 = EDGE_LOOP ( 'NONE', ( #79972, #1587, #40644, #52689 ) ) ;
#21060 = CARTESIAN_POINT ( 'NONE',  ( 22.24498329749999925, 1508.411266897830046, 192.4020607342980043 ) ) ;
#21062 = CYLINDRICAL_SURFACE ( 'NONE', #80178, 2.000000000000003553 ) ;
#21063 = CARTESIAN_POINT ( 'NONE',  ( 12.37943797690240189, 1512.150422497869840, 224.0155786243819875 ) ) ;
#21064 = ADVANCED_FACE ( 'NONE', ( #79783 ), #102418, .F. ) ;
#21065 = ORIENTED_EDGE ( 'NONE', *, *, #93835, .T. ) ;
#21066 = ORIENTED_EDGE ( 'NONE', *, *, #53596, .T. ) ;
#21067 = CARTESIAN_POINT ( 'NONE',  ( -110.0636332773229924, 1384.926148836659877, 296.9511394268049571 ) ) ;
#21068 = FACE_OUTER_BOUND ( 'NONE', #7180, .T. ) ;
#21069 = CARTESIAN_POINT ( 'NONE',  ( 7.868158389100000427, 1422.937290482379922, 214.1570520181289794 ) ) ;
#21071 = CARTESIAN_POINT ( 'NONE',  ( 1.874402367650000219E-09, 1463.532726170529941, 231.7907868339979984 ) ) ;
#21070 = CARTESIAN_POINT ( 'NONE',  ( 29.59289186111734793, 1419.279954201788541, 269.4665317194949239 ) ) ;
#21072 = CARTESIAN_POINT ( 'NONE',  ( -20.18744379279999990, 1494.501811925929815, 190.4612313790980238 ) ) ;
#21073 = AXIS2_PLACEMENT_3D ( 'NONE', #88161, #104948, #59781 ) ;
#21074 = CARTESIAN_POINT ( 'NONE',  ( -11.92399326099999968, 1433.494514533970005, 150.2018804083979830 ) ) ;
#21075 = CARTESIAN_POINT ( 'NONE',  ( 27.34966551919999844, 1509.645409999729964, 203.9598639501480193 ) ) ;
#21076 = CARTESIAN_POINT ( 'NONE',  ( -18.96987419410000086, 1486.105584072130114, 189.3878642699980048 ) ) ;
#21077 = FACE_OUTER_BOUND ( 'NONE', #35262, .T. ) ;
#21078 = AXIS2_PLACEMENT_3D ( 'NONE', #19138, #79096, #95873 ) ;
#21079 = CARTESIAN_POINT ( 'NONE',  ( -0.4151546846821905778, 1522.382868172863937, 244.9330574173806951 ) ) ;
#21080 = CARTESIAN_POINT ( 'NONE',  ( -0.2472019593338070087, 1515.155075545679892, 213.4489306029969953 ) ) ;
#21081 = CARTESIAN_POINT ( 'NONE',  ( -108.0661742336610018, 1378.913060387289988, 308.5496305239910271 ) ) ;
#21082 = CARTESIAN_POINT ( 'NONE',  ( -10.27310637450800002, 1479.785839561440071, 214.7842258919359892 ) ) ;
#21083 = CARTESIAN_POINT ( 'NONE',  ( -13.18094245060510517, 1509.496846870918034, 236.0820355107387627 ) ) ;
#21085 = ORIENTED_EDGE ( 'NONE', *, *, #22808, .F. ) ;
#21084 = CARTESIAN_POINT ( 'NONE',  ( 1.582871032461760074E-08, 1407.860659628199983, 263.2896717771570252 ) ) ;
#21086 = VERTEX_POINT ( 'NONE', #93110 ) ;
#21087 = CARTESIAN_POINT ( 'NONE',  ( -12.20494468169999891, 1503.566125598490089, 208.5052328696230006 ) ) ;
#21088 = AXIS2_PLACEMENT_3D ( 'NONE', #53109, #87246, #47865 ) ;
#21089 = CARTESIAN_POINT ( 'NONE',  ( -11.64556911059999855, 1484.153277220190148, 228.3908460861989909 ) ) ;
#21090 = CARTESIAN_POINT ( 'NONE',  ( -29.04152419889999948, 1466.259437530530022, 270.1335450958980005 ) ) ;
#21091 = CARTESIAN_POINT ( 'NONE',  ( -23.93572934907803784, 1435.909525931274629, 211.2608146398322333 ) ) ;
#21092 = CARTESIAN_POINT ( 'NONE',  ( -125.2268008667000174, 1376.302340817389904, 304.2218459572590064 ) ) ;
#21093 = FACE_OUTER_BOUND ( 'NONE', #87540, .T. ) ;
#21094 = CARTESIAN_POINT ( 'NONE',  ( 4.327218846664220742, 1515.149950449760127, 209.5076553614100021 ) ) ;
#21095 = CARTESIAN_POINT ( 'NONE',  ( -12.81872062859999950, 1420.998869512129886, 230.6915806954980042 ) ) ;
#21096 = CARTESIAN_POINT ( 'NONE',  ( 20.86040077215431410, 1508.959081887785487, 227.6602567278162041 ) ) ;
#21097 = CARTESIAN_POINT ( 'NONE',  ( -1.185300654861193514, 1484.701227333132692, 182.2327694872268182 ) ) ;
#21098 = CARTESIAN_POINT ( 'NONE',  ( 8.476942927298200203, 1362.523913559719858, 210.6218459616991936 ) ) ;
#21099 = CARTESIAN_POINT ( 'NONE',  ( -45.70040227590190085, 1436.740216172639975, 268.5066267783719809 ) ) ;
#21100 = ORIENTED_EDGE ( 'NONE', *, *, #41168, .F. ) ;
#21101 = CARTESIAN_POINT ( 'NONE',  ( -3.532157406807699740, 1490.686494827730030, 181.6769642933810189 ) ) ;
#21102 = ORIENTED_EDGE ( 'NONE', *, *, #61460, .F. ) ;
#21103 = EDGE_LOOP ( 'NONE', ( #23897, #57997, #56545, #2625 ) ) ;
#21104 = CARTESIAN_POINT ( 'NONE',  ( -2.864043456445000135, 1516.811292230880099, 211.4208600009669965 ) ) ;
#21105 = CARTESIAN_POINT ( 'NONE',  ( -9.191661361731490842, 1447.246705968339938, 212.1312239747880142 ) ) ;
#21106 = VECTOR ( 'NONE', #574, 1000.000000000000114 ) ;
#21107 = CARTESIAN_POINT ( 'NONE',  ( -21.92450687779999896, 1509.678681038230025, 190.3751805934979870 ) ) ;
#21108 = DIRECTION ( 'NONE',  ( -0.2857341017153708362, -0.9583089392864680978, -7.447054303646096154E-07 ) ) ;
#21109 = CARTESIAN_POINT ( 'NONE',  ( -16.45911293875139592, 1470.466665006630137, 228.6107017031530120 ) ) ;
#21110 = ORIENTED_EDGE ( 'NONE', *, *, #55628, .F. ) ;
#21111 = CARTESIAN_POINT ( 'NONE',  ( 6.941727252324999320, 1516.882217593000178, 201.7906628411569727 ) ) ;
#21112 = CARTESIAN_POINT ( 'NONE',  ( 18.46505084572267563, 1509.557874171173125, 187.1463136620376702 ) ) ;
#21113 = CARTESIAN_POINT ( 'NONE',  ( -5.144873395449999443, 1502.885538352589947, 229.8910404859989853 ) ) ;
#21114 = ORIENTED_EDGE ( 'NONE', *, *, #36740, .T. ) ;
#21115 = CARTESIAN_POINT ( 'NONE',  ( -8.488567187765550415, 1409.798321788380008, 270.3692809364429763 ) ) ;
#21116 = CARTESIAN_POINT ( 'NONE',  ( -33.91369110859999836, 1435.681798638700002, 135.0664268289980043 ) ) ;
#21117 = CARTESIAN_POINT ( 'NONE',  ( 8.822677033039550309, 1435.308442571839805, 207.3766048290129902 ) ) ;
#21119 = ORIENTED_EDGE ( 'NONE', *, *, #44217, .T. ) ;
#21118 = CARTESIAN_POINT ( 'NONE',  ( -7.999735567014255366, 1364.908477751830560, 209.6218459617148824 ) ) ;
#21120 = ORIENTED_EDGE ( 'NONE', *, *, #125, .T. ) ;
#21121 = CARTESIAN_POINT ( 'NONE',  ( 42.04647649369601936, 1454.209662175047924, 269.0745616169903656 ) ) ;
#21122 = CARTESIAN_POINT ( 'NONE',  ( -1.419179629244010199, 1467.807880198409975, 220.1457629506999751 ) ) ;
#21123 = CARTESIAN_POINT ( 'NONE',  ( -13.87677329403120119, 1436.230442017350015, 150.3050677568869844 ) ) ;
#21124 = CARTESIAN_POINT ( 'NONE',  ( -0.03489894090345890126, 1409.380919406509975, 185.4002601856399792 ) ) ;
#21125 = LINE ( 'NONE', #3283, #80554 ) ;
#21126 = CARTESIAN_POINT ( 'NONE',  ( -18.72553219700000326, 1435.775956364280091, 225.5898836715979883 ) ) ;
#21127 = CARTESIAN_POINT ( 'NONE',  ( 15.79272951203170017, 1474.038596115399969, 268.9599971491709880 ) ) ;
#21128 = CARTESIAN_POINT ( 'NONE',  ( -1.500739301586951013, 1467.017219971860868, 235.3803771181077593 ) ) ;
#21129 = CARTESIAN_POINT ( 'NONE',  ( 7.158636770289999340, 1447.499260772210164, 185.4013549890980244 ) ) ;
#21130 = CARTESIAN_POINT ( 'NONE',  ( 1.701729820345000199, 1516.969638403840008, 206.2395199527169893 ) ) ;
#21131 = VERTEX_POINT ( 'NONE', #92555 ) ;
#21132 = CARTESIAN_POINT ( 'NONE',  ( -38.81202642568430150, 1450.612734564189850, 135.0584858587309895 ) ) ;
#21133 = CARTESIAN_POINT ( 'NONE',  ( -12.93261306534080113, 1416.826860677879949, 196.5036138660090046 ) ) ;
#21134 = EDGE_LOOP ( 'NONE', ( #102173, #18097, #61819, #72302, #33327 ) ) ;
#21135 = CARTESIAN_POINT ( 'NONE',  ( -4.367937192439999450, 1447.898255911189835, 190.6350925615990093 ) ) ;
#21136 = CARTESIAN_POINT ( 'NONE',  ( -5.102340803919999779, 1483.010473641589897, 199.7820758705289848 ) ) ;
#21137 = CARTESIAN_POINT ( 'NONE',  ( 14.23393746390000025, 1416.021639799829927, 196.8145123778979837 ) ) ;
#21138 = CARTESIAN_POINT ( 'NONE',  ( -9.109477210328888575, 1384.590310583010250, 199.9607628076590231 ) ) ;
#21139 = CARTESIAN_POINT ( 'NONE',  ( 19.18632316300000085, 1409.583061558729923, 197.9438956507979981 ) ) ;
#21140 = CARTESIAN_POINT ( 'NONE',  ( 22.74352444629999681, 1409.874439160429802, 207.7226808069280253 ) ) ;
#21141 = CARTESIAN_POINT ( 'NONE',  ( -23.61227025210000008, 1435.322036687620084, 137.2858276859979867 ) ) ;
#21142 = CARTESIAN_POINT ( 'NONE',  ( -24.45428651019999933, 1432.411055651390143, 210.5059752880879955 ) ) ;
#21143 = CARTESIAN_POINT ( 'NONE',  ( 0.3740290774567820442, 1452.976564944560096, 183.2744728122640083 ) ) ;
#21144 = CYLINDRICAL_SURFACE ( 'NONE', #45970, 1.999999999999996669 ) ;
#21145 = AXIS2_PLACEMENT_3D ( 'NONE', #62027, #27846, #19425 ) ;
#21146 = CARTESIAN_POINT ( 'NONE',  ( -0.7376675409259989546, 1517.104497701820037, 214.9086937099069985 ) ) ;
#21147 = VERTEX_POINT ( 'NONE', #23143 ) ;
#21148 = CARTESIAN_POINT ( 'NONE',  ( 7.708852660943830593, 1516.527466478090219, 206.9210818302649955 ) ) ;
#21149 = B_SPLINE_SURFACE_WITH_KNOTS ( 'NONE', 5, 5, ( 
 ( #100217, #82856, #6145, #74486, #44184, #27365 ),
 ( #18390, #104627, #96230, #103511, #2750, #53141 ),
 ( #60438, #62106, #87279, #43628, #36315, #78324 ),
 ( #45298, #51466, #27924, #94556, #36870, #79438 ),
 ( #8898, #19507, #17829, #102949, #537, #53712 ),
 ( #77776, #26814, #70512, #9463, #87850, #1636 ),
 ( #52588, #1088, #71064, #35773, #35214, #69400 ),
 ( #61002, #62671, #95128, #28478, #17275, #18946 ),
 ( #26250, #10574, #86721, #86170, #85598, #43076 ),
 ( #69956, #68845, #10014, #61547, #44745, #104070 ),
 ( #105186, #77236, #95678, #11138, #78895, #2201 ),
 ( #34661, #52034, #72163, #3854, #106817, #98968 ),
 ( #72694, #88382, #22242, #29033, #71629, #79981 ),
 ( #37981, #46406, #106280, #4916, #88925, #39055 ),
 ( #13850, #21139, #12211, #48034, #12775, #80539 ),
 ( #29566, #63750, #31222, #97864, #107929, #96792 ),
 ( #20062, #105749, #98423, #55346, #54793, #54256 ),
 ( #107378, #38515, #37431, #89480, #30108, #90019 ),
 ( #21695, #82172, #11672, #46952, #56440, #81072 ),
 ( #13296, #4387, #64303, #55901, #47489, #81612 ),
 ( #30673, #90571, #45848, #5472, #73235, #3300 ) ),
 .UNSPECIFIED., .F., .F., .F.,
 ( 6, 3, 3, 3, 3, 3, 6 ),
 ( 6, 6 ),
 ( 29.50806686130000145, 31.51384161189999844, 32.22913687700000196, 33.93149951750000071, 35.63386215799999945, 39.03858743909999873, 48.56910801690000312 ),
 ( 0.000000000000000000, 1.468540379180000022 ),
 .UNSPECIFIED. ) ;
#21150 = DIRECTION ( 'NONE',  ( 0.000000000000000000, -0.07083107041561081951, -0.9974883254774358221 ) ) ;
#21151 = CIRCLE ( 'NONE', #57012, 0.9999999999999930056 ) ;
#21152 = DIRECTION ( 'NONE',  ( 0.000000000000000000, 0.000000000000000000, -1.000000000000000000 ) ) ;
#21153 = CIRCLE ( 'NONE', #98072, 2.000012941106792841 ) ;
#21154 = CARTESIAN_POINT ( 'NONE',  ( -5.553848058839999879, 1423.191816860230119, 91.03168606369779070 ) ) ;
#21155 = CARTESIAN_POINT ( 'NONE',  ( -40.14605221587299155, 1445.134064018490108, 136.9416851659559882 ) ) ;
#21156 = CARTESIAN_POINT ( 'NONE',  ( 11.60004869885203682, 1425.984133098859502, 137.6624196891229133 ) ) ;
#21157 = CARTESIAN_POINT ( 'NONE',  ( 2.108904356780865186, 1417.396421507168725, 233.2477812154150172 ) ) ;
#21158 = CARTESIAN_POINT ( 'NONE',  ( -1.929425373146870015, 1464.862440756950264, 183.7962778897980058 ) ) ;
#21159 = CARTESIAN_POINT ( 'NONE',  ( -12.31544236599309983, 1378.361828460810102, 209.6885106622719945 ) ) ;
#21160 = CARTESIAN_POINT ( 'NONE',  ( -10.16997697100000053, 1474.408914113430001, 269.6186555620979561 ) ) ;
#21161 = CARTESIAN_POINT ( 'NONE',  ( 29.33985996377240113, 1440.913060386940060, 236.1580507230389969 ) ) ;
#21162 = CARTESIAN_POINT ( 'NONE',  ( 0.5890887500919901321, 1526.382868172863937, 243.2762031678882977 ) ) ;
#21163 = CARTESIAN_POINT ( 'NONE',  ( 11.23090178780859993, 1499.222069974919805, 203.1659750294479920 ) ) ;
#21164 = ORIENTED_EDGE ( 'NONE', *, *, #109564, .T. ) ;
#21165 = CARTESIAN_POINT ( 'NONE',  ( 11.76012779522459972, 1479.338680739629808, 208.6262329665489972 ) ) ;
#21166 = LINE ( 'NONE', #55374, #40754 ) ;
#21167 = CARTESIAN_POINT ( 'NONE',  ( 1.834068947563254337, 1397.968134176382819, 196.2250787140935699 ) ) ;
#21168 = CARTESIAN_POINT ( 'NONE',  ( 2.894887617429999782, 1490.918242441229950, 235.2239209075980000 ) ) ;
#21169 = AXIS2_PLACEMENT_3D ( 'NONE', #86669, #27317, #95628 ) ;
#21170 = DIRECTION ( 'NONE',  ( 0.000000000000000000, 1.000000000000000000, 0.000000000000000000 ) ) ;
#21171 = CARTESIAN_POINT ( 'NONE',  ( -12.44137076039999990, 1509.176489603729806, 234.5038223836979796 ) ) ;
#21172 = CARTESIAN_POINT ( 'NONE',  ( -19.11991078017920032, 1383.854501207500107, 220.4169213401859793 ) ) ;
#21173 = CARTESIAN_POINT ( 'NONE',  ( -2.487923653944299929, 1509.038644359520049, 204.6345969248399967 ) ) ;
#21174 = CARTESIAN_POINT ( 'NONE',  ( 2.499942005323459782, 1419.859829899919987, 115.5959393205330059 ) ) ;
#21175 = CARTESIAN_POINT ( 'NONE',  ( 2.684660662710000256, 1464.593469353430010, 236.4393482303979965 ) ) ;
#21177 = ORIENTED_EDGE ( 'NONE', *, *, #104951, .F. ) ;
#21176 = FACE_OUTER_BOUND ( 'NONE', #96653, .T. ) ;
#21178 = CARTESIAN_POINT ( 'NONE',  ( -1.406481360810000192, 1450.686779281020108, 182.3753173715980154 ) ) ;
#21179 = CARTESIAN_POINT ( 'NONE',  ( -24.66946762459999931, 1380.257393238360009, 206.6025861486290012 ) ) ;
#21180 = CARTESIAN_POINT ( 'NONE',  ( -3.453907602370000163, 1475.036073752090033, 198.6389954596989753 ) ) ;
#21181 = ADVANCED_FACE ( 'NONE', ( #84158 ), #99849, .F. ) ;
#21183 = ORIENTED_EDGE ( 'NONE', *, *, #15912, .F. ) ;
#21182 = CYLINDRICAL_SURFACE ( 'NONE', #62652, 0.9999999999999970024 ) ;
#21184 = CARTESIAN_POINT ( 'NONE',  ( -18.65942656951699874, 1468.219847912240084, 201.0822107266409944 ) ) ;
#21185 = VERTEX_POINT ( 'NONE', #25339 ) ;
#21186 = CARTESIAN_POINT ( 'NONE',  ( -9.095095392940001133, 1388.475365584439942, 217.6269457225290012 ) ) ;
#21187 = CARTESIAN_POINT ( 'NONE',  ( 15.41142278176256575, 1416.181292664740113, 209.1057902910335997 ) ) ;
#21188 = FACE_OUTER_BOUND ( 'NONE', #41398, .T. ) ;
#21189 = CARTESIAN_POINT ( 'NONE',  ( -11.60004869885204215, 1426.273944179774844, 138.2686100621498326 ) ) ;
#21190 = CARTESIAN_POINT ( 'NONE',  ( -30.25425994617014780, 1522.382868172863937, 199.2916410102373277 ) ) ;
#21191 = CARTESIAN_POINT ( 'NONE',  ( -10.14235463135029924, 1472.524663116719921, 207.2163364872419891 ) ) ;
#21192 = CARTESIAN_POINT ( 'NONE',  ( 4.580542335331530879, 1409.073016450339992, 194.8569092263689981 ) ) ;
#21193 = DIRECTION ( 'NONE',  ( 0.000000000000000000, -1.000000000000000000, 0.000000000000000000 ) ) ;
#21194 = CARTESIAN_POINT ( 'NONE',  ( -91.93155929093219925, 1385.198662290420089, 293.6444189235990052 ) ) ;
#21195 = DIRECTION ( 'NONE',  ( -1.000000000000000000, 0.000000000000000000, 0.000000000000000000 ) ) ;
#21196 = CARTESIAN_POINT ( 'NONE',  ( 20.71343476517534299, 1512.187213306747481, 238.3377464195763764 ) ) ;
#21197 = B_SPLINE_CURVE_WITH_KNOTS ( 'NONE', 3,
 ( #69602, #95325, #37069, #96991, #52782, #86918, #10210, #56633, #99706, #72885, #82921, #23561, #30312, #38709, #65593, #39825, #47680, #48799, #21880, #66160, #80731, #91327, #6213, #5681, #12412, #108677, #81260, #14050, #13490, #107574, #64501, #106477, #40364, #100281, #89124, #38167, #30860 ),
 .UNSPECIFIED., .F., .F.,
 ( 4, 3, 3, 3, 3, 3, 3, 3, 3, 3, 3, 3, 4 ),
 ( -1.999999848858570184, -1.897891335478260055, -1.728761196501279906, -1.557452151978439892, -1.384905003028850112, -1.210695231704240094, -1.035838572815900083, -0.8607549783656509579, -0.6858798835383781434, -0.5121999524719260677, -0.3398111961833858441, -0.1690102497754839561, -5.802412736954920547E-06 ),
 .UNSPECIFIED. ) ;
#21198 = CARTESIAN_POINT ( 'NONE',  ( -2.560277166941169913, 1449.672157588639948, 183.8693981670420214 ) ) ;
#21199 = VERTEX_POINT ( 'NONE', #32113 ) ;
#21200 = VERTEX_POINT ( 'NONE', #48381 ) ;
#21201 = CARTESIAN_POINT ( 'NONE',  ( 20.37381179411493548, 1524.397344074318880, 237.9604625470743997 ) ) ;
#21202 = CARTESIAN_POINT ( 'NONE',  ( -18.74729292449999818, 1442.199705176290081, 209.1218459616989946 ) ) ;
#21203 = CARTESIAN_POINT ( 'NONE',  ( 2.196337318485120260, 1497.056153613870038, 196.9180676716810012 ) ) ;
#21204 = CARTESIAN_POINT ( 'NONE',  ( 12.55930903091550022, 1420.665439290649829, 201.1166257793219927 ) ) ;
#21205 = CARTESIAN_POINT ( 'NONE',  ( -20.39295167552050003, 1501.158379912629925, 190.5839871636399891 ) ) ;
#21206 = CARTESIAN_POINT ( 'NONE',  ( -5.393559028770000581E-12, 1395.913060387330006, 220.1216245191979795 ) ) ;
#21207 = CARTESIAN_POINT ( 'NONE',  ( -109.2202009529999884, 1384.950645967480114, 311.2644681782590510 ) ) ;
#21208 = CARTESIAN_POINT ( 'NONE',  ( -1.184997839870000069, 1455.069883079229839, 183.4791223000979983 ) ) ;
#21209 = CARTESIAN_POINT ( 'NONE',  ( -10.90461552211807295, 1364.061143884626290, 207.6218459616987673 ) ) ;
#21210 = CARTESIAN_POINT ( 'NONE',  ( -26.34474851411561147, 1436.712219889005382, 136.8403030806463505 ) ) ;
#21211 = CARTESIAN_POINT ( 'NONE',  ( 2.738357492517908387, 1525.795403621571040, 177.3070692402450845 ) ) ;
#21212 = ADVANCED_FACE ( 'NONE', ( #49481 ), #88219, .T. ) ;
#21213 = CARTESIAN_POINT ( 'NONE',  ( 6.548200587644999793, 1516.632821972880038, 207.9912384682270101 ) ) ;
#21214 = CARTESIAN_POINT ( 'NONE',  ( 11.59211330538789930, 1433.842074355000022, 151.2028293458270127 ) ) ;
#21215 = VECTOR ( 'NONE', #28420, 1000.000000000000000 ) ;
#21216 = CARTESIAN_POINT ( 'NONE',  ( -13.13217473943669944, 1436.055352265540023, 150.6849122874139937 ) ) ;
#21217 = DIRECTION ( 'NONE',  ( 1.000000000000000000, 0.000000000000000000, 0.000000000000000000 ) ) ;
#21218 = CARTESIAN_POINT ( 'NONE',  ( 1.101790807069999989, 1496.828157016689829, 196.7632638577989894 ) ) ;
#21220 = DIRECTION ( 'NONE',  ( 0.000000000000000000, 0.000000000000000000, -1.000000000000000000 ) ) ;
#21219 = AXIS2_PLACEMENT_3D ( 'NONE', #75978, #23898, #74354 ) ;
#21221 = ORIENTED_EDGE ( 'NONE', *, *, #9062, .F. ) ;
#21222 = AXIS2_PLACEMENT_3D ( 'NONE', #16598, #102825, #84927 ) ;
#21223 = CARTESIAN_POINT ( 'NONE',  ( 5.301749018989998952, 1413.741945239130018, 248.5896189552980218 ) ) ;
#21224 = CARTESIAN_POINT ( 'NONE',  ( -24.64286055450000035, 1488.680273902429917, 199.5172922023679973 ) ) ;
#21226 = CARTESIAN_POINT ( 'NONE',  ( 2.956412232989999457E-14, 1420.418457356630142, 243.9198229339980060 ) ) ;
#21225 = CARTESIAN_POINT ( 'NONE',  ( -10.41164713266690001, 1425.393357077480005, 96.73048425825258789 ) ) ;
#21227 =( BOUNDED_CURVE ( )  B_SPLINE_CURVE ( 3, ( #20612, #31238, #82749, #107391 ),
 .UNSPECIFIED., .F., .F. ) 
 B_SPLINE_CURVE_WITH_KNOTS ( ( 4, 4 ),
 ( 3.141592653589793116, 4.712388980384689674 ),
 .UNSPECIFIED. ) 
 CURVE ( )  GEOMETRIC_REPRESENTATION_ITEM ( )  RATIONAL_B_SPLINE_CURVE ( ( 1.000000000000000000, 0.8047378541243649375, 0.8047378541243649375, 1.000000000000000000 ) ) 
 REPRESENTATION_ITEM ( '' )  );
#21228 = CARTESIAN_POINT ( 'NONE',  ( 18.72196290327717705, 1507.117986391379645, 196.2613482712523592 ) ) ;
#21229 = CARTESIAN_POINT ( 'NONE',  ( 1.630039620769999944E-09, 1416.130848190830193, 240.4142140047979694 ) ) ;
#21230 = CARTESIAN_POINT ( 'NONE',  ( -0.09768190207400140324, 1486.875687893489840, 220.0842578668990086 ) ) ;
#21231 = CARTESIAN_POINT ( 'NONE',  ( 0.8007374150823964865, 1415.525414496541998, 233.2555237395259269 ) ) ;
#21232 = CARTESIAN_POINT ( 'NONE',  ( 29.25358229339999738, 1451.890933296829871, 135.2860531028979949 ) ) ;
#21233 = VERTEX_POINT ( 'NONE', #25894 ) ;
#21234 = CARTESIAN_POINT ( 'NONE',  ( -0.06016863597635770111, 1397.283821687630052, 196.1836521277020040 ) ) ;
#21235 = CARTESIAN_POINT ( 'NONE',  ( 13.95549232207893553, 1513.969110081093959, 225.7819657676807594 ) ) ;
#21236 = CARTESIAN_POINT ( 'NONE',  ( -4.326079330693803016, 1515.193466806617153, 206.7917118350173382 ) ) ;
#21237 = VERTEX_POINT ( 'NONE', #42725 ) ;
#21238 = ORIENTED_EDGE ( 'NONE', *, *, #45772, .T. ) ;
#21239 = CARTESIAN_POINT ( 'NONE',  ( 10.53595400140370053, 1452.843899432660010, 210.2517208858830031 ) ) ;
#21240 = CARTESIAN_POINT ( 'NONE',  ( -24.10461029974740299, 1411.115259933990046, 208.6981664729640045 ) ) ;
#21241 = ORIENTED_EDGE ( 'NONE', *, *, #5496, .T. ) ;
#21242 = CARTESIAN_POINT ( 'NONE',  ( -2.762222941174190094, 1441.249766939880146, 203.6130042841640204 ) ) ;
#21243 = DIRECTION ( 'NONE',  ( 0.1362866687051670078, -0.4503100534970719271, 0.8824096552354309120 ) ) ;
#21244 = CARTESIAN_POINT ( 'NONE',  ( -7.416235415360000083, 1489.056178334129982, 234.6541755130980107 ) ) ;
#21245 = CARTESIAN_POINT ( 'NONE',  ( 17.04790460296295507, 1526.208281990540172, 235.6077665793653466 ) ) ;
#21246 = ORIENTED_EDGE ( 'NONE', *, *, #4050, .T. ) ;
#21247 = EDGE_CURVE ( 'NONE', #44154, #3217, #43286, .T. ) ;
#21248 = CARTESIAN_POINT ( 'NONE',  ( 46.02990061730259441, 1440.912967656690171, 268.4960838911439964 ) ) ;
#21249 = EDGE_CURVE ( 'NONE', #93813, #60698, #101541, .T. ) ;
#21250 = CARTESIAN_POINT ( 'NONE',  ( -31.23437356469425907, 1523.382868172864164, 221.8968241038847964 ) ) ;
#21251 = CARTESIAN_POINT ( 'NONE',  ( 0.1168360841530000083, 1420.456612005029911, 182.7029863163980110 ) ) ;
#21252 = CARTESIAN_POINT ( 'NONE',  ( -5.782749439735000330, 1516.858301627840092, 203.3453548368569841 ) ) ;
#21253 = ORIENTED_EDGE ( 'NONE', *, *, #54007, .T. ) ;
#21255 = EDGE_CURVE ( 'NONE', #49156, #5142, #67606, .T. ) ;
#21254 = CARTESIAN_POINT ( 'NONE',  ( 8.824912719755909407, 1482.390745019529959, 216.9842546517499784 ) ) ;
#21256 = CARTESIAN_POINT ( 'NONE',  ( 13.05663714242001028, 1442.990000998531968, 187.2968644710537660 ) ) ;
#21257 = EDGE_LOOP ( 'NONE', ( #93173, #2329, #65321, #38487, #94984, #66478, #14920, #7957 ) ) ;
#21258 = ORIENTED_EDGE ( 'NONE', *, *, #245, .F. ) ;
#21259 = CARTESIAN_POINT ( 'NONE',  ( -11.88114669040890092, 1481.846449482240132, 209.1712150661669796 ) ) ;
#21260 = ADVANCED_FACE ( 'NONE', ( #85254 ), #71261, .T. ) ;
#21261 = DIRECTION ( 'NONE',  ( -0.7071067811865475727, 0.000000000000000000, 0.7071067811865475727 ) ) ;
#21262 = CARTESIAN_POINT ( 'NONE',  ( -18.33789049558490092, 1409.553433634309840, 198.1058259467170046 ) ) ;
#21263 = B_SPLINE_CURVE_WITH_KNOTS ( 'NONE', 5,
 ( #77803, #76691, #59366, #3, #86193, #26275 ),
 .UNSPECIFIED., .F., .F.,
 ( 6, 6 ),
 ( 0.000000000000000000, 1.000000000000000000 ),
 .UNSPECIFIED. ) ;
#21264 = ADVANCED_FACE ( 'NONE', ( #89135 ), #76534, .F. ) ;
#21265 = CARTESIAN_POINT ( 'NONE',  ( -3.048199684790729780, 1468.133964442819888, 219.8853629577970139 ) ) ;
#21266 = DIRECTION ( 'NONE',  ( -0.1115146105487929418, 0.9937625046796735306, 0.0007588984999193657075 ) ) ;
#21267 = CARTESIAN_POINT ( 'NONE',  ( 8.315094184529998600, 1421.392059295079889, 196.2232414242990046 ) ) ;
#21268 = DIRECTION ( 'NONE',  ( 0.9942586961433758086, 0.000000000000000000, 0.1070030146457303932 ) ) ;
#21269 = CARTESIAN_POINT ( 'NONE',  ( -108.3767226235554375, 1381.034261239543866, 298.1262863712069020 ) ) ;
#21270 = CARTESIAN_POINT ( 'NONE',  ( 3.827327205999999649, 1409.546157813730133, 146.1721969590979882 ) ) ;
#21271 = CARTESIAN_POINT ( 'NONE',  ( 0.03003581927826226919, 1409.173052036745048, 232.6080437499834943 ) ) ;
#21272 = ADVANCED_FACE ( 'NONE', ( #63961 ), #96440, .F. ) ;
#21274 = CARTESIAN_POINT ( 'NONE',  ( -106.4020727818770098, 1391.913060387289988, 304.2008118092670088 ) ) ;
#21273 = CARTESIAN_POINT ( 'NONE',  ( -19.06723915664710134, 1485.490521620860136, 189.6150037022410118 ) ) ;
#21275 = CARTESIAN_POINT ( 'NONE',  ( 11.42187775320380005, 1422.318575770460029, 207.1307412838170023 ) ) ;
#21276 = CARTESIAN_POINT ( 'NONE',  ( -25.07152577354069933, 1509.629181063510032, 222.8076647697269834 ) ) ;
#21277 = B_SPLINE_CURVE_WITH_KNOTS ( 'NONE', 5,
 ( #38835, #31541, #80860, #91461, #57335, #55131 ),
 .UNSPECIFIED., .F., .F.,
 ( 6, 6 ),
 ( -2.000000000000000000, 0.000000000000000000 ),
 .UNSPECIFIED. ) ;
#21278 = CARTESIAN_POINT ( 'NONE',  ( -6.527830581335000382, 1512.220794350740107, 201.3447709183070060 ) ) ;
#21279 = ORIENTED_EDGE ( 'NONE', *, *, #77433, .T. ) ;
#21280 = CARTESIAN_POINT ( 'NONE',  ( 23.42675388089999799, 1438.250513043230058, 234.3916895697979612 ) ) ;
#21281 = DIRECTION ( 'NONE',  ( -1.000000000000000000, 0.000000000000000000, 0.000000000000000000 ) ) ;
#21282 = CARTESIAN_POINT ( 'NONE',  ( -91.22333267815579916, 1384.966695060079928, 309.0954049842840163 ) ) ;
#21283 = B_SPLINE_SURFACE_WITH_KNOTS ( 'NONE', 5, 5, ( 
 ( #45782, #3230, #44669, #37357, #103997, #3781 ),
 ( #27294, #97797, #21075, #12145, #71558, #19431 ),
 ( #89410, #28961, #63150, #78810, #80466, #97250 ),
 ( #37913, #104556, #53068, #20526, #87205, #29491 ),
 ( #63686, #12698, #35691, #95602, #69881, #18870 ),
 ( #53632, #2125, #70437, #27851, #45226, #62032 ) ),
 .UNSPECIFIED., .F., .F., .F.,
 ( 6, 6 ),
 ( 6, 6 ),
 ( 57.19174229819999766, 70.68201800039999227 ),
 ( 0.000000000000000000, 2.000000000000000000 ),
 .UNSPECIFIED. ) ;
#21284 = CARTESIAN_POINT ( 'NONE',  ( -9.398774730970000491, 1388.838992215879898, 201.0120684272889946 ) ) ;
#21285 = CARTESIAN_POINT ( 'NONE',  ( -15.47916639359999991, 1416.003150712520210, 210.9846457611390065 ) ) ;
#21286 = EDGE_CURVE ( 'NONE', #101260, #81031, #88056, .T. ) ;
#21288 = ORIENTED_EDGE ( 'NONE', *, *, #66459, .T. ) ;
#21287 = CARTESIAN_POINT ( 'NONE',  ( -15.88906974165360175, 1420.257646009350083, 209.8690693256239967 ) ) ;
#21289 = CARTESIAN_POINT ( 'NONE',  ( 3.959152859930000101, 1428.396642669490120, 216.3690266601789745 ) ) ;
#21290 = CYLINDRICAL_SURFACE ( 'NONE', #19192, 0.9999999999999569233 ) ;
#21291 = AXIS2_PLACEMENT_3D ( 'NONE', #54, #605, #34735 ) ;
#21292 = CARTESIAN_POINT ( 'NONE',  ( -13.79590941699999895, 1416.844618638129987, 221.9094009297979824 ) ) ;
#21293 = CARTESIAN_POINT ( 'NONE',  ( -1.860819933241510071, 1429.530525759420243, 199.9260310902689923 ) ) ;
#21294 = CARTESIAN_POINT ( 'NONE',  ( 15.37680647863500205, 1514.414736986979960, 224.4895214034669948 ) ) ;
#21295 = CARTESIAN_POINT ( 'NONE',  ( 4.401912331127000755, 1370.456889401766148, 209.4259416260188686 ) ) ;
#21296 = EDGE_CURVE ( 'NONE', #65505, #26062, #71835, .T. ) ;
#21297 = FACE_OUTER_BOUND ( 'NONE', #63726, .T. ) ;
#21298 = CARTESIAN_POINT ( 'NONE',  ( -13.46280551501950029, 1426.665735440540175, 222.2126077582630046 ) ) ;
#21299 = EDGE_CURVE ( 'NONE', #82900, #83651, #56091, .T. ) ;
#21300 = CARTESIAN_POINT ( 'NONE',  ( 12.71163532969999821, 1422.101025195029933, 229.2301305095980126 ) ) ;
#21301 = CARTESIAN_POINT ( 'NONE',  ( -0.5697989934050000649, 1450.893162568020216, 169.5117309619979835 ) ) ;
#21302 = CARTESIAN_POINT ( 'NONE',  ( -0.7579263249019989601, 1516.927039499179955, 207.4176752179770347 ) ) ;
#21303 = CARTESIAN_POINT ( 'NONE',  ( 41.54683551029999222, 1425.087414133530046, 267.1293096718979427 ) ) ;
#21304 = CARTESIAN_POINT ( 'NONE',  ( -18.40570622650000132, 1410.918580325929952, 224.0732781207979940 ) ) ;
#21305 = CARTESIAN_POINT ( 'NONE',  ( 17.03727604480000224, 1436.327040906540105, 148.1886016197979927 ) ) ;
#21306 = VECTOR ( 'NONE', #96786, 1000.000000000000000 ) ;
#21307 = EDGE_CURVE ( 'NONE', #47741, #104308, #15676, .T. ) ;
#21308 = DIRECTION ( 'NONE',  ( 0.000000000000000000, 1.000000000000000000, -0.000000000000000000 ) ) ;
#21309 = CARTESIAN_POINT ( 'NONE',  ( -17.00536272201560095, 1410.873511664369744, 191.9510081054149850 ) ) ;
#21310 = AXIS2_PLACEMENT_3D ( 'NONE', #89915, #12109, #46302 ) ;
#21311 = CARTESIAN_POINT ( 'NONE',  ( 12.27023112300000030, 1416.839692131129823, 223.5796784315980119 ) ) ;
#21312 = CARTESIAN_POINT ( 'NONE',  ( 13.15726396704670087, 1415.954755714380099, 198.0473975409559841 ) ) ;
#21313 = CARTESIAN_POINT ( 'NONE',  ( -37.80877602953309946, 1438.319709222639858, 136.5786655222570118 ) ) ;
#21314 = CARTESIAN_POINT ( 'NONE',  ( 0.2166443802809689678, 1453.632411855340024, 183.2262637060080124 ) ) ;
#21315 = CARTESIAN_POINT ( 'NONE',  ( -13.68698573120000006, 1409.391020461129983, 216.8549264454580054 ) ) ;
#21316 = CARTESIAN_POINT ( 'NONE',  ( -12.95840179510000034, 1416.218047894730262, 196.6656609298980243 ) ) ;
#21317 = CARTESIAN_POINT ( 'NONE',  ( 20.71343476517376558, 1522.906561336852974, 179.9059455038184581 ) ) ;
#21318 = CARTESIAN_POINT ( 'NONE',  ( -0.07406262508839699110, 1484.296809990774818, 198.4210634843702508 ) ) ;
#21319 = CARTESIAN_POINT ( 'NONE',  ( 12.06118834549999974, 1433.903448631609990, 147.9454112030979900 ) ) ;
#21320 = CARTESIAN_POINT ( 'NONE',  ( -38.70428745504600698, 1437.478004126309997, 134.0999999972650016 ) ) ;
#21321 = CARTESIAN_POINT ( 'NONE',  ( 11.79755445260000002, 1442.026836458709795, 187.8249092859979896 ) ) ;
#21322 = VERTEX_POINT ( 'NONE', #12420 ) ;
#21323 = CARTESIAN_POINT ( 'NONE',  ( 4.049945658389999537, 1478.539621255289831, 199.3912200899090124 ) ) ;
#21324 = CARTESIAN_POINT ( 'NONE',  ( 39.60771322839999442, 1439.514900260280001, 136.6564050689979979 ) ) ;
#21325 = CARTESIAN_POINT ( 'NONE',  ( 1.823067188510389982E-15, 1517.051704408389924, 209.1218459616989946 ) ) ;
#21326 = CARTESIAN_POINT ( 'NONE',  ( 20.92767404034517753, 1512.187213306747481, 235.3888156262294444 ) ) ;
#21327 = CARTESIAN_POINT ( 'NONE',  ( -13.86457764730300113, 1451.730262176210090, 194.4398952447820079 ) ) ;
#21328 = CARTESIAN_POINT ( 'NONE',  ( 1.090037377353519974E-11, 1406.777728848529932, 269.6500679732980075 ) ) ;
#21330 = AXIS2_PLACEMENT_3D ( 'NONE', #103227, #42246, #16996 ) ;
#21329 = DIRECTION ( 'NONE',  ( 1.755985294532469921E-16, -1.000000000000000000, 1.338183447452831989E-16 ) ) ;
#21331 = CARTESIAN_POINT ( 'NONE',  ( -19.97968237250000101, 1483.906011188890034, 214.0068283976289933 ) ) ;
#21332 = CARTESIAN_POINT ( 'NONE',  ( -17.04532912216367180, 1517.151704408390060, 196.9538555332918293 ) ) ;
#21333 = CARTESIAN_POINT ( 'NONE',  ( -101.9108661632280075, 1384.597254715800091, 311.0043636481769909 ) ) ;
#21334 = CARTESIAN_POINT ( 'NONE',  ( -36.32278535918399598, 1384.981498583400025, 209.7013335389069937 ) ) ;
#21335 = B_SPLINE_CURVE_WITH_KNOTS ( 'NONE', 3,
 ( #76656, #101834, #102398, #25681, #43066, #8334, #67727, #100734, #67174, #24018, #77226, #83394, #110806, #25128, #101273, #6692, #59874, #83949, #34098, #58760, #7249, #34652, #42498, #59331, #92341, #24570, #41411, #68836, #40848, #68291, #26240, #93442, #60429, #94547, #84501, #51457, #75578, #109171, #17820, #75021, #66633, #16711, #32458, #85044, #109710, #32985, #16172, #50375, #7791, #77767, #35763, #36307 ),
 .UNSPECIFIED., .F., .F.,
 ( 4, 2, 2, 1, 1, 2, 2, 2, 1, 1, 1, 2, 2, 2, 2, 1, 1, 1, 2, 2, 2, 2, 1, 1, 1, 2, 2, 1, 1, 1, 2, 2, 4 ),
 ( 0.000000000000000000, 0.06249999999992944533, 0.09374999999989959421, 0.1093749999999656525, 0.1171875000000026784, 0.1210937500000212053, 0.1250000000000397182, 0.1875000000002257361, 0.2187500000004227174, 0.2343750000005219991, 0.2421875000006816214, 0.2460937500006476764, 0.2500000000006137313, 0.3750000000008417711, 0.4375000000009564016, 0.4687500000009153234, 0.4843750000008948398, 0.4921875000008845702, 0.4960937500008881229, 0.5000000000008917311, 0.6250000000009093837, 0.6875000000008434364, 0.7187500000009037215, 0.7343750000010336176, 0.7421875000011902701, 0.7460937500011635137, 0.7500000000011366463, 0.8125000000007555068, 0.8437500000004857226, 0.8593750000003508305, 0.8671875000002831069, 0.8750000000002154943, 1.000000000000000000 ),
 .UNSPECIFIED. ) ;
#21336 = CARTESIAN_POINT ( 'NONE',  ( -4.979503507856909650, 1508.551704408389924, 206.4216282949940364 ) ) ;
#21337 = FACE_OUTER_BOUND ( 'NONE', #17187, .T. ) ;
#21338 = CARTESIAN_POINT ( 'NONE',  ( -31.12456774391181469, 1525.960063244516959, 201.1524202391567258 ) ) ;
#21340 = EDGE_LOOP ( 'NONE', ( #55957, #39106, #83633 ) ) ;
#21339 = CARTESIAN_POINT ( 'NONE',  ( 5.059013353549999259, 1501.257177412389865, 229.8390314845989906 ) ) ;
#21341 = CARTESIAN_POINT ( 'NONE',  ( -109.6573945330000157, 1384.913341287360026, 311.3230419672590301 ) ) ;
#21342 = CARTESIAN_POINT ( 'NONE',  ( 1.442193076691909992, 1490.929412776270055, 236.0730353711790031 ) ) ;
#21343 = EDGE_CURVE ( 'NONE', #20574, #32804, #80741, .T. ) ;
#21344 = CARTESIAN_POINT ( 'NONE',  ( -3.907660151049999975, 1495.688198251490121, 219.6140096315990036 ) ) ;
#21345 = CARTESIAN_POINT ( 'NONE',  ( -12.77587743780000018, 1416.568813547830132, 195.5427461491979955 ) ) ;
#21346 = DIRECTION ( 'NONE',  ( -0.000000000000000000, -1.000000000000000000, -0.000000000000000000 ) ) ;
#21347 = AXIS2_PLACEMENT_3D ( 'NONE', #100964, #41073, #109400 ) ;
#21348 = CARTESIAN_POINT ( 'NONE',  ( 21.69405894630000020, 1409.835083189130046, 215.3959610885380016 ) ) ;
#21349 = CARTESIAN_POINT ( 'NONE',  ( -2.922656181083440163, 1412.660035859490108, 186.5114004217930130 ) ) ;
#21350 = CARTESIAN_POINT ( 'NONE',  ( -19.64813173790599876, 1466.604908830560134, 204.2400468754019869 ) ) ;
#21351 = CARTESIAN_POINT ( 'NONE',  ( -5.360299083833290013, 1422.241314829860130, 144.2409028308489667 ) ) ;
#21353 = CARTESIAN_POINT ( 'NONE',  ( -12.42424857989999865, 1378.957147359669989, 207.0567700494690087 ) ) ;
#21352 = CARTESIAN_POINT ( 'NONE',  ( 4.097009089535375459, 1512.187213306747481, 201.1608118946568311 ) ) ;
#21354 = CARTESIAN_POINT ( 'NONE',  ( 24.86506402033909779, 1430.503309461649906, 208.3719473011869923 ) ) ;
#21355 = CARTESIAN_POINT ( 'NONE',  ( -102.6425412750940325, 1375.179104070689846, 310.0986725874599870 ) ) ;
#21356 = CARTESIAN_POINT ( 'NONE',  ( -32.02808312589908013, 1511.187213306747708, 219.9649204700466782 ) ) ;
#21357 = CARTESIAN_POINT ( 'NONE',  ( -1.383935618409999790, 1416.536379228330134, 233.4680935172980014 ) ) ;
#21358 = CARTESIAN_POINT ( 'NONE',  ( 6.892224678229999846, 1361.632554499760090, 210.6218459616991936 ) ) ;
#21359 = ADVANCED_FACE ( 'NONE', ( #55553 ), #86361, .F. ) ;
#21360 = CARTESIAN_POINT ( 'NONE',  ( 3.448206878685000198, 1516.904492006980036, 205.0794281543969646 ) ) ;
#21361 = CARTESIAN_POINT ( 'NONE',  ( -4.338088841202789148, 1484.259041794070072, 183.5077872766069902 ) ) ;
#21362 = ORIENTED_EDGE ( 'NONE', *, *, #56853, .F. ) ;
#21363 = CARTESIAN_POINT ( 'NONE',  ( -9553.690947211385719, 5182.767774292097783, 845.7647807759669831 ) ) ;
#21364 = CARTESIAN_POINT ( 'NONE',  ( 18.08041632129999954, 1415.296882296330068, 210.6774151550479814 ) ) ;
#21366 = ORIENTED_EDGE ( 'NONE', *, *, #77, .F. ) ;
#21365 = CARTESIAN_POINT ( 'NONE',  ( -67.68653639069999883, 1379.747580689210054, 278.9655481578590184 ) ) ;
#21367 = ORIENTED_EDGE ( 'NONE', *, *, #86710, .F. ) ;
#21368 = CARTESIAN_POINT ( 'NONE',  ( 29.02287039530000001, 1509.869659243430078, 211.4398731524179880 ) ) ;
#21369 = ORIENTED_EDGE ( 'NONE', *, *, #95300, .F. ) ;
#21370 = CARTESIAN_POINT ( 'NONE',  ( -24.89939545272470056, 1440.978110083920001, 210.4300214511639808 ) ) ;
#21371 = CARTESIAN_POINT ( 'NONE',  ( 1.547463840030000037, 1414.913060387329779, 192.3096136973980208 ) ) ;
#21373 = CARTESIAN_POINT ( 'NONE',  ( 0.4819869456859999790, 1507.639374880330024, 180.9399793378979950 ) ) ;
#21372 = CARTESIAN_POINT ( 'NONE',  ( 15.81261799660090084, 1415.231763502519925, 191.3817023155100117 ) ) ;
#21374 = CARTESIAN_POINT ( 'NONE',  ( -4.028611259245000298, 1516.744381837270112, 210.2562039408269925 ) ) ;
#21375 = AXIS2_PLACEMENT_3D ( 'NONE', #442, #35113, #26706 ) ;
#21376 = EDGE_CURVE ( 'NONE', #18619, #90692, #75269, .T. ) ;
#21377 = CARTESIAN_POINT ( 'NONE',  ( -25.25219063472429681, 1451.151841954119845, 137.3646034387350028 ) ) ;
#21378 = CARTESIAN_POINT ( 'NONE',  ( -0.4528338272850009893, 1469.497291256290055, 219.1901816671989991 ) ) ;
#21379 = CARTESIAN_POINT ( 'NONE',  ( 2.825023431620000025, 1409.011712379730170, 230.6343984061979882 ) ) ;
#21380 = CARTESIAN_POINT ( 'NONE',  ( 9.978765032700469106, 1482.348874302069817, 212.8318254667499900 ) ) ;
#21381 = PRODUCT_CONTEXT ( 'NONE', #22664, 'mechanical' ) ;
#21382 = CARTESIAN_POINT ( 'NONE',  ( 39.89055406515740287, 1448.739173192549970, 134.0999999981559938 ) ) ;
#21383 =( BOUNDED_SURFACE ( )  B_SPLINE_SURFACE ( 5, 5, ( 
 ( #43053, #31466, #513, #57802, #39326, #34638 ),
 ( #40418, #68822, #102923, #32022, #26223, #60412 ),
 ( #97301, #53117, #78871, #44159, #77753, #43602 ),
 ( #2177, #86695, #3275, #1062, #104605, #9989 ),
 ( #36292, #105725, #18367, #71604, #27898, #87254 ),
 ( #54232, #52562, #35190, #10546, #36847, #45275 ),
 ( #78296, #88359, #62081, #96207, #70485, #1609 ),
 ( #95652, #19482, #53685, #44719, #79413, #69933 ),
 ( #11648, #87826, #35746, #11114, #104046, #27338 ),
 ( #61524, #62646, #2725, #71039, #29009, #45825 ),
 ( #105160, #28452, #79958, #18919, #96768, #63194 ),
 ( #37405, #20037, #52005, #86145, #103483, #9438 ),
 ( #69374, #26788, #60976, #95101, #22218, #106794 ),
 ( #21671, #47465, #12748, #46382, #12189, #39031 ),
 ( #55323, #82708, #40149, #80514, #63730, #3831 ),
 ( #72668, #88903, #74332, #22766, #89998, #30084 ),
 ( #30650, #56970, #64278, #37959, #13273, #81586 ),
 ( #72140, #13823, #31742, #106257, #64836, #55877 ),
 ( #48009, #98943, #73776, #38491, #56416, #29543 ),
 ( #14380, #48573, #5446, #4890, #39606, #46930 ),
 ( #97840, #98398, #21118, #73210, #90546, #107900 ),
 ( #89455, #107354, #81048, #31193, #4363, #91102 ),
 ( #82147, #65380, #99483, #5997, #108460, #65929 ),
 ( #20572, #54771, #101917, #42038, #50, #8975 ),
 ( #16251, #26891, #67806, #68922, #43147, #86791 ),
 ( #34731, #76739, #25206, #34181, #94077, #77304 ),
 ( #26318, #35848, #60510, #1708, #10081, #68366 ),
 ( #92978, #94634, #95196, #76190, #103022, #18456 ),
 ( #35286, #102473, #25763, #70033, #59962, #51542 ),
 ( #50455, #84579, #602, #85679, #59410, #44256 ),
 ( #7871, #93523, #110337, #33609, #17346, #16792 ),
 ( #50996, #17908, #52105, #42586, #86235, #69471 ),
 ( #85126, #61081, #9526, #43694, #8414, #78398 ),
 ( #77847, #1156, #103591, #58844, #52654, #24644 ),
 ( #87919, #104694, #56926, #70577, #2274, #27989 ),
 ( #53211, #12706, #38994, #5961, #47423, #39565 ),
 ( #95746, #96300, #78969, #81015, #36388, #81546 ),
 ( #82107, #4847, #13234, #107861, #62174, #73171 ),
 ( #30046, #87352, #48531, #91055, #19580, #22176 ),
 ( #72624, #107315, #106756, #22724, #82670, #53782 ),
 ( #30610, #64238, #99447, #31150, #46889, #19010 ),
 ( #98906, #10648, #4321, #65338, #64797, #56375 ),
 ( #38452, #14341, #98360, #90505, #13783, #21633 ),
 ( #89959, #47965, #44815, #40106, #55838, #5405 ),
 ( #73738, #104145, #27430, #61613, #110070, #66985 ),
 ( #76468, #49630, #32801, #33346, #110621, #41216 ),
 ( #93795, #109525, #101642, #74833, #102211, #58580 ),
 ( #67541, #33903, #14891, #41759, #68098, #15438 ),
 ( #75388, #83765, #8697, #101096, #24395, #66443 ),
 ( #65885, #92709, #15985, #108976, #25492, #17069 ),
 ( #6506, #57490, #100005, #7061, #31702, #51266 ),
 ( #50188, #84314, #92167, #7605, #8147, #59682 ),
 ( #85399, #75918, #24930, #91614, #74288, #32263 ),
 ( #59140, #100558, #108418, #93263, #16526, #50717 ),
 ( #23293, #49082, #83217, #40660, #84846, #42313 ),
 ( #23838, #58030, #85971, #60802, #102744, #35562 ),
 ( #61909, #87078, #19299, #70317, #26039, #9271 ),
 ( #95479, #889, #60232, #103875, #78118, #26606 ),
 ( #104984, #43431, #51834, #77580, #94928, #94351 ),
 ( #10362, #54064, #18746, #87643, #68644, #34467 ),
 ( #17630, #18200, #35011, #52940, #69192, #53499 ),
 ( #103298, #52397, #27176, #96590, #86520, #62469 ),
 ( #43981, #36678, #45105, #9813, #1422, #69759 ),
 ( #36132, #61360, #44535, #79245, #78680, #1997 ),
 ( #104430, #2555, #27723, #96027, #10929, #70871 ),
 ( #28274, #19861, #88191, #42877, #77034, #342 ),
 ( #88741, #38316, #106086, #22038, #47283, #4183 ),
 ( #13643, #97680, #80888, #81406, #47833, #89280 ),
 ( #4718, #99312, #107734, #20954, #12576, #30471 ),
 ( #55158, #22585, #11484, #13100, #56790, #97135 ),
 ( #46757, #20404, #72495, #106624, #3656, #81966 ),
 ( #29911, #64104, #46205, #73605, #31019, #3104 ),
 ( #105546, #37233, #63565, #79798, #65199, #5273 ),
 ( #98224, #29364, #21494, #39429, #55707, #28833 ),
 ( #89827, #71430, #63030, #38862, #45660, #54609 ),
 ( #73040, #12025, #107181, #64658, #98776, #80340 ),
 ( #56236, #90365, #37786, #71974, #15308, #110492 ),
 ( #7478, #91489, #8023, #75256, #48399, #15845 ) ),
 .UNSPECIFIED., .F., .F., .T. ) 
 B_SPLINE_SURFACE_WITH_KNOTS ( ( 6, 3, 3, 3, 3, 3, 3, 3, 3, 3, 3, 3, 3, 3, 3, 3, 3, 3, 3, 3, 3, 3, 3, 3, 3, 6 ),
 ( 6, 6 ),
 ( 0.000000000000000000, 3.902585213099999617, 6.240861926940000082, 6.790072646649999655, 8.377982366400001268, 8.928580102349998882, 10.97133995140000096, 12.98949692180000071, 13.60228008900000063, 15.24737252870000148, 15.86745694640000082, 18.51059426890000026, 22.57641725190000059, 26.75087197450000076, 31.16005629229999840, 33.90953505430000092, 34.60237748540000524, 36.31249047570000243, 36.97255805550000218, 38.99052022429999909, 41.04947707190000017, 41.62972334150000364, 43.19545136810000230, 43.76106149099999953, 46.17824368760000198, 50.04091111600000374 ),
 ( 4.712388980370019631, 9.424777960769999297 ),
 .UNSPECIFIED. ) 
 GEOMETRIC_REPRESENTATION_ITEM ( )  RATIONAL_B_SPLINE_SURFACE ( (
 ( 0.2500000000000000000, 0.2499999999993640087, 0.2999999999990460298, 0.3999999999987279842, 0.5999999999987279953, 1.000000000000000000),
 ( 0.2500000000000000000, 0.2499999999993640087, 0.2999999999990460298, 0.3999999999987279842, 0.5999999999987279953, 1.000000000000000000),
 ( 0.2500000000000000000, 0.2499999999993640087, 0.2999999999990460298, 0.3999999999987279842, 0.5999999999987279953, 1.000000000000000000),
 ( 0.2500000000000000000, 0.2499999999993640087, 0.2999999999990460298, 0.3999999999987279842, 0.5999999999987279953, 1.000000000000000000),
 ( 0.2500000000000000000, 0.2499999999993640087, 0.2999999999990460298, 0.3999999999987279842, 0.5999999999987279953, 1.000000000000000000),
 ( 0.2500000000000000000, 0.2499999999993640087, 0.2999999999990460298, 0.3999999999987279842, 0.5999999999987279953, 1.000000000000000000),
 ( 0.2500000000000000000, 0.2499999999993640087, 0.2999999999990460298, 0.3999999999987279842, 0.5999999999987279953, 1.000000000000000000),
 ( 0.2500000000000000000, 0.2499999999993640087, 0.2999999999990460298, 0.3999999999987279842, 0.5999999999987279953, 1.000000000000000000),
 ( 0.2500000000000000000, 0.2499999999993640087, 0.2999999999990460298, 0.3999999999987279842, 0.5999999999987279953, 1.000000000000000000),
 ( 0.2500000000000000000, 0.2499999999993640087, 0.2999999999990460298, 0.3999999999987279842, 0.5999999999987279953, 1.000000000000000000),
 ( 0.2500000000000000000, 0.2499999999993640087, 0.2999999999990460298, 0.3999999999987279842, 0.5999999999987279953, 1.000000000000000000),
 ( 0.2500000000000000000, 0.2499999999993640087, 0.2999999999990460298, 0.3999999999987279842, 0.5999999999987279953, 1.000000000000000000),
 ( 0.2500000000000000000, 0.2499999999993640087, 0.2999999999990460298, 0.3999999999987279842, 0.5999999999987279953, 1.000000000000000000),
 ( 0.2500000000000000000, 0.2499999999993640087, 0.2999999999990460298, 0.3999999999987279842, 0.5999999999987279953, 1.000000000000000000),
 ( 0.2500000000000000000, 0.2499999999993640087, 0.2999999999990460298, 0.3999999999987279842, 0.5999999999987279953, 1.000000000000000000),
 ( 0.2500000000000000000, 0.2499999999993640087, 0.2999999999990460298, 0.3999999999987279842, 0.5999999999987279953, 1.000000000000000000),
 ( 0.2500000000000000000, 0.2499999999993640087, 0.2999999999990460298, 0.3999999999987279842, 0.5999999999987279953, 1.000000000000000000),
 ( 0.2500000000000000000, 0.2499999999993640087, 0.2999999999990460298, 0.3999999999987279842, 0.5999999999987279953, 1.000000000000000000),
 ( 0.2500000000000000000, 0.2499999999993640087, 0.2999999999990460298, 0.3999999999987279842, 0.5999999999987279953, 1.000000000000000000),
 ( 0.2500000000000000000, 0.2499999999993640087, 0.2999999999990460298, 0.3999999999987279842, 0.5999999999987279953, 1.000000000000000000),
 ( 0.2500000000000000000, 0.2499999999993640087, 0.2999999999990460298, 0.3999999999987279842, 0.5999999999987279953, 1.000000000000000000),
 ( 0.2500000000000000000, 0.2499999999993640087, 0.2999999999990460298, 0.3999999999987279842, 0.5999999999987279953, 1.000000000000000000),
 ( 0.2500000000000000000, 0.2499999999993640087, 0.2999999999990460298, 0.3999999999987279842, 0.5999999999987279953, 1.000000000000000000),
 ( 0.2500000000000000000, 0.2499999999993640087, 0.2999999999990460298, 0.3999999999987279842, 0.5999999999987279953, 1.000000000000000000),
 ( 0.2500000000000000000, 0.2499999999993640087, 0.2999999999990460298, 0.3999999999987279842, 0.5999999999987279953, 1.000000000000000000),
 ( 0.2500000000000000000, 0.2499999999993640087, 0.2999999999990460298, 0.3999999999987279842, 0.5999999999987279953, 1.000000000000000000),
 ( 0.2500000000000000000, 0.2499999999993640087, 0.2999999999990460298, 0.3999999999987279842, 0.5999999999987279953, 1.000000000000000000),
 ( 0.2500000000000000000, 0.2499999999993640087, 0.2999999999990460298, 0.3999999999987279842, 0.5999999999987279953, 1.000000000000000000),
 ( 0.2500000000000000000, 0.2499999999993640087, 0.2999999999990460298, 0.3999999999987279842, 0.5999999999987279953, 1.000000000000000000),
 ( 0.2500000000000000000, 0.2499999999993640087, 0.2999999999990460298, 0.3999999999987279842, 0.5999999999987279953, 1.000000000000000000),
 ( 0.2500000000000000000, 0.2499999999993640087, 0.2999999999990460298, 0.3999999999987279842, 0.5999999999987279953, 1.000000000000000000),
 ( 0.2500000000000000000, 0.2499999999993640087, 0.2999999999990460298, 0.3999999999987279842, 0.5999999999987279953, 1.000000000000000000),
 ( 0.2500000000000000000, 0.2499999999993640087, 0.2999999999990460298, 0.3999999999987279842, 0.5999999999987279953, 1.000000000000000000),
 ( 0.2500000000000000000, 0.2499999999993640087, 0.2999999999990460298, 0.3999999999987279842, 0.5999999999987279953, 1.000000000000000000),
 ( 0.2500000000000000000, 0.2499999999993640087, 0.2999999999990460298, 0.3999999999987279842, 0.5999999999987279953, 1.000000000000000000),
 ( 0.2500000000000000000, 0.2499999999993640087, 0.2999999999990460298, 0.3999999999987279842, 0.5999999999987279953, 1.000000000000000000),
 ( 0.2500000000000000000, 0.2499999999993640087, 0.2999999999990460298, 0.3999999999987279842, 0.5999999999987279953, 1.000000000000000000),
 ( 0.2500000000000000000, 0.2499999999993640087, 0.2999999999990460298, 0.3999999999987279842, 0.5999999999987279953, 1.000000000000000000),
 ( 0.2500000000000000000, 0.2499999999993640087, 0.2999999999990460298, 0.3999999999987279842, 0.5999999999987279953, 1.000000000000000000),
 ( 0.2500000000000000000, 0.2499999999993640087, 0.2999999999990460298, 0.3999999999987279842, 0.5999999999987279953, 1.000000000000000000),
 ( 0.2500000000000000000, 0.2499999999993640087, 0.2999999999990460298, 0.3999999999987279842, 0.5999999999987279953, 1.000000000000000000),
 ( 0.2500000000000000000, 0.2499999999993640087, 0.2999999999990460298, 0.3999999999987279842, 0.5999999999987279953, 1.000000000000000000),
 ( 0.2500000000000000000, 0.2499999999993640087, 0.2999999999990460298, 0.3999999999987279842, 0.5999999999987279953, 1.000000000000000000),
 ( 0.2500000000000000000, 0.2499999999993640087, 0.2999999999990460298, 0.3999999999987279842, 0.5999999999987279953, 1.000000000000000000),
 ( 0.2500000000000000000, 0.2499999999993640087, 0.2999999999990460298, 0.3999999999987279842, 0.5999999999987279953, 1.000000000000000000),
 ( 0.2500000000000000000, 0.2499999999993640087, 0.2999999999990460298, 0.3999999999987279842, 0.5999999999987279953, 1.000000000000000000),
 ( 0.2500000000000000000, 0.2499999999993640087, 0.2999999999990460298, 0.3999999999987279842, 0.5999999999987279953, 1.000000000000000000),
 ( 0.2500000000000000000, 0.2499999999993640087, 0.2999999999990460298, 0.3999999999987279842, 0.5999999999987279953, 1.000000000000000000),
 ( 0.2500000000000000000, 0.2499999999993640087, 0.2999999999990460298, 0.3999999999987279842, 0.5999999999987279953, 1.000000000000000000),
 ( 0.2500000000000000000, 0.2499999999993640087, 0.2999999999990460298, 0.3999999999987279842, 0.5999999999987279953, 1.000000000000000000),
 ( 0.2500000000000000000, 0.2499999999993640087, 0.2999999999990460298, 0.3999999999987279842, 0.5999999999987279953, 1.000000000000000000),
 ( 0.2500000000000000000, 0.2499999999993640087, 0.2999999999990460298, 0.3999999999987279842, 0.5999999999987279953, 1.000000000000000000),
 ( 0.2500000000000000000, 0.2499999999993640087, 0.2999999999990460298, 0.3999999999987279842, 0.5999999999987279953, 1.000000000000000000),
 ( 0.2500000000000000000, 0.2499999999993640087, 0.2999999999990460298, 0.3999999999987279842, 0.5999999999987279953, 1.000000000000000000),
 ( 0.2500000000000000000, 0.2499999999993640087, 0.2999999999990460298, 0.3999999999987279842, 0.5999999999987279953, 1.000000000000000000),
 ( 0.2500000000000000000, 0.2499999999993640087, 0.2999999999990460298, 0.3999999999987279842, 0.5999999999987279953, 1.000000000000000000),
 ( 0.2500000000000000000, 0.2499999999993640087, 0.2999999999990460298, 0.3999999999987279842, 0.5999999999987279953, 1.000000000000000000),
 ( 0.2500000000000000000, 0.2499999999993640087, 0.2999999999990460298, 0.3999999999987279842, 0.5999999999987279953, 1.000000000000000000),
 ( 0.2500000000000000000, 0.2499999999993640087, 0.2999999999990460298, 0.3999999999987279842, 0.5999999999987279953, 1.000000000000000000),
 ( 0.2500000000000000000, 0.2499999999993640087, 0.2999999999990460298, 0.3999999999987279842, 0.5999999999987279953, 1.000000000000000000),
 ( 0.2500000000000000000, 0.2499999999993640087, 0.2999999999990460298, 0.3999999999987279842, 0.5999999999987279953, 1.000000000000000000),
 ( 0.2500000000000000000, 0.2499999999993640087, 0.2999999999990460298, 0.3999999999987279842, 0.5999999999987279953, 1.000000000000000000),
 ( 0.2500000000000000000, 0.2499999999993640087, 0.2999999999990460298, 0.3999999999987279842, 0.5999999999987279953, 1.000000000000000000),
 ( 0.2500000000000000000, 0.2499999999993640087, 0.2999999999990460298, 0.3999999999987279842, 0.5999999999987279953, 1.000000000000000000),
 ( 0.2500000000000000000, 0.2499999999993640087, 0.2999999999990460298, 0.3999999999987279842, 0.5999999999987279953, 1.000000000000000000),
 ( 0.2500000000000000000, 0.2499999999993640087, 0.2999999999990460298, 0.3999999999987279842, 0.5999999999987279953, 1.000000000000000000),
 ( 0.2500000000000000000, 0.2499999999993640087, 0.2999999999990460298, 0.3999999999987279842, 0.5999999999987279953, 1.000000000000000000),
 ( 0.2500000000000000000, 0.2499999999993640087, 0.2999999999990460298, 0.3999999999987279842, 0.5999999999987279953, 1.000000000000000000),
 ( 0.2500000000000000000, 0.2499999999993640087, 0.2999999999990460298, 0.3999999999987279842, 0.5999999999987279953, 1.000000000000000000),
 ( 0.2500000000000000000, 0.2499999999993640087, 0.2999999999990460298, 0.3999999999987279842, 0.5999999999987279953, 1.000000000000000000),
 ( 0.2500000000000000000, 0.2499999999993640087, 0.2999999999990460298, 0.3999999999987279842, 0.5999999999987279953, 1.000000000000000000),
 ( 0.2500000000000000000, 0.2499999999993640087, 0.2999999999990460298, 0.3999999999987279842, 0.5999999999987279953, 1.000000000000000000),
 ( 0.2500000000000000000, 0.2499999999993640087, 0.2999999999990460298, 0.3999999999987279842, 0.5999999999987279953, 1.000000000000000000),
 ( 0.2500000000000000000, 0.2499999999993640087, 0.2999999999990460298, 0.3999999999987279842, 0.5999999999987279953, 1.000000000000000000),
 ( 0.2500000000000000000, 0.2499999999993640087, 0.2999999999990460298, 0.3999999999987279842, 0.5999999999987279953, 1.000000000000000000),
 ( 0.2500000000000000000, 0.2499999999993640087, 0.2999999999990460298, 0.3999999999987279842, 0.5999999999987279953, 1.000000000000000000),
 ( 0.2500000000000000000, 0.2499999999993640087, 0.2999999999990460298, 0.3999999999987279842, 0.5999999999987279953, 1.000000000000000000),
 ( 0.2500000000000000000, 0.2499999999993640087, 0.2999999999990460298, 0.3999999999987279842, 0.5999999999987279953, 1.000000000000000000) ) ) 
 REPRESENTATION_ITEM ( '' )  SURFACE ( )  );
#21384 = CARTESIAN_POINT ( 'NONE',  ( 3.552713678799999608E-15, 1384.913060387289988, 209.1218459572589836 ) ) ;
#21385 = ORIENTED_EDGE ( 'NONE', *, *, #83639, .F. ) ;
#21386 = CARTESIAN_POINT ( 'NONE',  ( 18.28863001267049881, 1430.119171029580002, 201.0315453683600140 ) ) ;
#21387 = CARTESIAN_POINT ( 'NONE',  ( -17.04521188157725931, 1526.211528530236592, 235.5955628457882653 ) ) ;
#21388 = ORIENTED_EDGE ( 'NONE', *, *, #20659, .T. ) ;
#21389 = VERTEX_POINT ( 'NONE', #96728 ) ;
#21390 = ORIENTED_EDGE ( 'NONE', *, *, #105003, .F. ) ;
#21391 = CARTESIAN_POINT ( 'NONE',  ( -6.017564101925000131, 1514.771170611759999, 217.0138083832570146 ) ) ;
#21392 = CARTESIAN_POINT ( 'NONE',  ( 16.44706023844862841, 1514.320576807016550, 194.6473512539881199 ) ) ;
#21393 = CARTESIAN_POINT ( 'NONE',  ( -14.09820228469869896, 1379.801286730300035, 211.4211468150479902 ) ) ;
#21394 = CARTESIAN_POINT ( 'NONE',  ( -3.004397273099999932, 1485.815138895830160, 182.5519705833980026 ) ) ;
#21395 = AXIS2_PLACEMENT_3D ( 'NONE', #51219, #87023, #34417 ) ;
#21396 = CARTESIAN_POINT ( 'NONE',  ( -17.53521452141892922, 1448.184789224442511, 218.0158466994055857 ) ) ;
#21397 = CARTESIAN_POINT ( 'NONE',  ( -68.30823798306452943, 1379.747042357273358, 279.0703650132669509 ) ) ;
#21398 = CARTESIAN_POINT ( 'NONE',  ( -1.157238773510000041, 1464.257248818090147, 199.2213037580589798 ) ) ;
#21399 = EDGE_CURVE ( 'NONE', #7904, #45774, #49702, .T. ) ;
#21400 = CARTESIAN_POINT ( 'NONE',  ( -9.862951377749247683, 1522.051704408389924, 228.3939896778649654 ) ) ;
#21401 = CARTESIAN_POINT ( 'NONE',  ( 34.18677586421181758, 1501.977400791986611, 198.4504086008745389 ) ) ;
#21402 = CARTESIAN_POINT ( 'NONE',  ( -61.12661706479850210, 1384.679990717839928, 246.4532168033390178 ) ) ;
#21403 = EDGE_LOOP ( 'NONE', ( #24724, #94354, #49724, #40139 ) ) ;
#21404 = CARTESIAN_POINT ( 'NONE',  ( -1.136814071995000175, 1516.854133554269993, 206.8377924607469822 ) ) ;
#21405 = EDGE_LOOP ( 'NONE', ( #83805, #98486, #73894, #88233 ) ) ;
#21406 = CARTESIAN_POINT ( 'NONE',  ( 40.21729846317249724, 1440.913060387330006, 267.6250173488770088 ) ) ;
#21407 = B_SPLINE_CURVE_WITH_KNOTS ( 'NONE', 3,
 ( #96211, #13277, #12193, #4895, #63199, #20576, #105729, #21122, #81591, #19486, #2729, #97306, #97846, #55327, #79418, #12752, #53689, #55881, #45279, #27902, #71043, #11653, #90002, #46386, #39035, #105165, #89459, #11119, #3279, #36851, #79962, #80518, #47469, #104609, #3835, #96772, #71608 ),
 .UNSPECIFIED., .F., .F.,
 ( 4, 3, 3, 3, 3, 3, 3, 3, 3, 3, 3, 3, 4 ),
 ( -11.90357780880000149, -11.65138654548870001, -10.97030762600710041, -10.24753412388749929, -9.484849656234679571, -8.666253744101309664, -7.699452457123720173, -6.772837301347459871, -5.935629956368320137, -5.021959782221260049, -4.226855386626629851, -3.539500458311259479, -2.894173653930000256 ),
 .UNSPECIFIED. ) ;
#21408 = CARTESIAN_POINT ( 'NONE',  ( -0.0005665943966642099589, 1451.957582760023797, 153.9843603111906134 ) ) ;
#21409 = EDGE_CURVE ( 'NONE', #80799, #26062, #69381, .T. ) ;
#21410 = VERTEX_POINT ( 'NONE', #9948 ) ;
#21411 = CARTESIAN_POINT ( 'NONE',  ( -17.19739463999666285, 1525.960063244516959, 181.9833109756550584 ) ) ;
#21412 = CARTESIAN_POINT ( 'NONE',  ( -16.40120703590000062, 1409.652464985630104, 192.2255933302979827 ) ) ;
#21413 = CARTESIAN_POINT ( 'NONE',  ( -24.35246777550132435, 1439.602140306827550, 212.0316767823215685 ) ) ;
#21414 = CARTESIAN_POINT ( 'NONE',  ( -9.783936650027678539, 1438.409968310599879, 210.7790528106160082 ) ) ;
#21415 = CARTESIAN_POINT ( 'NONE',  ( -5.704331135097779892, 1511.494703458840149, 200.8748168550339983 ) ) ;
#21416 = CARTESIAN_POINT ( 'NONE',  ( 14.57089808959999999, 1407.761835850630177, 266.8771382033980331 ) ) ;
#21417 = CARTESIAN_POINT ( 'NONE',  ( -5.567211192487503624, 1510.484595312941110, 201.5712314627286617 ) ) ;
#21418 = CARTESIAN_POINT ( 'NONE',  ( 26.21319982379560187, 1493.418275869099944, 206.2276069840760044 ) ) ;
#21420 = LINE ( 'NONE', #84647, #11802 ) ;
#21419 = CARTESIAN_POINT ( 'NONE',  ( 10.17186614039999881, 1464.738249403130112, 232.3595462222980075 ) ) ;
#21421 = CIRCLE ( 'NONE', #28555, 2.000048411567817652 ) ;
#21422 = B_SPLINE_SURFACE_WITH_KNOTS ( 'NONE', 5, 5, ( 
 ( #11583, #27270, #71535, #28378, #61454, #26144 ),
 ( #94452, #62579, #36228, #104533, #27829, #19405 ),
 ( #19968, #2654, #53609, #54162, #17731, #86074 ),
 ( #44214, #86753, #51499, #76695, #35807, #102981 ),
 ( #69989, #78357, #1116, #1666, #53170, #7 ),
 ( #43106, #101874, #50957, #8932, #103546, #85632 ),
 ( #34143, #104104, #95158, #60469, #27393, #26280 ),
 ( #16751, #17866, #87312, #67762, #68327, #102435 ),
 ( #25719, #77265, #94586, #10043, #34690, #77807 ),
 ( #26849, #10605, #44776, #78927, #8373, #564 ),
 ( #35245, #61037, #85084, #59370, #61575, #95708 ),
 ( #18974, #18417, #52065, #33570, #25167, #68880 ) ),
 .UNSPECIFIED., .F., .F., .F.,
 ( 6, 3, 3, 6 ),
 ( 6, 6 ),
 ( 30.85152358798220007, 67.48111802349998811, 89.44935581500000410, 144.2305269969999983 ),
 ( -1.869926188701470044E-05, 0.4689188517720000449 ),
 .UNSPECIFIED. ) ;
#21423 = CARTESIAN_POINT ( 'NONE',  ( 2.487103419534999915, 1516.577434278289957, 215.6681487122470173 ) ) ;
#21424 = ADVANCED_FACE ( 'NONE', ( #44120 ), #3239, .T. ) ;
#21425 = CARTESIAN_POINT ( 'NONE',  ( -2.472529913803022783, 1523.678648413191695, 242.8674788698241400 ) ) ;
#21426 = CARTESIAN_POINT ( 'NONE',  ( -0.1361220240859130071, 1507.783361145109893, 180.7555731139599970 ) ) ;
#21427 = CARTESIAN_POINT ( 'NONE',  ( 18.42528818938584223, 1446.189480375194762, 215.6021398651423340 ) ) ;
#21428 = CARTESIAN_POINT ( 'NONE',  ( 7.723480079395000253, 1517.086065052259983, 213.1573821953169841 ) ) ;
#21429 = CARTESIAN_POINT ( 'NONE',  ( -3.290427993577100100E-15, 1522.051704408389924, 209.1218459616989946 ) ) ;
#21431 = EDGE_LOOP ( 'NONE', ( #31891, #38636, #12729, #104321 ) ) ;
#21430 = CARTESIAN_POINT ( 'NONE',  ( -15.52294138480000107, 1421.387829696419885, 199.5510885761390227 ) ) ;
#21432 = DIRECTION ( 'NONE',  ( 0.000000000000000000, 0.000000000000000000, -1.000000000000000000 ) ) ;
#21433 = AXIS2_PLACEMENT_3D ( 'NONE', #71448, #14789, #4735 ) ;
#21434 = CARTESIAN_POINT ( 'NONE',  ( 19.46363819460000144, 1452.609789409330006, 213.2823703743680142 ) ) ;
#21435 = CARTESIAN_POINT ( 'NONE',  ( -11.76946808870000005, 1432.335038318230090, 150.8120985755979859 ) ) ;
#21436 = CARTESIAN_POINT ( 'NONE',  ( -15.22768491250000089, 1415.677402202029953, 208.4617985024749771 ) ) ;
#21437 = CARTESIAN_POINT ( 'NONE',  ( 1.804219641780000050, 1410.346235427530019, 232.1926713004979774 ) ) ;
#21438 = CARTESIAN_POINT ( 'NONE',  ( 16.73628186595820111, 1526.382868172864164, 184.0591879540915841 ) ) ;
#21439 = EDGE_CURVE ( 'NONE', #52400, #10255, #63939, .T. ) ;
#21440 = DIRECTION ( 'NONE',  ( 0.6709778558543737503, 0.000000000000000000, 0.7414773880254658112 ) ) ;
#21442 = CARTESIAN_POINT ( 'NONE',  ( 2.500000000000000000, 1428.988705744230174, 157.0781314899979861 ) ) ;
#21441 = CARTESIAN_POINT ( 'NONE',  ( -21.86656088110000340, 1470.082911937230165, 223.0158589924980106 ) ) ;
#21443 = CARTESIAN_POINT ( 'NONE',  ( 6.483588104269999874, 1462.707724100489941, 208.1814389384059893 ) ) ;
#21444 = EDGE_LOOP ( 'NONE', ( #61942, #4749, #60805, #21812 ) ) ;
#21445 = CARTESIAN_POINT ( 'NONE',  ( -2.297085753945000253, 1516.718889242609976, 205.0950684461469962 ) ) ;
#21446 = CARTESIAN_POINT ( 'NONE',  ( 2.744127903880000385, 1406.565768444329933, 269.4960847736980440 ) ) ;
#21447 = EDGE_CURVE ( 'NONE', #30006, #84966, #87215, .T. ) ;
#21448 = CARTESIAN_POINT ( 'NONE',  ( 0.7442430207950000431, 1515.589102391990082, 213.1386578140389929 ) ) ;
#21449 = CARTESIAN_POINT ( 'NONE',  ( 20.32238055547781741, 1427.042525162981065, 220.8319574201998421 ) ) ;
#21450 = CARTESIAN_POINT ( 'NONE',  ( -23.84533141485470153, 1452.080363065020038, 136.9869391916130041 ) ) ;
#21451 = CARTESIAN_POINT ( 'NONE',  ( 10.85844884284743550, 1424.793770695752301, 138.1921923629704168 ) ) ;
#21452 = B_SPLINE_CURVE_WITH_KNOTS ( 'NONE', 3,
 ( #56923, #101639, #76466, #32799, #24928, #83762, #58028, #58578, #50715, #74286, #32261, #6504, #110068, #8145, #99445, #49080, #59138, #5959, #91612 ),
 .UNSPECIFIED., .F., .F.,
 ( 4, 3, 3, 3, 3, 3, 4 ),
 ( -24.12443845425489997, -23.98402014143189831, -23.65737981169450066, -23.29041649494190125, -22.85542232492040071, -22.35670583347129892, -21.97924354190000074 ),
 .UNSPECIFIED. ) ;
#21453 = CARTESIAN_POINT ( 'NONE',  ( -10.32838887772869896, 1447.694493972999908, 209.8647986237220096 ) ) ;
#21454 = VECTOR ( 'NONE', #8055, 1000.000000000000000 ) ;
#21455 = CARTESIAN_POINT ( 'NONE',  ( -2.493007233162190417, 1449.246563095040074, 154.5202250740130125 ) ) ;
#21456 = CARTESIAN_POINT ( 'NONE',  ( -1.589953117590154230, 1450.801901463933291, 183.3727437628812709 ) ) ;
#21457 = CARTESIAN_POINT ( 'NONE',  ( 1.177008278681779929, 1450.813907473600011, 155.0627464472840131 ) ) ;
#21458 = CARTESIAN_POINT ( 'NONE',  ( -14.14453214052680075, 1415.673583083550056, 221.0709323776389965 ) ) ;
#21459 = CARTESIAN_POINT ( 'NONE',  ( -4.328507561560000383, 1515.100736413590084, 210.1977440287089962 ) ) ;
#21460 = AXIS2_PLACEMENT_3D ( 'NONE', #98916, #30621, #4333 ) ;
#21461 = CARTESIAN_POINT ( 'NONE',  ( -19.46212512329999811, 1433.716220832530098, 224.8635562271979893 ) ) ;
#21462 = B_SPLINE_CURVE_WITH_KNOTS ( 'NONE', 3,
 ( #47342, #81469, #29423, #12077, #107239, #20458, #3712, #105606, #38919, #90983, #4773, #29973, #64165, #39492, #71485, #56851, #63622, #73100, #72552, #55770, #89340, #14271, #80943, #30531, #106144, #46270, #73663, #64722, #98838, #22098, #97738, #56297, #89885, #21560, #37294, #72029, #21009, #55211, #88795, #46813 ),
 .UNSPECIFIED., .F., .F.,
 ( 4, 3, 3, 3, 3, 3, 3, 3, 3, 3, 3, 3, 3, 4 ),
 ( -1.999999742213449894, -1.877659734187909990, -1.724846248608389976, -1.569855302308919898, -1.413640332142279910, -1.255656791337570022, -1.096905799826189964, -0.9377556084170080020, -0.7786028042479620215, -0.6202726927077200081, -0.4629805089094820580, -0.3070336845188419428, -0.1526574299706571214, 0.000000000000000000 ),
 .UNSPECIFIED. ) ;
#21463 = B_SPLINE_CURVE_WITH_KNOTS ( 'NONE', 3,
 ( #27520, #71214, #61705, #105336, #70670, #80128, #45456, #95827, #3447, #79598, #19095, #2902, #28627 ),
 .UNSPECIFIED., .F., .F.,
 ( 4, 3, 3, 3, 4 ),
 ( -1.149508497110000027, -0.3382834629707950347, 0.4737402652647237922, 1.287219781555279718, 1.586334299330000031 ),
 .UNSPECIFIED. ) ;
#21464 = CARTESIAN_POINT ( 'NONE',  ( 11.02052227349364522, 1425.209676012653290, 138.6340692233841310 ) ) ;
#21465 = CARTESIAN_POINT ( 'NONE',  ( 3.670783216920000314, 1441.353588345389880, 162.1787147853980002 ) ) ;
#21466 = CARTESIAN_POINT ( 'NONE',  ( -0.3357575137870000281, 1475.318672749230018, 269.4986534752979992 ) ) ;
#21467 = CARTESIAN_POINT ( 'NONE',  ( -4.285659226341840267, 1446.893803312319960, 155.6485943791360000 ) ) ;
#21468 = CARTESIAN_POINT ( 'NONE',  ( -7.659352831203849910, 1423.043222450190115, 144.1531583550990092 ) ) ;
#21469 = CARTESIAN_POINT ( 'NONE',  ( -3.430286617134524096, 1448.286537935908427, 184.8322057208431488 ) ) ;
#21470 = CARTESIAN_POINT ( 'NONE',  ( -25.87963768509780138, 1384.843092929030036, 224.3457638931510019 ) ) ;
#21471 = DIRECTION ( 'NONE',  ( -0.6736849260863841948, 0.000000000000000000, 0.7390186874254148774 ) ) ;
#21472 = CARTESIAN_POINT ( 'NONE',  ( -105.9306909619999999, 1379.241374661100053, 301.2498419558590399 ) ) ;
#21473 = CARTESIAN_POINT ( 'NONE',  ( 31.32941717379424063, 1525.856064936179791, 217.0550765750803350 ) ) ;
#21474 = CARTESIAN_POINT ( 'NONE',  ( 8.053223258311438926, 1511.610050756687770, 205.5741034559911782 ) ) ;
#21475 = CARTESIAN_POINT ( 'NONE',  ( -10.50081440230080077, 1396.279756906559896, 212.6139382770819850 ) ) ;
#21476 = CARTESIAN_POINT ( 'NONE',  ( -14.49383190680000055, 1422.099016295730053, 229.4564906703980114 ) ) ;
#21477 = CARTESIAN_POINT ( 'NONE',  ( -44.38044571260000026, 1435.204496188100165, 269.7015000828980078 ) ) ;
#21478 = ORIENTED_EDGE ( 'NONE', *, *, #22780, .F. ) ;
#21479 = CARTESIAN_POINT ( 'NONE',  ( -11.33250792936460805, 1503.032974060135075, 207.0697244187343529 ) ) ;
#21480 = CARTESIAN_POINT ( 'NONE',  ( -13.58435925944560196, 1508.516896892319892, 210.0765856309430148 ) ) ;
#21481 = CARTESIAN_POINT ( 'NONE',  ( -20.21024070146840046, 1526.107876515966382, 233.6897457629616213 ) ) ;
#21483 = CARTESIAN_POINT ( 'NONE',  ( -12.84824846446499969, 1512.167884426309911, 193.7405250718670118 ) ) ;
#21482 = CARTESIAN_POINT ( 'NONE',  ( 11.02832889669999972, 1425.240829266930177, 135.9184656016980171 ) ) ;
#21484 = CARTESIAN_POINT ( 'NONE',  ( 0.000000000000000000, 1408.913060387329779, 209.1218459616979999 ) ) ;
#21485 = CARTESIAN_POINT ( 'NONE',  ( -6.991531664970000115, 1452.433546631890067, 202.2220901360489904 ) ) ;
#21486 = EDGE_CURVE ( 'NONE', #108761, #31410, #54740, .T. ) ;
#21487 = CIRCLE ( 'NONE', #55506, 1.999999999999998668 ) ;
#21488 = CARTESIAN_POINT ( 'NONE',  ( -2.873958889724999910, 1516.588006113850042, 202.1873174023370154 ) ) ;
#21489 = CARTESIAN_POINT ( 'NONE',  ( 7.799720914009999895, 1426.519650413049931, 211.9402747548089678 ) ) ;
#21490 = CARTESIAN_POINT ( 'NONE',  ( 10.99043244679999987, 1479.494642110589893, 229.8297439418990109 ) ) ;
#21491 = CARTESIAN_POINT ( 'NONE',  ( 4.084250106429999860, 1507.178795002029801, 181.6747636120979905 ) ) ;
#21492 = DIRECTION ( 'NONE',  ( 0.0002625959325066309024, 0.0002558942237557529668, 0.9999999327807589378 ) ) ;
#21493 = CARTESIAN_POINT ( 'NONE',  ( -66.50370960850830215, 1378.395022579190027, 281.8681772372950149 ) ) ;
#21494 = CARTESIAN_POINT ( 'NONE',  ( 5.679423221865293137, 1366.539118458927078, 209.6218459617148824 ) ) ;
#21496 = EDGE_LOOP ( 'NONE', ( #9425, #99335, #107600, #49653 ) ) ;
#21495 = CARTESIAN_POINT ( 'NONE',  ( 8.225616979109998894, 1452.226705206789802, 213.5360760307489727 ) ) ;
#21497 = ORIENTED_EDGE ( 'NONE', *, *, #96302, .F. ) ;
#21498 = CARTESIAN_POINT ( 'NONE',  ( -10.29370527480000064, 1396.272524496429924, 204.1694594168680226 ) ) ;
#21499 = FACE_OUTER_BOUND ( 'NONE', #101550, .T. ) ;
#21500 = CARTESIAN_POINT ( 'NONE',  ( -3.043932075285961769, 1516.569307157451021, 201.4118976829438736 ) ) ;
#21501 = CARTESIAN_POINT ( 'NONE',  ( -13.07809777927165662, 1444.819332124669927, 169.4094072714121637 ) ) ;
#21502 = CARTESIAN_POINT ( 'NONE',  ( 3.871411596960000256, 1475.513060387329915, 229.5852438705979921 ) ) ;
#21503 = CARTESIAN_POINT ( 'NONE',  ( -7.693233053164999724, 1511.639769324940062, 212.0885359432170389 ) ) ;
#21505 = CARTESIAN_POINT ( 'NONE',  ( 16.66093705349999965, 1410.867258618529831, 226.5061971588980043 ) ) ;
#21504 = CARTESIAN_POINT ( 'NONE',  ( -8.343937223730000241, 1384.261598685969830, 218.6501499107789925 ) ) ;
#21506 = AXIS2_PLACEMENT_3D ( 'NONE', #56043, #6724, #108080 ) ;
#21507 = B_SPLINE_CURVE_WITH_KNOTS ( 'NONE', 3,
 ( #35839, #105246, #104136, #53202 ),
 .UNSPECIFIED., .F., .F.,
 ( 4, 4 ),
 ( 0.000000000000000000, 0.0002960034161023848936 ),
 .UNSPECIFIED. ) ;
#21508 = EDGE_CURVE ( 'NONE', #92642, #90688, #78302, .T. ) ;
#21509 = CARTESIAN_POINT ( 'NONE',  ( -30.31940284292427634, 1523.382868172864164, 195.7503880523418616 ) ) ;
#21510 = CARTESIAN_POINT ( 'NONE',  ( -2.205815343605610046, 1463.135290986430164, 199.5903874811000094 ) ) ;
#21511 = CARTESIAN_POINT ( 'NONE',  ( -37.55262814633019275, 1450.862648038850011, 134.7342395472079772 ) ) ;
#21512 = CARTESIAN_POINT ( 'NONE',  ( 10.68392919824940002, 1396.286151416399889, 212.0224123608280138 ) ) ;
#21513 = CARTESIAN_POINT ( 'NONE',  ( -27.58075063647599734, 1440.826346164419874, 137.2340152947450065 ) ) ;
#21514 = CARTESIAN_POINT ( 'NONE',  ( 10.92291495829999981, 1429.022423092130111, 151.0007450078979900 ) ) ;
#21515 = FACE_OUTER_BOUND ( 'NONE', #66390, .T. ) ;
#21516 = VERTEX_POINT ( 'NONE', #103439 ) ;
#21517 = CARTESIAN_POINT ( 'NONE',  ( 12.89603720985889979, 1434.724810852120072, 149.2205511288100013 ) ) ;
#21518 = CARTESIAN_POINT ( 'NONE',  ( 21.28825147355426495, 1525.253972588462830, 234.3567090158657891 ) ) ;
#21519 = EDGE_LOOP ( 'NONE', ( #93690, #54666, #7514, #43563 ) ) ;
#21520 = VERTEX_POINT ( 'NONE', #63159 ) ;
#21521 = CARTESIAN_POINT ( 'NONE',  ( -18.71221083172660116, 1488.018745540989812, 229.0186356013300042 ) ) ;
#21522 = CARTESIAN_POINT ( 'NONE',  ( 7.818221670759999853, 1367.736483592530021, 207.6218459616989946 ) ) ;
#21523 = CARTESIAN_POINT ( 'NONE',  ( -15.26434951740000123, 1488.814055421730018, 194.3933819335980218 ) ) ;
#21524 = DIRECTION ( 'NONE',  ( -1.971756091734232514E-14, 0.9876883405951697448, 0.1564344650400280867 ) ) ;
#21525 = CARTESIAN_POINT ( 'NONE',  ( 2.488360629304999794, 1516.616791731099966, 214.8929950451170043 ) ) ;
#21526 = CARTESIAN_POINT ( 'NONE',  ( -12.58290190409640097, 1379.610136253339988, 209.8104529657169905 ) ) ;
#21527 = ORIENTED_EDGE ( 'NONE', *, *, #11724, .T. ) ;
#21528 = CARTESIAN_POINT ( 'NONE',  ( -17.39923563954690167, 1508.493391337249932, 212.6342160743549812 ) ) ;
#21529 = DIRECTION ( 'NONE',  ( -1.755985294532469921E-16, 1.000000000000000000, -1.338183447452831989E-16 ) ) ;
#21530 = CARTESIAN_POINT ( 'NONE',  ( -59.84652512769999788, 1378.966454954579831, 258.3077303883590048 ) ) ;
#21531 = CARTESIAN_POINT ( 'NONE',  ( 16.25813024210000179, 1415.087797054229895, 214.9303854824879920 ) ) ;
#21532 = CARTESIAN_POINT ( 'NONE',  ( 2.285487581364999965, 1517.001127920769704, 205.0775242521070254 ) ) ;
#21533 = VERTEX_POINT ( 'NONE', #19441 ) ;
#21534 = AXIS2_PLACEMENT_3D ( 'NONE', #29701, #39195, #2884 ) ;
#21535 = DIRECTION ( 'NONE',  ( 0.000000000000000000, 1.000000000000000000, 0.000000000000000000 ) ) ;
#21536 = EDGE_CURVE ( 'NONE', #68701, #97416, #36812, .T. ) ;
#21537 = B_SPLINE_SURFACE_WITH_KNOTS ( 'NONE', 5, 5, ( 
 ( #107591, #65056, #29780, #40382, #81826, #82936 ),
 ( #82400, #55015, #39841, #21354, #5129, #63968 ),
 ( #47151, #89686, #14068, #89142, #64517, #80748 ),
 ( #74004, #90785, #47698, #5696, #48257, #98083 ),
 ( #99169, #56097, #13510, #14627, #108136, #72363 ),
 ( #4057, #57220, #30328, #12968, #12428, #81276 ) ),
 .UNSPECIFIED., .F., .F., .F.,
 ( 6, 6 ),
 ( 6, 6 ),
 ( 30.58270283670000111, 167.9870597316549947 ),
 ( -0.001304527548221219926, 2.000000001660000137 ),
 .UNSPECIFIED. ) ;
#21538 = CARTESIAN_POINT ( 'NONE',  ( -29.83016982462270050, 1419.452566825586246, 269.4690044093881056 ) ) ;
#21539 = CARTESIAN_POINT ( 'NONE',  ( 6.277682552355000389, 1511.927085655879864, 217.0033795624569848 ) ) ;
#21540 = ADVANCED_FACE ( 'NONE', ( #79373 ), #62612, .F. ) ;
#21542 = EDGE_LOOP ( 'NONE', ( #34998, #18167, #48146, #70745 ) ) ;
#21541 = CARTESIAN_POINT ( 'NONE',  ( -3.294994957250000134, 1408.913060387329779, 191.6318278015979786 ) ) ;
#21543 = FACE_OUTER_BOUND ( 'NONE', #96224, .T. ) ;
#21544 = CARTESIAN_POINT ( 'NONE',  ( -32.50007362375909992, 1440.913060389729935, 245.3806128234339781 ) ) ;
#21545 = CARTESIAN_POINT ( 'NONE',  ( 20.41738288953820302, 1497.614343818499947, 226.1907077604399774 ) ) ;
#21546 = CARTESIAN_POINT ( 'NONE',  ( 21.02430346220000246, 1494.771309273490033, 208.1582823273150211 ) ) ;
#21547 = EDGE_CURVE ( 'NONE', #105727, #15990, #92603, .T. ) ;
#21548 = CARTESIAN_POINT ( 'NONE',  ( 19.98018488065979881, 1413.700872769210036, 269.6585487226739701 ) ) ;
#21550 = CARTESIAN_POINT ( 'NONE',  ( -2.865911554774999814, 1516.906233342200039, 212.5838411289170153 ) ) ;
#21549 = VECTOR ( 'NONE', #63589, 1000.000000000000000 ) ;
#21551 = CARTESIAN_POINT ( 'NONE',  ( -63.94472642409999708, 1379.737898519059854, 270.3073122244590536 ) ) ;
#21552 = B_SPLINE_CURVE_WITH_KNOTS ( 'NONE', 3,
 ( #68406, #6806, #15194, #49385 ),
 .UNSPECIFIED., .F., .F.,
 ( 4, 4 ),
 ( 0.000000000000000000, 0.0008471112791177455191 ),
 .UNSPECIFIED. ) ;
#21553 = EDGE_CURVE ( 'NONE', #72498, #102504, #87260, .T. ) ;
#21554 = CARTESIAN_POINT ( 'NONE',  ( 23.66726145979999885, 1411.111568590429897, 207.8869370808679946 ) ) ;
#21555 = CARTESIAN_POINT ( 'NONE',  ( 28.49879435371743241, 1526.382868173645875, 198.4011524119004264 ) ) ;
#21556 = CARTESIAN_POINT ( 'NONE',  ( -30.04668324475537844, 1524.739563915923100, 222.3144186811225609 ) ) ;
#21557 = CARTESIAN_POINT ( 'NONE',  ( -7.716338871780399344, 1516.813354641049955, 209.5384311660010042 ) ) ;
#21558 =( BOUNDED_CURVE ( )  B_SPLINE_CURVE ( 3, ( #77063, #101127, #58609, #68132 ),
 .UNSPECIFIED., .F., .F. ) 
 B_SPLINE_CURVE_WITH_KNOTS ( ( 4, 4 ),
 ( 4.700155481640241106, 5.195524193123958412 ),
 .UNSPECIFIED. ) 
 CURVE ( )  GEOMETRIC_REPRESENTATION_ITEM ( )  RATIONAL_B_SPLINE_CURVE ( ( 1.000000000000000000, 0.9796551486682428811, 0.9796551486682428811, 1.000000000000000000 ) ) 
 REPRESENTATION_ITEM ( '' )  );
#21559 = CARTESIAN_POINT ( 'NONE',  ( -3.449647478144999724, 1516.829948096479939, 209.8791439064560223 ) ) ;
#21560 = CARTESIAN_POINT ( 'NONE',  ( 4.261788892647819793, 1421.884621400550031, 184.2422145791730088 ) ) ;
#21561 = CARTESIAN_POINT ( 'NONE',  ( -4.154905845549999199, 1420.446155431829993, 232.6175161300979823 ) ) ;
#21562 = CARTESIAN_POINT ( 'NONE',  ( -89.64944567690000099, 1384.853425860309926, 308.7505802988590062 ) ) ;
#21563 = EDGE_LOOP ( 'NONE', ( #70873, #35824, #29953, #95496 ) ) ;
#21564 = CARTESIAN_POINT ( 'NONE',  ( -23.38007145301870082, 1385.262645945500026, 222.6269832384300003 ) ) ;
#21565 = CARTESIAN_POINT ( 'NONE',  ( 18.79734781009999978, 1416.844618635330107, 209.8348600162860009 ) ) ;
#21566 = CARTESIAN_POINT ( 'NONE',  ( -9.094494643104590992, 1384.946982382309898, 199.9428547751310248 ) ) ;
#21567 = CIRCLE ( 'NONE', #35911, 1.999999999999999556 ) ;
#21568 = CARTESIAN_POINT ( 'NONE',  ( -20.58241196329150213, 1507.840856726199945, 228.3121576391399685 ) ) ;
#21569 = CARTESIAN_POINT ( 'NONE',  ( 4.900006679340000559, 1499.255191946190052, 229.7873568473989963 ) ) ;
#21570 = CARTESIAN_POINT ( 'NONE',  ( 11.23526700939999934, 1422.470850597359913, 204.4982669692790012 ) ) ;
#21571 = DIRECTION ( 'NONE',  ( 1.988618688120850357E-13, 0.03085824620771311644, -0.9995237709234254808 ) ) ;
#21572 = VECTOR ( 'NONE', #55002, 1000.000000000000227 ) ;
#21574 = CARTESIAN_POINT ( 'NONE',  ( -15.98206112875141827, 1416.141927088484408, 209.1311918923094879 ) ) ;
#21573 = CARTESIAN_POINT ( 'NONE',  ( 7.330554133425000174, 1516.857992118400034, 216.4511490482170188 ) ) ;
#21575 = CARTESIAN_POINT ( 'NONE',  ( -25.42178969536794142, 1450.805819428513587, 137.2829917403189484 ) ) ;
#21576 = CARTESIAN_POINT ( 'NONE',  ( 10.10258394918160008, 1469.588079192369833, 207.6910948265980039 ) ) ;
#21577 = ORIENTED_EDGE ( 'NONE', *, *, #28927, .T. ) ;
#21578 = CARTESIAN_POINT ( 'NONE',  ( 7.329303077985000137, 1516.857992118400034, 201.7912917986770083 ) ) ;
#21579 = EDGE_CURVE ( 'NONE', #54902, #10255, #71029, .T. ) ;
#21580 = CARTESIAN_POINT ( 'NONE',  ( -13.58245605311162763, 1416.835806623488907, 221.9090835327766627 ) ) ;
#21581 = ORIENTED_EDGE ( 'NONE', *, *, #58489, .T. ) ;
#21582 = FACE_OUTER_BOUND ( 'NONE', #102790, .T. ) ;
#21583 = CARTESIAN_POINT ( 'NONE',  ( 10.64609503708443050, 1434.773768202574502, 152.0346824635861935 ) ) ;
#21584 = EDGE_CURVE ( 'NONE', #6924, #22249, #54632, .T. ) ;
#21585 = CARTESIAN_POINT ( 'NONE',  ( 7.972851048953825348, 1423.800244593099478, 195.8527174153489057 ) ) ;
#21586 =( BOUNDED_CURVE ( )  B_SPLINE_CURVE ( 3, ( #96070, #28321, #19904, #88234 ),
 .UNSPECIFIED., .F., .T. ) 
 B_SPLINE_CURVE_WITH_KNOTS ( ( 4, 4 ),
 ( 1.102258161761371813, 1.468409620127669957 ),
 .UNSPECIFIED. ) 
 CURVE ( )  GEOMETRIC_REPRESENTATION_ITEM ( )  RATIONAL_B_SPLINE_CURVE ( ( 1.000000000000000000, 0.9888589290277138844, 0.9888589290277138844, 1.000000000000000000 ) ) 
 REPRESENTATION_ITEM ( '' )  );
#21587 = CARTESIAN_POINT ( 'NONE',  ( 2.539157280710000020, 1443.442079612289945, 217.6697438749490061 ) ) ;
#21588 = CARTESIAN_POINT ( 'NONE',  ( -27.55471748229280138, 1509.768035665449815, 201.0693058872570020 ) ) ;
#21589 = AXIS2_PLACEMENT_3D ( 'NONE', #28793, #86476, #43937 ) ;
#21590 = CARTESIAN_POINT ( 'NONE',  ( 18.99535453092520143, 1472.738766242029897, 202.2605984988649936 ) ) ;
#21591 = CARTESIAN_POINT ( 'NONE',  ( -18.69805756450000089, 1425.031978227930040, 224.7610688237980128 ) ) ;
#21592 = CARTESIAN_POINT ( 'NONE',  ( 6.460996930076231770, 1486.649525340193122, 200.4524504349261633 ) ) ;
#21593 = CARTESIAN_POINT ( 'NONE',  ( -104.1991395359999899, 1389.999248167110181, 304.1793320542590209 ) ) ;
#21594 = CARTESIAN_POINT ( 'NONE',  ( 19.08482065080000112, 1478.519531283130164, 189.9637900503979893 ) ) ;
#21596 = CARTESIAN_POINT ( 'NONE',  ( -17.31582335683077645, 1433.702428048472257, 216.7375878835501339 ) ) ;
#21595 = CARTESIAN_POINT ( 'NONE',  ( -106.1577607520000015, 1391.913060387289988, 304.2026179676590232 ) ) ;
#21597 = CARTESIAN_POINT ( 'NONE',  ( -0.09453244570555620341, 1457.861743394589894, 229.1248241851770047 ) ) ;
#21598 = ORIENTED_EDGE ( 'NONE', *, *, #49371, .F. ) ;
#21599 = CARTESIAN_POINT ( 'NONE',  ( -105.0207718979999925, 1379.360663349339802, 304.0316769014589795 ) ) ;
#21600 = CARTESIAN_POINT ( 'NONE',  ( -14.42661198839999948, 1508.520312169789804, 215.9309591648589901 ) ) ;
#21601 = DIRECTION ( 'NONE',  ( 0.9455185755993182894, 0.000000000000000000, -0.3255681544571521480 ) ) ;
#21602 = CARTESIAN_POINT ( 'NONE',  ( 11.13973213087689906, 1470.272412021129867, 206.9146623043149873 ) ) ;
#21603 = DIRECTION ( 'NONE',  ( -0.2130860312228880504, 0.04225590415439329367, 0.9761192457183565097 ) ) ;
#21604 = CARTESIAN_POINT ( 'NONE',  ( -18.64061453619999753, 1509.327891199630130, 230.4796374886979891 ) ) ;
#21605 = CARTESIAN_POINT ( 'NONE',  ( -2.622430729443003816, 1523.621879633029039, 242.1535192357228254 ) ) ;
#21606 = CARTESIAN_POINT ( 'NONE',  ( -13.48891322911904922, 1444.164948460842197, 187.0585711215786091 ) ) ;
#21607 = CARTESIAN_POINT ( 'NONE',  ( -17.40764061960000220, 1414.996442553730049, 207.5654756531779697 ) ) ;
#21608 = CARTESIAN_POINT ( 'NONE',  ( 3.746245303161040319, 1495.153263702249888, 220.4845792887770131 ) ) ;
#21609 = CARTESIAN_POINT ( 'NONE',  ( -5.586162938070000195, 1491.245995699590139, 185.8699225748990216 ) ) ;
#21610 = CARTESIAN_POINT ( 'NONE',  ( -1.906499846882070084E-08, 1516.801704408389924, 209.1218459511669892 ) ) ;
#21611 = CARTESIAN_POINT ( 'NONE',  ( 0.4346943641293429805, 1517.051704428850144, 201.3992661435559910 ) ) ;
#21613 = VERTEX_POINT ( 'NONE', #100560 ) ;
#21612 = CARTESIAN_POINT ( 'NONE',  ( 13.77266209894789917, 1522.051704408389924, 201.2043266506040027 ) ) ;
#21614 = CARTESIAN_POINT ( 'NONE',  ( -106.5131656470000081, 1380.118154394319845, 307.6054082156589971 ) ) ;
#21615 = CARTESIAN_POINT ( 'NONE',  ( 13.96132452455360173, 1513.058738973300024, 224.4023983419680235 ) ) ;
#21616 = VERTEX_POINT ( 'NONE', #83768 ) ;
#21617 = ORIENTED_EDGE ( 'NONE', *, *, #50118, .F. ) ;
#21618 = DIRECTION ( 'NONE',  ( -0.1070030146457234405, 0.000000000000000000, 0.9942586961433764747 ) ) ;
#21619 = CARTESIAN_POINT ( 'NONE',  ( -110.0632502760000051, 1384.922727919980161, 296.9512166178590178 ) ) ;
#21620 = CARTESIAN_POINT ( 'NONE',  ( -8.999250544063707835, 1381.632011801812951, 200.5706445290884972 ) ) ;
#21622 = CARTESIAN_POINT ( 'NONE',  ( -27.17992432010000314, 1457.024587825630078, 248.2870168934979915 ) ) ;
#21621 = CARTESIAN_POINT ( 'NONE',  ( 37.67883452730400506, 1427.401834259486805, 269.5711273142176765 ) ) ;
#21623 = CARTESIAN_POINT ( 'NONE',  ( 9.756688738945658912, 1436.057734518939924, 210.3833036739349893 ) ) ;
#21624 = CARTESIAN_POINT ( 'NONE',  ( -11.93743581870000092, 1433.478165980000085, 150.0011823557980222 ) ) ;
#21625 = DIRECTION ( 'NONE',  ( 1.989737444810000148E-13, 6.825857443600000379E-15, -1.000000000000000000 ) ) ;
#21626 = CARTESIAN_POINT ( 'NONE',  ( 11.67392614361510006, 1426.737874814250063, 139.6575252623269989 ) ) ;
#21627 = DIRECTION ( 'NONE',  ( 0.000000000000000000, 0.000000000000000000, -1.000000000000000000 ) ) ;
#21628 = CARTESIAN_POINT ( 'NONE',  ( -26.48225558509999900, 1437.467569122950181, 136.8764125097979729 ) ) ;
#21629 = CARTESIAN_POINT ( 'NONE',  ( 1.324264359491340137, 1515.084669001950033, 213.4507742627420157 ) ) ;
#21630 = CARTESIAN_POINT ( 'NONE',  ( 17.02668221408760019, 1422.112876149069962, 226.8213126862850118 ) ) ;
#21631 = CARTESIAN_POINT ( 'NONE',  ( -10.12731387375120029, 1479.682647925139918, 215.0256783668529863 ) ) ;
#21632 = AXIS2_PLACEMENT_3D ( 'NONE', #110085, #42890, #42328 ) ;
#21633 = CARTESIAN_POINT ( 'NONE',  ( 4.262353028419999745, 1360.811275533920025, 207.6218459616989946 ) ) ;
#21634 = CARTESIAN_POINT ( 'NONE',  ( -18.80593852474190797, 1509.688961265932903, 232.5129852480815487 ) ) ;
#21636 = ORIENTED_EDGE ( 'NONE', *, *, #15782, .T. ) ;
#21635 = CARTESIAN_POINT ( 'NONE',  ( 5.455728723259139821E-10, 1411.010528177349897, 256.1339838009660070 ) ) ;
#21637 = ORIENTED_EDGE ( 'NONE', *, *, #108527, .F. ) ;
#21638 = CARTESIAN_POINT ( 'NONE',  ( -11.79691506120000000, 1504.510891942089984, 208.2439356722240120 ) ) ;
#21639 = CARTESIAN_POINT ( 'NONE',  ( -5.695425083339999972, 1491.838932079990172, 185.8634046642990256 ) ) ;
#21640 = CARTESIAN_POINT ( 'NONE',  ( -33.87346585150000067, 1461.272374640529961, 270.3444747636979741 ) ) ;
#21641 = CARTESIAN_POINT ( 'NONE',  ( 7.854071199910000800, 1421.721864916329878, 195.9105866898989916 ) ) ;
#21642 = CARTESIAN_POINT ( 'NONE',  ( -9.992007221630000153E-16, 1432.353292893639946, 155.3998094795979910 ) ) ;
#21643 = CARTESIAN_POINT ( 'NONE',  ( 34.60209068530420495, 1451.703683649660206, 135.1317529420850292 ) ) ;
#21644 = CARTESIAN_POINT ( 'NONE',  ( 0.2153768123770790077, 1452.918741419729940, 183.2557861667889938 ) ) ;
#21645 = CARTESIAN_POINT ( 'NONE',  ( 4.099884065022929569, 1484.480468068710024, 220.2376187541709953 ) ) ;
#21646 = CARTESIAN_POINT ( 'NONE',  ( 3.931910744533549718, 1448.296755838050103, 184.2998928686550073 ) ) ;
#21647 = CARTESIAN_POINT ( 'NONE',  ( -5.637866616400000197, 1457.357056849289847, 216.8187349542390052 ) ) ;
#21648 = CARTESIAN_POINT ( 'NONE',  ( 7.622608667027140683, 1359.902596381179819, 208.3718459617010978 ) ) ;
#21649 = CARTESIAN_POINT ( 'NONE',  ( -39.91655809679639333, 1422.699949167599925, 267.8112314109329759 ) ) ;
#21650 = ORIENTED_EDGE ( 'NONE', *, *, #41252, .T. ) ;
#21651 = CARTESIAN_POINT ( 'NONE',  ( -3.530576738627919653, 1489.241048346600110, 181.7384218624920038 ) ) ;
#21652 = ORIENTED_EDGE ( 'NONE', *, *, #30125, .F. ) ;
#21653 = EDGE_LOOP ( 'NONE', ( #18726, #24658, #109328, #45806 ) ) ;
#21654 = CARTESIAN_POINT ( 'NONE',  ( 3.269984781304999810, 1516.999105586269934, 210.8242519552970009 ) ) ;
#21655 = CARTESIAN_POINT ( 'NONE',  ( -8.557209110492459914, 1448.617779613390212, 212.3361752075699940 ) ) ;
#21657 = SURFACE_STYLE_USAGE ( .BOTH. , #98386 ) ;
#21656 = CARTESIAN_POINT ( 'NONE',  ( 5.786837678925000006, 1517.040132827679827, 212.3790665729270017 ) ) ;
#21658 = CARTESIAN_POINT ( 'NONE',  ( -12.33247831520000126, 1440.430499810650190, 187.9573111595979924 ) ) ;
#21659 = CARTESIAN_POINT ( 'NONE',  ( -17.92792478850000037, 1415.296882282229944, 208.1699612212720183 ) ) ;
#21660 = ORIENTED_EDGE ( 'NONE', *, *, #103789, .F. ) ;
#21661 = CARTESIAN_POINT ( 'NONE',  ( -26.34468263449999981, 1436.394472913030086, 136.7595242481980051 ) ) ;
#21662 = CARTESIAN_POINT ( 'NONE',  ( -0.01073133209419849937, 1516.939491476980038, 201.7897819926569980 ) ) ;
#21663 = VECTOR ( 'NONE', #77505, 1000.000000000000000 ) ;
#21664 = ADVANCED_FACE ( 'NONE', ( #58032 ), #92711, .F. ) ;
#21665 = CARTESIAN_POINT ( 'NONE',  ( -30.51231035492510557, 1524.382868172863937, 218.1578534183722979 ) ) ;
#21666 = CARTESIAN_POINT ( 'NONE',  ( 1.177525951771697388, 1508.992568668472586, 238.7712217697011852 ) ) ;
#21667 = VECTOR ( 'NONE', #98996, 1000.000000000000114 ) ;
#21668 = CARTESIAN_POINT ( 'NONE',  ( -43.48935866962139585, 1430.236520443860172, 269.7109362569590303 ) ) ;
#21669 = CARTESIAN_POINT ( 'NONE',  ( -0.7772817352909999755, 1427.305457135430061, 123.0297916884979941 ) ) ;
#21670 = CARTESIAN_POINT ( 'NONE',  ( -5.343479798080000620, 1396.099658813630185, 199.4684377197879996 ) ) ;
#21672 = ORIENTED_EDGE ( 'NONE', *, *, #20626, .F. ) ;
#21671 = CARTESIAN_POINT ( 'NONE',  ( -9.516636888345459511, 1366.309137899877896, 210.6218459616987957 ) ) ;
#21673 = ORIENTED_EDGE ( 'NONE', *, *, #105511, .F. ) ;
#21674 = CARTESIAN_POINT ( 'NONE',  ( 45.62303547458256503, 1441.762580339629494, 268.9751351163830577 ) ) ;
#21675 = CARTESIAN_POINT ( 'NONE',  ( -2.311558444226220033, 1425.028861818389942, 191.2692960788320136 ) ) ;
#21676 = CARTESIAN_POINT ( 'NONE',  ( -14.18979468069059990, 1436.254652937099763, 150.1235830601330008 ) ) ;
#21677 = LINE ( 'NONE', #22773, #82980 ) ;
#21678 = CARTESIAN_POINT ( 'NONE',  ( 0.7579262867720020225, 1516.927039499179955, 210.8260166843570005 ) ) ;
#21679 = CARTESIAN_POINT ( 'NONE',  ( -21.40977040799994668, 1506.404057888697707, 214.0392949286786859 ) ) ;
#21680 = CARTESIAN_POINT ( 'NONE',  ( -18.58859720539999927, 1430.796697030029918, 225.4129132132979692 ) ) ;
#21681 = EDGE_CURVE ( 'NONE', #88376, #32787, #110623, .T. ) ;
#21682 = CARTESIAN_POINT ( 'NONE',  ( 10.65073847843230048, 1475.392797246900045, 267.2046423057439597 ) ) ;
#21683 = CARTESIAN_POINT ( 'NONE',  ( 12.65530650809999891, 1416.254459046630018, 223.0920568362980134 ) ) ;
#21684 = CARTESIAN_POINT ( 'NONE',  ( 7.618992673874999788, 1511.297452611750032, 205.9539561133169911 ) ) ;
#21685 = CARTESIAN_POINT ( 'NONE',  ( -3.462620856235000044, 1516.938330505699923, 206.6435391121569864 ) ) ;
#21686 = ORIENTED_EDGE ( 'NONE', *, *, #74031, .F. ) ;
#21687 = CARTESIAN_POINT ( 'NONE',  ( -36.37832866295150325, 1435.767865547330075, 135.6928026007940105 ) ) ;
#21688 = CARTESIAN_POINT ( 'NONE',  ( -0.9370951672101170971, 1516.671995221562156, 201.6725580799513011 ) ) ;
#21689 = ORIENTED_EDGE ( 'NONE', *, *, #72159, .F. ) ;
#21690 = CARTESIAN_POINT ( 'NONE',  ( 3.727901463303194163, 1457.491499694037429, 228.5408078901032525 ) ) ;
#21692 = EDGE_CURVE ( 'NONE', #65489, #23415, #15988, .T. ) ;
#21691 = CARTESIAN_POINT ( 'NONE',  ( 25.25202363594589983, 1450.803879461809856, 137.6136435803179836 ) ) ;
#21693 = CARTESIAN_POINT ( 'NONE',  ( 2.689344463419570452, 1464.716346866380036, 236.9361821190090041 ) ) ;
#21694 = CARTESIAN_POINT ( 'NONE',  ( -16.82269271239999853, 1418.343879150699877, 203.5371288789889945 ) ) ;
#21695 = CARTESIAN_POINT ( 'NONE',  ( 20.63995201750000064, 1409.633823394030060, 203.6085390534680073 ) ) ;
#21696 = CARTESIAN_POINT ( 'NONE',  ( -3.873467979927594396, 1446.300338454377652, 170.5362326176377508 ) ) ;
#21697 = CARTESIAN_POINT ( 'NONE',  ( -24.89775034519999863, 1442.835538705840008, 210.5176537872779932 ) ) ;
#21698 = DIRECTION ( 'NONE',  ( -0.6736849260149578855, 0.000000000000000000, 0.7390186874905266823 ) ) ;
#21699 = CARTESIAN_POINT ( 'NONE',  ( 30.61115703707575264, 1523.542365884046148, 221.8239785241844686 ) ) ;
#21700 = CARTESIAN_POINT ( 'NONE',  ( 24.11105221579398616, 1446.721418104631312, 214.9938192866167697 ) ) ;
#21701 = CARTESIAN_POINT ( 'NONE',  ( 2.500000000000000000, 1439.495310474650068, 163.5954646090490030 ) ) ;
#21702 = CARTESIAN_POINT ( 'NONE',  ( 4.037378256055000669, 1516.688761843659904, 215.6706679112870120 ) ) ;
#21703 = ORIENTED_EDGE ( 'NONE', *, *, #42673, .T. ) ;
#21704 = CARTESIAN_POINT ( 'NONE',  ( 7.712858129429029930, 1516.680429148250141, 208.2106503431979831 ) ) ;
#21705 = CARTESIAN_POINT ( 'NONE',  ( -4.878146142590000345, 1474.403035727189945, 198.7818668649990173 ) ) ;
#21706 = CARTESIAN_POINT ( 'NONE',  ( 34.18677586421181758, 1512.187213306747481, 198.4504086008745389 ) ) ;
#21707 = CARTESIAN_POINT ( 'NONE',  ( -2.809892567274479891, 1422.122748121970062, 101.6305808166549980 ) ) ;
#21708 = CARTESIAN_POINT ( 'NONE',  ( -38.94952215260590123, 1447.803421510810040, 136.5227995632060072 ) ) ;
#21709 = EDGE_CURVE ( 'NONE', #110516, #345, #30600, .T. ) ;
#21710 = DIRECTION ( 'NONE',  ( -0.001619481660810790291, -0.06184550950385309803, 0.9980844203940660853 ) ) ;
#21711 = CARTESIAN_POINT ( 'NONE',  ( 1.982459036158376930, 1417.212962208210001, 233.0589578014529479 ) ) ;
#21712 = CARTESIAN_POINT ( 'NONE',  ( -2.500000000000000000, 1422.798905948130141, 153.2868469301980099 ) ) ;
#21713 = CARTESIAN_POINT ( 'NONE',  ( -109.1677958815039915, 1385.012782240220076, 297.1338810903739613 ) ) ;
#21714 = CARTESIAN_POINT ( 'NONE',  ( -4.829762623019999701, 1474.871956953530116, 269.6371214077980198 ) ) ;
#21715 = CARTESIAN_POINT ( 'NONE',  ( 30.42008586110589974, 1440.913060385229983, 239.6619397494469865 ) ) ;
#21716 = CARTESIAN_POINT ( 'NONE',  ( -10.19612387162210076, 1470.689520798050125, 211.8176239230739952 ) ) ;
#21717 = FACE_OUTER_BOUND ( 'NONE', #33987, .T. ) ;
#21718 = ORIENTED_EDGE ( 'NONE', *, *, #74781, .T. ) ;
#21719 = VERTEX_POINT ( 'NONE', #25494 ) ;
#21720 = CARTESIAN_POINT ( 'NONE',  ( 11.77531401088269902, 1479.418202641479866, 208.9148487659819864 ) ) ;
#21721 = CARTESIAN_POINT ( 'NONE',  ( -19.07182359474698075, 1485.494300952754202, 189.6180619917788590 ) ) ;
#21722 = VECTOR ( 'NONE', #7192, 1000.000000000000000 ) ;
#21723 = CARTESIAN_POINT ( 'NONE',  ( -1.355725730386620587, 1410.152070539702208, 185.6110041341284216 ) ) ;
#21724 = CARTESIAN_POINT ( 'NONE',  ( 2.892637806539999801, 1499.013587024830031, 235.5840335634979965 ) ) ;
#21725 = CARTESIAN_POINT ( 'NONE',  ( -10.77132304329999890, 1491.639218371489960, 211.5210277313490224 ) ) ;
#21726 = CARTESIAN_POINT ( 'NONE',  ( -1.899216484965220220, 1508.551704408389924, 220.0743039580760012 ) ) ;
#21727 = CARTESIAN_POINT ( 'NONE',  ( -44.28647047321589980, 1383.821342991460142, 249.7482539287410077 ) ) ;
#21728 = CARTESIAN_POINT ( 'NONE',  ( -18.92738908012519872, 1503.346139213670085, 222.1981866595989743 ) ) ;
#21729 = CARTESIAN_POINT ( 'NONE',  ( -12.45702678070000147, 1416.837177098230086, 194.7670154063979737 ) ) ;
#21730 = CARTESIAN_POINT ( 'NONE',  ( -11.90000415720300175, 1434.913060496859998, 147.6452464505769910 ) ) ;
#21731 = CARTESIAN_POINT ( 'NONE',  ( 2.623456343980000049, 1464.614364364229914, 236.5050914573980094 ) ) ;
#21733 = ORIENTED_EDGE ( 'NONE', *, *, #89320, .F. ) ;
#21732 = CARTESIAN_POINT ( 'NONE',  ( -11.14671771210699980, 1434.019356486030119, 151.6529807626459956 ) ) ;
#21734 = CARTESIAN_POINT ( 'NONE',  ( -0.3166280363130000164, 1452.331784132529947, 183.2228567541980055 ) ) ;
#21735 = AXIS2_PLACEMENT_3D ( 'NONE', #102682, #70260, #78061 ) ;
#21736 = CARTESIAN_POINT ( 'NONE',  ( -34.14316623799999917, 1378.983883636150040, 218.5549180040089823 ) ) ;
#21737 = CARTESIAN_POINT ( 'NONE',  ( 3.930410875824919881, 1508.551704408389924, 204.5918276205729853 ) ) ;
#21739 = ORIENTED_EDGE ( 'NONE', *, *, #38495, .F. ) ;
#21738 = CARTESIAN_POINT ( 'NONE',  ( -31.54873523817366632, 1525.317349363549965, 216.6695393792268192 ) ) ;
#21740 = CARTESIAN_POINT ( 'NONE',  ( 0.5708410311183980124, 1460.784089514889729, 230.4191078033510109 ) ) ;
#21741 = ORIENTED_EDGE ( 'NONE', *, *, #89320, .T. ) ;
#21742 = CARTESIAN_POINT ( 'NONE',  ( -10.78513347949999890, 1390.743336494430196, 215.1699270643190118 ) ) ;
#21743 = CARTESIAN_POINT ( 'NONE',  ( 2.174856522119999802, 1490.282954593489876, 188.3516094669990082 ) ) ;
#21744 = CARTESIAN_POINT ( 'NONE',  ( 8.515581525185790923, 1522.051704408389924, 191.3277396192498543 ) ) ;
#21745 = CARTESIAN_POINT ( 'NONE',  ( 8.266917622984580660, 1505.524528093398885, 217.3397827525526509 ) ) ;
#21746 = LINE ( 'NONE', #55948, #53564 ) ;
#21747 = DIRECTION ( 'NONE',  ( -0.8775825618903733139, -0.000000000000000000, -0.4794255386042020062 ) ) ;
#21748 = CARTESIAN_POINT ( 'NONE',  ( 11.27697011000779881, 1409.306860861120185, 199.3051403546259905 ) ) ;
#21749 = CARTESIAN_POINT ( 'NONE',  ( 2.745142294599053567, 1419.769955103634175, 137.0999999980979567 ) ) ;
#21750 = DIRECTION ( 'NONE',  ( -0.6736849260863839728, 0.000000000000000000, 0.7390186874254150995 ) ) ;
#21751 = CARTESIAN_POINT ( 'NONE',  ( 18.70459388984919968, 1509.566239199539950, 186.5372755781170042 ) ) ;
#21752 = CARTESIAN_POINT ( 'NONE',  ( 11.57603212340000098, 1432.304338796609954, 151.1967213793979852 ) ) ;
#21753 = AXIS2_PLACEMENT_3D ( 'NONE', #101710, #6022, #23364 ) ;
#21754 = DIRECTION ( 'NONE',  ( 0.8644545129124839855, 0.5024715467361959842, 0.01551579278589970169 ) ) ;
#21755 = ORIENTED_EDGE ( 'NONE', *, *, #66480, .F. ) ;
#21756 = ORIENTED_EDGE ( 'NONE', *, *, #60512, .T. ) ;
#21757 = CARTESIAN_POINT ( 'NONE',  ( 17.44374831407513682, 1524.130440953581001, 237.5220222273273976 ) ) ;
#21758 = CARTESIAN_POINT ( 'NONE',  ( -11.70773956410279837, 1415.348334734199852, 195.2149244325059954 ) ) ;
#21759 = VECTOR ( 'NONE', #36534, 1000.000000000000000 ) ;
#21760 = CARTESIAN_POINT ( 'NONE',  ( -12.91587818989999903, 1435.175565185170171, 150.4504693756979918 ) ) ;
#21761 = CARTESIAN_POINT ( 'NONE',  ( 12.78079900903480137, 1420.829302377369913, 202.2958744884179794 ) ) ;
#21762 = CARTESIAN_POINT ( 'NONE',  ( -20.06702669026240216, 1490.601403728770038, 190.8896936984549768 ) ) ;
#21763 = CARTESIAN_POINT ( 'NONE',  ( -14.80319198780000001, 1420.559702942450031, 212.4542102459990076 ) ) ;
#21764 = CARTESIAN_POINT ( 'NONE',  ( -109.9471644529999992, 1385.741605226209913, 311.4145034772590179 ) ) ;
#21765 = CARTESIAN_POINT ( 'NONE',  ( -8.790528956024720841, 1511.742084109019970, 215.3764313309009992 ) ) ;
#21766 = CARTESIAN_POINT ( 'NONE',  ( -11.55751048842087059, 1366.520570492055640, 208.3718459617010978 ) ) ;
#21767 = CARTESIAN_POINT ( 'NONE',  ( -46.02767451640849572, 1440.466588444049876, 268.4960630891500273 ) ) ;
#21768 = CARTESIAN_POINT ( 'NONE',  ( -20.73258660329999614, 1507.783934695429934, 191.7300198070979889 ) ) ;
#21769 = CARTESIAN_POINT ( 'NONE',  ( 7.321169230994999388, 1516.531533746980131, 207.4131249475269954 ) ) ;
#21770 = CARTESIAN_POINT ( 'NONE',  ( -9.065759682986140433, 1448.140860388920146, 211.0596819856369848 ) ) ;
#21771 = CARTESIAN_POINT ( 'NONE',  ( 5.257336836053539741, 1408.563318105239887, 221.6654867046719914 ) ) ;
#21772 = CARTESIAN_POINT ( 'NONE',  ( -13.84829814514429991, 1435.980421560989953, 150.2434240975769910 ) ) ;
#21773 = CARTESIAN_POINT ( 'NONE',  ( -8.021176654290000485, 1385.031491206999817, 218.7854548825889935 ) ) ;
#21774 = CARTESIAN_POINT ( 'NONE',  ( 1.121268454170000206, 1416.831305841230005, 190.1585927629979835 ) ) ;
#21775 = CARTESIAN_POINT ( 'NONE',  ( 7.433591009027219698, 1425.184177341129953, 212.3839561552370014 ) ) ;
#21776 = CARTESIAN_POINT ( 'NONE',  ( -7.548339362227099336, 1493.934769483920036, 206.2816082653209833 ) ) ;
#21777 = VERTEX_POINT ( 'NONE', #59684 ) ;
#21778 = CARTESIAN_POINT ( 'NONE',  ( 25.82475784460000057, 1425.523015328830070, 244.3435519239979783 ) ) ;
#21779 = CARTESIAN_POINT ( 'NONE',  ( -28.30919303690000177, 1508.136605795629976, 209.2395761310839930 ) ) ;
#21781 = CARTESIAN_POINT ( 'NONE',  ( 13.58235846979999906, 1416.828040475229955, 196.3349388281980055 ) ) ;
#21780 = CARTESIAN_POINT ( 'NONE',  ( -1.528188101399999832, 1489.032157980530201, 181.5697705370980088 ) ) ;
#21782 = B_SPLINE_CURVE_WITH_KNOTS ( 'NONE', 3,
 ( #5986, #22753, #58059, #40689 ),
 .UNSPECIFIED., .F., .F.,
 ( 4, 4 ),
 ( -0.005718497747916959605, -1.599190933582878005E-07 ),
 .UNSPECIFIED. ) ;
#21783 = CARTESIAN_POINT ( 'NONE',  ( 1.448679645196929933, 1507.129709964000085, 181.1126013477120011 ) ) ;
#21784 = CARTESIAN_POINT ( 'NONE',  ( -11.09767598430000035, 1423.160780147529977, 216.2628275680980039 ) ) ;
#21785 = CARTESIAN_POINT ( 'NONE',  ( -0.9121791906100019665, 1486.347595431690024, 220.6238279289989919 ) ) ;
#21786 = CARTESIAN_POINT ( 'NONE',  ( -5.277973487429999722, 1391.913060387289988, 214.4789392792089870 ) ) ;
#21787 = CARTESIAN_POINT ( 'NONE',  ( 27.42695666749999717, 1450.667309086389878, 136.4365165660979926 ) ) ;
#21788 = VERTEX_POINT ( 'NONE', #68645 ) ;
#21789 = CARTESIAN_POINT ( 'NONE',  ( -2.500000000000000000, 1432.183427936470025, 157.4912586936979721 ) ) ;
#21790 = CARTESIAN_POINT ( 'NONE',  ( 12.99084550840746566, 1513.436209034644207, 225.9095066078032801 ) ) ;
#21791 = CARTESIAN_POINT ( 'NONE',  ( 2.958832406229999989, 1509.097160381630147, 238.9948613597979943 ) ) ;
#21792 = B_SPLINE_CURVE_WITH_KNOTS ( 'NONE', 3,
 ( #68225, #32923, #102332, #40784 ),
 .UNSPECIFIED., .F., .F.,
 ( 4, 4 ),
 ( 0.000000000000000000, 0.0002220129587134773411 ),
 .UNSPECIFIED. ) ;
#21793 = ORIENTED_EDGE ( 'NONE', *, *, #25438, .T. ) ;
#21794 = ORIENTED_EDGE ( 'NONE', *, *, #91290, .F. ) ;
#21795 = CARTESIAN_POINT ( 'NONE',  ( -9.852560507769998921, 1384.650985176700033, 199.8802037849889928 ) ) ;
#21796 = CARTESIAN_POINT ( 'NONE',  ( 5.437914377660000298, 1423.457374358000152, 194.5338318222989926 ) ) ;
#21797 = VERTEX_POINT ( 'NONE', #17071 ) ;
#21798 = VECTOR ( 'NONE', #8440, 1000.000000000000000 ) ;
#21799 = CARTESIAN_POINT ( 'NONE',  ( 4.534010743204659910, 1508.610336716400070, 204.8848650279689991 ) ) ;
#21800 = FACE_BOUND ( 'NONE', #101332, .T. ) ;
#21801 = CARTESIAN_POINT ( 'NONE',  ( -4.356169890730000382, 1470.481192091330058, 234.8232070940980236 ) ) ;
#21802 = CARTESIAN_POINT ( 'NONE',  ( 16.73628186595829703, 1526.382868172864164, 234.1845039693042452 ) ) ;
#21803 = VERTEX_POINT ( 'NONE', #51269 ) ;
#21804 = CARTESIAN_POINT ( 'NONE',  ( 11.15483420530000025, 1425.160608745730087, 144.1639996081979973 ) ) ;
#21805 = CARTESIAN_POINT ( 'NONE',  ( -13.01538513870579905, 1416.535698381769862, 221.8985197201349990 ) ) ;
#21806 = CARTESIAN_POINT ( 'NONE',  ( -0.1377404852739999852, 1420.462255397929766, 182.7340595799979894 ) ) ;
#21807 = CARTESIAN_POINT ( 'NONE',  ( -4.038637500854999729, 1516.734985836460055, 203.3481771172569950 ) ) ;
#21808 = ORIENTED_EDGE ( 'NONE', *, *, #62503, .F. ) ;
#21809 = CARTESIAN_POINT ( 'NONE',  ( 11.31504837134619912, 1480.564413193109885, 212.4592244812710078 ) ) ;
#21810 = VECTOR ( 'NONE', #35670, 1000.000000000000000 ) ;
#21811 = CARTESIAN_POINT ( 'NONE',  ( 13.39209664583887260, 1443.386748700186445, 187.8724463653802275 ) ) ;
#21812 = ORIENTED_EDGE ( 'NONE', *, *, #56592, .F. ) ;
#21813 = ORIENTED_EDGE ( 'NONE', *, *, #10991, .T. ) ;
#21814 = CARTESIAN_POINT ( 'NONE',  ( 2.383407846123591689, 1522.906363951597314, 174.9517353176829602 ) ) ;
#21815 = CARTESIAN_POINT ( 'NONE',  ( 4.678155150208202606, 1508.611350403811457, 205.6342600829154321 ) ) ;
#21816 = CARTESIAN_POINT ( 'NONE',  ( 4.552654400296909820, 1499.043495457450035, 198.6118221592419957 ) ) ;
#21817 = CARTESIAN_POINT ( 'NONE',  ( -13.34643008454949964, 1512.594488815709838, 193.8269363163149990 ) ) ;
#21818 = CARTESIAN_POINT ( 'NONE',  ( 20.12564951288285542, 1511.187213306747708, 237.5287294252014192 ) ) ;
#21819 = CARTESIAN_POINT ( 'NONE',  ( 10.47155213350000125, 1420.411604161809919, 197.7872679537989882 ) ) ;
#21820 = CARTESIAN_POINT ( 'NONE',  ( 1.257109029569680070, 1474.977242891490050, 220.4718170348219815 ) ) ;
#21821 = CARTESIAN_POINT ( 'NONE',  ( -7.790472862750560168, 1493.948223036720037, 199.5897708613550208 ) ) ;
#21822 = CARTESIAN_POINT ( 'NONE',  ( -20.06202041079472664, 1509.646782119672707, 231.0063366968753940 ) ) ;
#21823 = DIRECTION ( 'NONE',  ( -0.9993908270190798859, -0.03489949670295298956, 0.000000000000000000 ) ) ;
#21825 = CARTESIAN_POINT ( 'NONE',  ( 16.63654589489999935, 1507.631725798030175, 193.5314252907980119 ) ) ;
#21824 = CARTESIAN_POINT ( 'NONE',  ( 29.95987888842581981, 1525.317359687823455, 196.6841832611087284 ) ) ;
#21826 = CARTESIAN_POINT ( 'NONE',  ( 10.74706036746959903, 1424.980385092369943, 206.5419776234139988 ) ) ;
#21827 = CARTESIAN_POINT ( 'NONE',  ( -24.56184656835360158, 1509.239445071429827, 222.5723712071969942 ) ) ;
#21828 = CARTESIAN_POINT ( 'NONE',  ( 11.00428676220000135, 1425.778354413130046, 91.15517427569778874 ) ) ;
#21829 = ORIENTED_EDGE ( 'NONE', *, *, #62533, .F. ) ;
#21830 = CARTESIAN_POINT ( 'NONE',  ( 6.509745603069999831, 1426.468882613529786, 219.6133830848980040 ) ) ;
#21831 = CIRCLE ( 'NONE', #2234, 0.9999999999999981126 ) ;
#21832 = DIRECTION ( 'NONE',  ( 0.3255681544571567554, 0.000000000000000000, 0.9455185755993167351 ) ) ;
#21833 = CARTESIAN_POINT ( 'NONE',  ( -78.73038605992259420, 1384.997356039029910, 302.9955482565979992 ) ) ;
#21834 = CARTESIAN_POINT ( 'NONE',  ( -9.090173430379998365, 1385.732952333820094, 200.0315116276589720 ) ) ;
#21835 = CARTESIAN_POINT ( 'NONE',  ( -15.37186486470000091, 1415.677402295069896, 210.2490173072590096 ) ) ;
#21837 = VERTEX_POINT ( 'NONE', #85400 ) ;
#21836 = CARTESIAN_POINT ( 'NONE',  ( -17.36663402931900180, 1419.536926980039880, 207.6991980856880105 ) ) ;
#21838 = CARTESIAN_POINT ( 'NONE',  ( 3.554081219399999991, 1430.009957168990013, 217.0886355354290060 ) ) ;
#21839 = B_SPLINE_CURVE_WITH_KNOTS ( 'NONE', 5,
 ( #7558, #66393, #49580, #41712, #108370, #59087 ),
 .UNSPECIFIED., .F., .F.,
 ( 6, 6 ),
 ( 0.000000000000000000, 1.000000000000000000 ),
 .UNSPECIFIED. ) ;
#21840 = CARTESIAN_POINT ( 'NONE',  ( -1.665548205979999974, 1442.756953654919926, 150.7199974615980125 ) ) ;
#21841 = CARTESIAN_POINT ( 'NONE',  ( -8.000190175716028307, 1477.087591074789543, 215.7421536445566801 ) ) ;
#21842 = CARTESIAN_POINT ( 'NONE',  ( -12.75406323559999855, 1424.720109696429972, 222.3910987067980045 ) ) ;
#21843 = CARTESIAN_POINT ( 'NONE',  ( 13.99234587423499931, 1513.736060322949925, 225.8518394019669984 ) ) ;
#21844 = CARTESIAN_POINT ( 'NONE',  ( -34.68852446352935459, 1501.977400791986611, 218.2490599186011764 ) ) ;
#21845 = CARTESIAN_POINT ( 'NONE',  ( 9.788553136239070085, 1435.243871060430138, 208.4607419252359932 ) ) ;
#21846 = CARTESIAN_POINT ( 'NONE',  ( -107.3576381908248862, 1390.051752611091615, 299.1848643298906723 ) ) ;
#21847 = CARTESIAN_POINT ( 'NONE',  ( 16.22122407919999887, 1419.769442695729822, 227.2112992638979847 ) ) ;
#21848 = CARTESIAN_POINT ( 'NONE',  ( -20.71343476517491311, 1522.382868172863937, 238.3377464195766890 ) ) ;
#21849 = CARTESIAN_POINT ( 'NONE',  ( 0.7350231981660010350, 1516.970035769810011, 206.8242163110469960 ) ) ;
#21850 = DIRECTION ( 'NONE',  ( 0.000000000000000000, 1.000000000000000000, 0.000000000000000000 ) ) ;
#21851 = CARTESIAN_POINT ( 'NONE',  ( -18.65369358539999922, 1410.060631937529934, 223.2007661954980051 ) ) ;
#21852 = CARTESIAN_POINT ( 'NONE',  ( 1.549824244036819954, 1416.029511582939904, 190.4358552523449930 ) ) ;
#21853 = CARTESIAN_POINT ( 'NONE',  ( -1.341950169440000007, 1416.837177099130031, 228.0806925301980073 ) ) ;
#21854 = LINE ( 'NONE', #30282, #11075 ) ;
#21855 = CARTESIAN_POINT ( 'NONE',  ( 1.842962231260000028, 1515.551704408389924, 205.2922258481490303 ) ) ;
#21856 = LINE ( 'NONE', #54432, #45989 ) ;
#21857 = CARTESIAN_POINT ( 'NONE',  ( 4.222531898828509433, 1446.229786520979815, 170.5365406785500113 ) ) ;
#21858 = CARTESIAN_POINT ( 'NONE',  ( 0.2089863181176309925, 1457.918365060180122, 183.0423947760509975 ) ) ;
#21859 = CARTESIAN_POINT ( 'NONE',  ( -8.161124881772790829, 1407.550611316829873, 219.8408402379180018 ) ) ;
#21860 = CARTESIAN_POINT ( 'NONE',  ( -18.11157280723839946, 1509.545530446499924, 231.7129765844609892 ) ) ;
#21861 = CARTESIAN_POINT ( 'NONE',  ( 16.87900699709538799, 1524.382868172804365, 181.2327155136467809 ) ) ;
#21862 = CARTESIAN_POINT ( 'NONE',  ( -28.95760783391549964, 1509.892758078639872, 211.5366180273940131 ) ) ;
#21863 = CARTESIAN_POINT ( 'NONE',  ( 11.87938290520000173, 1433.311437408509846, 148.5014532950980026 ) ) ;
#21864 = CARTESIAN_POINT ( 'NONE',  ( -27.25231198120000187, 1435.447456822929780, 135.7102113810979915 ) ) ;
#21865 = CARTESIAN_POINT ( 'NONE',  ( 7.124127264130000192, 1440.776731797129742, 185.7078817695979751 ) ) ;
#21866 = ORIENTED_EDGE ( 'NONE', *, *, #15906, .T. ) ;
#21867 = CARTESIAN_POINT ( 'NONE',  ( 2.536775590219999987, 1486.674089103790266, 197.8596855731989876 ) ) ;
#21868 = CARTESIAN_POINT ( 'NONE',  ( 7.049774511539999899, 1478.792398035790029, 201.1901003775490153 ) ) ;
#21869 = CARTESIAN_POINT ( 'NONE',  ( -3.536556481637670224, 1409.036559661029969, 223.6857672521330187 ) ) ;
#21870 = CARTESIAN_POINT ( 'NONE',  ( -11.07948225550000032, 1491.871587465490165, 207.6232410549289966 ) ) ;
#21871 = CARTESIAN_POINT ( 'NONE',  ( -1.438891081339280120, 1452.191228260170192, 183.8587004481619829 ) ) ;
#21872 = FACE_OUTER_BOUND ( 'NONE', #361, .T. ) ;
#21873 = CARTESIAN_POINT ( 'NONE',  ( 40.47987261475308429, 1425.122386052929869, 269.1161687812102059 ) ) ;
#21874 = CARTESIAN_POINT ( 'NONE',  ( -9.360741662101576210, 1480.861349342385893, 227.8150666596004328 ) ) ;
#21875 = CARTESIAN_POINT ( 'NONE',  ( -12.58289157959999827, 1379.610106932609824, 209.8104170840169900 ) ) ;
#21876 = CARTESIAN_POINT ( 'NONE',  ( -88.41516169894879340, 1384.622141336479899, 308.1440992471430036 ) ) ;
#21877 = CARTESIAN_POINT ( 'NONE',  ( -63.64159431314190840, 1385.079648997679897, 252.0084059150040048 ) ) ;
#21878 = CARTESIAN_POINT ( 'NONE',  ( -12.16337101708979951, 1490.862671263889979, 207.5438459304560013 ) ) ;
#21879 = CARTESIAN_POINT ( 'NONE',  ( 20.59684415220000275, 1507.762623718730083, 227.6602567104980039 ) ) ;
#21880 = CARTESIAN_POINT ( 'NONE',  ( -28.66375040065220148, 1509.283859623159969, 208.7539660915670083 ) ) ;
#21881 = CARTESIAN_POINT ( 'NONE',  ( -3.549608351769999892, 1507.276797637930031, 180.9704965309979912 ) ) ;
#21883 = VERTEX_POINT ( 'NONE', #60233 ) ;
#21882 = CARTESIAN_POINT ( 'NONE',  ( 0.04730083781539890647, 1508.790176069789823, 218.1427984678689995 ) ) ;
#21884 = CARTESIAN_POINT ( 'NONE',  ( -109.3072984829999967, 1384.913227208139915, 311.2647025462590022 ) ) ;
#21885 = ADVANCED_FACE ( 'NONE', ( #92169 ), #8699, .T. ) ;
#21886 = CARTESIAN_POINT ( 'NONE',  ( 40.26903804221177552, 1443.994134351532466, 137.1270700188907483 ) ) ;
#21887 = EDGE_CURVE ( 'NONE', #97701, #55731, #50642, .T. ) ;
#21888 =( BOUNDED_SURFACE ( )  B_SPLINE_SURFACE ( 1, 2, ( 
 ( #70763, #104874, #19756 ),
 ( #28164, #96476, #53958 ) ),
 .UNSPECIFIED., .F., .F., .F. ) 
 B_SPLINE_SURFACE_WITH_KNOTS ( ( 2, 2 ),
 ( 3, 3 ),
 ( -10000.00000000000000, 10000.00000000000000 ),
 ( 5.178100005969419328, 6.283185307179590673 ),
 .UNSPECIFIED. ) 
 GEOMETRIC_REPRESENTATION_ITEM ( )  RATIONAL_B_SPLINE_SURFACE ( (
 ( 0.8778166915507200629, 0.7939440108092760129, 1.000000000000000000),
 ( 0.8778166915507200629, 0.7939440108092760129, 1.000000000000000000) ) ) 
 REPRESENTATION_ITEM ( '' )  SURFACE ( )  );
#21889 = CARTESIAN_POINT ( 'NONE',  ( -3.839533257769999874, 1495.661383543789952, 219.6378539895989945 ) ) ;
#21890 = CARTESIAN_POINT ( 'NONE',  ( -0.1204520906467640012, 1419.725873375750098, 184.2476600981560182 ) ) ;
#21891 = DIRECTION ( 'NONE',  ( 0.000000000000000000, 0.000000000000000000, 1.000000000000000000 ) ) ;
#21892 = EDGE_CURVE ( 'NONE', #27217, #37900, #19300, .T. ) ;
#21893 = CARTESIAN_POINT ( 'NONE',  ( 21.21836729700000390, 1410.149259758630023, 217.3752858609580016 ) ) ;
#21894 = CARTESIAN_POINT ( 'NONE',  ( -2.193561875386760285, 1410.361078172129965, 186.3822773651310172 ) ) ;
#21895 = EDGE_CURVE ( 'NONE', #6969, #16284, #66721, .T. ) ;
#21896 = CARTESIAN_POINT ( 'NONE',  ( -16.50647692859999793, 1466.206009311390062, 220.8253520350990016 ) ) ;
#21897 = CARTESIAN_POINT ( 'NONE',  ( -16.47684141300000249, 1422.522700970730057, 227.3110121918980155 ) ) ;
#21899 = CARTESIAN_POINT ( 'NONE',  ( -11.60004869885203682, 1426.786830457828273, 134.3786150874268799 ) ) ;
#21898 = CARTESIAN_POINT ( 'NONE',  ( -3.179706416137069169, 1511.827399571667684, 201.1786234408949952 ) ) ;
#21900 = CARTESIAN_POINT ( 'NONE',  ( -12.22846866959999979, 1380.845870869829923, 215.9110647297389960 ) ) ;
#21901 = CARTESIAN_POINT ( 'NONE',  ( -102.7365228771000005, 1314.643966242390206, 304.2218459572590064 ) ) ;
#21902 = DIRECTION ( 'NONE',  ( 0.000000000000000000, 1.000000000000000000, 0.000000000000000000 ) ) ;
#21903 = CARTESIAN_POINT ( 'NONE',  ( -2.165008118169999829, 1417.511146367829951, 235.1473874566980271 ) ) ;
#21904 = CARTESIAN_POINT ( 'NONE',  ( 9.663424421700000266, 1363.752474719050042, 210.6218459616991936 ) ) ;
#21905 = CARTESIAN_POINT ( 'NONE',  ( -0.7572979743539989261, 1516.829948096479939, 205.6721984920870057 ) ) ;
#21906 = CARTESIAN_POINT ( 'NONE',  ( -10.60916564155689912, 1486.014526782129906, 184.0550009821979813 ) ) ;
#21907 = ORIENTED_EDGE ( 'NONE', *, *, #44061, .F. ) ;
#21908 = CARTESIAN_POINT ( 'NONE',  ( 11.14102298704129979, 1502.488688627300007, 213.5626339687910047 ) ) ;
#21909 = CARTESIAN_POINT ( 'NONE',  ( -10.55892651390957226, 1422.392461757438696, 210.6415085614188740 ) ) ;
#21911 = ORIENTED_EDGE ( 'NONE', *, *, #52966, .F. ) ;
#21910 = CARTESIAN_POINT ( 'NONE',  ( -67.35605454205490616, 1379.745124473419992, 278.5250339855529660 ) ) ;
#21912 = VERTEX_POINT ( 'NONE', #18201 ) ;
#21913 = CARTESIAN_POINT ( 'NONE',  ( 3.958338197117936108, 1515.551704392563124, 207.2788821125622860 ) ) ;
#21914 = ORIENTED_EDGE ( 'NONE', *, *, #35693, .T. ) ;
#21915 = CARTESIAN_POINT ( 'NONE',  ( -2.260822717048510455, 1486.453532151730087, 220.8355371193659948 ) ) ;
#21916 = CARTESIAN_POINT ( 'NONE',  ( 11.49897960310000045, 1501.122200346590034, 207.7066828831089822 ) ) ;
#21918 = CARTESIAN_POINT ( 'NONE',  ( 15.71155388851390100, 1410.111410872460056, 191.7201049767249685 ) ) ;
#21917 = CARTESIAN_POINT ( 'NONE',  ( -15.69847554260145728, 1410.486759826540947, 226.6795578664016375 ) ) ;
#21919 = CARTESIAN_POINT ( 'NONE',  ( 7.339107202615000602, 1517.203017563489766, 210.2473558205170150 ) ) ;
#21920 = EDGE_CURVE ( 'NONE', #94174, #101515, #10356, .T. ) ;
#21921 = CARTESIAN_POINT ( 'NONE',  ( -25.31040623107189802, 1451.150865907959997, 137.2672303054409895 ) ) ;
#21922 = CARTESIAN_POINT ( 'NONE',  ( -107.6824634920189965, 1378.913060387289988, 308.0758627141039483 ) ) ;
#21923 = CARTESIAN_POINT ( 'NONE',  ( 13.47022716080000215, 1410.756447827730199, 228.3151136380979835 ) ) ;
#21924 = CARTESIAN_POINT ( 'NONE',  ( 8.091656396857121791, 1483.420753468610201, 216.4477029494279918 ) ) ;
#21925 = DIRECTION ( 'NONE',  ( 0.000000000000000000, 0.000000000000000000, 1.000000000000000000 ) ) ;
#21926 = EDGE_CURVE ( 'NONE', #53780, #92019, #41314, .T. ) ;
#21927 = CARTESIAN_POINT ( 'NONE',  ( 41.66188030070000536, 1443.681299837730194, 134.0999999982049928 ) ) ;
#21928 = FACE_OUTER_BOUND ( 'NONE', #52967, .T. ) ;
#21929 = CARTESIAN_POINT ( 'NONE',  ( 14.22286847238659924, 1435.189194894129969, 149.2182491042620143 ) ) ;
#21930 = CARTESIAN_POINT ( 'NONE',  ( -3.812371247207599900, 1428.459941768050157, 200.5740418269730014 ) ) ;
#21931 = VERTEX_POINT ( 'NONE', #52398 ) ;
#21932 = ORIENTED_EDGE ( 'NONE', *, *, #7006, .F. ) ;
#21933 = ADVANCED_FACE ( 'NONE', ( #104431 ), #54266, .T. ) ;
#21934 = CARTESIAN_POINT ( 'NONE',  ( 9.130068049997401403, 1410.607079801739701, 230.1289593719837967 ) ) ;
#21935 = CARTESIAN_POINT ( 'NONE',  ( 16.25130722332281152, 1514.566425926116381, 194.3271904957884999 ) ) ;
#21936 = CARTESIAN_POINT ( 'NONE',  ( -14.08968533280249957, 1379.756368969990035, 211.4767688306389744 ) ) ;
#21937 = CARTESIAN_POINT ( 'NONE',  ( -19.37835159994689960, 1508.551704408389924, 210.4314531256320038 ) ) ;
#21938 = CARTESIAN_POINT ( 'NONE',  ( -26.92695807870000380, 1508.008395488129963, 203.1594552079080245 ) ) ;
#21939 = LINE ( 'NONE', #39329, #35793 ) ;
#21940 = CARTESIAN_POINT ( 'NONE',  ( -0.7524479025939990740, 1465.050001273689986, 198.5341880975990136 ) ) ;
#21941 = B_SPLINE_CURVE_WITH_KNOTS ( 'NONE', 5,
 ( #4782, #47902, #21016, #107249, #46822, #20465 ),
 .UNSPECIFIED., .F., .F.,
 ( 6, 6 ),
 ( 0.000000000000000000, 1.000000000000000000 ),
 .UNSPECIFIED. ) ;
#21942 = CARTESIAN_POINT ( 'NONE',  ( -5.303285988883490454, 1442.879254652209966, 200.5943008362860098 ) ) ;
#21943 = CARTESIAN_POINT ( 'NONE',  ( 10.58917204930000011, 1416.519106787730152, 194.4914516038979855 ) ) ;
#21944 = CARTESIAN_POINT ( 'NONE',  ( -81.42396034917169345, 1384.801295219920121, 284.9086290667029857 ) ) ;
#21945 = ORIENTED_EDGE ( 'NONE', *, *, #55537, .F. ) ;
#21946 = CARTESIAN_POINT ( 'NONE',  ( -1.984413551915469975, 1522.051704408389924, 219.3307686695569885 ) ) ;
#21947 = CARTESIAN_POINT ( 'NONE',  ( 2.865636809105000182, 1516.815173273089840, 207.9858416580370033 ) ) ;
#21948 = ORIENTED_EDGE ( 'NONE', *, *, #34316, .T. ) ;
#21949 = CARTESIAN_POINT ( 'NONE',  ( 35.01374679072880269, 1440.913060387330006, 260.8650110618089570 ) ) ;
#21950 = CARTESIAN_POINT ( 'NONE',  ( 19.56640942089999768, 1477.362144060529999, 227.5239896928979988 ) ) ;
#21951 = ORIENTED_EDGE ( 'NONE', *, *, #69903, .T. ) ;
#21952 = CARTESIAN_POINT ( 'NONE',  ( -0.03276332933436820055, 1451.172142415660119, 182.5300517626539829 ) ) ;
#21953 = CARTESIAN_POINT ( 'NONE',  ( -15.50892216750000152, 1410.826985104829873, 191.0414747596979907 ) ) ;
#21954 = CARTESIAN_POINT ( 'NONE',  ( -18.31568283352659066, 1508.457201626663391, 211.3964485825274835 ) ) ;
#21955 = CARTESIAN_POINT ( 'NONE',  ( -9.792761917529839266, 1461.792922494570121, 207.9051543940479974 ) ) ;
#21956 = B_SPLINE_CURVE_WITH_KNOTS ( 'NONE', 3,
 ( #92740, #102775, #101125, #50216 ),
 .UNSPECIFIED., .F., .F.,
 ( 4, 4 ),
 ( 0.9214954035317776126, 1.000000000000000000 ),
 .UNSPECIFIED. ) ;
#21957 = CARTESIAN_POINT ( 'NONE',  ( 22.24622733321460188, 1410.233794050260030, 206.2464451110010089 ) ) ;
#21958 = CARTESIAN_POINT ( 'NONE',  ( -6.247704817804169863, 1510.876154134900162, 201.6775610366950104 ) ) ;
#21959 = CARTESIAN_POINT ( 'NONE',  ( 1.328042612950000034, 1406.002643151530037, 266.9604903208979749 ) ) ;
#21960 = CARTESIAN_POINT ( 'NONE',  ( -5.761500042352934337, 1510.554407334616599, 201.5803765894013111 ) ) ;
#21961 = CARTESIAN_POINT ( 'NONE',  ( -21.19880661589042248, 1524.382868172863937, 184.6948938244650833 ) ) ;
#21963 = CARTESIAN_POINT ( 'NONE',  ( 0.2456417414777120334, 1457.830897802899926, 228.9878416128509855 ) ) ;
#21962 = CARTESIAN_POINT ( 'NONE',  ( 16.16575468819999983, 1459.553750540530018, 229.8409642424979893 ) ) ;
#21964 = CARTESIAN_POINT ( 'NONE',  ( -7.328676208015000526, 1516.833844030519913, 216.0648195994369871 ) ) ;
#21965 = B_SPLINE_CURVE_WITH_KNOTS ( 'NONE', 3,
 ( #60905, #17732, #26146, #95031, #76568, #50823, #59242, #8244, #8798, #44086, #51933, #59788, #93907, #42413 ),
 .UNSPECIFIED., .F., .F.,
 ( 4, 2, 2, 1, 1, 2, 2, 4 ),
 ( 0.000000000000000000, 0.2499999999987723154, 0.3749999999981014076, 0.4374999999978853027, 0.4687499999975743292, 0.4843749999974187870, 0.4999999999972633002, 1.000000000000000000 ),
 .UNSPECIFIED. ) ;
#21966 = CARTESIAN_POINT ( 'NONE',  ( -11.78824854703250047, 1517.151704408390060, 206.8304425649369875 ) ) ;
#21967 = PRODUCT_DEFINITION ( 'UNKNOWN', '', #26123, #86055 ) ;
#21968 = CARTESIAN_POINT ( 'NONE',  ( -0.1573922665717430169, 1507.260657537599855, 180.8910309565839896 ) ) ;
#21969 = CARTESIAN_POINT ( 'NONE',  ( 2.412842859265553308, 1516.533219998030972, 216.8308492924006998 ) ) ;
#21970 = CARTESIAN_POINT ( 'NONE',  ( -1.702754409475000008, 1517.014196759610059, 212.5856132281170119 ) ) ;
#21971 = CARTESIAN_POINT ( 'NONE',  ( 18.66848652210000026, 1509.564978301430074, 187.1506650077980112 ) ) ;
#21972 = CARTESIAN_POINT ( 'NONE',  ( 16.62866627238343753, 1455.169317704825971, 198.5414531324474865 ) ) ;
#21974 = EDGE_LOOP ( 'NONE', ( #34751, #49674, #30665, #18188 ) ) ;
#21973 = CARTESIAN_POINT ( 'NONE',  ( -113.4000000000000057, 1387.988142337750105, 310.3973246102589769 ) ) ;
#21975 = CARTESIAN_POINT ( 'NONE',  ( -8.604091250959998050, 1384.887133344300082, 199.8687245402490191 ) ) ;
#21976 = CARTESIAN_POINT ( 'NONE',  ( 25.89198661420000036, 1440.913060407119929, 221.6500998374979758 ) ) ;
#21977 = CARTESIAN_POINT ( 'NONE',  ( -11.56980561469999991, 1431.824675720370124, 151.1783349937979892 ) ) ;
#21978 = CARTESIAN_POINT ( 'NONE',  ( -15.11369138130000067, 1415.717925739890006, 206.7297616978289909 ) ) ;
#21979 = CARTESIAN_POINT ( 'NONE',  ( -7.855691861358739203, 1441.328234993660089, 203.4967717689210076 ) ) ;
#21980 = CARTESIAN_POINT ( 'NONE',  ( -0.3885940661755200032, 1508.683165393880245, 238.1397126418920038 ) ) ;
#21981 = CARTESIAN_POINT ( 'NONE',  ( 17.12202622827918219, 1526.104292489127602, 182.3009725563080963 ) ) ;
#21982 = CARTESIAN_POINT ( 'NONE',  ( 12.40989122010000045, 1445.169290119350080, 186.8528423751979801 ) ) ;
#21983 = EDGE_CURVE ( 'NONE', #1894, #5115, #5218, .T. ) ;
#21985 = CARTESIAN_POINT ( 'NONE',  ( 5.366743882629579687, 1426.154185019739998, 152.4687380856059917 ) ) ;
#21984 = CARTESIAN_POINT ( 'NONE',  ( -20.97306094379999664, 1457.442401685129880, 223.5384559969980103 ) ) ;
#21986 = FACE_OUTER_BOUND ( 'NONE', #25533, .T. ) ;
#21987 = ORIENTED_EDGE ( 'NONE', *, *, #17933, .F. ) ;
#21988 = CARTESIAN_POINT ( 'NONE',  ( 5.772727908745000747, 1516.691414181030041, 205.6645793267070133 ) ) ;
#21989 = CARTESIAN_POINT ( 'NONE',  ( 2.094456431300000254, 1406.299313630030156, 269.2930948147979962 ) ) ;
#21990 = EDGE_CURVE ( 'NONE', #63851, #22743, #45303, .T. ) ;
#21991 = CARTESIAN_POINT ( 'NONE',  ( -1.491125504899999843, 1515.528285129289998, 213.1665752102589977 ) ) ;
#21992 = LINE ( 'NONE', #6328, #85372 ) ;
#21993 = CARTESIAN_POINT ( 'NONE',  ( 23.71260330876479827, 1434.455778039984807, 214.5166046885597098 ) ) ;
#21994 = DIRECTION ( 'NONE',  ( 0.000000000000000000, 1.000000000000000000, 0.000000000000000000 ) ) ;
#21995 = CARTESIAN_POINT ( 'NONE',  ( 11.60004869885203682, 1423.633693347439475, 135.8154946617876249 ) ) ;
#21996 = CARTESIAN_POINT ( 'NONE',  ( -9.873159097401318363, 1446.847070703570125, 212.1006879182309888 ) ) ;
#21997 = EDGE_CURVE ( 'NONE', #87290, #1678, #90366, .T. ) ;
#21998 = CARTESIAN_POINT ( 'NONE',  ( -0.5697989934050000649, 1450.893162568020216, 155.6080925171979743 ) ) ;
#21999 = CARTESIAN_POINT ( 'NONE',  ( -1.554371093571602636, 1451.096106140563052, 183.6610704733489285 ) ) ;
#22000 = CARTESIAN_POINT ( 'NONE',  ( 2.318887788901189850, 1449.808491804770028, 155.3361369919100241 ) ) ;
#22001 = CARTESIAN_POINT ( 'NONE',  ( -13.59781064528760020, 1415.089996090609930, 220.5183280911249994 ) ) ;
#22002 = CARTESIAN_POINT ( 'NONE',  ( -12.31967538714310173, 1378.053937847460020, 209.2867312577349992 ) ) ;
#22003 = CARTESIAN_POINT ( 'NONE',  ( -32.79207798510000771, 1428.560640286930038, 262.6648722511980054 ) ) ;
#22004 = DIRECTION ( 'NONE',  ( -0.9455185755993177343, 0.000000000000000000, 0.3255681544571540909 ) ) ;
#22005 = CARTESIAN_POINT ( 'NONE',  ( 3.654458881370000078, 1441.526081356940040, 166.9096120827979917 ) ) ;
#22006 = CARTESIAN_POINT ( 'NONE',  ( -2.111022820160000091, 1476.015127867530055, 268.4819080596980143 ) ) ;
#22007 = CARTESIAN_POINT ( 'NONE',  ( 9.767576865416099707, 1416.948096802409964, 215.8813206395359998 ) ) ;
#22008 = CARTESIAN_POINT ( 'NONE',  ( -11.28286893315524964, 1512.859150068915596, 192.9221778144517145 ) ) ;
#22009 = EDGE_CURVE ( 'NONE', #17382, #68939, #43861, .T. ) ;
#22010 = CARTESIAN_POINT ( 'NONE',  ( -2.500000000000000000, 1448.210448412289907, 183.1418046154980175 ) ) ;
#22011 = CARTESIAN_POINT ( 'NONE',  ( -25.34879943620689957, 1384.844904870469918, 223.9545694878910069 ) ) ;
#22012 = DIRECTION ( 'NONE',  ( 6.360620485575798415E-17, 1.000000000000000000, -8.754643039332639448E-17 ) ) ;
#22013 = CARTESIAN_POINT ( 'NONE',  ( -21.34258212929999488, 1507.002782982890039, 212.5338223445889980 ) ) ;
#22014 = CARTESIAN_POINT ( 'NONE',  ( 12.03979944771670141, 1491.360865940330086, 206.6897700099570159 ) ) ;
#22015 = CARTESIAN_POINT ( 'NONE',  ( 32.28368668151611587, 1524.972383263452684, 217.0406336501054341 ) ) ;
#22016 = CARTESIAN_POINT ( 'NONE',  ( 8.150367991650082189, 1511.506734315487620, 205.2632391311709057 ) ) ;
#22017 = ADVANCED_FACE ( 'NONE', ( #64105 ), #52422, .F. ) ;
#22018 = CARTESIAN_POINT ( 'NONE',  ( -2.054592539991249911, 1395.984808339839901, 219.9445789274560070 ) ) ;
#22019 = ADVANCED_FACE ( 'NONE', ( #51010 ), #108243, .T. ) ;
#22020 = CARTESIAN_POINT ( 'NONE',  ( -2.572244737866500319, 1508.551704408389924, 204.1347675067580099 ) ) ;
#22021 = CARTESIAN_POINT ( 'NONE',  ( -44.83996340390000057, 1438.826799026090157, 269.6929264061980120 ) ) ;
#22022 = ORIENTED_EDGE ( 'NONE', *, *, #33518, .F. ) ;
#22023 = CARTESIAN_POINT ( 'NONE',  ( 10.56407690400000021, 1452.658140130590027, 209.7432180304350027 ) ) ;
#22024 = CARTESIAN_POINT ( 'NONE',  ( -7.469839269216643984, 1510.808998940006859, 215.2720920852931101 ) ) ;
#22025 = CARTESIAN_POINT ( 'NONE',  ( -17.66147422868510120, 1440.150478810159939, 218.7822781200609938 ) ) ;
#22026 =( BOUNDED_CURVE ( )  B_SPLINE_CURVE ( 2, ( #16033, #91108, #73214 ),
 .UNSPECIFIED., .F., .T. ) 
 B_SPLINE_CURVE_WITH_KNOTS ( ( 3, 3 ),
 ( -0.2337410562555060078, -0.1572692978119380192 ),
 .UNSPECIFIED. ) 
 CURVE ( )  GEOMETRIC_REPRESENTATION_ITEM ( )  RATIONAL_B_SPLINE_CURVE ( ( 1.002760198482619991, 1.002448066741719934, 1.002044729649790078 ) ) 
 REPRESENTATION_ITEM ( '' )  );
#22028 = CARTESIAN_POINT ( 'NONE',  ( -12.38398713116500005, 1512.136030808819896, 194.2018088040669852 ) ) ;
#22027 = CARTESIAN_POINT ( 'NONE',  ( -16.30135123648100048, 1416.771455524889916, 208.9839307753329649 ) ) ;
#22029 = CARTESIAN_POINT ( 'NONE',  ( 17.17241001986483795, 1512.187213306747481, 180.6185504016043240 ) ) ;
#22030 = CARTESIAN_POINT ( 'NONE',  ( 40.24526342089999531, 1444.639349322710132, 137.0236526114979938 ) ) ;
#22031 = ADVANCED_FACE ( 'NONE', ( #53797 ), #12850, .F. ) ;
#22032 = CARTESIAN_POINT ( 'NONE',  ( -4.036119682645000317, 1516.647924054489977, 201.7978713257969900 ) ) ;
#22033 = CARTESIAN_POINT ( 'NONE',  ( 7.563118004889999746, 1426.194615592600030, 212.1958855806589952 ) ) ;
#22034 = CARTESIAN_POINT ( 'NONE',  ( -22.19117979949999864, 1483.602007700189915, 216.8115292462290142 ) ) ;
#22035 = CARTESIAN_POINT ( 'NONE',  ( 5.949633633660000420, 1509.124405061829975, 180.2787687912980061 ) ) ;
#22036 = CARTESIAN_POINT ( 'NONE',  ( -16.25298958656239989, 1420.731237529160126, 203.3078988358529955 ) ) ;
#22037 = CARTESIAN_POINT ( 'NONE',  ( -75.28129077213660025, 1378.304634124660197, 294.2128303316549705 ) ) ;
#22038 = CARTESIAN_POINT ( 'NONE',  ( 7.862230021551401826, 1365.371610286726764, 208.3718459617061285 ) ) ;
#22039 = EDGE_CURVE ( 'NONE', #32788, #71548, #106907, .T. ) ;
#22041 = ORIENTED_EDGE ( 'NONE', *, *, #20799, .T. ) ;
#22040 = CARTESIAN_POINT ( 'NONE',  ( 9.699838434020000122, 1453.359120720189821, 212.1672247696689908 ) ) ;
#22042 = VERTEX_POINT ( 'NONE', #89006 ) ;
#22043 = CARTESIAN_POINT ( 'NONE',  ( -11.33516131130000026, 1396.308892942629882, 207.6268627275279925 ) ) ;
#22044 = CARTESIAN_POINT ( 'NONE',  ( -21.35664706530000245, 1409.658850939629929, 213.3192769937880087 ) ) ;
#22045 = CARTESIAN_POINT ( 'NONE',  ( -2.759740495412019712, 1516.551695078709827, 201.4123589199890034 ) ) ;
#22046 = CARTESIAN_POINT ( 'NONE',  ( -13.17594539069787274, 1444.732583810137385, 169.3946485105632291 ) ) ;
#22047 = DIRECTION ( 'NONE',  ( 0.000000000000000000, 0.000000000000000000, 1.000000000000000000 ) ) ;
#22048 = CARTESIAN_POINT ( 'NONE',  ( -7.575166957224999997, 1511.422242621320265, 211.8233863454470054 ) ) ;
#22050 = CARTESIAN_POINT ( 'NONE',  ( -21.51358107078230120, 1505.588370892289959, 209.3658540944720130 ) ) ;
#22049 = CARTESIAN_POINT ( 'NONE',  ( -105.5067510789999972, 1391.271045334170140, 304.2081904284589768 ) ) ;
#22051 = CARTESIAN_POINT ( 'NONE',  ( 1.298837812259999946, 1410.307958403729799, 185.2609176365979806 ) ) ;
#22052 = CARTESIAN_POINT ( 'NONE',  ( -7.090791903819999575, 1414.913060387329779, 194.3735294399980091 ) ) ;
#22053 = CARTESIAN_POINT ( 'NONE',  ( -41.14894028195599418, 1446.681896710060073, 135.2730459677599981 ) ) ;
#22054 =( LENGTH_UNIT ( ) NAMED_UNIT ( * ) SI_UNIT ( .MILLI., .METRE. ) );
#22055 = CARTESIAN_POINT ( 'NONE',  ( 10.14935679994219875, 1396.267483737839939, 213.5348577357469821 ) ) ;
#22056 = CARTESIAN_POINT ( 'NONE',  ( 1.124394188919999982, 1416.535385209630022, 190.1732668564980031 ) ) ;
#22057 = CARTESIAN_POINT ( 'NONE',  ( 11.20517263770000049, 1426.030335666529936, 148.0940953015980028 ) ) ;
#22058 = CARTESIAN_POINT ( 'NONE',  ( 8.680232473730548293, 1509.216213366276406, 181.1240079135133954 ) ) ;
#22059 = ORIENTED_EDGE ( 'NONE', *, *, #93344, .F. ) ;
#22060 = CARTESIAN_POINT ( 'NONE',  ( -17.12202622829238052, 1526.104292489134423, 182.3009725563086931 ) ) ;
#22061 = ORIENTED_EDGE ( 'NONE', *, *, #28887, .T. ) ;
#22062 = EDGE_CURVE ( 'NONE', #108306, #93939, #71226, .T. ) ;
#22063 = EDGE_LOOP ( 'NONE', ( #55861, #85699, #54004, #76029 ) ) ;
#22064 = CARTESIAN_POINT ( 'NONE',  ( -19.00773967308149892, 1468.169424052289969, 227.6346832009180048 ) ) ;
#22065 = CARTESIAN_POINT ( 'NONE',  ( 9.532517564019999057, 1366.286862064870093, 207.6218459616989946 ) ) ;
#22066 = CARTESIAN_POINT ( 'NONE',  ( -109.9353129566706002, 1385.616331449368545, 311.4122602311213655 ) ) ;
#22067 = CARTESIAN_POINT ( 'NONE',  ( -28.44964981547095917, 1526.382868172864164, 198.3640452512632351 ) ) ;
#22068 = CARTESIAN_POINT ( 'NONE',  ( 3.261007131564999995, 1516.596789218710001, 216.4445556570670135 ) ) ;
#22069 = DIRECTION ( 'NONE',  ( 0.000000000000000000, 0.000000000000000000, 1.000000000000000000 ) ) ;
#22070 = B_SPLINE_SURFACE_WITH_KNOTS ( 'NONE', 5, 5, ( 
 ( #84165, #41627, #7465, #32120, #67401, #31559 ),
 ( #16387, #8012, #15297, #42179, #48944, #74692 ),
 ( #6368, #48388, #49489, #99301, #22575, #56779 ),
 ( #14202, #82531, #23150, #5827, #75244, #57353 ),
 ( #91478, #40514, #108824, #87502, #43837, #69060 ),
 ( #70182, #34323, #93652, #68502, #10792, #1857 ) ),
 .UNSPECIFIED., .F., .F., .F.,
 ( 6, 6 ),
 ( 6, 6 ),
 ( -0.001190444914978719881, 1.957152629518910114 ),
 ( 0.000000000000000000, 2.001190444958909964 ),
 .UNSPECIFIED. ) ;
#22071 = ADVANCED_FACE ( 'NONE', ( #72240 ), #51108, .T. ) ;
#22072 = ORIENTED_EDGE ( 'NONE', *, *, #89939, .F. ) ;
#22073 = CARTESIAN_POINT ( 'NONE',  ( -16.80117805631029881, 1508.522152650069984, 213.2817618438170086 ) ) ;
#22074 = CARTESIAN_POINT ( 'NONE',  ( 2.500000000000059952, 1448.812655445319933, 156.5234696244650081 ) ) ;
#22075 = CARTESIAN_POINT ( 'NONE',  ( -41.40570855549999862, 1375.117442312619914, 227.6002677670589947 ) ) ;
#22076 = CARTESIAN_POINT ( 'NONE',  ( 16.97980319039999841, 1414.913060387329779, 210.1126989473540050 ) ) ;
#22077 = CARTESIAN_POINT ( 'NONE',  ( -7.722536802824999214, 1517.050041317280147, 204.5049460973469877 ) ) ;
#22078 = VERTEX_POINT ( 'NONE', #12294 ) ;
#22079 = CARTESIAN_POINT ( 'NONE',  ( -1.122033430074999893, 1516.972341476009888, 209.8777854684929878 ) ) ;
#22080 = CARTESIAN_POINT ( 'NONE',  ( -9.572080927779999334E-17, 1389.913060387289988, 209.1218459616989946 ) ) ;
#22081 = CARTESIAN_POINT ( 'NONE',  ( -27.65802006675362890, 1417.861769239410251, 269.4462164507287980 ) ) ;
#22082 = CARTESIAN_POINT ( 'NONE',  ( 6.396410510614999545, 1511.623805160500069, 216.5973402254469988 ) ) ;
#22084 = ORIENTED_EDGE ( 'NONE', *, *, #20343, .T. ) ;
#22083 = CARTESIAN_POINT ( 'NONE',  ( 2.356903266504112082, 1525.394057003702756, 176.3139131587520012 ) ) ;
#22085 = CARTESIAN_POINT ( 'NONE',  ( -0.01247695416628590015, 1452.307842348659960, 183.1512626530130206 ) ) ;
#22086 = CARTESIAN_POINT ( 'NONE',  ( -32.66611254161259836, 1440.913060389849988, 245.7919302191029942 ) ) ;
#22087 = CARTESIAN_POINT ( 'NONE',  ( -67.06144730649998564, 1384.373230830070042, 292.1716250880589882 ) ) ;
#22088 = CARTESIAN_POINT ( 'NONE',  ( -0.06005238713462270062, 1466.393664084419925, 235.6964261762240085 ) ) ;
#22089 = CARTESIAN_POINT ( 'NONE',  ( 29.04137415450000148, 1415.566708622129909, 270.1335617710980159 ) ) ;
#22090 = CARTESIAN_POINT ( 'NONE',  ( -5.772403812434999892, 1516.676340709600026, 212.3853678745870184 ) ) ;
#22091 = CARTESIAN_POINT ( 'NONE',  ( -65.04611674080000228, 1379.740440402699960, 272.5882088742590099 ) ) ;
#22092 = CARTESIAN_POINT ( 'NONE',  ( 23.72329886969999890, 1410.130063465129979, 208.9290854598660019 ) ) ;
#22093 = EDGE_CURVE ( 'NONE', #42405, #29094, #20728, .T. ) ;
#22094 = DIRECTION ( 'NONE',  ( -1.755985294532469921E-16, 1.000000000000000000, -1.338183447452831989E-16 ) ) ;
#22095 = CARTESIAN_POINT ( 'NONE',  ( 12.43796050777599937, 1426.539880023309934, 196.0224772779999967 ) ) ;
#22096 = CARTESIAN_POINT ( 'NONE',  ( -7.709261221864290192, 1516.543067334049965, 210.8692578450250039 ) ) ;
#22097 = CARTESIAN_POINT ( 'NONE',  ( -2.284053509485000077, 1516.854133554269993, 210.2586600040969813 ) ) ;
#22098 = CARTESIAN_POINT ( 'NONE',  ( 4.213210515277539869, 1421.777857766699981, 184.5142607373319947 ) ) ;
#22099 = CARTESIAN_POINT ( 'NONE',  ( 17.22845748920278197, 1525.848198008145346, 181.7617192448029186 ) ) ;
#22100 = CARTESIAN_POINT ( 'NONE',  ( -5.513435759310994833, 1508.884207225798491, 201.6131390159873717 ) ) ;
#22102 = VERTEX_POINT ( 'NONE', #55430 ) ;
#22101 = CARTESIAN_POINT ( 'NONE',  ( -25.94961989419999782, 1385.251886777470190, 224.2307850120589876 ) ) ;
#22103 = CARTESIAN_POINT ( 'NONE',  ( -23.13586480360919850, 1385.263656115849926, 222.4840418823009998 ) ) ;
#22104 = DIRECTION ( 'NONE',  ( -0.03248864917721539652, 0.9989961268278857442, 0.03084195612347889401 ) ) ;
#22105 = CARTESIAN_POINT ( 'NONE',  ( 0.7357070794679999581, 1416.194395688229861, 233.4110786845979817 ) ) ;
#22106 = CARTESIAN_POINT ( 'NONE',  ( 4.487249772970000272, 1509.038615934189920, 211.6097810847190033 ) ) ;
#22107 = CARTESIAN_POINT ( 'NONE',  ( 7.549016763624999626, 1510.423579818979988, 204.6938642082269837 ) ) ;
#22108 = CARTESIAN_POINT ( 'NONE',  ( 12.10442663210000092, 1426.312261714450187, 203.5844782087590090 ) ) ;
#22109 = CARTESIAN_POINT ( 'NONE',  ( -1.351911418288906486, 1498.080636687657943, 197.8999588905911935 ) ) ;
#22110 = AXIS2_PLACEMENT_3D ( 'NONE', #55593, #12994, #36026 ) ;
#22111 = EDGE_CURVE ( 'NONE', #56812, #46627, #58571, .T. ) ;
#22113 = DIRECTION ( 'NONE',  ( 0.9232892630913372978, -0.3773383177895360263, 0.07178252285910749486 ) ) ;
#22112 = CARTESIAN_POINT ( 'NONE',  ( 3.455377977254999955, 1516.627618683580067, 216.0573038954169931 ) ) ;
#22114 = DIRECTION ( 'NONE',  ( 0.03489949677589983257, 0.9993908270165325902, 3.539110176465913504E-10 ) ) ;
#22115 = CARTESIAN_POINT ( 'NONE',  ( 10.70393068008039883, 1470.122838572239971, 207.0328785961279721 ) ) ;
#22116 = ORIENTED_EDGE ( 'NONE', *, *, #47932, .T. ) ;
#22117 = CARTESIAN_POINT ( 'NONE',  ( -1.708721022705000037, 1516.531533746980131, 201.8006767011069940 ) ) ;
#22118 = CARTESIAN_POINT ( 'NONE',  ( 27.79064039367209915, 1508.605033446070138, 207.7520403700050053 ) ) ;
#22119 = ORIENTED_EDGE ( 'NONE', *, *, #18509, .T. ) ;
#22120 = CARTESIAN_POINT ( 'NONE',  ( -15.52404079726500896, 1511.843510977570077, 220.5312950707671291 ) ) ;
#22121 = AXIS2_PLACEMENT_3D ( 'NONE', #27604, #11910, #36556 ) ;
#22122 = DIRECTION ( 'NONE',  ( 0.9786619618251657382, 0.000000000000000000, 0.2054769195713179730 ) ) ;
#22123 = CARTESIAN_POINT ( 'NONE',  ( 10.80173838838189937, 1461.850243658630006, 211.0554024487279889 ) ) ;
#22124 = CARTESIAN_POINT ( 'NONE',  ( 8.321056393114139027, 1511.434991102970116, 203.7361516517889868 ) ) ;
#22125 = CARTESIAN_POINT ( 'NONE',  ( 0.8893565964429990256, 1443.272965271590010, 218.1164608023390201 ) ) ;
#22126 = CARTESIAN_POINT ( 'NONE',  ( 16.31593820514824245, 1421.547646607773231, 227.2390930618354332 ) ) ;
#22127 = EDGE_CURVE ( 'NONE', #99467, #73683, #99791, .T. ) ;
#22128 = DIRECTION ( 'NONE',  ( 0.000000000000000000, 0.000000000000000000, 1.000000000000000000 ) ) ;
#22129 = CARTESIAN_POINT ( 'NONE',  ( -19.63203962769999933, 1425.837002826029902, 223.1478923402980001 ) ) ;
#22130 = CARTESIAN_POINT ( 'NONE',  ( -31.87156127897992164, 1465.374349214318727, 269.3184216098884463 ) ) ;
#22131 = CARTESIAN_POINT ( 'NONE',  ( -103.8898683500000004, 1389.939938586880089, 304.1778429387589995 ) ) ;
#22132 = CARTESIAN_POINT ( 'NONE',  ( 16.88838891829999866, 1438.560075112930235, 190.6614884790980113 ) ) ;
#22134 = CARTESIAN_POINT ( 'NONE',  ( 29.78452510889999871, 1510.001069734030125, 209.1390482955230254 ) ) ;
#22133 = FACE_OUTER_BOUND ( 'NONE', #61537, .T. ) ;
#22135 = CARTESIAN_POINT ( 'NONE',  ( -10.92505087063870661, 1470.396171842393642, 269.3500471555659033 ) ) ;
#22136 = ORIENTED_EDGE ( 'NONE', *, *, #5717, .T. ) ;
#22137 = AXIS2_PLACEMENT_3D ( 'NONE', #92880, #67156, #31320 ) ;
#22138 = ADVANCED_FACE ( 'NONE', ( #89561 ), #97274, .T. ) ;
#22139 = CARTESIAN_POINT ( 'NONE',  ( -11.35634668980000050, 1508.540398121890121, 217.9340572581489823 ) ) ;
#22140 = CARTESIAN_POINT ( 'NONE',  ( 11.52810963750000006, 1441.751267666019885, 147.8533156590980013 ) ) ;
#22141 = CARTESIAN_POINT ( 'NONE',  ( 11.39624612213719956, 1470.888150039209904, 208.8400483771679887 ) ) ;
#22142 = CARTESIAN_POINT ( 'NONE',  ( -11.73230603450000054, 1475.513060387329915, 226.3291547820980156 ) ) ;
#22143 = CARTESIAN_POINT ( 'NONE',  ( 3.089458805060000035, 1471.641899322389918, 189.2928579873990032 ) ) ;
#22144 = CARTESIAN_POINT ( 'NONE',  ( -5.257080573758879716, 1517.151704408390060, 199.2452589303538275 ) ) ;
#22145 = CARTESIAN_POINT ( 'NONE',  ( -13.38968634609168973, 1444.443546846214304, 186.8783483159165257 ) ) ;
#22146 = CIRCLE ( 'NONE', #11483, 33.13701971169416538 ) ;
#22147 = DIRECTION ( 'NONE',  ( 0.3090169943749582204, -0.000000000000000000, 0.9510565162951499785 ) ) ;
#22148 = CARTESIAN_POINT ( 'NONE',  ( 2.670462192661819945, 1494.657381268529889, 220.1092738806310081 ) ) ;
#22149 = CARTESIAN_POINT ( 'NONE',  ( -14.20882318218850671, 1410.783320127021625, 226.8601890847973550 ) ) ;
#22150 = CARTESIAN_POINT ( 'NONE',  ( -108.1212971963999934, 1383.758655145139983, 311.0734215935020188 ) ) ;
#22151 = CARTESIAN_POINT ( 'NONE',  ( 23.71772659069999989, 1435.325744483010112, 137.0491500660980080 ) ) ;
#22152 = CARTESIAN_POINT ( 'NONE',  ( -0.1688575540563629906, 1516.885624574960048, 201.4036151776949737 ) ) ;
#22154 = VERTEX_POINT ( 'NONE', #78778 ) ;
#22153 = CARTESIAN_POINT ( 'NONE',  ( 21.45381977619999958, 1509.599256739130169, 189.3186887596979773 ) ) ;
#22155 = CARTESIAN_POINT ( 'NONE',  ( -109.9987473180000137, 1381.991098133720016, 297.9223374245589753 ) ) ;
#22156 = EDGE_CURVE ( 'NONE', #3437, #31004, #9193, .T. ) ;
#22157 = CARTESIAN_POINT ( 'NONE',  ( 14.21962190857029995, 1513.293387711980131, 224.3376499801869954 ) ) ;
#22158 = ORIENTED_EDGE ( 'NONE', *, *, #23342, .F. ) ;
#22159 = ORIENTED_EDGE ( 'NONE', *, *, #18478, .F. ) ;
#22160 = CARTESIAN_POINT ( 'NONE',  ( -11.43660070340000168, 1501.123905251690076, 209.6404345575209902 ) ) ;
#22161 = CARTESIAN_POINT ( 'NONE',  ( 7.396545043095000160, 1511.069621805459974, 202.7496783316070150 ) ) ;
#22163 = CARTESIAN_POINT ( 'NONE',  ( -29.79081509809999773, 1446.796541104080234, 240.1465591067980085 ) ) ;
#22162 = CARTESIAN_POINT ( 'NONE',  ( 16.13326284106888409, 1412.745257486696573, 269.3696321425749147 ) ) ;
#22164 = EDGE_CURVE ( 'NONE', #13345, #40573, #18294, .T. ) ;
#22165 = B_SPLINE_CURVE_WITH_KNOTS ( 'NONE', 3,
 ( #101377, #5714, #32002, #100310, #24128, #73477 ),
 .UNSPECIFIED., .F., .F.,
 ( 4, 2, 4 ),
 ( -0.2778631991162420212, -0.1390217994342580199, -1.348645189525043975E-06 ),
 .UNSPECIFIED. ) ;
#22166 = CARTESIAN_POINT ( 'NONE',  ( -19.61843700589999884, 1487.979149483630181, 189.7675855031980063 ) ) ;
#22167 = CARTESIAN_POINT ( 'NONE',  ( -11.27542400379999954, 1433.368079989050102, 151.5215836857980207 ) ) ;
#22168 = ADVANCED_FACE ( 'NONE', ( #61449 ), #74303, .T. ) ;
#22169 = DIRECTION ( 'NONE',  ( 2.042903098301770100E-14, 1.000000000000000000, -6.143886524153290706E-15 ) ) ;
#22170 = CARTESIAN_POINT ( 'NONE',  ( 11.66274484067749917, 1426.745571914170114, 138.8594401931470088 ) ) ;
#22171 = LINE ( 'NONE', #90500, #66151 ) ;
#22172 = CARTESIAN_POINT ( 'NONE',  ( -2.383407846123591689, 1522.906363951597314, 243.2919566057130396 ) ) ;
#22173 = CARTESIAN_POINT ( 'NONE',  ( -24.36390206349999943, 1440.635616014810012, 211.6747593621879844 ) ) ;
#22174 = DIRECTION ( 'NONE',  ( 0.9455185755993178454, 0.000000000000000000, -0.3255681544571537578 ) ) ;
#22175 = CARTESIAN_POINT ( 'NONE',  ( -7.058092113492199005, 1478.002960266890113, 218.3245252530660139 ) ) ;
#22176 = CARTESIAN_POINT ( 'NONE',  ( -0.7618909056700008398, 1360.403425203260213, 207.6218459616989946 ) ) ;
#22177 = B_SPLINE_CURVE_WITH_KNOTS ( 'NONE', 5,
 ( #85212, #8503, #60603, #70124, #26983, #18549 ),
 .UNSPECIFIED., .F., .F.,
 ( 6, 6 ),
 ( -48.27399248280480037, -29.43575841650000058 ),
 .UNSPECIFIED. ) ;
#22178 = ADVANCED_FACE ( 'NONE', ( #77672 ), #52955, .T. ) ;
#22179 = CARTESIAN_POINT ( 'NONE',  ( 1.632486301776860348E-07, 1509.047264794319972, 239.1218459617020073 ) ) ;
#22181 = VERTEX_POINT ( 'NONE', #62042 ) ;
#22180 = CARTESIAN_POINT ( 'NONE',  ( 2.013013938216309949E-10, 1411.227950868479866, 255.5841367965100517 ) ) ;
#22182 = ORIENTED_EDGE ( 'NONE', *, *, #94887, .T. ) ;
#22183 = LINE ( 'NONE', #97261, #49779 ) ;
#22184 = CARTESIAN_POINT ( 'NONE',  ( -21.44268124680000298, 1506.807080485189999, 216.0956879933890207 ) ) ;
#22185 = CARTESIAN_POINT ( 'NONE',  ( -19.91919522000000242, 1467.971789498529915, 269.3862225696980204 ) ) ;
#22186 = CARTESIAN_POINT ( 'NONE',  ( 0.2984413201195192933, 1473.419535434050658, 219.3416222726238800 ) ) ;
#22187 = CARTESIAN_POINT ( 'NONE',  ( 11.86590139589999815, 1432.348266868109931, 151.0567667964980103 ) ) ;
#22188 = CARTESIAN_POINT ( 'NONE',  ( 2.500000000000000000, 1425.929641634319978, 183.3886485707629959 ) ) ;
#22189 = CARTESIAN_POINT ( 'NONE',  ( 0.2130409879942949947, 1451.905578552620000, 182.9902910394959861 ) ) ;
#22190 = DIRECTION ( 'NONE',  ( 0.000000000000000000, 0.000000000000000000, -1.000000000000000000 ) ) ;
#22191 = CARTESIAN_POINT ( 'NONE',  ( 10.03721076337500051, 1469.143571486790051, 209.2919969481099827 ) ) ;
#22192 = CARTESIAN_POINT ( 'NONE',  ( -5.931789999490000298, 1459.036866685989935, 218.1324649368089865 ) ) ;
#22193 = CARTESIAN_POINT ( 'NONE',  ( 9.704582620014180705, 1366.001145740636048, 210.6218459616991936 ) ) ;
#22194 = CARTESIAN_POINT ( 'NONE',  ( -24.16313269558360233, 1410.872200102120132, 267.2902278704040100 ) ) ;
#22195 = ORIENTED_EDGE ( 'NONE', *, *, #7641, .T. ) ;
#22196 = CARTESIAN_POINT ( 'NONE',  ( -3.538842271800570316, 1496.895311935370046, 181.4128009767959782 ) ) ;
#22197 = ADVANCED_FACE ( 'NONE', ( #11617 ), #52523, .F. ) ;
#22198 = AXIS2_PLACEMENT_3D ( 'NONE', #23467, #49797, #91773 ) ;
#22199 = ORIENTED_EDGE ( 'NONE', *, *, #67080, .T. ) ;
#22200 = ORIENTED_EDGE ( 'NONE', *, *, #84290, .T. ) ;
#22201 = CARTESIAN_POINT ( 'NONE',  ( 4.044321679994999919, 1517.001127920769704, 211.4073335515969916 ) ) ;
#22202 = CARTESIAN_POINT ( 'NONE',  ( -8.701122736030638904, 1447.991463143899864, 212.1854974882720057 ) ) ;
#22203 = EDGE_CURVE ( 'NONE', #96481, #110373, #74642, .T. ) ;
#22205 = PRESENTATION_STYLE_ASSIGNMENT (( #21657 ) ) ;
#22204 = CARTESIAN_POINT ( 'NONE',  ( -6.546951720715000533, 1516.606339319019980, 211.9964348928969855 ) ) ;
#22206 = CARTESIAN_POINT ( 'NONE',  ( -15.54206776589999883, 1455.451630440330064, 188.8651685368980395 ) ) ;
#22207 = CARTESIAN_POINT ( 'NONE',  ( -16.16160143211049771, 1461.177280122519960, 228.3234948423969968 ) ) ;
#22208 = B_SPLINE_SURFACE_WITH_KNOTS ( 'NONE', 5, 5, ( 
 ( #59114, #93239, #33881, #16505, #17047, #34443, #68619, #102721, #26015 ),
 ( #50163, #84291, #89331, #12626, #4233, #29964, #64713, #3703, #106674 ),
 ( #62517, #70920, #80935, #45149, #28326, #54658, #37833, #19909, #105035 ),
 ( #88238, #96639, #28881, #72018, #54109, #11530, #98829, #45705, #106135 ),
 ( #79843, #29411, #2600, #13147, #63076, #36725, #107231, #30521, #98275 ),
 ( #105598, #22089, #12068, #88787, #46805, #89877, #4766, #3152, #47331 ),
 ( #37284, #46260, #81460, #63612, #73092, #64157, #38366, #79290, #97728 ),
 ( #80387, #20999, #71476, #20449, #72543, #55203, #56287, #21548, #55760 ),
 ( #90416, #97176, #38909, #99920, #41687, #66364, #15360, #40028, #24317 ),
 ( #50104, #14264, #84229, #58500, #90976, #103086, #108338, #73655, #7530 ),
 ( #5883, #100484, #26386, #108888, #32731, #68985, #39483, #14817, #101019 ),
 ( #65798, #92628, #83678, #23765, #107786, #40579, #666, #49552, #92085 ),
 ( #83138, #41128, #6977, #5324, #31070, #15903, #75308, #57414, #49004 ),
 ( #32181, #77365, #34797, #60581, #13696, #65251, #99364, #22638, #6433 ),
 ( #74208, #57952, #47882, #109452, #66911, #82020, #56843, #74751, #48454 ),
 ( #23214, #82593, #31622, #91540, #2335, #86855, #53845, #10147, #61147 ),
 ( #45432, #11805, #17977, #94702, #36447, #52172, #70645, #43758, #104210 ),
 ( #53278, #69538, #77910, #28606, #35914, #44320, #70097, #2880, #78464 ),
 ( #28047, #62237, #87982, #79576, #3427, #87417, #36999, #71191, #1216 ),
 ( #19642, #86303, #35351, #27497, #10713, #103659, #9587, #1778, #26957 ),
 ( #61684, #44884, #95262, #18523, #37559, #52720, #79034, #104762, #95807 ),
 ( #96363, #105875, #19074, #11270, #105313, #62806, #96922, #20189, #54387 ),
 ( #88520, #45974, #80108, #71759, #29156, #56018, #13985, #29698, #56569 ),
 ( #99090, #99638, #90142, #81739, #108612, #90699, #107507, #5609, #54926 ) ),
 .UNSPECIFIED., .F., .F., .F.,
 ( 6, 3, 3, 3, 3, 3, 3, 6 ),
 ( 6, 3, 6 ),
 ( 24.02057840196890126, 75.98747947549999537, 109.6124278280000084, 126.4746888579999933, 132.7969126290000190, 135.9580245150000053, 139.1191364009999916, 143.3302516649309837 ),
 ( 0.000000000000000000, 1.000000000000000000, 2.000029560931110062 ),
 .UNSPECIFIED. ) ;
#22209 = VERTEX_POINT ( 'NONE', #11066 ) ;
#22210 = CARTESIAN_POINT ( 'NONE',  ( -26.79414277889999951, 1435.433175433119914, 135.2874649707979984 ) ) ;
#22211 = SHAPE_REPRESENTATION ( 'Feed Screw', ( #21632 ), #28938 ) ;
#22212 = CARTESIAN_POINT ( 'NONE',  ( 7.716252052974999387, 1516.810037859429940, 202.1795012402670011 ) ) ;
#22213 = CARTESIAN_POINT ( 'NONE',  ( 3.211131771843309668, 1415.841837342140252, 233.8555552817769865 ) ) ;
#22214 = CARTESIAN_POINT ( 'NONE',  ( 2.688586027246119947, 1509.006950727750109, 238.2845013960090057 ) ) ;
#22215 = CARTESIAN_POINT ( 'NONE',  ( -43.48865910597699980, 1440.913050606110119, 270.3367101327119713 ) ) ;
#22216 = DIRECTION ( 'NONE',  ( 0.000000000000000000, -0.9990482215818579093, -0.04361938736533144123 ) ) ;
#22217 = CARTESIAN_POINT ( 'NONE',  ( 0.06016749670950000128, 1397.283812747630009, 196.1836558358980085 ) ) ;
#22219 = EDGE_LOOP ( 'NONE', ( #81813, #29835, #2504, #92599 ) ) ;
#22218 = CARTESIAN_POINT ( 'NONE',  ( -8.589335072474291621, 1365.868898122805376, 207.6218459616988241 ) ) ;
#22220 = VERTEX_POINT ( 'NONE', #10507 ) ;
#22221 = DIRECTION ( 'NONE',  ( 0.01484500364079610613, 0.5669078173018522460, -0.8236474686107853049 ) ) ;
#22222 = CARTESIAN_POINT ( 'NONE',  ( -12.26760366359999921, 1381.106678608419998, 202.8726028786589950 ) ) ;
#22223 = CARTESIAN_POINT ( 'NONE',  ( -2.500000000000000000, 1419.443562236106345, 141.2948928672179818 ) ) ;
#22224 = CARTESIAN_POINT ( 'NONE',  ( -1.075916898909999864, 1485.885486078329905, 181.8684512949980103 ) ) ;
#22225 = CARTESIAN_POINT ( 'NONE',  ( 6.952166382295000169, 1517.213554313520035, 210.8305935944869987 ) ) ;
#22226 = CARTESIAN_POINT ( 'NONE',  ( 6.325405113577525107, 1460.162224217434868, 201.8389639430470481 ) ) ;
#22227 = CARTESIAN_POINT ( 'NONE',  ( 9.609447197979999800, 1453.954725363390025, 213.7354802858189942 ) ) ;
#22228 = CARTESIAN_POINT ( 'NONE',  ( -14.61523087940000032, 1430.144796240230107, 222.1530162304980252 ) ) ;
#22229 = CARTESIAN_POINT ( 'NONE',  ( 12.78667948450000047, 1416.822690122329959, 222.9174005869979851 ) ) ;
#22230 = CARTESIAN_POINT ( 'NONE',  ( 7.552141914295000369, 1510.542924508009946, 205.3415595432570058 ) ) ;
#22231 = ORIENTED_EDGE ( 'NONE', *, *, #83503, .F. ) ;
#22232 = CARTESIAN_POINT ( 'NONE',  ( -2.300729664794999962, 1516.923170579120097, 207.4211391557370234 ) ) ;
#22233 = EDGE_LOOP ( 'NONE', ( #5978, #14457, #87661, #5729, #47441 ) ) ;
#22234 = LINE ( 'NONE', #106810, #75939 ) ;
#22235 = CONICAL_SURFACE ( 'NONE', #99382, 12.50000000000000000, 0.02617993877989872875 ) ;
#22236 = CARTESIAN_POINT ( 'NONE',  ( -3.061616997868380553E-17, 1389.413060387289988, 209.1218459616989946 ) ) ;
#22237 = VERTEX_POINT ( 'NONE', #86654 ) ;
#22238 = CARTESIAN_POINT ( 'NONE',  ( -5.106893092629549713, 1391.877272788475011, 214.4361776400186557 ) ) ;
#22239 = CARTESIAN_POINT ( 'NONE',  ( 23.92107583702020079, 1452.077735920189980, 137.0198744514089810 ) ) ;
#22240 = CARTESIAN_POINT ( 'NONE',  ( 13.53550618839999942, 1416.067629290630066, 196.4934937118979974 ) ) ;
#22241 = LINE ( 'NONE', #91127, #27086 ) ;
#22242 = CARTESIAN_POINT ( 'NONE',  ( 18.92936377790000080, 1409.738736466630144, 196.3471921528980033 ) ) ;
#22243 = CARTESIAN_POINT ( 'NONE',  ( -27.68254001883949655, 1507.989615300039986, 210.5775529569929745 ) ) ;
#22244 = CARTESIAN_POINT ( 'NONE',  ( -14.05847445561479958, 1379.589564867563695, 211.7968567430240228 ) ) ;
#22245 = CARTESIAN_POINT ( 'NONE',  ( 3.074703527060000052, 1441.333178254290033, 218.5515148082390056 ) ) ;
#22246 = CARTESIAN_POINT ( 'NONE',  ( -8.881784196999999612E-15, 1446.564900598709983, 126.8032249175980155 ) ) ;
#22247 = CARTESIAN_POINT ( 'NONE',  ( 2.500000000000000000, 1439.361286091369948, 161.1256395968530057 ) ) ;
#22248 = CARTESIAN_POINT ( 'NONE',  ( 2.487103419534999915, 1516.577434278289957, 215.6681487122470173 ) ) ;
#22249 = VERTEX_POINT ( 'NONE', #45236 ) ;
#22250 = CARTESIAN_POINT ( 'NONE',  ( 7.712420241246189967, 1516.663706873209776, 208.1377185825360243 ) ) ;
#22251 = CARTESIAN_POINT ( 'NONE',  ( -29.18142758420000149, 1466.479558604430167, 269.9486951468979896 ) ) ;
#22252 = CARTESIAN_POINT ( 'NONE',  ( -2.500000000000000000, 1448.894380913990062, 183.1110194797979887 ) ) ;
#22253 = CARTESIAN_POINT ( 'NONE',  ( -2.885915196579980080, 1421.960918650529948, 112.2554875371340017 ) ) ;
#22254 = FACE_OUTER_BOUND ( 'NONE', #1963, .T. ) ;
#22255 = LINE ( 'NONE', #39647, #37059 ) ;
#22256 = CARTESIAN_POINT ( 'NONE',  ( -21.38516915558008336, 1524.726013923371283, 180.3939891059723664 ) ) ;
#22257 = CARTESIAN_POINT ( 'NONE',  ( -1.918070871662279853, 1477.784538725520179, 183.2207360801660059 ) ) ;
#22258 = CARTESIAN_POINT ( 'NONE',  ( -105.8429516820000060, 1379.429574992919925, 301.1876983431590133 ) ) ;
#22259 = CARTESIAN_POINT ( 'NONE',  ( -21.53981368633656857, 1523.542365884045694, 183.9340804168635088 ) ) ;
#22260 = CARTESIAN_POINT ( 'NONE',  ( 27.70013467925890183, 1440.913060387809992, 229.9159422604259930 ) ) ;
#22261 = CARTESIAN_POINT ( 'NONE',  ( -10.11770193674129992, 1472.442116771029987, 210.2941300317889954 ) ) ;
#22262 = DIRECTION ( 'NONE',  ( 0.9858563016923833633, 0.000000000000000000, 0.1675928173085483863 ) ) ;
#22263 = ORIENTED_EDGE ( 'NONE', *, *, #102772, .T. ) ;
#22264 = VERTEX_POINT ( 'NONE', #62615 ) ;
#22265 = CIRCLE ( 'NONE', #29407, 0.9999999999999991118 ) ;
#22266 = CARTESIAN_POINT ( 'NONE',  ( 10.55879509197319877, 1480.973079402069970, 209.1396683372450127 ) ) ;
#22267 = CARTESIAN_POINT ( 'NONE',  ( 0.000000000000000000, 1511.187213306747708, 209.1218459616979999 ) ) ;
#22268 = CARTESIAN_POINT ( 'NONE',  ( -2.858448621680000024, 1443.821599769190016, 199.4616741486989895 ) ) ;
#22269 = CARTESIAN_POINT ( 'NONE',  ( 7.550320201100000794, 1423.033199310010104, 195.6993168036990198 ) ) ;
#22270 = DIRECTION ( 'NONE',  ( 0.9455185755993178454, 0.000000000000000000, -0.3255681544571538688 ) ) ;
#22271 = AXIS2_PLACEMENT_3D ( 'NONE', #64593, #4662, #105475 ) ;
#22272 = AXIS2_PLACEMENT_3D ( 'NONE', #81641, #56471, #109083 ) ;
#22273 = CARTESIAN_POINT ( 'NONE',  ( 15.10324330609999954, 1409.440477264029823, 192.5109551743979921 ) ) ;
#22274 = CARTESIAN_POINT ( 'NONE',  ( 2.310682350337450064, 1508.551704408389924, 219.5967718590839866 ) ) ;
#22275 = CARTESIAN_POINT ( 'NONE',  ( -48.77857038591120187, 1383.813927605060144, 258.8276066785749663 ) ) ;
#22276 = CARTESIAN_POINT ( 'NONE',  ( -4.805077596034999843, 1510.399296111369949, 201.5734650597370035 ) ) ;
#22277 = CARTESIAN_POINT ( 'NONE',  ( -15.54069288340000021, 1507.627022993330229, 192.2862817006979981 ) ) ;
#22278 = CARTESIAN_POINT ( 'NONE',  ( -11.41800801098339946, 1501.040032621129967, 208.6024801871049874 ) ) ;
#22279 = CARTESIAN_POINT ( 'NONE',  ( 1.476596736730000137, 1465.998869369329896, 235.0546012516979886 ) ) ;
#22280 = ORIENTED_EDGE ( 'NONE', *, *, #5122, .T. ) ;
#22281 = CARTESIAN_POINT ( 'NONE',  ( -0.5361601820109999084, 1452.003350861930130, 183.1486451269979909 ) ) ;
#22282 = EDGE_CURVE ( 'NONE', #22747, #74953, #98128, .T. ) ;
#22283 = CARTESIAN_POINT ( 'NONE',  ( -37.54707235840000124, 1380.310470099769873, 214.8595787094589866 ) ) ;
#22284 = ADVANCED_FACE ( 'NONE', ( #35702 ), #10010, .T. ) ;
#22285 = CARTESIAN_POINT ( 'NONE',  ( -3.229911446790000085, 1475.410210782889862, 198.9236622250990081 ) ) ;
#22287 = ORIENTED_EDGE ( 'NONE', *, *, #43609, .F. ) ;
#22286 = CARTESIAN_POINT ( 'NONE',  ( -31.56779946216799360, 1525.408327360765952, 216.2063941007895380 ) ) ;
#22288 = CARTESIAN_POINT ( 'NONE',  ( -20.36852575855199987, 1464.956479398600095, 210.9457983963280014 ) ) ;
#22289 = VERTEX_POINT ( 'NONE', #5411 ) ;
#22290 = PRODUCT ( 'Grinding Plate', 'Grinding Plate', '', ( #17379 ) ) ;
#22291 = CARTESIAN_POINT ( 'NONE',  ( -13.85142996899100076, 1390.139986880880087, 212.7740396815260056 ) ) ;
#22292 = CARTESIAN_POINT ( 'NONE',  ( 34.51169404606030611, 1437.059671538590237, 136.5459531931829815 ) ) ;
#22293 = CARTESIAN_POINT ( 'NONE',  ( -4.759967386468179740, 1475.369894740059181, 199.9752752562233979 ) ) ;
#22294 = CARTESIAN_POINT ( 'NONE',  ( -11.60004869885204215, 1426.371424667298925, 136.9558864814476919 ) ) ;
#22295 = CARTESIAN_POINT ( 'NONE',  ( -104.8261132509999953, 1380.717247260959994, 300.0167969450589567 ) ) ;
#22296 = CYLINDRICAL_SURFACE ( 'NONE', #67866, 2.000000000000003553 ) ;
#22297 = CARTESIAN_POINT ( 'NONE',  ( 3.348647037815445149, 1523.530870145311383, 242.0864809827354520 ) ) ;
#22298 = CARTESIAN_POINT ( 'NONE',  ( 8.233640524757710466, 1409.200585450159906, 196.6252762661590054 ) ) ;
#22299 = CARTESIAN_POINT ( 'NONE',  ( 18.02093605269999799, 1424.326858638329895, 225.1991111336980111 ) ) ;
#22300 = CARTESIAN_POINT ( 'NONE',  ( 4.617353517619999792, 1460.098150474590057, 228.0971968620989969 ) ) ;
#22301 = CARTESIAN_POINT ( 'NONE',  ( -19.07203922379999739, 1485.640791703330024, 189.6106623856980207 ) ) ;
#22302 = CARTESIAN_POINT ( 'NONE',  ( 19.59884465730837277, 1526.382868172864164, 237.0995590530538948 ) ) ;
#22303 = EDGE_CURVE ( 'NONE', #58921, #94817, #22183, .T. ) ;
#22304 = CARTESIAN_POINT ( 'NONE',  ( -2.499989904720139933, 1448.906960178189820, 183.3908600069959789 ) ) ;
#22305 = ORIENTED_EDGE ( 'NONE', *, *, #62285, .F. ) ;
#22306 = ORIENTED_EDGE ( 'NONE', *, *, #91361, .F. ) ;
#22307 = CONICAL_SURFACE ( 'NONE', #38399, 1.000000000000009104, 0.7853981633970000820 ) ;
#22308 = CARTESIAN_POINT ( 'NONE',  ( -7.321627547103849665, 1508.611138448550037, 214.6350682845269944 ) ) ;
#22309 = CARTESIAN_POINT ( 'NONE',  ( 17.96600282473259824, 1457.758676852030021, 228.7894647061090154 ) ) ;
#22310 = CARTESIAN_POINT ( 'NONE',  ( -12.65205114049999935, 1435.423691554170091, 150.7971429281979852 ) ) ;
#22311 = CARTESIAN_POINT ( 'NONE',  ( 3.320959845659019973E-10, 1465.220663907560038, 238.5330492740649788 ) ) ;
#22312 = CARTESIAN_POINT ( 'NONE',  ( -20.36866774749589837, 1500.371803671309863, 190.6068050527740070 ) ) ;
#22313 = CARTESIAN_POINT ( 'NONE',  ( -14.67572137840000046, 1420.538682257900064, 213.1455671837790078 ) ) ;
#22314 = CARTESIAN_POINT ( 'NONE',  ( -109.6996574960000004, 1385.658284643630168, 311.3154365352589821 ) ) ;
#22315 = VECTOR ( 'NONE', #102512, 1000.000000000000114 ) ;
#22316 = CARTESIAN_POINT ( 'NONE',  ( -7.658720568233269965, 1511.445028088800200, 215.2217939408990048 ) ) ;
#22317 = CARTESIAN_POINT ( 'NONE',  ( -10.61207710156363149, 1361.707344756497832, 209.6218459617033432 ) ) ;
#22318 = CARTESIAN_POINT ( 'NONE',  ( -46.15243863885639541, 1440.913067582900112, 268.2044766056350227 ) ) ;
#22319 = CARTESIAN_POINT ( 'NONE',  ( -19.39897567239999887, 1468.962688716530010, 192.4463568245979843 ) ) ;
#22320 = CARTESIAN_POINT ( 'NONE',  ( 6.935801261535000428, 1516.621991115350056, 207.9918434378369909 ) ) ;
#22321 = CARTESIAN_POINT ( 'NONE',  ( -9.818885166255999053, 1447.613981975209754, 210.5167627897619980 ) ) ;
#22322 = CARTESIAN_POINT ( 'NONE',  ( 1.344050583552389933, 1408.775600028340023, 223.1975148624649989 ) ) ;
#22323 = CARTESIAN_POINT ( 'NONE',  ( -13.47209471068070030, 1435.515832415140039, 150.2099290526579694 ) ) ;
#22324 = CARTESIAN_POINT ( 'NONE',  ( -7.543563443440000071, 1384.985423750119935, 219.0866481152289964 ) ) ;
#22325 = B_SPLINE_SURFACE_WITH_KNOTS ( 'NONE', 5, 5, ( 
 ( #4158, #108248, #72467, #40492, #47802, #99279 ),
 ( #30439, #38832, #74670, #23127, #98192, #31538 ),
 ( #106597, #74119, #14736, #57332, #22005, #47253 ),
 ( #73572, #32097, #108803, #48924, #82508, #83052 ),
 ( #81377, #107704, #13614, #29882, #21465, #90334 ),
 ( #56202, #5807, #4692, #66284, #65714, #30989 ),
 ( #65164, #56759, #55674, #14180, #57869, #38285 ),
 ( #73010, #91457, #81937, #6345, #39947, #64073 ),
 ( #99835, #100400, #107146, #64624, #89795, #23684 ) ),
 .UNSPECIFIED., .F., .F., .F.,
 ( 6, 3, 6 ),
 ( 6, 6 ),
 ( 50.07766623440000586, 62.52389936639999490, 69.76872775750000244 ),
 ( 0.000000000000000000, 2.000000000000000000 ),
 .UNSPECIFIED. ) ;
#22326 = ADVANCED_FACE ( 'NONE', ( #72630 ), #4852, .F. ) ;
#22327 = CARTESIAN_POINT ( 'NONE',  ( 4.221337299212926553, 1424.740940193975348, 226.9639360934303056 ) ) ;
#22328 = DIRECTION ( 'NONE',  ( 0.5877852522924709167, 0.000000000000000000, 0.8090169943749491166 ) ) ;
#22329 = ORIENTED_EDGE ( 'NONE', *, *, #55979, .T. ) ;
#22330 = CARTESIAN_POINT ( 'NONE',  ( 35.93744661969999754, 1433.966419429300004, 254.6052924894979697 ) ) ;
#22331 = CARTESIAN_POINT ( 'NONE',  ( -27.53546928409999950, 1508.129852613929870, 205.2718258483980094 ) ) ;
#22333 = CARTESIAN_POINT ( 'NONE',  ( -0.02955819112566620069, 1517.051704408389924, 225.0080808726450243 ) ) ;
#22332 = CARTESIAN_POINT ( 'NONE',  ( -11.59563781346980171, 1491.413760601690001, 206.8061924195220058 ) ) ;
#22334 = EDGE_CURVE ( 'NONE', #105623, #109427, #34559, .T. ) ;
#22335 = CARTESIAN_POINT ( 'NONE',  ( 1.447786046769359292, 1507.396806431331242, 181.1008358461068610 ) ) ;
#22336 = CARTESIAN_POINT ( 'NONE',  ( -8.692320600269997755, 1418.992648084129996, 231.7739325360979876 ) ) ;
#22337 = CARTESIAN_POINT ( 'NONE',  ( -4.637174521050656750, 1378.050660721826034, 214.3535596345795966 ) ) ;
#22338 = CARTESIAN_POINT ( 'NONE',  ( -17.43240527195019851, 1452.304307381109993, 145.9273250573520215 ) ) ;
#22339 = CARTESIAN_POINT ( 'NONE',  ( 28.27346568420000139, 1451.774185556130078, 135.7527207400979989 ) ) ;
#22340 = VERTEX_POINT ( 'NONE', #67546 ) ;
#22341 = CARTESIAN_POINT ( 'NONE',  ( -108.0838200535449971, 1378.913060387289988, 299.8681954501259952 ) ) ;
#22342 = CARTESIAN_POINT ( 'NONE',  ( -2.372478608332516892, 1501.977400791986611, 174.8996806668726549 ) ) ;
#22343 = CARTESIAN_POINT ( 'NONE',  ( 15.87012503028160282, 1422.606634508830211, 228.1220680369120259 ) ) ;
#22344 = EDGE_LOOP ( 'NONE', ( #34277, #14674, #28041, #48305, #87760 ) ) ;
#22345 = ORIENTED_EDGE ( 'NONE', *, *, #24808, .F. ) ;
#22346 = CARTESIAN_POINT ( 'NONE',  ( 9.675872734536000053, 1452.418772690649803, 210.2673697975640152 ) ) ;
#22347 = CARTESIAN_POINT ( 'NONE',  ( -22.82106830618239712, 1409.719725320740054, 209.4798526508069756 ) ) ;
#22348 = ORIENTED_EDGE ( 'NONE', *, *, #65817, .T. ) ;
#22349 = CARTESIAN_POINT ( 'NONE',  ( 4.237005577396040223, 1508.610336687640029, 204.5878445095659970 ) ) ;
#22350 = CARTESIAN_POINT ( 'NONE',  ( -8.537822636805000087, 1517.051704408389924, 205.6971256312070011 ) ) ;
#22351 = CARTESIAN_POINT ( 'NONE',  ( -24.46348847106868618, 1436.579504986744041, 139.1503910763263718 ) ) ;
#22352 = CARTESIAN_POINT ( 'NONE',  ( 16.81611548245470189, 1526.382868172864164, 234.5451076435186053 ) ) ;
#22353 = VERTEX_POINT ( 'NONE', #17074 ) ;
#22354 = CARTESIAN_POINT ( 'NONE',  ( 46.02601385349320395, 1443.739552433979952, 268.2087485089310235 ) ) ;
#22355 = B_SPLINE_CURVE_WITH_KNOTS ( 'NONE', 5,
 ( #59148, #37791, #79804, #106631, #72502, #71979, #11490, #54070, #106092, #20959, #37238, #70877, #61916, #55163, #28839, #62475, #87083, #71437 ),
 .UNSPECIFIED., .F., .F.,
 ( 6, 3, 3, 3, 3, 6 ),
 ( 10.40199318109999993, 19.90315615969999996, 26.66638367519999875, 26.99360131220000270, 28.03535140669999848, 29.40431913829999999 ),
 .UNSPECIFIED. ) ;
#22356 = CIRCLE ( 'NONE', #38530, 2.000000000000001776 ) ;
#22357 = CARTESIAN_POINT ( 'NONE',  ( -13.15726442299999910, 1416.543503932829935, 221.9001046233979935 ) ) ;
#22358 = CARTESIAN_POINT ( 'NONE',  ( -7.447340581099999746, 1425.934151271280143, 204.0825129966889904 ) ) ;
#22359 = CARTESIAN_POINT ( 'NONE',  ( -1.713317447804999949, 1516.660388280709867, 204.5138242629670060 ) ) ;
#22360 = ORIENTED_EDGE ( 'NONE', *, *, #100694, .F. ) ;
#22361 = CARTESIAN_POINT ( 'NONE',  ( 13.51222313460685776, 1443.793701217813350, 188.0482377676655119 ) ) ;
#22362 = ORIENTED_EDGE ( 'NONE', *, *, #108, .F. ) ;
#22363 = VERTEX_POINT ( 'NONE', #8702 ) ;
#22364 = CARTESIAN_POINT ( 'NONE',  ( -11.01402028494999996, 1481.503834766900127, 208.8098579862920019 ) ) ;
#22365 = CARTESIAN_POINT ( 'NONE',  ( -29.00779973304124937, 1526.382868172863937, 217.2942086403127178 ) ) ;
#22366 = CARTESIAN_POINT ( 'NONE',  ( -12.82673418834020040, 1512.305164330070056, 193.9674763234050090 ) ) ;
#22367 = CARTESIAN_POINT ( 'NONE',  ( 7.191291722693810229, 1452.661934946750080, 151.5666603189569912 ) ) ;
#22368 = B_SPLINE_CURVE_WITH_KNOTS ( 'NONE', 3,
 ( #12699, #89953, #46883, #98900, #81008, #4315, #45783, #22170, #21626, #64791, #88312, #20527, #13227, #47417, #81539, #4840, #36805, #30603, #56368, #201, #77441, #39558, #16388, #31144, #75782, #102601, #42732, #110480, #34324, #76891, #15833, #50583, #16935, #8013, #42180, #26463, #8560, #84166, #94782, #109935, #25347, #17491, #84713, #93653, #60658, #33758, #33213, #94216, #47959, #9127, #51689, #68503, #76330, #67955, #25902, #43293, #742, #67402, #102065, #41628, #59540, #60100, #51137, #85263, #24788, #58990, #82100 ),
 .UNSPECIFIED., .F., .F.,
 ( 4, 3, 3, 3, 3, 3, 3, 3, 3, 3, 3, 3, 3, 3, 3, 3, 3, 3, 3, 3, 3, 3, 4 ),
 ( 75.70921875734188689, 77.32181385522589778, 80.91190279622159665, 84.29463333639999689, 84.51613493880849148, 84.74302641768430533, 84.97629439946371122, 85.21717448936620087, 85.47327895300539069, 85.74291095813249797, 86.03175759668660305, 86.35217251418519879, 86.77738762425410357, 87.13887373325040642, 87.44388152653429813, 87.72348157678361247, 87.98689693641620124, 88.23857955550479915, 88.48405268548279423, 88.71622240253540781, 88.94338408580298960, 89.16444926645201008, 89.22047207541669422 ),
 .UNSPECIFIED. ) ;
#22369 = CARTESIAN_POINT ( 'NONE',  ( 9.539810668950000405, 1420.903745483679813, 197.1733355697989793 ) ) ;
#22370 = DIRECTION ( 'NONE',  ( -6.123233995736769734E-17, -1.000000000000000000, -1.124819836996399911E-32 ) ) ;
#22371 = CARTESIAN_POINT ( 'NONE',  ( -109.1922049499590486, 1382.216944093681832, 297.5007580629779227 ) ) ;
#22372 = CARTESIAN_POINT ( 'NONE',  ( -10.97588638302280017, 1432.726111932770209, 151.7698415246060222 ) ) ;
#22373 = CARTESIAN_POINT ( 'NONE',  ( 0.02589805802711389951, 1409.083993410460153, 232.4593697285492340 ) ) ;
#22375 = CARTESIAN_POINT ( 'NONE',  ( -106.7031369453130054, 1391.913060387289988, 306.7753017128669626 ) ) ;
#22374 = DIRECTION ( 'NONE',  ( 1.098156484365624113E-07, 0.8818472373848361689, 0.4715352053842007951 ) ) ;
#22376 = CARTESIAN_POINT ( 'NONE',  ( 10.70518913711110010, 1423.800132577800014, 206.7158561157320094 ) ) ;
#22377 = CARTESIAN_POINT ( 'NONE',  ( -9.819155800674218781, 1439.994030334630224, 207.1637469923470007 ) ) ;
#22378 = CARTESIAN_POINT ( 'NONE',  ( 11.74015320060000001, 1428.979986575930070, 144.1938086916980239 ) ) ;
#22379 = ORIENTED_EDGE ( 'NONE', *, *, #76306, .F. ) ;
#22380 = CARTESIAN_POINT ( 'NONE',  ( 20.41675352909999930, 1440.913060387330006, 219.6133834379979817 ) ) ;
#22381 = CARTESIAN_POINT ( 'NONE',  ( -17.03149518429903608, 1417.396562231937196, 206.8274202490092648 ) ) ;
#22382 = CARTESIAN_POINT ( 'NONE',  ( -92.43541484565200506, 1384.963896024199812, 309.4382857164679876 ) ) ;
#22383 = AXIS2_PLACEMENT_3D ( 'NONE', #81635, #55370, #64881 ) ;
#22384 = CARTESIAN_POINT ( 'NONE',  ( -8.312690972840000470, 1386.943181267609816, 199.8519208937690053 ) ) ;
#22385 = CARTESIAN_POINT ( 'NONE',  ( 11.11857203984600062, 1427.722971555709819, 210.2004789491199972 ) ) ;
#22387 = ORIENTED_EDGE ( 'NONE', *, *, #82542, .T. ) ;
#22386 = CARTESIAN_POINT ( 'NONE',  ( -6.816032832730000379, 1464.119504676089946, 200.4313534491789994 ) ) ;
#22388 = CARTESIAN_POINT ( 'NONE',  ( 16.81223226430000039, 1414.913060387329779, 210.6693098017280192 ) ) ;
#22389 = CARTESIAN_POINT ( 'NONE',  ( -1.669693912109999845, 1443.913060387330006, 150.7596247526980164 ) ) ;
#22390 = CARTESIAN_POINT ( 'NONE',  ( -16.76063698560000148, 1417.345490017750080, 208.1330266677999816 ) ) ;
#22391 = CARTESIAN_POINT ( 'NONE',  ( -12.78776258895079998, 1416.851343896850040, 195.5391574246120001 ) ) ;
#22392 = CARTESIAN_POINT ( 'NONE',  ( 12.85916294179999930, 1469.933320803330162, 268.3665355202980436 ) ) ;
#22393 = CARTESIAN_POINT ( 'NONE',  ( 1.228114002177200126, 1450.757138880049979, 181.5372592238319953 ) ) ;
#22394 = CIRCLE ( 'NONE', #110034, 2.000000000000002220 ) ;
#22395 = CARTESIAN_POINT ( 'NONE',  ( 4.347845440834370301, 1459.306986539150103, 200.4470736973389933 ) ) ;
#22396 = CARTESIAN_POINT ( 'NONE',  ( -107.2768973518786311, 1390.144646088828495, 299.2871404242311542 ) ) ;
#22397 = CARTESIAN_POINT ( 'NONE',  ( 17.08931884779999777, 1422.113171145530032, 226.7814393765980014 ) ) ;
#22398 = CARTESIAN_POINT ( 'NONE',  ( 1.188224663175142970, 1410.329429681951297, 232.8079325243718642 ) ) ;
#22399 = CARTESIAN_POINT ( 'NONE',  ( 3.319698225923770174, 1474.465735597630101, 220.0484424645880210 ) ) ;
#22400 = CARTESIAN_POINT ( 'NONE',  ( -16.19082880930000101, 1409.478456588029985, 225.0103237202980040 ) ) ;
#22401 = CARTESIAN_POINT ( 'NONE',  ( -0.4986843622567649348, 1508.982343520079894, 238.8510830230749775 ) ) ;
#22402 = CARTESIAN_POINT ( 'NONE',  ( -1.340352705809999989, 1422.344613506229962, 228.3239229121980145 ) ) ;
#22403 = CARTESIAN_POINT ( 'NONE',  ( -27.12584415899999968, 1450.023914463320125, 136.5580354838980099 ) ) ;
#22404 = CARTESIAN_POINT ( 'NONE',  ( 21.80961351509229473, 1523.919943579690425, 183.3321359269316986 ) ) ;
#22405 = CARTESIAN_POINT ( 'NONE',  ( 7.016443067423660379E-06, 1406.952554981560070, 196.1216945173329975 ) ) ;
#22406 = CARTESIAN_POINT ( 'NONE',  ( 12.54203963119180010, 1427.020850620109968, 206.2427846923719983 ) ) ;
#22407 = CARTESIAN_POINT ( 'NONE',  ( -5.386185223340929973, 1432.347042777500064, 154.6076275972019971 ) ) ;
#22408 = CARTESIAN_POINT ( 'NONE',  ( -8.403208055529999498, 1415.931391677329884, 224.9948233075980113 ) ) ;
#22409 = CARTESIAN_POINT ( 'NONE',  ( 0.2079255321337470097, 1458.515647613060082, 183.0167680703569886 ) ) ;
#22410 = CARTESIAN_POINT ( 'NONE',  ( -9.949544832400000871, 1409.260506149029879, 198.1586515674979978 ) ) ;
#22411 = CARTESIAN_POINT ( 'NONE',  ( -0.3212355716730000421, 1418.619114157530021, 184.6997714626980098 ) ) ;
#22412 = CARTESIAN_POINT ( 'NONE',  ( -7.701966621347670738, 1441.125018359749902, 154.1230950350289959 ) ) ;
#22413 = CARTESIAN_POINT ( 'NONE',  ( 11.94142139689999915, 1433.615122234779847, 147.9453765516980184 ) ) ;
#22414 = CARTESIAN_POINT ( 'NONE',  ( -27.69668320559999941, 1436.360686759009923, 136.6994006594979965 ) ) ;
#22415 = DIRECTION ( 'NONE',  ( -1.156023075842281927E-31, 1.000000000000000000, -1.698192320643030073E-16 ) ) ;
#22416 = VERTEX_POINT ( 'NONE', #41764 ) ;
#22417 = CARTESIAN_POINT ( 'NONE',  ( -16.88555899346171785, 1525.556089352344770, 181.6768889465036523 ) ) ;
#22418 = CARTESIAN_POINT ( 'NONE',  ( 3.412268725760000176, 1476.681763699690009, 198.4748995137989880 ) ) ;
#22419 = CARTESIAN_POINT ( 'NONE',  ( -103.6308070735486524, 1379.927247807891035, 304.9220808158690375 ) ) ;
#22420 = CARTESIAN_POINT ( 'NONE',  ( -11.43222421799999999, 1490.997350406890064, 208.8577229060449838 ) ) ;
#22421 = B_SPLINE_CURVE_WITH_KNOTS ( 'NONE', 3,
 ( #69853, #110717, #26704, #987, #77136, #1530, #60901, #102305, #441, #34008, #95026, #18296, #35112, #102848, #52489, #60332, #94448, #17727, #51929, #25592, #103971, #9367, #68202, #77674, #50818, #27268, #61451, #68745, #95575, #26141, #50288, #67637, #84417, #7702, #41861, #16622, #84949, #76014 ),
 .UNSPECIFIED., .F., .F.,
 ( 4, 2, 2, 1, 1, 1, 1, 2, 2, 2, 1, 1, 1, 1, 2, 2, 2, 2, 2, 2, 2, 2, 4 ),
 ( 0.000000000000000000, 0.2499999999998901989, 0.3749999999998352984, 0.4374999999998089306, 0.4687499999997937761, 0.4843749999997875033, 0.4921874999997847278, 0.4960937499997840616, 0.4999999999997833955, 0.6249999999998385736, 0.6874999999998663291, 0.7187499999998795408, 0.7343749999998852029, 0.7421874999998882005, 0.7460937499998898659, 0.7499999999998916422, 0.8124999999999265032, 0.8437499999999439337, 0.8593749999999512612, 0.8671874999999549249, 0.8710937499999568123, 0.8749999999999585887, 1.000000000000000000 ),
 .UNSPECIFIED. ) ;
#22422 = DIRECTION ( 'NONE',  ( 0.4090087482554189968, 0.000000000000000000, 0.9125304618754023211 ) ) ;
#22423 = DIRECTION ( 'NONE',  ( 0.000000000000000000, 0.000000000000000000, -1.000000000000000000 ) ) ;
#22424 = CARTESIAN_POINT ( 'NONE',  ( 33.05090165468867980, 1417.318103022701280, 269.2938148436854249 ) ) ;
#22425 = CARTESIAN_POINT ( 'NONE',  ( 21.31406882950000181, 1471.311257372230102, 210.6477718704180120 ) ) ;
#22426 = CARTESIAN_POINT ( 'NONE',  ( 2.372478608332516892, 1522.382868172863937, 243.3440112565233449 ) ) ;
#22427 = CARTESIAN_POINT ( 'NONE',  ( 2.500000011050000026, 1436.902470912989884, 183.4044075271980034 ) ) ;
#22428 = CARTESIAN_POINT ( 'NONE',  ( -65.13748019436710024, 1385.087367150850014, 255.3513583967259706 ) ) ;
#22429 = CARTESIAN_POINT ( 'NONE',  ( -3.246772394788719929, 1511.187213306747708, 241.0944358625217774 ) ) ;
#22430 = CARTESIAN_POINT ( 'NONE',  ( -24.89775034519999863, 1442.835538705840008, 210.5176537872779932 ) ) ;
#22431 = CARTESIAN_POINT ( 'NONE',  ( -27.78835558220000124, 1451.082283293030059, 136.3521884964980018 ) ) ;
#22432 = CARTESIAN_POINT ( 'NONE',  ( -16.57709675719999964, 1409.867837143930046, 226.0335794272980081 ) ) ;
#22433 = EDGE_CURVE ( 'NONE', #34842, #51303, #78859, .T. ) ;
#22435 = ORIENTED_EDGE ( 'NONE', *, *, #67787, .T. ) ;
#22434 = CARTESIAN_POINT ( 'NONE',  ( 2.589318363809999912, 1507.773265401989875, 217.6873885498590084 ) ) ;
#22436 = CARTESIAN_POINT ( 'NONE',  ( -109.8252913419999999, 1384.913429218860074, 311.3807689642590049 ) ) ;
#22438 = CARTESIAN_POINT ( 'NONE',  ( 10.95090191305459904, 1471.837486416480033, 212.3990077965439980 ) ) ;
#22437 = AXIS2_PLACEMENT_3D ( 'NONE', #7203, #41903, #76604 ) ;
#22439 = CARTESIAN_POINT ( 'NONE',  ( 18.53418652026280000, 1507.620785850910124, 188.5293807599879869 ) ) ;
#22440 = CARTESIAN_POINT ( 'NONE',  ( -109.8284014480000081, 1384.811872824480133, 311.3795260262589863 ) ) ;
#22441 = CARTESIAN_POINT ( 'NONE',  ( -0.1213678470291219974, 1420.435499575030235, 183.0499996374540217 ) ) ;
#22442 = CARTESIAN_POINT ( 'NONE',  ( 0.4118372133359999854, 1466.367795784230111, 235.6625353782980028 ) ) ;
#22443 = ADVANCED_FACE ( 'NONE', ( #14896 ), #69456, .T. ) ;
#22444 = CARTESIAN_POINT ( 'NONE',  ( 21.69352049569999963, 1409.670614816029911, 212.9121036625780050 ) ) ;
#22445 = B_SPLINE_SURFACE_WITH_KNOTS ( 'NONE', 3, 1, ( 
 ( #83097, #65759 ),
 ( #31581, #90937 ),
 ( #6933, #74714 ),
 ( #16410, #50604 ) ),
 .UNSPECIFIED., .F., .F., .F.,
 ( 4, 4 ),
 ( 2, 2 ),
 ( 0.000000000000000000, 1.000000000000000000 ),
 ( 0.000000000000000000, 1.000000000000000000 ),
 .UNSPECIFIED. ) ;
#22446 = CARTESIAN_POINT ( 'NONE',  ( 0.4512475842468137710, 1450.897302474460503, 181.2782477060373481 ) ) ;
#22447 = CARTESIAN_POINT ( 'NONE',  ( -9.495330813260000724, 1465.238080356989940, 228.3114829157989902 ) ) ;
#22448 = DIRECTION ( 'NONE',  ( 0.9900965937346508650, -0.1403878024439509931, 3.790652827686682019E-16 ) ) ;
#22450 = DIRECTION ( 'NONE',  ( 1.000000000000000000, 0.000000000000000000, 0.000000000000000000 ) ) ;
#22449 = CARTESIAN_POINT ( 'NONE',  ( -3.196839497313484380, 1511.813433987939788, 201.1737305778248697 ) ) ;
#22451 = CARTESIAN_POINT ( 'NONE',  ( 7.108361874469999897, 1480.745134477889906, 207.3349235958489771 ) ) ;
#22452 = CARTESIAN_POINT ( 'NONE',  ( -106.4559248862599361, 1358.631207110789774, 297.2777708435190220 ) ) ;
#22453 = DIRECTION ( 'NONE',  ( -0.000000000000000000, -1.000000000000000000, -0.000000000000000000 ) ) ;
#22454 = CARTESIAN_POINT ( 'NONE',  ( -0.9341545002969999789, 1415.826342224429936, 233.3075236840979869 ) ) ;
#22455 = CARTESIAN_POINT ( 'NONE',  ( 9.971295257850000482, 1364.502667329740007, 210.6218459616991936 ) ) ;
#22456 = CARTESIAN_POINT ( 'NONE',  ( -5.010423001364999962, 1516.929569650079884, 205.0907035804270038 ) ) ;
#22457 = CARTESIAN_POINT ( 'NONE',  ( -17.64168070010000022, 1423.919165630929911, 226.5634843356980070 ) ) ;
#22458 = ORIENTED_EDGE ( 'NONE', *, *, #88472, .T. ) ;
#22459 = CARTESIAN_POINT ( 'NONE',  ( -32.36513277069977335, 1523.847248782568386, 216.1093201122535561 ) ) ;
#22460 = CARTESIAN_POINT ( 'NONE',  ( -4.229761814456889368, 1441.533620886849803, 164.9558944606160082 ) ) ;
#22462 = ORIENTED_EDGE ( 'NONE', *, *, #29916, .F. ) ;
#22461 = CARTESIAN_POINT ( 'NONE',  ( -67.99044070674879947, 1379.746877581120089, 279.4179884241240188 ) ) ;
#22463 = ORIENTED_EDGE ( 'NONE', *, *, #7202, .F. ) ;
#22464 = CARTESIAN_POINT ( 'NONE',  ( -11.84045693795016874, 1377.795153884136198, 212.6165618655485900 ) ) ;
#22465 = ORIENTED_EDGE ( 'NONE', *, *, #71459, .T. ) ;
#22466 = CARTESIAN_POINT ( 'NONE',  ( 1.157679221055670116, 1485.519117650379940, 220.9368485806469948 ) ) ;
#22467 = CIRCLE ( 'NONE', #25833, 3.999999999999997335 ) ;
#22468 = CARTESIAN_POINT ( 'NONE',  ( 11.41568233489999962, 1500.982773024489916, 207.1620391477790122 ) ) ;
#22470 = CYLINDRICAL_SURFACE ( 'NONE', #59380, 1.436538049339995737 ) ;
#22469 = CARTESIAN_POINT ( 'NONE',  ( -20.59684415639999955, 1507.762623716630060, 190.3921826403979765 ) ) ;
#22471 = CARTESIAN_POINT ( 'NONE',  ( -6.938478822895000064, 1516.719999691880048, 209.8757167055200057 ) ) ;
#22472 = CARTESIAN_POINT ( 'NONE',  ( -24.96771051035950251, 1452.035975450660089, 135.7298172057880095 ) ) ;
#22473 = CARTESIAN_POINT ( 'NONE',  ( -11.43735029920000024, 1425.481221014229959, 144.1633320290980009 ) ) ;
#22474 = CARTESIAN_POINT ( 'NONE',  ( 2.234897854288949937, 1512.314859079350072, 217.7207912642259942 ) ) ;
#22475 = CARTESIAN_POINT ( 'NONE',  ( 20.41258333560000082, 1494.156730172889866, 204.1224707391089908 ) ) ;
#22476 = CARTESIAN_POINT ( 'NONE',  ( 0.000000000000000000, 0.000000000000000000, 0.000000000000000000 ) ) ;
#22477 = CARTESIAN_POINT ( 'NONE',  ( -40.06284621443700189, 1441.966320483619938, 136.9295851911570026 ) ) ;
#22478 = EDGE_LOOP ( 'NONE', ( #29320, #92473, #55179 ) ) ;
#22479 = CARTESIAN_POINT ( 'NONE',  ( 5.076283890730000081, 1469.790178736790040, 187.8425608535989966 ) ) ;
#22480 = CARTESIAN_POINT ( 'NONE',  ( -2.746886073237670089, 1430.908227116830176, 201.2170371325859719 ) ) ;
#22481 = EDGE_LOOP ( 'NONE', ( #17989, #2163, #91228, #53290, #85731, #22631, #22280, #89872, #87216, #77620, #52423, #34263 ) ) ;
#22482 = ORIENTED_EDGE ( 'NONE', *, *, #31051, .T. ) ;
#22483 = CARTESIAN_POINT ( 'NONE',  ( 14.13769145736555899, 1410.779407556687829, 227.9671458598623701 ) ) ;
#22484 = CARTESIAN_POINT ( 'NONE',  ( 31.55060375016905638, 1525.712835404586031, 217.0331836276179160 ) ) ;
#22485 = CARTESIAN_POINT ( 'NONE',  ( 0.3000392389890000344, 1450.902582786230141, 181.2594265962979705 ) ) ;
#22486 = CARTESIAN_POINT ( 'NONE',  ( -3.343564312049999820, 1485.815321652630018, 182.5922648735979692 ) ) ;
#22487 = CARTESIAN_POINT ( 'NONE',  ( -2.500000000000000000, 1439.361286679139994, 161.1256493471019837 ) ) ;
#22488 = CARTESIAN_POINT ( 'NONE',  ( -2.620401159549917480, 1523.382868172864164, 242.1631858340802239 ) ) ;
#22489 = CARTESIAN_POINT ( 'NONE',  ( -62.06363869513148046, 1379.731149298604578, 265.9958807297100520 ) ) ;
#22490 = CARTESIAN_POINT ( 'NONE',  ( -0.8071984717899990391, 1465.223756610790133, 198.1240437993990042 ) ) ;
#22491 = CARTESIAN_POINT ( 'NONE',  ( -0.9156123448460000702, 1507.627023022429967, 232.0153169555979957 ) ) ;
#22492 = CARTESIAN_POINT ( 'NONE',  ( -10.32735784461773498, 1519.913060387329779, 184.1749888460368538 ) ) ;
#22493 = CARTESIAN_POINT ( 'NONE',  ( -77.18480047366641372, 1384.779630308949891, 279.0553653738320463 ) ) ;
#22494 = EDGE_LOOP ( 'NONE', ( #86825, #24464 ) ) ;
#22495 = CARTESIAN_POINT ( 'NONE',  ( 7.717505752974999744, 1516.857914730730045, 201.4043401791270185 ) ) ;
#22496 = CARTESIAN_POINT ( 'NONE',  ( 2.284053471355000031, 1516.854133554269993, 207.9850318982369970 ) ) ;
#22497 = VERTEX_POINT ( 'NONE', #11489 ) ;
#22498 = CARTESIAN_POINT ( 'NONE',  ( 11.04992432786889900, 1414.913526854310021, 222.2523931539879811 ) ) ;
#22499 = CARTESIAN_POINT ( 'NONE',  ( -0.0002245325643044376212, 1452.164049364258972, 153.8748112245245636 ) ) ;
#22500 = ORIENTED_EDGE ( 'NONE', *, *, #65274, .F. ) ;
#22501 = CARTESIAN_POINT ( 'NONE',  ( -0.2499161997042609884, 1451.685132841090081, 183.0451107522330005 ) ) ;
#22502 = CARTESIAN_POINT ( 'NONE',  ( -16.48822391639999907, 1410.861292066530041, 191.6305835189980087 ) ) ;
#22503 = CARTESIAN_POINT ( 'NONE',  ( -109.0351219020656828, 1384.329096908686552, 311.2187149847616752 ) ) ;
#22504 = CARTESIAN_POINT ( 'NONE',  ( -9.585289191388769225, 1462.057342544479980, 206.7320176240860121 ) ) ;
#22505 = CARTESIAN_POINT ( 'NONE',  ( -12.71293088880000077, 1419.901838804629733, 222.1500227018980240 ) ) ;
#22506 = CARTESIAN_POINT ( 'NONE',  ( -13.74310390781900004, 1522.051704408389924, 201.1531303618569950 ) ) ;
#22507 = CARTESIAN_POINT ( 'NONE',  ( -1.429922479960000103, 1509.031031462129704, 179.3412831849980194 ) ) ;
#22508 = CARTESIAN_POINT ( 'NONE',  ( -6.343099832323124687, 1511.025938544041082, 201.7141561594071959 ) ) ;
#22509 = CARTESIAN_POINT ( 'NONE',  ( -21.71247731328945108, 1523.982201850120191, 183.5488543797130490 ) ) ;
#22511 = CARTESIAN_POINT ( 'NONE',  ( -11.60004869885203682, 1425.704216035731406, 137.2038747579310893 ) ) ;
#22510 = CARTESIAN_POINT ( 'NONE',  ( 17.66572951889999743, 1459.830952528330045, 228.2832691448980142 ) ) ;
#22512 = CARTESIAN_POINT ( 'NONE',  ( 6.705798878809999586, 1469.980848758390039, 210.5526231697390074 ) ) ;
#22513 = CARTESIAN_POINT ( 'NONE',  ( 6.554764161265000055, 1516.786099423779888, 216.8374711732070068 ) ) ;
#22514 = CARTESIAN_POINT ( 'NONE',  ( -22.71284877100005772, 1409.706192817229748, 209.1573958980538634 ) ) ;
#22515 = CARTESIAN_POINT ( 'NONE',  ( -0.09497152921324419905, 1508.365128300149991, 180.3902598306100060 ) ) ;
#22516 = TOROIDAL_SURFACE ( 'NONE', #56529, 10.10241613150000006, 2.000000000000000000 ) ;
#22517 = CARTESIAN_POINT ( 'NONE',  ( 2.155390440473662128, 1516.527465808152328, 216.8306986136358887 ) ) ;
#22518 = CARTESIAN_POINT ( 'NONE',  ( -3.448206916814999801, 1516.904492006980036, 213.1642637479369853 ) ) ;
#22519 = ADVANCED_FACE ( 'NONE', ( #26043 ), #2001, .T. ) ;
#22520 = CARTESIAN_POINT ( 'NONE',  ( 2.329898367294779504, 1515.064791340959800, 213.4512947642129745 ) ) ;
#22521 = DIRECTION ( 'NONE',  ( -1.836970198721029688E-16, -1.000000000000000000, -1.314768175368352060E-31 ) ) ;
#22523 = ORIENTED_EDGE ( 'NONE', *, *, #46707, .F. ) ;
#22522 = CARTESIAN_POINT ( 'NONE',  ( -11.62069923840673091, 1507.830660535743391, 207.5518435106793618 ) ) ;
#22524 = CARTESIAN_POINT ( 'NONE',  ( -1.961418762358051238, 1526.143142182166912, 177.8224660300539313 ) ) ;
#22525 = CARTESIAN_POINT ( 'NONE',  ( 1.901370350220000116, 1507.955859758289989, 220.6917275793990143 ) ) ;
#22526 = ADVANCED_FACE ( 'NONE', ( #104434 ), #64096, .T. ) ;
#22527 = CARTESIAN_POINT ( 'NONE',  ( -11.74544487829999895, 1430.504254567329781, 150.5476776824980334 ) ) ;
#22528 = LINE ( 'NONE', #91970, #77254 ) ;
#22529 = ADVANCED_FACE ( 'NONE', ( #45664 ), #17085, .T. ) ;
#22530 = CARTESIAN_POINT ( 'NONE',  ( -109.9268356472339860, 1384.151773320029861, 311.4065111799300212 ) ) ;
#22531 = CARTESIAN_POINT ( 'NONE',  ( -23.59335433665016524, 1517.051704408389924, 209.8811657366738928 ) ) ;
#22532 = CARTESIAN_POINT ( 'NONE',  ( 10.46140733719999893, 1420.326681975860083, 197.7779852210990157 ) ) ;
#22533 = CARTESIAN_POINT ( 'NONE',  ( 12.09505026880000145, 1446.483279760800087, 187.9542664695979681 ) ) ;
#22535 = CARTESIAN_POINT ( 'NONE',  ( -10.15848146045460076, 1480.881806938720047, 206.2592734015669862 ) ) ;
#22534 = CARTESIAN_POINT ( 'NONE',  ( -19.83923968069999688, 1457.446133080529989, 225.5370320128979813 ) ) ;
#22536 = CARTESIAN_POINT ( 'NONE',  ( -1.674135989289999848, 1484.258142909130129, 182.6938733975980256 ) ) ;
#22537 = ORIENTED_EDGE ( 'NONE', *, *, #32170, .F. ) ;
#22538 = CARTESIAN_POINT ( 'NONE',  ( 0.7365611785030020675, 1517.066898074209803, 204.4979538714769944 ) ) ;
#22539 = CARTESIAN_POINT ( 'NONE',  ( 3.414736771379999869, 1406.358550222729946, 269.2903006555980028 ) ) ;
#22540 = CARTESIAN_POINT ( 'NONE',  ( 0.000000000000000000, 1523.051704408389696, 209.1218459616979999 ) ) ;
#22541 = CARTESIAN_POINT ( 'NONE',  ( 10.84315941642620018, 1489.732817849439925, 207.6990053546570039 ) ) ;
#22542 = AXIS2_PLACEMENT_3D ( 'NONE', #56279, #88781, #46798 ) ;
#22543 = CARTESIAN_POINT ( 'NONE',  ( 24.15782421630898114, 1436.331097753197355, 213.4530830919744062 ) ) ;
#22544 = CARTESIAN_POINT ( 'NONE',  ( -1.354610398945402805, 1463.304784733452152, 199.4317993211560065 ) ) ;
#22545 =( BOUNDED_SURFACE ( )  B_SPLINE_SURFACE ( 1, 2, ( 
 ( #63970, #62899, #98085, #90787, #2968, #80198, #3516, #98634, #20820 ),
 ( #72366, #71846, #106497, #71289, #88611, #72903, #105402, #54474, #11893 ) ),
 .UNSPECIFIED., .F., .T., .F. ) 
 B_SPLINE_SURFACE_WITH_KNOTS ( ( 2, 2 ),
 ( 3, 2, 2, 2, 3 ),
 ( -10000.00000000000000, 10000.00000000000000 ),
 ( 0.000000000000000000, 1.570796326794899889, 3.141592653589790007, 4.712388980384689674, 6.283185307179590673 ),
 .UNSPECIFIED. ) 
 GEOMETRIC_REPRESENTATION_ITEM ( )  RATIONAL_B_SPLINE_SURFACE ( (
 ( 1.000000000000000000, 0.7071067811865480168, 1.000000000000000000, 0.7071067811865480168, 1.000000000000000000, 0.7071067811865480168, 1.000000000000000000, 0.7071067811865480168, 1.000000000000000000),
 ( 1.000000000000000000, 0.7071067811865480168, 1.000000000000000000, 0.7071067811865480168, 1.000000000000000000, 0.7071067811865480168, 1.000000000000000000, 0.7071067811865480168, 1.000000000000000000) ) ) 
 REPRESENTATION_ITEM ( '' )  SURFACE ( )  );
#22546 = CARTESIAN_POINT ( 'NONE',  ( 14.38014760757803145, 1517.051704408389924, 208.3596762285818045 ) ) ;
#22547 = CARTESIAN_POINT ( 'NONE',  ( -10.24550950064739929, 1447.425523760389979, 210.5433215532739837 ) ) ;
#22548 = CARTESIAN_POINT ( 'NONE',  ( -2.500000000000000000, 1448.894380904760055, 155.6080925163979884 ) ) ;
#22549 = CARTESIAN_POINT ( 'NONE',  ( -1.589333880778387442, 1451.431681818979996, 183.9171754951539981 ) ) ;
#22550 = CARTESIAN_POINT ( 'NONE',  ( 12.94448954231350868, 1511.163060387329779, 232.8165751327380519 ) ) ;
#22551 = CARTESIAN_POINT ( 'NONE',  ( -19.66678637224480397, 1519.551704408389924, 215.8936635741279986 ) ) ;
#22552 = CARTESIAN_POINT ( 'NONE',  ( -4.015743051850000356, 1515.588776726489868, 209.8750191343430060 ) ) ;
#22553 = CARTESIAN_POINT ( 'NONE',  ( -6.719124544191419801, 1517.051704408389924, 184.2328727701749926 ) ) ;
#22554 = CARTESIAN_POINT ( 'NONE',  ( 4.329790235878672178, 1515.051704408389924, 205.2060425482754056 ) ) ;
#22555 = CARTESIAN_POINT ( 'NONE',  ( -21.13431252044160047, 1409.651086843229905, 211.8287216663260040 ) ) ;
#22556 = CARTESIAN_POINT ( 'NONE',  ( -7.073260216319999572, 1475.574671051529776, 267.2142456188980191 ) ) ;
#22557 = CARTESIAN_POINT ( 'NONE',  ( -4.247024088876750092, 1446.448240483110112, 161.6103351768979906 ) ) ;
#22558 = CARTESIAN_POINT ( 'NONE',  ( -6.522631655713630572, 1422.592458550150013, 144.1528597353479881 ) ) ;
#22559 = CARTESIAN_POINT ( 'NONE',  ( 17.75177446265830028, 1414.289121907220078, 223.7769287431660246 ) ) ;
#22560 = CARTESIAN_POINT ( 'NONE',  ( -32.13574913744070471, 1384.820411185770126, 230.4565343730859865 ) ) ;
#22561 = CARTESIAN_POINT ( 'NONE',  ( -106.9331110549079966, 1391.913060387289988, 301.8577884849000270 ) ) ;
#22562 = CARTESIAN_POINT ( 'NONE',  ( -21.57330136150000044, 1507.349411603790031, 210.4857862235489847 ) ) ;
#22563 = CARTESIAN_POINT ( 'NONE',  ( -18.28985832939523348, 1519.551704408389924, 198.5293912879491529 ) ) ;
#22564 = CARTESIAN_POINT ( 'NONE',  ( 32.09351624765461253, 1524.374142163904480, 216.7021085575802317 ) ) ;
#22565 = CARTESIAN_POINT ( 'NONE',  ( 8.280658185778859703, 1511.427938672825576, 204.8576795970872695 ) ) ;
#22566 = CARTESIAN_POINT ( 'NONE',  ( -22.69629448799999949, 1411.065802167830043, 203.8940129321279926 ) ) ;
#22567 = CARTESIAN_POINT ( 'NONE',  ( -15.65146756583599874, 1421.348246145913890, 227.1285423004100039 ) ) ;
#22568 = CARTESIAN_POINT ( 'NONE',  ( 19.46330959930472204, 1455.604926216044305, 225.6731016573391457 ) ) ;
#22569 = ORIENTED_EDGE ( 'NONE', *, *, #27503, .F. ) ;
#22570 = EDGE_CURVE ( 'NONE', #43475, #18765, #9275, .T. ) ;
#22571 = CARTESIAN_POINT ( 'NONE',  ( -19.77045317620000020, 1466.948919781690165, 211.0321804172989744 ) ) ;
#22572 = CARTESIAN_POINT ( 'NONE',  ( -7.501250516761643894, 1510.704533478968187, 215.1450708915986070 ) ) ;
#22573 = CARTESIAN_POINT ( 'NONE',  ( -9.838224505892318561, 1462.268909613540245, 227.9668215274659815 ) ) ;
#22575 = CARTESIAN_POINT ( 'NONE',  ( -13.46738151552789908, 1379.591386266799873, 211.6550698743690191 ) ) ;
#22574 = CARTESIAN_POINT ( 'NONE',  ( 3.448830483803564828, 1518.913060387330006, 175.1594891075192209 ) ) ;
#22576 = CARTESIAN_POINT ( 'NONE',  ( 17.78112617924024264, 1523.954924407802764, 237.8273222678101035 ) ) ;
#22577 = DIRECTION ( 'NONE',  ( 0.9455185755993178454, 0.000000000000000000, -0.3255681544571539243 ) ) ;
#22578 = CARTESIAN_POINT ( 'NONE',  ( -4.784282693639999806, 1454.717937669690173, 201.0055521229189992 ) ) ;
#22579 = CARTESIAN_POINT ( 'NONE',  ( -1.129386240404999908, 1516.613712827999962, 201.7984555248870038 ) ) ;
#22580 = CARTESIAN_POINT ( 'NONE',  ( 7.363738131959999933, 1426.807041349819883, 212.7119719394189872 ) ) ;
#22581 = CARTESIAN_POINT ( 'NONE',  ( -6.232532191338900240, 1398.098440470949981, 197.7132727547819968 ) ) ;
#22582 = CARTESIAN_POINT ( 'NONE',  ( 16.42424928753500168, 1513.961173499609913, 194.5327833756670088 ) ) ;
#22583 = CARTESIAN_POINT ( 'NONE',  ( -22.55307526729999879, 1417.538526918689968, 209.9295645762900051 ) ) ;
#22584 = CARTESIAN_POINT ( 'NONE',  ( -7.483730530865719821, 1379.920825505379980, 211.0169310811999708 ) ) ;
#22585 = CARTESIAN_POINT ( 'NONE',  ( 7.917631394359482044, 1366.221626954849626, 210.6218459617142003 ) ) ;
#22586 = CARTESIAN_POINT ( 'NONE',  ( 21.37693747720000204, 1440.913060387330006, 224.8635562088979896 ) ) ;
#22588 = ORIENTED_EDGE ( 'NONE', *, *, #61063, .T. ) ;
#22587 = CARTESIAN_POINT ( 'NONE',  ( 4.802241234501059886, 1508.551704408389924, 204.6921032804660001 ) ) ;
#22589 = B_SPLINE_CURVE_WITH_KNOTS ( 'NONE', 3,
 ( #53875, #10174, #1240, #77933, #18553, #79606, #53305, #78491 ),
 .UNSPECIFIED., .F., .F.,
 ( 4, 2, 2, 4 ),
 ( -0.07674005832873599664, -0.05880084693797370254, -0.03415900950112209927, -1.075081518253639956E-08 ),
 .UNSPECIFIED. ) ;
#22590 = EDGE_LOOP ( 'NONE', ( #79011, #93267, #66650 ) ) ;
#22591 = CARTESIAN_POINT ( 'NONE',  ( -8.482826003179999574, 1397.255022998529967, 199.1539838373379894 ) ) ;
#22592 = CARTESIAN_POINT ( 'NONE',  ( -22.53878036859999767, 1411.058442714630019, 212.0450777197879972 ) ) ;
#22593 = CARTESIAN_POINT ( 'NONE',  ( -2.827546459321990557, 1516.555886569700306, 201.4122491134000086 ) ) ;
#22594 = CARTESIAN_POINT ( 'NONE',  ( -12.89659922727121177, 1444.936763667012883, 169.4369277064754726 ) ) ;
#22595 = CARTESIAN_POINT ( 'NONE',  ( -24.68679851519999957, 1508.521770562530037, 197.5360056163980005 ) ) ;
#22596 = CARTESIAN_POINT ( 'NONE',  ( -7.686100042665000132, 1512.192993275409890, 211.8118285282569957 ) ) ;
#22598 = CARTESIAN_POINT ( 'NONE',  ( -1.356522590142140050, 1410.335674017130032, 185.6037846924129724 ) ) ;
#22597 = CARTESIAN_POINT ( 'NONE',  ( 3.442291544270000170, 1445.232941167789932, 200.8115262291190106 ) ) ;
#22599 = CARTESIAN_POINT ( 'NONE',  ( 5.358763871729999906, 1429.765654666730143, 185.6049313592980070 ) ) ;
#22600 = CARTESIAN_POINT ( 'NONE',  ( -12.26986021650000147, 1416.828040557830036, 194.6643751810979950 ) ) ;
#22601 = DIRECTION ( 'NONE',  ( 0.1402804634180424004, 0.9901118076173111016, 0.000000000000000000 ) ) ;
#22602 = CARTESIAN_POINT ( 'NONE',  ( 10.61042346008030179, 1396.283584539540016, 212.2790510548149996 ) ) ;
#22603 = CARTESIAN_POINT ( 'NONE',  ( 14.37881581500380079, 1416.259629948840029, 196.9329869028040036 ) ) ;
#22604 = CARTESIAN_POINT ( 'NONE',  ( 11.73075292130000058, 1429.442647445629973, 150.1417213462979987 ) ) ;
#22605 = CARTESIAN_POINT ( 'NONE',  ( 8.127041000494140022, 1509.197164375159218, 180.9360732693761804 ) ) ;
#22606 = ORIENTED_EDGE ( 'NONE', *, *, #15619, .F. ) ;
#22607 = CARTESIAN_POINT ( 'NONE',  ( -16.75454338844485846, 1526.382868172571079, 183.6974516591949396 ) ) ;
#22608 = CARTESIAN_POINT ( 'NONE',  ( 2.151265163027241911, 1450.023995276909773, 182.0536789941844802 ) ) ;
#22609 = ORIENTED_EDGE ( 'NONE', *, *, #93180, .T. ) ;
#22610 = ORIENTED_EDGE ( 'NONE', *, *, #63149, .F. ) ;
#22611 = EDGE_CURVE ( 'NONE', #9033, #14535, #9309, .T. ) ;
#22612 = CARTESIAN_POINT ( 'NONE',  ( 0.000000000000000000, 1523.382868172864164, 209.1218459616979999 ) ) ;
#22613 = CARTESIAN_POINT ( 'NONE',  ( -34.18677586421195258, 1512.187213306747481, 198.4504086008750505 ) ) ;
#22614 = CARTESIAN_POINT ( 'NONE',  ( -109.8119358823353338, 1386.120803211467546, 311.3368505780957207 ) ) ;
#22615 = CARTESIAN_POINT ( 'NONE',  ( -29.16136750932367150, 1526.143142182265592, 197.5843855542967731 ) ) ;
#22616 = CARTESIAN_POINT ( 'NONE',  ( -0.7386049428049979992, 1517.122674412569950, 215.6839400395269877 ) ) ;
#22617 = CARTESIAN_POINT ( 'NONE',  ( -12.62128053491670165, 1379.543530202440252, 209.2104001695750242 ) ) ;
#22618 = AXIS2_PLACEMENT_3D ( 'NONE', #75875, #2373, #36489 ) ;
#22619 = VERTEX_POINT ( 'NONE', #26610 ) ;
#22620 = CARTESIAN_POINT ( 'NONE',  ( -11.32684497959999881, 1503.073821494790081, 207.0295587123389964 ) ) ;
#22621 = CARTESIAN_POINT ( 'NONE',  ( -2.966095081577469816, 1509.131301283620132, 179.1608205533310070 ) ) ;
#22622 = CARTESIAN_POINT ( 'NONE',  ( -45.66666430340000460, 1375.391324216819839, 231.3493056147590039 ) ) ;
#22623 = B_SPLINE_CURVE_WITH_KNOTS ( 'NONE', 5,
 ( #71597, #104597, #97834, #106251, #21112, #20565 ),
 .UNSPECIFIED., .F., .F.,
 ( 6, 6 ),
 ( 0.000000000000000000, 1.000000000000000000 ),
 .UNSPECIFIED. ) ;
#22624 = CARTESIAN_POINT ( 'NONE',  ( -1.135460355084999762, 1516.790374942449944, 205.8685445508469911 ) ) ;
#22625 = VERTEX_POINT ( 'NONE', #88195 ) ;
#22626 = CARTESIAN_POINT ( 'NONE',  ( -7.332063977575000280, 1516.939491476980038, 209.1325772641960157 ) ) ;
#22627 = CARTESIAN_POINT ( 'NONE',  ( -19.86733818529999951, 1508.094164518030084, 229.2433209336980156 ) ) ;
#22628 = CARTESIAN_POINT ( 'NONE',  ( -17.58753714432851822, 1413.209790116180329, 269.3766082286189203 ) ) ;
#22629 = CARTESIAN_POINT ( 'NONE',  ( -2.179564447600000232, 1409.156885224530015, 232.1843940729979749 ) ) ;
#22631 = ORIENTED_EDGE ( 'NONE', *, *, #28676, .T. ) ;
#22630 = CARTESIAN_POINT ( 'NONE',  ( -3.820317395759999561E-10, 1453.313060387329870, 189.4452657542980205 ) ) ;
#22632 = CARTESIAN_POINT ( 'NONE',  ( 2.500000000000000000, 1427.007219668030075, 156.3926178584979994 ) ) ;
#22634 = B_SPLINE_CURVE_WITH_KNOTS ( 'NONE', 5,
 ( #58203, #76102, #26230, #60420, #59865, #25672, #42490, #15603, #110797, #49807, #100725, #58748, #7240, #34089, #41400, #68282, #8876, #102390, #109700, #50367, #93990, #3282, #63201, #104053, #97308, #88365, #44727, #77759, #71045, #35196, #1068, #69382, #78878, #103490, #2183, #37411, #29016, #2731, #60983 ),
 .UNSPECIFIED., .F., .F.,
 ( 6, 3, 3, 3, 3, 3, 3, 3, 3, 3, 3, 3, 6 ),
 ( 0.000000000000000000, 0.01986406830872220960, 0.03714071196419825582, 0.05441735561967429857, 0.08897064292978833222, 0.1583566291595912279, 0.2277426153893942207, 0.5076826711937041381, 0.6470691381323538938, 0.7864556050751944083, 0.8932279473768452993, 0.9466141185318610596, 1.000000000000000000 ),
 .UNSPECIFIED. ) ;
#22633 = CARTESIAN_POINT ( 'NONE',  ( -29.42918164984530094, 1440.913060386839788, 236.4667028220079885 ) ) ;
#22635 = B_SPLINE_CURVE_WITH_KNOTS ( 'NONE', 3,
 ( #29480, #89940, #47405, #64779, #99429, #80456 ),
 .UNSPECIFIED., .F., .F.,
 ( 4, 2, 4 ),
 ( -1.131363979617846934E-05, 0.001067788114095997044, 0.002146889867988172572 ),
 .UNSPECIFIED. ) ;
#22636 = CARTESIAN_POINT ( 'NONE',  ( -36.25797752260000095, 1383.833857111379984, 235.3800711337590030 ) ) ;
#22637 = DIRECTION ( 'NONE',  ( 0.000000000000000000, 0.000000000000000000, -1.000000000000000000 ) ) ;
#22638 = CARTESIAN_POINT ( 'NONE',  ( 6.215215835796609412, 1410.569368109790048, 269.6190100981399951 ) ) ;
#22639 = CARTESIAN_POINT ( 'NONE',  ( -4.029572678834999699, 1516.858649670339901, 213.1633184439769764 ) ) ;
#22640 = CARTESIAN_POINT ( 'NONE',  ( 24.11333318339999821, 1410.980709295929955, 209.4832115230679790 ) ) ;
#22641 = CARTESIAN_POINT ( 'NONE',  ( -20.70700216050000009, 1509.300535355729835, 188.9489426423980092 ) ) ;
#22642 = CARTESIAN_POINT ( 'NONE',  ( 17.37368555716430052, 1428.575912512719924, 203.8623300055620007 ) ) ;
#22644 = EDGE_CURVE ( 'NONE', #61380, #110254, #37153, .T. ) ;
#22643 = CARTESIAN_POINT ( 'NONE',  ( -7.711857127811300394, 1516.642200982649911, 210.2014009544199951 ) ) ;
#22645 = CARTESIAN_POINT ( 'NONE',  ( -3.445201526505000000, 1516.743010792419909, 210.8372070624770060 ) ) ;
#22646 = ADVANCED_FACE ( 'NONE', ( #13647 ), #38320, .T. ) ;
#22647 = DIRECTION ( 'NONE',  ( -0.1151936120068250274, -0.4472295632498141660, -0.8869702077906571613 ) ) ;
#22648 = CARTESIAN_POINT ( 'NONE',  ( 0.1896301300600000128, 1420.480785433730034, 182.7505287346979799 ) ) ;
#22649 = CARTESIAN_POINT ( 'NONE',  ( 9.459682105082901415, 1424.144415159054688, 137.0999999983294231 ) ) ;
#22650 = EDGE_CURVE ( 'NONE', #36071, #66446, #99212, .T. ) ;
#22652 = ORIENTED_EDGE ( 'NONE', *, *, #104492, .F. ) ;
#22651 = CARTESIAN_POINT ( 'NONE',  ( -36.12389091449999512, 1385.203813137380166, 235.4649545851590062 ) ) ;
#22653 = CARTESIAN_POINT ( 'NONE',  ( -42.09313388289950097, 1385.169883172800155, 245.8983665241910046 ) ) ;
#22654 = CARTESIAN_POINT ( 'NONE',  ( -7.891777529692960869, 1512.314860027450095, 212.0638759934929851 ) ) ;
#22655 = EDGE_CURVE ( 'NONE', #107049, #22497, #37237, .T. ) ;
#22656 = CARTESIAN_POINT ( 'NONE',  ( -3.464457313471830169, 1370.273648968840689, 210.1175475933252130 ) ) ;
#22657 = VECTOR ( 'NONE', #3306, 1000.000000000000000 ) ;
#22658 = ADVANCED_FACE ( 'NONE', ( #72499 ), #101110, .T. ) ;
#22659 = CARTESIAN_POINT ( 'NONE',  ( -8.373664085718591110, 1414.913060387329779, 223.0268086914393848 ) ) ;
#22660 = CARTESIAN_POINT ( 'NONE',  ( -5.392699262009999828, 1433.241572010809932, 154.6274253439979987 ) ) ;
#22661 = CARTESIAN_POINT ( 'NONE',  ( 10.61261630010000090, 1424.158067204230065, 205.9607122707290046 ) ) ;
#22662 = CARTESIAN_POINT ( 'NONE',  ( -115.7111929266684882, 1304.231242809270043, 308.4524562320341943 ) ) ;
#22663 = ADVANCED_FACE ( 'NONE', ( #27598 ), #17315, .F. ) ;
#22664 = APPLICATION_CONTEXT ( 'automotive_design' ) ;
#22666 = CARTESIAN_POINT ( 'NONE',  ( -8.862056540259999338, 1384.892951007150259, 218.6851137892589918 ) ) ;
#22665 = CARTESIAN_POINT ( 'NONE',  ( -6.941727290454999810, 1516.882217593000178, 216.4530290611770056 ) ) ;
#22667 = DIRECTION ( 'NONE',  ( 0.000000000000000000, 0.000000000000000000, 1.000000000000000000 ) ) ;
#22668 = CARTESIAN_POINT ( 'NONE',  ( 33.14208818188833305, 1524.841055067849538, 220.4153344904927678 ) ) ;
#22669 = VERTEX_POINT ( 'NONE', #104307 ) ;
#22670 = CARTESIAN_POINT ( 'NONE',  ( 1.125509850285000280, 1517.203017563489766, 201.7827387294869936 ) ) ;
#22671 = CARTESIAN_POINT ( 'NONE',  ( 10.43886700434340042, 1480.990255025190208, 207.5644369805290239 ) ) ;
#22672 = ORIENTED_EDGE ( 'NONE', *, *, #74187, .F. ) ;
#22673 = CARTESIAN_POINT ( 'NONE',  ( 27.96976553579999702, 1509.201555290030001, 207.5796322327380210 ) ) ;
#22674 = CONICAL_SURFACE ( 'NONE', #103099, 18.60900368820000850, 0.6981317007980000211 ) ;
#22675 = CARTESIAN_POINT ( 'NONE',  ( 19.44122429240000116, 1456.941909337529978, 224.4539435408979955 ) ) ;
#22676 = CARTESIAN_POINT ( 'NONE',  ( 7.872090775853918920, 1438.237761097329212, 153.7477460425555478 ) ) ;
#22677 = CARTESIAN_POINT ( 'NONE',  ( 9.521227846441806975, 1425.375466301815777, 195.5306922762230215 ) ) ;
#22678 = ADVANCED_FACE ( 'NONE', ( #79127 ), #91257, .F. ) ;
#22679 = CARTESIAN_POINT ( 'NONE',  ( 0.7868378234909989555, 1442.894628652889878, 218.3517676095690092 ) ) ;
#22680 = FACE_OUTER_BOUND ( 'NONE', #97043, .T. ) ;
#22681 = CARTESIAN_POINT ( 'NONE',  ( -3.684086113900000292, 1446.644897779309986, 159.4624714679980002 ) ) ;
#22682 = CARTESIAN_POINT ( 'NONE',  ( -19.12894962059999671, 1426.100227420630063, 225.4496986463979908 ) ) ;
#22683 = CARTESIAN_POINT ( 'NONE',  ( 10.52956383476244007, 1489.196172734509446, 206.2018118126233333 ) ) ;
#22684 = CARTESIAN_POINT ( 'NONE',  ( -105.5763038039999913, 1391.607272681279710, 303.0949483744590225 ) ) ;
#22685 = CARTESIAN_POINT ( 'NONE',  ( 18.82869366990000159, 1461.938562382830014, 190.8087292768979921 ) ) ;
#22686 = CARTESIAN_POINT ( 'NONE',  ( 18.20258715539999983, 1429.723789929190161, 209.1218459616989946 ) ) ;
#22687 = EDGE_CURVE ( 'NONE', #19377, #47729, #105163, .T. ) ;
#22688 = CARTESIAN_POINT ( 'NONE',  ( -38.35150357969526169, 1453.387763860978112, 269.5822590821125573 ) ) ;
#22689 = VERTEX_POINT ( 'NONE', #53942 ) ;
#22690 = CARTESIAN_POINT ( 'NONE',  ( -10.81507089441019964, 1424.921187596680056, 144.1620444830689962 ) ) ;
#22691 = EDGE_CURVE ( 'NONE', #49944, #81708, #70488, .T. ) ;
#22692 = CARTESIAN_POINT ( 'NONE',  ( 11.14479613505110045, 1470.280215154140024, 206.9369914153219838 ) ) ;
#22693 = FACE_OUTER_BOUND ( 'NONE', #47817, .T. ) ;
#22694 = CARTESIAN_POINT ( 'NONE',  ( -0.1431367926419999936, 1417.281368496930099, 234.8519457758980309 ) ) ;
#22695 = AXIS2_PLACEMENT_3D ( 'NONE', #1920, #88670, #36057 ) ;
#22696 = CARTESIAN_POINT ( 'NONE',  ( -13.29029361451234159, 1444.600243103134289, 186.7172809443856920 ) ) ;
#22697 = CARTESIAN_POINT ( 'NONE',  ( -8.611480341139710504, 1436.906018617760083, 209.7133912976819943 ) ) ;
#22698 = PLANE ( 'NONE',  #63357 ) ;
#22699 = EDGE_CURVE ( 'NONE', #103179, #45409, #67902, .T. ) ;
#22700 = CARTESIAN_POINT ( 'NONE',  ( -21.59687142900000012, 1507.523380033690046, 209.4572543540780032 ) ) ;
#22701 = CARTESIAN_POINT ( 'NONE',  ( -18.19590854888185305, 1501.977400791986611, 180.0410247165186490 ) ) ;
#22702 = CARTESIAN_POINT ( 'NONE',  ( 24.76239166610000098, 1435.860790453759819, 137.6237234474980085 ) ) ;
#22703 = CARTESIAN_POINT ( 'NONE',  ( 5.181410150655000990, 1510.418062979269962, 216.6707182703270291 ) ) ;
#22705 = ORIENTED_EDGE ( 'NONE', *, *, #75722, .T. ) ;
#22704 = CARTESIAN_POINT ( 'NONE',  ( -13.39865269429999906, 1409.380951649529834, 225.6837777353979959 ) ) ;
#22706 = CARTESIAN_POINT ( 'NONE',  ( -106.7568774629999950, 1381.977856463960052, 297.8845616112589596 ) ) ;
#22707 = CARTESIAN_POINT ( 'NONE',  ( 12.53206804002270047, 1512.191474810040063, 224.1219235409020030 ) ) ;
#22708 = ORIENTED_EDGE ( 'NONE', *, *, #27359, .T. ) ;
#22709 = ORIENTED_EDGE ( 'NONE', *, *, #61644, .F. ) ;
#22710 = CARTESIAN_POINT ( 'NONE',  ( -11.45038415740000026, 1501.280273630989996, 209.1761187364329828 ) ) ;
#22711 = CARTESIAN_POINT ( 'NONE',  ( 6.298908594212630163, 1516.706529261382684, 205.0487668162192563 ) ) ;
#22713 = CARTESIAN_POINT ( 'NONE',  ( -20.03573726089999596, 1460.150672173630028, 240.3194873113979781 ) ) ;
#22712 = CARTESIAN_POINT ( 'NONE',  ( 41.25049345058425132, 1434.982249775052424, 269.6332951576844152 ) ) ;
#22714 = CARTESIAN_POINT ( 'NONE',  ( -19.69775028829999997, 1484.707692800029918, 190.1282803529979901 ) ) ;
#22715 = CARTESIAN_POINT ( 'NONE',  ( -11.14272688560000013, 1433.633229230830011, 151.6530944731979957 ) ) ;
#22716 = DIRECTION ( 'NONE',  ( 1.755985294532464991E-16, -1.000000000000000000, 1.338183447452830017E-16 ) ) ;
#22717 = CARTESIAN_POINT ( 'NONE',  ( -5.032977198260000229, 1391.805267112089950, 203.8075142969990168 ) ) ;
#22718 = CARTESIAN_POINT ( 'NONE',  ( 9.457965440796609613, 1464.320992644629996, 211.7920758070480076 ) ) ;
#22719 = CARTESIAN_POINT ( 'NONE',  ( 2.500000000000000000, 1448.210448412289907, 170.6974824052979898 ) ) ;
#22720 = CARTESIAN_POINT ( 'NONE',  ( 1.629715277548020147, 1515.068677689339893, 213.4511930101580219 ) ) ;
#22721 = FACE_BOUND ( 'NONE', #13666, .T. ) ;
#22722 = CARTESIAN_POINT ( 'NONE',  ( -2.760778634279479782, 1409.009468901610035, 188.0459411385839985 ) ) ;
#22723 = B_SPLINE_CURVE_WITH_KNOTS ( 'NONE', 3,
 ( #66506, #14944, #68159, #91670, #100610, #67046, #76521, #102266, #41274, #58635, #23894, #49690, #83819, #75447, #25546, #16044, #50245, #51317, #84374, #102803, #68698, #44037, #35070, #2609, #87704, #87134, #51889, #105045 ),
 .UNSPECIFIED., .F., .F.,
 ( 4, 3, 3, 3, 3, 3, 3, 3, 3, 4 ),
 ( 11.45157243117470003, 11.57484800204929876, 11.69873572308700105, 11.82299213567229934, 11.94767712729789899, 12.07285275658629864, 12.19896151394710060, 12.32556630458410041, 12.45304517163829949, 12.51194700650879987 ),
 .UNSPECIFIED. ) ;
#22724 = CARTESIAN_POINT ( 'NONE',  ( 0.05351389538980268201, 1362.267411265992223, 208.3718459617061285 ) ) ;
#22725 = CARTESIAN_POINT ( 'NONE',  ( -19.52630014007766945, 1509.713547991464338, 231.9178196453461283 ) ) ;
#22726 = EDGE_CURVE ( 'NONE', #21322, #84181, #49050, .T. ) ;
#22728 = ORIENTED_EDGE ( 'NONE', *, *, #19031, .T. ) ;
#22727 = CARTESIAN_POINT ( 'NONE',  ( 1.447894037093860002E-08, 1408.513036702840054, 261.9187567895989446 ) ) ;
#22729 = ORIENTED_EDGE ( 'NONE', *, *, #56184, .T. ) ;
#22730 = CARTESIAN_POINT ( 'NONE',  ( -11.86282332673470030, 1432.107038623590142, 149.9775339942419805 ) ) ;
#22731 = EDGE_CURVE ( 'NONE', #6988, #98270, #33034, .T. ) ;
#22732 = CARTESIAN_POINT ( 'NONE',  ( 24.12566577620000174, 1497.029149703290159, 206.7581795058389957 ) ) ;
#22733 = CARTESIAN_POINT ( 'NONE',  ( -7.478702111819999665, 1472.804222987030016, 270.4228357808979695 ) ) ;
#22734 = CARTESIAN_POINT ( 'NONE',  ( 1.396945595908719806, 1473.097535771269804, 219.2356281669150064 ) ) ;
#22735 = CARTESIAN_POINT ( 'NONE',  ( -103.0210057964301740, 1376.302340817391269, 309.8919163327337856 ) ) ;
#22736 = CARTESIAN_POINT ( 'NONE',  ( 35.10549739602630126, 1450.762126806190054, 136.1476404445799915 ) ) ;
#22737 = CARTESIAN_POINT ( 'NONE',  ( 0.2070356852857530017, 1452.599831121419811, 183.2333262594050041 ) ) ;
#22738 = CARTESIAN_POINT ( 'NONE',  ( -7.964207469239999782, 1384.720725717920004, 199.4939945441389852 ) ) ;
#22739 = CARTESIAN_POINT ( 'NONE',  ( 10.02252456385629920, 1469.313878311580083, 209.8095366709860059 ) ) ;
#22740 = CARTESIAN_POINT ( 'NONE',  ( -2.958239116441676586, 1515.068899845848136, 204.7925047304020723 ) ) ;
#22741 = CARTESIAN_POINT ( 'NONE',  ( 9.532517564019499900, 1366.286862064863953, 210.6218459616991936 ) ) ;
#22742 = CARTESIAN_POINT ( 'NONE',  ( -39.86365974965330139, 1422.738695774160078, 267.1848028950000185 ) ) ;
#22743 = VERTEX_POINT ( 'NONE', #51564 ) ;
#22744 = CARTESIAN_POINT ( 'NONE',  ( -3.541941751390889959, 1499.841325333280110, 181.2873610080370099 ) ) ;
#22745 = ORIENTED_EDGE ( 'NONE', *, *, #74314, .F. ) ;
#22746 = AXIS2_PLACEMENT_3D ( 'NONE', #64737, #89899, #38933 ) ;
#22747 = VERTEX_POINT ( 'NONE', #76759 ) ;
#22748 = CARTESIAN_POINT ( 'NONE',  ( 0.01265818781360149997, 1516.959716008189844, 210.8316124642570060 ) ) ;
#22749 = EDGE_CURVE ( 'NONE', #65751, #103878, #4452, .T. ) ;
#22750 = CARTESIAN_POINT ( 'NONE',  ( 37.73087422431532190, 1445.052233488290312, 136.8113442565054925 ) ) ;
#22751 = DIRECTION ( 'NONE',  ( 0.000000000000000000, 1.000000000000000000, 0.000000000000000000 ) ) ;
#22753 = CARTESIAN_POINT ( 'NONE',  ( -14.39948585115419988, 1509.538292535830124, 182.8035031149169924 ) ) ;
#22752 = CARTESIAN_POINT ( 'NONE',  ( -4.609673279564999504, 1516.754149861460064, 212.3872530880769887 ) ) ;
#22754 = CARTESIAN_POINT ( 'NONE',  ( -16.26535344460000232, 1425.423310974930018, 190.7822913542979961 ) ) ;
#22755 = DIRECTION ( 'NONE',  ( 0.000000000000000000, -1.000000000000000000, 0.000000000000000000 ) ) ;
#22756 = VERTEX_POINT ( 'NONE', #59427 ) ;
#22757 = CARTESIAN_POINT ( 'NONE',  ( -26.49906707450000098, 1436.567897694819976, 136.7771845898980132 ) ) ;
#22758 = CARTESIAN_POINT ( 'NONE',  ( 3.452289182574999948, 1517.069378699710114, 202.5601595088670024 ) ) ;
#22759 = EDGE_CURVE ( 'NONE', #106841, #21883, #69489, .T. ) ;
#22760 = DIRECTION ( 'NONE',  ( -1.000000000000000000, 0.000000000000000000, 0.000000000000000000 ) ) ;
#22761 = CARTESIAN_POINT ( 'NONE',  ( -19.67891453321817963, 1505.885360177188886, 218.9962822164112310 ) ) ;
#22762 = CARTESIAN_POINT ( 'NONE',  ( -40.78591513166909976, 1431.459864284900050, 269.6245610256719942 ) ) ;
#22763 = CARTESIAN_POINT ( 'NONE',  ( -17.30126322281408235, 1523.382868172864164, 180.8506073313487548 ) ) ;
#22764 = CARTESIAN_POINT ( 'NONE',  ( -6.220302149359999255, 1397.477102017430070, 197.7753768589980155 ) ) ;
#22765 = EDGE_CURVE ( 'NONE', #22209, #66863, #31772, .T. ) ;
#22767 = ORIENTED_EDGE ( 'NONE', *, *, #25752, .T. ) ;
#22766 = CARTESIAN_POINT ( 'NONE',  ( -8.059092760027739999, 1365.100440301198660, 208.3718459617061285 ) ) ;
#22768 = VERTEX_POINT ( 'NONE', #87372 ) ;
#22769 = CARTESIAN_POINT ( 'NONE',  ( 0.2381205061309999982, 1451.685209519130240, 183.0508848106979940 ) ) ;
#22770 = CARTESIAN_POINT ( 'NONE',  ( -28.54794148642016793, 1526.382868172864164, 219.8054320333061185 ) ) ;
#22771 = CARTESIAN_POINT ( 'NONE',  ( 3.753290028884420426, 1426.393640232169901, 191.4546578126879979 ) ) ;
#22772 = CARTESIAN_POINT ( 'NONE',  ( 19.02974267272306719, 1517.051704408389924, 211.0809136819971741 ) ) ;
#22773 = CARTESIAN_POINT ( 'NONE',  ( -2.632747685671116500, 1379.913060387289988, 207.6835693458863830 ) ) ;
#22774 = CIRCLE ( 'NONE', #51425, 1.999999999999999556 ) ;
#22775 = CARTESIAN_POINT ( 'NONE',  ( 2.300729626665000360, 1516.923170579120097, 210.8225527465970117 ) ) ;
#22776 = CARTESIAN_POINT ( 'NONE',  ( 6.721016565425069089, 1460.347746334779004, 202.1888905636935192 ) ) ;
#22777 = CARTESIAN_POINT ( 'NONE',  ( 5.510117011110000185, 1440.199971711730086, 154.7606381671979818 ) ) ;
#22778 = CARTESIAN_POINT ( 'NONE',  ( 6.590784414382070189, 1439.968245627540000, 215.2411843296279983 ) ) ;
#22779 = CARTESIAN_POINT ( 'NONE',  ( 18.80464302510000252, 1425.801049065629968, 225.6039134470979945 ) ) ;
#22780 = EDGE_CURVE ( 'NONE', #60349, #9033, #59927, .T. ) ;
#22781 = CARTESIAN_POINT ( 'NONE',  ( 7.557029907284999126, 1510.729589429620091, 203.9615281313170101 ) ) ;
#22782 = CARTESIAN_POINT ( 'NONE',  ( 7.710966977635000497, 1516.608208975040043, 207.9930883710269711 ) ) ;
#22783 = ORIENTED_EDGE ( 'NONE', *, *, #21447, .F. ) ;
#22784 = CARTESIAN_POINT ( 'NONE',  ( -40.71747595839300260, 1448.637563203250011, 135.3761645363250068 ) ) ;
#22785 = CARTESIAN_POINT ( 'NONE',  ( -11.16222505900650042, 1428.970455565040083, 101.8803122854220078 ) ) ;
#22786 = CARTESIAN_POINT ( 'NONE',  ( -12.78776258889159934, 1416.851343895820037, 195.9645815067300134 ) ) ;
#22787 = ORIENTED_EDGE ( 'NONE', *, *, #4553, .F. ) ;
#22788 = CARTESIAN_POINT ( 'NONE',  ( -28.27139721233055170, 1526.382868172863937, 198.6830693683576214 ) ) ;
#22789 = EDGE_CURVE ( 'NONE', #28487, #25667, #104163, .T. ) ;
#22790 = CARTESIAN_POINT ( 'NONE',  ( 12.57551620087889788, 1435.697644940459895, 150.8998391666309828 ) ) ;
#22791 = CARTESIAN_POINT ( 'NONE',  ( 14.04614445250000188, 1415.579607678529783, 197.0459619348980027 ) ) ;
#22792 = DIRECTION ( 'NONE',  ( -1.755985294532469921E-16, 1.000000000000000000, -1.338183447452831989E-16 ) ) ;
#22793 = CARTESIAN_POINT ( 'NONE',  ( -11.43993018048137245, 1425.780984131823061, 139.0081881035810341 ) ) ;
#22794 = CARTESIAN_POINT ( 'NONE',  ( 11.36216713388179933, 1503.110266152410077, 211.0233809544849919 ) ) ;
#22795 = CYLINDRICAL_SURFACE ( 'NONE', #40408, 2.000000000000011102 ) ;
#22796 = CARTESIAN_POINT ( 'NONE',  ( -18.31482527320000031, 1445.278739201789904, 204.5307550449689984 ) ) ;
#22797 = CARTESIAN_POINT ( 'NONE',  ( 23.15864443164504394, 1450.075779451102335, 217.7010643741785145 ) ) ;
#22798 = ADVANCED_FACE ( 'NONE', ( #8994 ), #22307, .T. ) ;
#22799 = AXIS2_PLACEMENT_3D ( 'NONE', #54704, #65301, #88281 ) ;
#22800 = CARTESIAN_POINT ( 'NONE',  ( 2.500000000000000000, 1439.588444383649858, 166.1975927366900123 ) ) ;
#22801 = DIRECTION ( 'NONE',  ( -1.000000000000000000, 0.000000000000000000, 0.000000000000000000 ) ) ;
#22802 = CARTESIAN_POINT ( 'NONE',  ( 1.709358663124999955, 1516.542957540330008, 216.0554336257470140 ) ) ;
#22803 = EDGE_LOOP ( 'NONE', ( #11524, #21066, #53449, #97053 ) ) ;
#22804 = CARTESIAN_POINT ( 'NONE',  ( 7.710670337728189772, 1516.596880753980031, 207.8068798501710148 ) ) ;
#22805 = CARTESIAN_POINT ( 'NONE',  ( -20.94370973279999859, 1470.568016209030020, 270.0430967339979702 ) ) ;
#22806 = CARTESIAN_POINT ( 'NONE',  ( -4.161387699379999638, 1448.641049173779948, 185.0955448841980342 ) ) ;
#22807 = ADVANCED_FACE ( 'NONE', ( #53231 ), #26336, .T. ) ;
#22808 = EDGE_CURVE ( 'NONE', #97581, #48553, #54420, .T. ) ;
#22809 = CARTESIAN_POINT ( 'NONE',  ( 2.453594186590829734E-14, 1422.045703570280011, 122.9812613506829990 ) ) ;
#22810 = CARTESIAN_POINT ( 'NONE',  ( -3.527118517899999972, 1475.290297289889850, 218.8061209762090016 ) ) ;
#22811 = CARTESIAN_POINT ( 'NONE',  ( 18.85256022773900142, 1509.571403847920010, 185.0368585482190156 ) ) ;
#22812 = CARTESIAN_POINT ( 'NONE',  ( 11.60004869885216472, 1425.961673676839155, 138.7012799492945305 ) ) ;
#22813 = CARTESIAN_POINT ( 'NONE',  ( 2.543548742221767966, 1417.726526468788506, 233.7963267752078877 ) ) ;
#22814 = CARTESIAN_POINT ( 'NONE',  ( -2.640038298730670085, 1471.339824109930078, 183.8587828106460336 ) ) ;
#22815 = DIRECTION ( 'NONE',  ( 0.000000000000000000, 0.000000000000000000, 1.000000000000000000 ) ) ;
#22816 = CARTESIAN_POINT ( 'NONE',  ( 6.823004602010799484E-10, 1406.914363899970112, 222.1218459632040094 ) ) ;
#22817 = CARTESIAN_POINT ( 'NONE',  ( 31.90208977857959738, 1440.913060383340053, 243.8577475931840013 ) ) ;
#22819 = FACE_BOUND ( 'NONE', #25755, .T. ) ;
#22818 = SPHERICAL_SURFACE ( 'NONE', #80520, 2.000000000000000000 ) ;
#22820 = CARTESIAN_POINT ( 'NONE',  ( 3.235048521747439842, 1466.472015811129950, 219.6884157710169916 ) ) ;
#22821 = EDGE_LOOP ( 'NONE', ( #91526, #87664, #98159, #85220 ) ) ;
#22822 = ORIENTED_EDGE ( 'NONE', *, *, #48148, .F. ) ;
#22823 = EDGE_CURVE ( 'NONE', #78966, #21516, #25780, .T. ) ;
#22824 = CARTESIAN_POINT ( 'NONE',  ( 13.51610093808349866, 1443.913060387330006, 206.7785865123599933 ) ) ;
#22825 = AXIS2_PLACEMENT_3D ( 'NONE', #62864, #97513, #1260 ) ;
#22826 = CARTESIAN_POINT ( 'NONE',  ( 3.034663161748390348, 1440.440203176670138, 157.2490260270419924 ) ) ;
#22827 = CARTESIAN_POINT ( 'NONE',  ( -2.530629316699999798, 1443.373190519289892, 200.1619764056190149 ) ) ;
#22828 = CARTESIAN_POINT ( 'NONE',  ( -1.546867746862319981, 1416.839692133689823, 228.0214409764060122 ) ) ;
#22829 = DIRECTION ( 'NONE',  ( -0.6736849260863839728, 0.000000000000000000, 0.7390186874254150995 ) ) ;
#22830 = EDGE_CURVE ( 'NONE', #55613, #13824, #77863, .T. ) ;
#22831 = CARTESIAN_POINT ( 'NONE',  ( -4.848919996459999382, 1489.192135936889827, 188.8958457811990002 ) ) ;
#22832 = CARTESIAN_POINT ( 'NONE',  ( 16.33500296837753041, 1522.051704408389924, 214.0369884316988305 ) ) ;
#22833 = CARTESIAN_POINT ( 'NONE',  ( -30.31940284289361998, 1523.456924617336654, 222.4933038711236577 ) ) ;
#22834 = CARTESIAN_POINT ( 'NONE',  ( -38.67527654348140231, 1383.830167042470066, 239.5321249052780104 ) ) ;
#22835 = PRESENTATION_LAYER_ASSIGNMENT (  '', '', ( #47889 ) ) ;
#22836 = CARTESIAN_POINT ( 'NONE',  ( -4.813011424114999492, 1510.693074690949970, 201.5657718700469729 ) ) ;
#22837 = CARTESIAN_POINT ( 'NONE',  ( -12.78776258900000151, 1416.851343898729965, 195.5391574245979882 ) ) ;
#22838 = CARTESIAN_POINT ( 'NONE',  ( -12.78943302956389871, 1502.708798875820094, 209.0180534851929792 ) ) ;
#22839 = CARTESIAN_POINT ( 'NONE',  ( 2.745794554380000196, 1464.572481067230001, 236.3736730967980009 ) ) ;
#22841 = ORIENTED_EDGE ( 'NONE', *, *, #22726, .T. ) ;
#22840 = CARTESIAN_POINT ( 'NONE',  ( -2.320817964079999740, 1456.878784100789971, 218.4789852815589768 ) ) ;
#22842 = CARTESIAN_POINT ( 'NONE',  ( 34.09113935471038559, 1523.429859730330918, 219.7507174562238390 ) ) ;
#22843 = CARTESIAN_POINT ( 'NONE',  ( -30.22254988470000114, 1380.278343034279942, 209.1988840933390179 ) ) ;
#22844 = CARTESIAN_POINT ( 'NONE',  ( 2.716551985052390261, 1508.551704408389924, 204.1452468848800095 ) ) ;
#22846 = ORIENTED_EDGE ( 'NONE', *, *, #67347, .F. ) ;
#22845 = CARTESIAN_POINT ( 'NONE',  ( -18.12896501130950000, 1435.130582088173014, 143.3945274439228683 ) ) ;
#22847 = ORIENTED_EDGE ( 'NONE', *, *, #35885, .T. ) ;
#22848 = CARTESIAN_POINT ( 'NONE',  ( 0.5624690339869999889, 1416.828040475229955, 190.4759594386979984 ) ) ;
#22849 = CARTESIAN_POINT ( 'NONE',  ( 34.03221148485429381, 1437.015149023179902, 136.5575608309000017 ) ) ;
#22850 = CARTESIAN_POINT ( 'NONE',  ( 3.487587010899057205, 1508.884207228265495, 213.6131390680183983 ) ) ;
#22851 = CARTESIAN_POINT ( 'NONE',  ( -11.60004869885204037, 1426.466820350880425, 135.9733956539067492 ) ) ;
#22852 = B_SPLINE_CURVE_WITH_KNOTS ( 'NONE', 5,
 ( #17589, #61321, #9768, #9230, #78078, #76989 ),
 .UNSPECIFIED., .F., .F.,
 ( 6, 6 ),
 ( -2.000000000000000000, -3.790778899670499413E-06 ),
 .UNSPECIFIED. ) ;
#22853 = CARTESIAN_POINT ( 'NONE',  ( -105.6667097630000001, 1379.864153498549967, 301.0124091048589889 ) ) ;
#22854 = CARTESIAN_POINT ( 'NONE',  ( -12.27608956948616026, 1509.341750881446160, 235.6884000609552174 ) ) ;
#22855 = CARTESIAN_POINT ( 'NONE',  ( -16.24421748424699885, 1508.551704408389924, 213.5434314520410339 ) ) ;
#22856 = AXIS2_PLACEMENT_3D ( 'NONE', #27278, #86628, #36235 ) ;
#22857 = CARTESIAN_POINT ( 'NONE',  ( 5.533180669438849897, 1409.106283314009943, 195.2035214513250025 ) ) ;
#22858 = CARTESIAN_POINT ( 'NONE',  ( 18.12085357038199973, 1425.008622401126104, 225.3887946363380195 ) ) ;
#22859 = CARTESIAN_POINT ( 'NONE',  ( 8.731332846349999954, 1459.404707344790040, 227.0651519182989944 ) ) ;
#22860 = CARTESIAN_POINT ( 'NONE',  ( -18.77987601960000319, 1452.005536572529991, 191.4523375352979997 ) ) ;
#22861 = CARTESIAN_POINT ( 'NONE',  ( -2.549034377637660054, 1448.919557215109990, 183.6707458025049959 ) ) ;
#22862 = ORIENTED_EDGE ( 'NONE', *, *, #13885, .T. ) ;
#22863 =( BOUNDED_SURFACE ( )  B_SPLINE_SURFACE ( 3, 2, ( 
 ( #80172, #36516, #54450 ),
 ( #70709, #62300, #88043 ),
 ( #96986, #96427, #19705 ),
 ( #3489, #11327, #37064 ),
 ( #53908, #105381, #28669 ),
 ( #20249, #107017, #82375 ) ),
 .UNSPECIFIED., .F., .F., .F. ) 
 B_SPLINE_SURFACE_WITH_KNOTS ( ( 4, 2, 4 ),
 ( 3, 3 ),
 ( -2.493664996716660198E-17, 0.001312027981647334932, 0.002624055963294695017 ),
 ( 0.000000000000000000, 1.000000000000000000 ),
 .UNSPECIFIED. ) 
 GEOMETRIC_REPRESENTATION_ITEM ( )  RATIONAL_B_SPLINE_SURFACE ( (
 ( 1.000000000000000000, 0.9376006582765856745, 1.000000000000000000),
 ( 1.000000000000000000, 0.9569320108032824956, 1.000000000000000000),
 ( 1.000000000000000000, 0.9725743441605260164, 1.000000000000000000),
 ( 1.000000000000000000, 0.9942095667149332128, 1.000000000000000000),
 ( 1.000000000000000000, 1.000043666449679236, 1.000000000000000000),
 ( 1.000000000000000000, 1.000000000000000000, 1.000000000000000000) ) ) 
 REPRESENTATION_ITEM ( '' )  SURFACE ( )  );
#22864 = CARTESIAN_POINT ( 'NONE',  ( 16.68062049856738938, 1526.382868172863937, 236.8314524626094055 ) ) ;
#22865 = CARTESIAN_POINT ( 'NONE',  ( 19.30835196975910151, 1456.473163433020090, 228.7023210262429984 ) ) ;
#22866 = CARTESIAN_POINT ( 'NONE',  ( -12.03079994940000041, 1433.765461728309901, 150.2535422845980122 ) ) ;
#22867 = CARTESIAN_POINT ( 'NONE',  ( 2.442485525661060236E-10, 1465.745499712829996, 240.5333668247809840 ) ) ;
#22868 = CARTESIAN_POINT ( 'NONE',  ( -33.42844755915814403, 1522.861859112239472, 222.1271778627171329 ) ) ;
#22869 = CARTESIAN_POINT ( 'NONE',  ( -15.57028380409999890, 1420.200962988549918, 211.3154909670090262 ) ) ;
#22870 = CARTESIAN_POINT ( 'NONE',  ( -108.6463189709999995, 1386.108622646309868, 311.0727272582590217 ) ) ;
#22871 = CARTESIAN_POINT ( 'NONE',  ( -7.558973857277559993, 1511.169205552290123, 215.1889176642449968 ) ) ;
#22872 = CARTESIAN_POINT ( 'NONE',  ( -9.655745333040000489, 1363.739547551590022, 207.6218459616989946 ) ) ;
#22873 = CARTESIAN_POINT ( 'NONE',  ( -46.02294315243130285, 1440.251626319409979, 268.4962080042990351 ) ) ;
#22874 = CARTESIAN_POINT ( 'NONE',  ( 3.448830483803564828, 1512.187213306747481, 175.1594891075192209 ) ) ;
#22875 = DIRECTION ( 'NONE',  ( -1.000000000000000000, 0.000000000000000000, 0.000000000000000000 ) ) ;
#22876 = CARTESIAN_POINT ( 'NONE',  ( 3.445201488374999954, 1516.743010792419909, 207.4064848398570291 ) ) ;
#22877 = AXIS2_PLACEMENT_3D ( 'NONE', #50171, #58563, #101080 ) ;
#22878 = DIRECTION ( 'NONE',  ( -5.980589973904019347E-17, 1.000000000000000000, -1.736889445713099699E-16 ) ) ;
#22879 =( LENGTH_UNIT ( ) NAMED_UNIT ( * ) SI_UNIT ( .MILLI., .METRE. ) );
#22880 = CARTESIAN_POINT ( 'NONE',  ( -14.22857088754179955, 1379.587268947920165, 207.8738992505469980 ) ) ;
#22881 = CARTESIAN_POINT ( 'NONE',  ( 7.471609634030699887, 1425.264358481019826, 212.3048529994830176 ) ) ;
#22882 = EDGE_LOOP ( 'NONE', ( #61541, #99537, #105849, #56378, #25799 ) ) ;
#22883 = CARTESIAN_POINT ( 'NONE',  ( 33.33289073430000116, 1436.626756256089948, 248.0947902361980084 ) ) ;
#22884 = CARTESIAN_POINT ( 'NONE',  ( -0.5624325259219991047, 1417.052906817089934, 204.0409946397689964 ) ) ;
#22886 = CARTESIAN_POINT ( 'NONE',  ( -14.97619056944999905, 1512.179780174510142, 221.6162844670500078 ) ) ;
#22885 = CARTESIAN_POINT ( 'NONE',  ( -0.5073518436949999710, 1478.157470870929956, 182.0636189244980017 ) ) ;
#22887 = CARTESIAN_POINT ( 'NONE',  ( 1.585275487640332992, 1508.725511249230976, 180.2575163523052311 ) ) ;
#22888 = CARTESIAN_POINT ( 'NONE',  ( -17.22939366680000361, 1424.306326232029960, 225.2395885692979789 ) ) ;
#22889 = CARTESIAN_POINT ( 'NONE',  ( 7.644479751013899538, 1517.051704408389924, 209.5582147999029985 ) ) ;
#22890 = ADVANCED_FACE ( 'NONE', ( #61099 ), #10667, .T. ) ;
#22891 = CARTESIAN_POINT ( 'NONE',  ( -18.52802004830289917, 1452.266047670050057, 144.8817897837620023 ) ) ;
#22892 = CARTESIAN_POINT ( 'NONE',  ( 28.26594772519999665, 1451.926830112729931, 135.3157343196979809 ) ) ;
#22893 = ORIENTED_EDGE ( 'NONE', *, *, #53430, .T. ) ;
#22894 = CARTESIAN_POINT ( 'NONE',  ( -107.4518942052619934, 1378.913060387349788, 300.6024564064820197 ) ) ;
#22895 = CARTESIAN_POINT ( 'NONE',  ( 16.66231036550724909, 1523.604703353109699, 237.7554842931445762 ) ) ;
#22896 = CARTESIAN_POINT ( 'NONE',  ( 16.72074854044890202, 1422.807583317619901, 227.2334935513920016 ) ) ;
#22897 = CARTESIAN_POINT ( 'NONE',  ( -3.931500257436271184, 1448.981219870369159, 185.0407271323569489 ) ) ;
#22898 = VERTEX_POINT ( 'NONE', #35303 ) ;
#22899 = VERTEX_POINT ( 'NONE', #95215 ) ;
#22900 = AXIS2_PLACEMENT_3D ( 'NONE', #19392, #9905, #1524 ) ;
#22901 = CARTESIAN_POINT ( 'NONE',  ( -37.21779252409999827, 1384.846743917189997, 210.1685376368189964 ) ) ;
#22902 = CARTESIAN_POINT ( 'NONE',  ( -24.08818477799610136, 1410.733297714309856, 209.1412261076660002 ) ) ;
#22903 = ORIENTED_EDGE ( 'NONE', *, *, #505, .F. ) ;
#22904 = CARTESIAN_POINT ( 'NONE',  ( 4.487249369889919848, 1509.038630944639863, 205.6342588291649918 ) ) ;
#22905 = CARTESIAN_POINT ( 'NONE',  ( -106.6183162539999927, 1379.688366450070134, 308.3260602744589960 ) ) ;
#22906 = AXIS2_PLACEMENT_3D ( 'NONE', #71275, #56641, #20808 ) ;
#22907 = AXIS2_PLACEMENT_3D ( 'NONE', #75629, #102448, #16767 ) ;
#22908 = CARTESIAN_POINT ( 'NONE',  ( -0.6048355684939999977, 1507.643512198230155, 237.2981531702980078 ) ) ;
#22909 = CARTESIAN_POINT ( 'NONE',  ( -17.38482318170000340, 1410.884444280730122, 225.7833539147979707 ) ) ;
#22910 = AXIS2_PLACEMENT_3D ( 'NONE', #10705, #28040, #1209 ) ;
#22911 = CARTESIAN_POINT ( 'NONE',  ( 45.23891030401149749, 1446.067212034520026, 266.2005835343620106 ) ) ;
#22912 = CARTESIAN_POINT ( 'NONE',  ( -4.491288177712689844, 1508.884219106000046, 205.6342588895329868 ) ) ;
#22913 = CARTESIAN_POINT ( 'NONE',  ( -0.04185304873460000269, 1420.435852020029870, 183.3187823327980084 ) ) ;
#22914 = CARTESIAN_POINT ( 'NONE',  ( 4.610938211375000151, 1516.815231249920089, 205.0813186281270077 ) ) ;
#22915 = EDGE_LOOP ( 'NONE', ( #104652, #3793, #42988, #45792, #33384 ) ) ;
#22916 = CARTESIAN_POINT ( 'NONE',  ( 10.14952118758730037, 1481.589675501239981, 215.1524303884280300 ) ) ;
#22917 = CIRCLE ( 'NONE', #108794, 41.35631769782009570 ) ;
#22918 = CARTESIAN_POINT ( 'NONE',  ( 6.802837640179999923, 1469.003421131590130, 208.5716255075389824 ) ) ;
#22919 = CARTESIAN_POINT ( 'NONE',  ( 12.86933871999277734, 1442.875697286375271, 186.9746649412792863 ) ) ;
#22920 = VERTEX_POINT ( 'NONE', #94095 ) ;
#22921 = ORIENTED_EDGE ( 'NONE', *, *, #13086, .T. ) ;
#22922 = CARTESIAN_POINT ( 'NONE',  ( 2.372478608332517336, 1522.382868172863937, 174.8996806668726549 ) ) ;
#22923 = EDGE_CURVE ( 'NONE', #7222, #777, #17367, .T. ) ;
#22924 = FACE_OUTER_BOUND ( 'NONE', #86981, .T. ) ;
#22925 = CARTESIAN_POINT ( 'NONE',  ( -4.263034242833646736, 1424.151093693061966, 185.2294109041083345 ) ) ;
#22926 = B_SPLINE_CURVE_WITH_KNOTS ( 'NONE', 3,
 ( #69802, #70358, #27765, #80384, #105030, #103920, #36721, #44581, #89327, #61956, #96071, #70914, #19905, #1475, #88235, #11526, #79840, #37280, #63073, #37828, #106132, #29405, #97725, #106671, #107782, #65794, #92081, #66361, #107228, #100480, #91536, #5880, #90972, #83134, #13693, #6430, #47878, #65247, #73650, #23762, #29960, #64153, #40575, #15356, #82589, #74745, #22633, #31067, #108334, #57949, #13143, #82016, #56282, #49001, #80931, #38362, #98825, #108884, #55756, #47327, #32177, #74203, #4229, #90413, #73088, #72540, #81457, #98272, #40024, #21544, #22086, #99916, #4762, #5321, #99359, #56839, #39480, #31617, #23211, #48451, #14261, #57411, #14814, #89874, #38906, #30518, #64708, #1954, #35524, #3064, #79757, #36092, #10890, #70832, #37192, #27136, #97099, #94883, #104942, #1382, #88154, #18160, #9769, #62989, #70278, #2512, #36636, #19251, #43935, #44494, #11442, #95985, #104387, #52357, #28232, #86474, #62420, #60759, #27684, #53457, #69717, #87601, #103836, #19819, #45617, #71386, #28791, #96545, #54026, #103255, #105499, #78638, #61322, #46169, #20364, #61868, #79206, #11985, #54571 ),
 .UNSPECIFIED., .F., .F.,
 ( 4, 3, 3, 3, 3, 3, 3, 3, 3, 3, 3, 3, 3, 3, 3, 3, 3, 3, 3, 3, 3, 3, 3, 3, 3, 3, 3, 3, 3, 3, 3, 3, 3, 3, 3, 3, 3, 3, 3, 3, 3, 3, 3, 3, 3, 3, 4 ),
 ( -29.89576149997330035, -27.93066200461270299, -25.77370346504809717, -23.34209498118620019, -21.15356506553399996, -19.17231324189400254, -17.32574871330879773, -15.57444149077680073, -13.93194560254629977, -12.30963008990289964, -10.75531893239759995, -9.233619782032960188, -7.754183433082701526, -6.990622735083189099, -5.857671294819962071, -4.582768379358419963, -3.327899758805628494, -2.055712155490059700, -0.7650328573970526236, 0.5655583436393420982, 1.790039819582720071, 3.161605655697446338, 4.341552028872310842, 5.758073910464208467, 7.176843838457021008, 8.662804671664009248, 10.14364948196800142, 11.62076542165629789, 13.16096764701680044, 14.68906546968660010, 15.67372708160739947, 16.66824346166319870, 17.65430721703309658, 18.64662466131919771, 19.64424912027570613, 20.64604275194010441, 21.65069957589760108, 22.65678741700699916, 23.66280606768819794, 24.66584900615290010, 25.66547144059130758, 26.66059974112859621, 27.65030847251239621, 28.63422864500930487, 29.60788831232530427, 30.59693873741260361, 31.58598916250000244 ),
 .UNSPECIFIED. ) ;
#22927 = CARTESIAN_POINT ( 'NONE',  ( 6.195357806510189747, 1504.701517326509929, 220.2771928074470225 ) ) ;
#22928 = EDGE_CURVE ( 'NONE', #109266, #68079, #102557, .T. ) ;
#22929 = CARTESIAN_POINT ( 'NONE',  ( 12.65728676320000012, 1420.119835126070029, 200.3472210942090044 ) ) ;
#22930 = CARTESIAN_POINT ( 'NONE',  ( 5.385523159618170297, 1511.435001054559962, 217.7746220610370074 ) ) ;
#22931 = FACE_OUTER_BOUND ( 'NONE', #45893, .T. ) ;
#22932 = CARTESIAN_POINT ( 'NONE',  ( -5.030159814880000191, 1495.846928005290010, 198.9636958132990117 ) ) ;
#22933 = CARTESIAN_POINT ( 'NONE',  ( 0.03684459895644798949, 1409.761386472454660, 233.0934521079545334 ) ) ;
#22935 = CARTESIAN_POINT ( 'NONE',  ( -105.7922123186220063, 1391.671139054730020, 305.5979281096929867 ) ) ;
#22934 = CARTESIAN_POINT ( 'NONE',  ( -13.09172112396450061, 1434.821155476560079, 149.0943168348729841 ) ) ;
#22936 = CARTESIAN_POINT ( 'NONE',  ( 11.43232951270710096, 1426.317992301700087, 206.5079432659420036 ) ) ;
#22937 = EDGE_CURVE ( 'NONE', #77302, #49611, #89431, .T. ) ;
#22938 = AXIS2_PLACEMENT_3D ( 'NONE', #60665, #59548, #8568 ) ;
#22939 = CARTESIAN_POINT ( 'NONE',  ( -24.77531906373999959, 1509.438340469299874, 222.6714807735559987 ) ) ;
#22940 = CARTESIAN_POINT ( 'NONE',  ( -7.665825202615000222, 1514.407352313670117, 203.3587699272470104 ) ) ;
#22941 = ORIENTED_EDGE ( 'NONE', *, *, #58529, .T. ) ;
#22942 = CARTESIAN_POINT ( 'NONE',  ( 19.00000000000000000, 1440.913060387330006, 209.1218459616979999 ) ) ;
#22943 = DIRECTION ( 'NONE',  ( -1.000000000000000000, 0.000000000000000000, 0.000000000000000000 ) ) ;
#22944 = CARTESIAN_POINT ( 'NONE',  ( -99.83489338526950974, 1384.946744245190075, 310.8186357852670199 ) ) ;
#22945 = EDGE_CURVE ( 'NONE', #82950, #103478, #4993, .T. ) ;
#22946 = CARTESIAN_POINT ( 'NONE',  ( -8.515298204750001432, 1385.582038790579873, 199.8542761591889985 ) ) ;
#22947 = CARTESIAN_POINT ( 'NONE',  ( 19.88011795350000099, 1476.500998830189928, 213.0752383808189734 ) ) ;
#22949 = ORIENTED_EDGE ( 'NONE', *, *, #91905, .T. ) ;
#22948 = CARTESIAN_POINT ( 'NONE',  ( 11.04498765331799959, 1424.577033446239966, 203.0973991204349716 ) ) ;
#22950 = CARTESIAN_POINT ( 'NONE',  ( 2.495739975459999815, 1430.974676233789978, 218.2901151006489897 ) ) ;
#22951 = CARTESIAN_POINT ( 'NONE',  ( -5.551115123129999164E-15, 1443.913060387330006, 150.8032249175980155 ) ) ;
#22952 = CARTESIAN_POINT ( 'NONE',  ( -14.20204673689999986, 1416.837080247930089, 221.7382503592980072 ) ) ;
#22953 = CARTESIAN_POINT ( 'NONE',  ( 11.29458427579999835, 1433.957910099769833, 151.5308368996980164 ) ) ;
#22954 = CARTESIAN_POINT ( 'NONE',  ( 42.15865170690000241, 1450.809155637750109, 271.1218459616979999 ) ) ;
#22955 = CARTESIAN_POINT ( 'NONE',  ( 12.77961858748670032, 1414.913057834419988, 198.0260298875460023 ) ) ;
#22956 = CARTESIAN_POINT ( 'NONE',  ( 0.003568499702431209702, 1467.142144108200000, 235.6416276161930057 ) ) ;
#22957 = CARTESIAN_POINT ( 'NONE',  ( -5.242935297045000276, 1514.523084723979991, 216.7782120477669991 ) ) ;
#22958 = CARTESIAN_POINT ( 'NONE',  ( -109.4214834242509795, 1387.219425580758980, 297.3509835002536761 ) ) ;
#22959 = CARTESIAN_POINT ( 'NONE',  ( 10.96015508933500016, 1512.830284628050094, 225.0317485278669949 ) ) ;
#22960 = DIRECTION ( 'NONE',  ( 0.000000000000000000, 1.000000000000000000, 0.000000000000000000 ) ) ;
#22961 = DIRECTION ( 'NONE',  ( -1.000000000000000000, 0.000000000000000000, 0.000000000000000000 ) ) ;
#22962 = CARTESIAN_POINT ( 'NONE',  ( -17.67161397030000103, 1410.454767058429979, 225.2840158849979844 ) ) ;
#22964 = EDGE_CURVE ( 'NONE', #15749, #94550, #11638, .T. ) ;
#22963 = EDGE_CURVE ( 'NONE', #8806, #71548, #72406, .T. ) ;
#22965 = CARTESIAN_POINT ( 'NONE',  ( -7.654188446680000091, 1491.752080352689973, 210.6569740451089956 ) ) ;
#22966 = CARTESIAN_POINT ( 'NONE',  ( 6.063466852619999514, 1461.859068799589977, 206.6237464781989956 ) ) ;
#22967 = CARTESIAN_POINT ( 'NONE',  ( -17.48733164209449953, 1410.446457955379856, 192.6364576323030064 ) ) ;
#22968 = CARTESIAN_POINT ( 'NONE',  ( -0.7398872336889990020, 1515.545288638290003, 204.9978666827690006 ) ) ;
#22969 = CARTESIAN_POINT ( 'NONE',  ( 11.14671379024469999, 1434.019377051509991, 151.6529839732360188 ) ) ;
#22970 = CARTESIAN_POINT ( 'NONE',  ( -17.11733441484010143, 1420.830776991170069, 201.6585818365429645 ) ) ;
#22971 = EDGE_CURVE ( 'NONE', #50075, #76159, #10354, .T. ) ;
#22972 = CARTESIAN_POINT ( 'NONE',  ( -8.506178470120000057, 1416.518532928330160, 225.1689260078979657 ) ) ;
#22973 = CARTESIAN_POINT ( 'NONE',  ( 0.2127819998068850027, 1455.787616099680008, 183.1338090387140198 ) ) ;
#22974 = B_SPLINE_CURVE_WITH_KNOTS ( 'NONE', 5,
 ( #930, #78159, #84354, #16562, #67578, #25531, #34505, #60274, #41799, #86559, #93300, #94392, #68681, #1471, #85438 ),
 .UNSPECIFIED., .F., .F.,
 ( 6, 3, 3, 3, 6 ),
 ( 0.000000000000000000, 0.1618001797507035155, 0.2522523987000994117, 0.4661970989643994812, 1.000000000000000000 ),
 .UNSPECIFIED. ) ;
#22976 = VERTEX_POINT ( 'NONE', #15464 ) ;
#22975 = CARTESIAN_POINT ( 'NONE',  ( -9.972378110560478959, 1407.313660260299912, 200.5612547303060182 ) ) ;
#22977 = DIRECTION ( 'NONE',  ( 0.000000000000000000, 0.000000000000000000, 1.000000000000000000 ) ) ;
#22978 = CARTESIAN_POINT ( 'NONE',  ( -29.17496190384160215, 1509.931872506899936, 211.7252048115940113 ) ) ;
#22979 = CARTESIAN_POINT ( 'NONE',  ( 13.19869229439999891, 1434.900411147940304, 148.5018195976979882 ) ) ;
#22980 = CARTESIAN_POINT ( 'NONE',  ( -36.70996913416379925, 1436.286710641700211, 134.0999999969339740 ) ) ;
#22981 = CARTESIAN_POINT ( 'NONE',  ( -3.994937574034520100, 1430.106198372560129, 201.8091617894969829 ) ) ;
#22982 = EDGE_LOOP ( 'NONE', ( #59294, #99332, #54033, #80998, #96099 ) ) ;
#22983 = CARTESIAN_POINT ( 'NONE',  ( -16.66231036550740541, 1523.604703353109699, 180.4882076302515372 ) ) ;
#22984 = CARTESIAN_POINT ( 'NONE',  ( -3.034143074970000242, 1440.440281792710039, 157.2495483846980164 ) ) ;
#22985 = CARTESIAN_POINT ( 'NONE',  ( -103.5801209296959939, 1379.883073482990085, 303.9981235976169955 ) ) ;
#22986 = CARTESIAN_POINT ( 'NONE',  ( -11.03225848849999835, 1492.060404916889865, 208.5626278536280154 ) ) ;
#22987 = LINE ( 'NONE', #82912, #67887 ) ;
#22988 = CARTESIAN_POINT ( 'NONE',  ( 16.41933790207369981, 1509.448631503890056, 232.9213397454749952 ) ) ;
#22989 = CARTESIAN_POINT ( 'NONE',  ( 44.41513596800174923, 1432.959676725966801, 269.0091301501007592 ) ) ;
#22990 = AXIS2_PLACEMENT_3D ( 'NONE', #7204, #73864, #31289 ) ;
#22991 = CARTESIAN_POINT ( 'NONE',  ( 8.758613636697381466, 1427.348504481640020, 211.4846159547069817 ) ) ;
#22992 = CARTESIAN_POINT ( 'NONE',  ( -12.49429521540000110, 1379.282925338159885, 210.7339652385390139 ) ) ;
#22993 = LINE ( 'NONE', #99149, #9680 ) ;
#22994 = CARTESIAN_POINT ( 'NONE',  ( -58.93529294637219351, 1385.056221149589874, 241.7207647726530126 ) ) ;
#22995 = CARTESIAN_POINT ( 'NONE',  ( 15.12003195112066933, 1522.051704408389924, 199.7262892757531745 ) ) ;
#22996 = CARTESIAN_POINT ( 'NONE',  ( -24.61293950550089704, 1444.770188684140066, 210.8869336946189890 ) ) ;
#22997 = ORIENTED_EDGE ( 'NONE', *, *, #57868, .T. ) ;
#22998 = AXIS2_PLACEMENT_3D ( 'NONE', #1181, #1736, #96326 ) ;
#22999 = CARTESIAN_POINT ( 'NONE',  ( 16.65010197087796939, 1526.345556099435726, 183.3431577551421299 ) ) ;
#23000 = CARTESIAN_POINT ( 'NONE',  ( -15.83424720296929600, 1409.491973313159860, 225.5800623810480090 ) ) ;
#23002 = EDGE_LOOP ( 'NONE', ( #107902, #69674, #56107, #65279, #28038, #31999, #11542, #50629, #7848, #63714 ) ) ;
#23001 = CARTESIAN_POINT ( 'NONE',  ( 0.4872611956131389643, 1418.409299200879786, 184.7253510064639954 ) ) ;
#23003 = CARTESIAN_POINT ( 'NONE',  ( -14.12786062849999880, 1509.345507838329922, 183.3895953394980154 ) ) ;
#23004 = CIRCLE ( 'NONE', #107110, 1.999999999999997780 ) ;
#23005 = CARTESIAN_POINT ( 'NONE',  ( 40.26684313263383785, 1444.090643208445044, 137.1176951931856252 ) ) ;
#23006 = CARTESIAN_POINT ( 'NONE',  ( 22.52609172630000245, 1509.699688844029879, 227.3081661019980118 ) ) ;
#23007 = CARTESIAN_POINT ( 'NONE',  ( -109.3027203169999950, 1384.654548469560041, 311.2558226302590469 ) ) ;
#23008 = CARTESIAN_POINT ( 'NONE',  ( -0.07668964449979870368, 1420.270968488830249, 183.5370586615759976 ) ) ;
#23009 = CARTESIAN_POINT ( 'NONE',  ( 1.300999044849999953, 1466.796436742230071, 235.1605608302979817 ) ) ;
#23010 = CARTESIAN_POINT ( 'NONE',  ( 20.88842237349999920, 1409.642500170129779, 215.0570138386379710 ) ) ;
#23011 = CARTESIAN_POINT ( 'NONE',  ( -0.03822279852769269737, 1452.916107821060223, 185.2425342979790059 ) ) ;
#23012 = CARTESIAN_POINT ( 'NONE',  ( -19.76672171450000093, 1468.192140521490046, 204.4230837022790297 ) ) ;
#23013 = CARTESIAN_POINT ( 'NONE',  ( -16.85198166820000054, 1421.787005334130072, 226.9070353815980070 ) ) ;
#23015 = CARTESIAN_POINT ( 'NONE',  ( 22.04844205597441231, 1506.512156832560095, 209.0500279883449934 ) ) ;
#23014 = CARTESIAN_POINT ( 'NONE',  ( -4.264264835409092846, 1511.427926070662124, 200.8411546547189630 ) ) ;
#23016 = CARTESIAN_POINT ( 'NONE',  ( -12.53694325390000053, 1380.612673806029761, 215.4769779826689842 ) ) ;
#23017 = CARTESIAN_POINT ( 'NONE',  ( -107.3060008061400197, 1358.631207110790911, 307.5510129717682162 ) ) ;
#23018 = CARTESIAN_POINT ( 'NONE',  ( 21.39771952614790251, 1509.704955107219803, 188.4542851670070149 ) ) ;
#23019 = CARTESIAN_POINT ( 'NONE',  ( -1.108882943119999798, 1417.340802340130040, 234.6777931048980008 ) ) ;
#23020 = CARTESIAN_POINT ( 'NONE',  ( 6.358435812109999752, 1368.427897723179967, 210.6218459616991936 ) ) ;
#23021 = CARTESIAN_POINT ( 'NONE',  ( -2.491188396525000126, 1516.733363207009916, 205.0947945262969938 ) ) ;
#23022 = AXIS2_PLACEMENT_3D ( 'NONE', #83367, #66609, #32963 ) ;
#23023 = DIRECTION ( 'NONE',  ( -0.3741289577892935592, 0.04424996905086078791, 0.9263203890568829646 ) ) ;
#23024 = ORIENTED_EDGE ( 'NONE', *, *, #66667, .F. ) ;
#23025 = CARTESIAN_POINT ( 'NONE',  ( -109.1147032029209925, 1384.600588565270073, 311.2513737746320430 ) ) ;
#23026 = CARTESIAN_POINT ( 'NONE',  ( -4.247058430120979722, 1441.377667071719998, 161.6040409347519926 ) ) ;
#23028 = ORIENTED_EDGE ( 'NONE', *, *, #61812, .T. ) ;
#23027 = CARTESIAN_POINT ( 'NONE',  ( -68.71407884372058561, 1379.747795434490172, 280.3090442124819788 ) ) ;
#23029 = VERTEX_POINT ( 'NONE', #75943 ) ;
#23030 = CARTESIAN_POINT ( 'NONE',  ( -11.56858258461559963, 1378.020591857488171, 213.4395426976007002 ) ) ;
#23031 = ORIENTED_EDGE ( 'NONE', *, *, #2886, .F. ) ;
#23032 = CARTESIAN_POINT ( 'NONE',  ( -1.740723996199489809, 1486.328230267929939, 220.9124301049980090 ) ) ;
#23033 = CARTESIAN_POINT ( 'NONE',  ( 11.42348759009999881, 1501.742913944189922, 208.1569337396019819 ) ) ;
#23035 = CARTESIAN_POINT ( 'NONE',  ( 15.77937509389199988, 1409.566674589380000, 192.3662456604770341 ) ) ;
#23034 = CARTESIAN_POINT ( 'NONE',  ( -11.44198449339859636, 1425.478516144404239, 144.4778108111833035 ) ) ;
#23036 = CARTESIAN_POINT ( 'NONE',  ( 5.014195101815000832, 1517.120861839400050, 210.8273123806970091 ) ) ;
#23037 = LINE ( 'NONE', #77872, #21798 ) ;
#23038 = CARTESIAN_POINT ( 'NONE',  ( -106.3515999725659924, 1378.913060387349788, 306.1522039670650202 ) ) ;
#23039 = CARTESIAN_POINT ( 'NONE',  ( -0.4018488818434700072, 1508.986311531569754, 179.3607565668060033 ) ) ;
#23040 = CARTESIAN_POINT ( 'NONE',  ( 17.03742609228944715, 1460.377087626990487, 228.7183869844807589 ) ) ;
#23041 = DIRECTION ( 'NONE',  ( 1.000000000000000000, 0.000000000000000000, 0.000000000000000000 ) ) ;
#23042 = CARTESIAN_POINT ( 'NONE',  ( 4.923775256296569758, 1508.551704408389924, 212.1750878591210210 ) ) ;
#23043 = CARTESIAN_POINT ( 'NONE',  ( -39.86280671402410292, 1441.327267167989930, 136.8612332179159807 ) ) ;
#23044 = CARTESIAN_POINT ( 'NONE',  ( -5.586172216781320365, 1491.246046052670181, 185.8699220213879926 ) ) ;
#23045 = DIRECTION ( 'NONE',  ( 0.000000000000000000, 1.000000000000000000, 0.000000000000000000 ) ) ;
#23046 = VERTEX_POINT ( 'NONE', #32288 ) ;
#23047 = ORIENTED_EDGE ( 'NONE', *, *, #79743, .T. ) ;
#23048 = CARTESIAN_POINT ( 'NONE',  ( 12.99443939928278979, 1410.739937348442027, 228.5427893857089998 ) ) ;
#23049 = CARTESIAN_POINT ( 'NONE',  ( -20.71343476517554905, 1522.382868172863937, 179.9059455038197086 ) ) ;
#23050 = CARTESIAN_POINT ( 'NONE',  ( 0.1984587786619999850, 1451.686688576329971, 183.0460370019980019 ) ) ;
#23051 = CARTESIAN_POINT ( 'NONE',  ( -21.12444512610820269, 1508.254181376620181, 209.6686171012820239 ) ) ;
#23052 = CARTESIAN_POINT ( 'NONE',  ( -2.500000000000000000, 1439.495310554470052, 163.5954663552189743 ) ) ;
#23053 = CIRCLE ( 'NONE', #107153, 2.000000000000002220 ) ;
#23054 = CARTESIAN_POINT ( 'NONE',  ( 11.79480876540000089, 1441.728078750129953, 187.9005510439980071 ) ) ;
#23055 = CARTESIAN_POINT ( 'NONE',  ( 36.37832870499009630, 1451.642701156129988, 135.0591089792199853 ) ) ;
#23056 = CARTESIAN_POINT ( 'NONE',  ( -12.63439616088674633, 1483.510510869872178, 226.0832403630100771 ) ) ;
#23057 = CARTESIAN_POINT ( 'NONE',  ( 25.79236023700000047, 1440.625197361159962, 138.3752390835979895 ) ) ;
#23058 = CARTESIAN_POINT ( 'NONE',  ( 0.9908529825249998702, 1414.913060387329779, 192.1420427703979783 ) ) ;
#23059 = CARTESIAN_POINT ( 'NONE',  ( -72.68496013324840987, 1384.753871603139942, 271.2572098337690250 ) ) ;
#23060 = ORIENTED_EDGE ( 'NONE', *, *, #2427, .F. ) ;
#23061 = CARTESIAN_POINT ( 'NONE',  ( 6.941100277744999936, 1516.858069504249897, 202.1782432786469883 ) ) ;
#23062 = CARTESIAN_POINT ( 'NONE',  ( 4.612671339784999880, 1516.783665406140017, 208.3654117178780041 ) ) ;
#23063 = ORIENTED_EDGE ( 'NONE', *, *, #102982, .F. ) ;
#23064 = CARTESIAN_POINT ( 'NONE',  ( 33.71823238038290071, 1440.913060387330006, 258.8638944021930115 ) ) ;
#23065 = VECTOR ( 'NONE', #4705, 1000.000000000000227 ) ;
#23066 = CARTESIAN_POINT ( 'NONE',  ( -0.002575616544385699036, 1451.742099234649004, 154.0620397922272105 ) ) ;
#23067 = ORIENTED_EDGE ( 'NONE', *, *, #68464, .F. ) ;
#23068 = VECTOR ( 'NONE', #101011, 1000.000000000000114 ) ;
#23069 = DIRECTION ( 'NONE',  ( -0.01668530547203104716, 0.7071067811868645414, 0.7069098956591685079 ) ) ;
#23070 = EDGE_CURVE ( 'NONE', #35843, #98270, #47249, .T. ) ;
#23071 = CARTESIAN_POINT ( 'NONE',  ( -15.77403878809999860, 1409.463901959830082, 192.8704306968979836 ) ) ;
#23072 = DIRECTION ( 'NONE',  ( 0.000000000000000000, -1.000000000000000000, 0.000000000000000000 ) ) ;
#23073 = CARTESIAN_POINT ( 'NONE',  ( -9.456798816358269022, 1461.539703310480036, 206.9210100075549974 ) ) ;
#23074 = CARTESIAN_POINT ( 'NONE',  ( 21.30389884161289871, 1409.667087122100156, 206.3896467061680369 ) ) ;
#23075 = CARTESIAN_POINT ( 'NONE',  ( -5.835879630796829254, 1511.569910118449798, 200.8476638080379928 ) ) ;
#23076 = CARTESIAN_POINT ( 'NONE',  ( -0.7414587291309999717, 1508.588857168030017, 180.2948226304979755 ) ) ;
#23077 = CARTESIAN_POINT ( 'NONE',  ( -5.818054453628801248, 1510.580107419785463, 201.5859676881361224 ) ) ;
#23078 = CARTESIAN_POINT ( 'NONE',  ( -22.69876404239752077, 1522.861859112239017, 181.3483716558110359 ) ) ;
#23080 = CARTESIAN_POINT ( 'NONE',  ( 19.66678637246580053, 1522.051704408389924, 202.3500283489900085 ) ) ;
#23079 = CARTESIAN_POINT ( 'NONE',  ( 17.11189916109999842, 1459.589049907830031, 228.7027963470980012 ) ) ;
#23081 = B_SPLINE_CURVE_WITH_KNOTS ( 'NONE', 3,
 ( #22930, #80109, #80666, #29699, #39193, #72282 ),
 .UNSPECIFIED., .F., .F.,
 ( 4, 2, 4 ),
 ( 0.000000000000000000, 0.5000000000000000000, 1.000000000000000000 ),
 .UNSPECIFIED. ) ;
#23082 = CARTESIAN_POINT ( 'NONE',  ( 6.784288798619999561, 1469.672316088890057, 209.8806407344229967 ) ) ;
#23083 = CARTESIAN_POINT ( 'NONE',  ( -5.779627092215000594, 1516.977993847330026, 216.8424961055369806 ) ) ;
#23084 = ORIENTED_EDGE ( 'NONE', *, *, #86219, .F. ) ;
#23085 = AXIS2_PLACEMENT_3D ( 'NONE', #20184, #36441, #79029 ) ;
#23086 = PLANE ( 'NONE',  #46243 ) ;
#23087 = CARTESIAN_POINT ( 'NONE',  ( -0.07316533871274499834, 1508.573872468679838, 180.1735049589379969 ) ) ;
#23088 = EDGE_CURVE ( 'NONE', #75280, #5728, #102239, .T. ) ;
#23089 = CIRCLE ( 'NONE', #87551, 1.999999999999999556 ) ;
#23090 = CARTESIAN_POINT ( 'NONE',  ( 18.62528357307473925, 1445.660712737476615, 215.1045338314846731 ) ) ;
#23091 = CARTESIAN_POINT ( 'NONE',  ( 6.949265646015000186, 1517.089216728169959, 212.5747629931370000 ) ) ;
#23092 = CARTESIAN_POINT ( 'NONE',  ( 18.51591337770000223, 1509.559650329829765, 187.1458710574979989 ) ) ;
#23093 = LINE ( 'NONE', #90859, #65252 ) ;
#23095 = ORIENTED_EDGE ( 'NONE', *, *, #91922, .F. ) ;
#23094 = CARTESIAN_POINT ( 'NONE',  ( 4.487249361289610050, 1509.038630936360050, 212.6094330339349767 ) ) ;
#23096 = CARTESIAN_POINT ( 'NONE',  ( -19.08918019649999920, 1507.695924774130162, 229.6553491538980154 ) ) ;
#23097 = CARTESIAN_POINT ( 'NONE',  ( 21.86388809379999998, 1452.023132390130058, 221.6453359476980154 ) ) ;
#23098 = EDGE_CURVE ( 'NONE', #73262, #43039, #86684, .T. ) ;
#23099 = CARTESIAN_POINT ( 'NONE',  ( -11.84000682719999986, 1430.430028094429872, 150.0882633680979836 ) ) ;
#23100 = CARTESIAN_POINT ( 'NONE',  ( -15.73032604960000036, 1415.742867544160163, 209.5189867902049912 ) ) ;
#23101 = CARTESIAN_POINT ( 'NONE',  ( -109.9627613373179997, 1384.389859246369952, 311.4306166055309859 ) ) ;
#23102 = CARTESIAN_POINT ( 'NONE',  ( -8.770759252174429504E-15, 1422.771840662260047, 151.0941882234770048 ) ) ;
#23103 = CARTESIAN_POINT ( 'NONE',  ( 7.943378312860001067, 1421.399538177179920, 195.9193817166990073 ) ) ;
#23104 = CARTESIAN_POINT ( 'NONE',  ( -3.052469087571969997, 1446.532390927849974, 214.7242444357609941 ) ) ;
#23106 = CARTESIAN_POINT ( 'NONE',  ( -11.41675301695839906, 1482.775673471900063, 205.7339463974809917 ) ) ;
#23105 = CARTESIAN_POINT ( 'NONE',  ( -24.08096867289999565, 1444.797005272369915, 211.7711350123979912 ) ) ;
#23107 = CARTESIAN_POINT ( 'NONE',  ( -2.248581038649999808, 1485.570063529730078, 182.6114682650980114 ) ) ;
#23108 = AXIS2_PLACEMENT_3D ( 'NONE', #5458, #58631, #73787 ) ;
#23109 = ORIENTED_EDGE ( 'NONE', *, *, #35830, .F. ) ;
#23110 = CARTESIAN_POINT ( 'NONE',  ( 7.322105067625000352, 1516.572193931679976, 206.2485165713470110 ) ) ;
#23111 = CARTESIAN_POINT ( 'NONE',  ( 12.73684339809999955, 1407.027259281629995, 267.7855128373979596 ) ) ;
#23112 = CARTESIAN_POINT ( 'NONE',  ( 0.06622282237950000150, 1409.084365868529858, 185.5721059075980008 ) ) ;
#23113 = CARTESIAN_POINT ( 'NONE',  ( 10.95494146437559912, 1490.325474812490029, 209.5571900555880234 ) ) ;
#23114 = CARTESIAN_POINT ( 'NONE',  ( 24.51223204819740786, 1438.674460532969078, 212.6365892752995421 ) ) ;
#23115 = CARTESIAN_POINT ( 'NONE',  ( 12.54766037970713022, 1509.351234348180014, 182.3718845436952734 ) ) ;
#23116 = CARTESIAN_POINT ( 'NONE',  ( 28.25086641300000068, 1508.135711190629991, 209.3856964555159834 ) ) ;
#23117 = EDGE_CURVE ( 'NONE', #11259, #105162, #43855, .T. ) ;
#23118 = CARTESIAN_POINT ( 'NONE',  ( -10.31774485735029856, 1447.649174093579859, 209.9773725357489980 ) ) ;
#23119 = CARTESIAN_POINT ( 'NONE',  ( -1.976367997842130242, 1450.328871335550048, 155.3359410068990201 ) ) ;
#23120 = CARTESIAN_POINT ( 'NONE',  ( -1.555918367431536442, 1451.038150671306767, 183.6095956534302900 ) ) ;
#23121 = LINE ( 'NONE', #57325, #65884 ) ;
#23122 = CARTESIAN_POINT ( 'NONE',  ( -14.13162141313859976, 1415.651572961190141, 221.0577713143219967 ) ) ;
#23123 = CARTESIAN_POINT ( 'NONE',  ( -11.67169904650000056, 1501.458093402889972, 211.3450001610790139 ) ) ;
#23124 = CARTESIAN_POINT ( 'NONE',  ( -9.365681194936280818, 1409.240117181489950, 197.4562387521140181 ) ) ;
#23125 = B_SPLINE_SURFACE_WITH_KNOTS ( 'NONE', 5, 5, ( 
 ( #11788, #64963, #81183, #4499, #45956, #63328, #5596, #22357, #99076 ),
 ( #98537, #80093, #3412, #106399, #46515, #73909, #56005, #21805, #38090 ),
 ( #105861, #48161, #82297, #89589, #88504, #99625, #80649, #39746, #29140 ),
 ( #54373, #71744, #38633, #3963, #97983, #97448, #29684, #5034, #73353 ),
 ( #13412, #39178, #108037, #37542, #20715, #90685, #90129, #54911, #31332 ),
 ( #13973, #64416, #12325, #65518, #89037, #107489, #72265, #72809, #106939 ) ),
 .UNSPECIFIED., .F., .F., .F.,
 ( 6, 6 ),
 ( 6, 3, 6 ),
 ( 0.4666582265190000189, 2.797885342507290041 ),
 ( -1.082961728884700041E-05, 1.000000000000000000, 2.000000000000000000 ),
 .UNSPECIFIED. ) ;
#23126 = DIRECTION ( 'NONE',  ( -0.4090087482554316534, 0.000000000000000000, -0.9125304618753966590 ) ) ;
#23127 = CARTESIAN_POINT ( 'NONE',  ( 3.115557368589999765, 1441.255753523060093, 168.7233852534980088 ) ) ;
#23128 = CARTESIAN_POINT ( 'NONE',  ( -2.101430478369999744, 1475.725219423630051, 269.0439765300980639 ) ) ;
#23129 = CARTESIAN_POINT ( 'NONE',  ( -4.221309154770310101, 1446.219907474799811, 169.0688074703510040 ) ) ;
#23130 = CARTESIAN_POINT ( 'NONE',  ( -11.65724572759794064, 1512.939396361188756, 192.6905581653945774 ) ) ;
#23131 = DIRECTION ( 'NONE',  ( 0.06270903725022243524, -1.833354768615425389E-16, -0.9980318515193542517 ) ) ;
#23132 = CARTESIAN_POINT ( 'NONE',  ( -54.44353615944859826, 1384.719267686110015, 270.7278933346339613 ) ) ;
#23133 = CARTESIAN_POINT ( 'NONE',  ( -31.32995031131182628, 1523.678648413191695, 221.9013357025048947 ) ) ;
#23134 = AXIS2_PLACEMENT_3D ( 'NONE', #106417, #91266, #98001 ) ;
#23135 = CARTESIAN_POINT ( 'NONE',  ( -3.873571707704530187, 1517.051704409849890, 215.9268917042280123 ) ) ;
#23136 = B_SPLINE_SURFACE_WITH_KNOTS ( 'NONE', 5, 5, ( 
 ( #45453, #62826, #11823, #38664, #106972, #96382 ),
 ( #104780, #105893, #80681, #19660, #80125, #70666 ),
 ( #79595, #53864, #29174, #106431, #89618, #72300 ),
 ( #88539, #45993, #98014, #3444, #21285, #55493 ),
 ( #12909, #21835, #37017, #30259, #4530, #56033 ),
 ( #88003, #11286, #31364, #82328, #15099, #7273 ) ),
 .UNSPECIFIED., .F., .F., .F.,
 ( 6, 6 ),
 ( 6, 6 ),
 ( 30.99314794090000191, 41.27704706610000329 ),
 ( 0.000000000000000000, 0.5000000000000000000 ),
 .UNSPECIFIED. ) ;
#23137 = CARTESIAN_POINT ( 'NONE',  ( 12.13947661551040014, 1491.513716010349981, 207.1733083333600121 ) ) ;
#23138 = CARTESIAN_POINT ( 'NONE',  ( -20.07149347155869634, 1526.186458717540972, 185.1794229323607794 ) ) ;
#23139 = CARTESIAN_POINT ( 'NONE',  ( 7.948111852743331873, 1511.813436676051879, 205.9250125053374632 ) ) ;
#23140 = CARTESIAN_POINT ( 'NONE',  ( -19.61370360329999940, 1409.597986017130097, 199.4731069177680070 ) ) ;
#23141 = CARTESIAN_POINT ( 'NONE',  ( 12.90425579462769790, 1421.183432210740193, 204.7522736897579989 ) ) ;
#23142 = CIRCLE ( 'NONE', #48195, 0.9999999999999988898 ) ;
#23143 = CARTESIAN_POINT ( 'NONE',  ( -21.38516915558007270, 1522.382868172863937, 180.3939891059723664 ) ) ;
#23144 = ORIENTED_EDGE ( 'NONE', *, *, #55611, .T. ) ;
#23145 = B_SPLINE_SURFACE_WITH_KNOTS ( 'NONE', 5, 5, ( 
 ( #60840, #18234, #86555, #84350, #41253, #75426 ),
 ( #34502, #101681, #7640, #42348, #17107, #85435 ),
 ( #76503, #110652, #59718, #93837, #8733, #42916 ),
 ( #65100, #27758, #30372, #87112, #63474, #1465 ),
 ( #47738, #98680, #13007, #89733, #20864, #52980 ),
 ( #35600, #46661, #69793, #22491, #4100, #97592 ) ),
 .UNSPECIFIED., .F., .F., .F.,
 ( 6, 6 ),
 ( 6, 6 ),
 ( 23.15748662889999920, 93.48651207330000545 ),
 ( -1.387778780779999841E-17, 1.000000000000000000 ),
 .UNSPECIFIED. ) ;
#23146 = DIRECTION ( 'NONE',  ( 0.9528104219824277132, 0.2959442204286599210, -0.06759673184807767077 ) ) ;
#23147 = DIRECTION ( 'NONE',  ( 0.000000000000000000, 0.000000000000000000, 1.000000000000000000 ) ) ;
#23148 = CARTESIAN_POINT ( 'NONE',  ( 0.9103524645702290030, 1462.760075378919964, 230.5111400575189862 ) ) ;
#23150 = CARTESIAN_POINT ( 'NONE',  ( -12.42270385469250016, 1378.931396367140223, 211.1644544291300178 ) ) ;
#23149 = CARTESIAN_POINT ( 'NONE',  ( 11.05149221029999929, 1425.226139737630092, 137.4273676322979725 ) ) ;
#23151 = B_SPLINE_CURVE_WITH_KNOTS ( 'NONE', 5,
 ( #37701, #106019, #63490, #18122, #5758, #90288, #89203, #21959, #46678, #6295, #13022, #81335, #38241, #73523, #56152, #40442, #64580, #97610, #21416, #89750, #55627, #4116, #12496, #91411, #31486, #80810, #72423, #47209, #106554, #65118, #39899, #4649, #29842 ),
 .UNSPECIFIED., .F., .F.,
 ( 6, 3, 3, 3, 3, 3, 3, 3, 3, 3, 6 ),
 ( 0.000000000000000000, 0.007518056952438774941, 0.01525203516534743772, 0.03845860237258517250, 0.06166516957982287606, 0.1235369933248144647, 0.2623877845595162794, 0.4012385757933799035, 0.5405419652431506794, 0.8197911058882223490, 1.000000000000000000 ),
 .UNSPECIFIED. ) ;
#23152 = CARTESIAN_POINT ( 'NONE',  ( 17.19754479272649661, 1524.059663615500085, 237.3738432385773365 ) ) ;
#23153 = CONICAL_SURFACE ( 'NONE', #14204, 0.9999999999999857891, 0.7853981633970000820 ) ;
#23154 = CARTESIAN_POINT ( 'NONE',  ( -14.35646903299999799, 1420.584115152450067, 213.7701001417389932 ) ) ;
#23155 = CARTESIAN_POINT ( 'NONE',  ( -4.732406976500000084, 1453.644983325290013, 200.2083546425689917 ) ) ;
#23156 = CARTESIAN_POINT ( 'NONE',  ( 5.777745395274999751, 1516.908489800550115, 202.5639360494670029 ) ) ;
#23157 = CARTESIAN_POINT ( 'NONE',  ( 8.309621275030000476, 1427.613389394789920, 212.3081093229889973 ) ) ;
#23158 = CARTESIAN_POINT ( 'NONE',  ( -12.63312964746819667, 1398.287568163796323, 212.1890067615559019 ) ) ;
#23159 = CARTESIAN_POINT ( 'NONE',  ( 15.64724539423500360, 1513.113451381389950, 194.8383152136670162 ) ) ;
#23160 = CARTESIAN_POINT ( 'NONE',  ( -17.74072797668249990, 1419.883333100649907, 204.5911605323600213 ) ) ;
#23161 = DIRECTION ( 'NONE',  ( -0.2054769195713296304, 0.000000000000000000, 0.9786619618251631847 ) ) ;
#23162 = VECTOR ( 'NONE', #70390, 1000.000000000000227 ) ;
#23163 = CARTESIAN_POINT ( 'NONE',  ( 20.20924716366269891, 1509.280845329529939, 229.6605187684139935 ) ) ;
#23164 = B_SPLINE_CURVE_WITH_KNOTS ( 'NONE', 3,
 ( #23133, #65171, #5247, #75226, #73580, #109378, #57338, #56765, #5814, #39953 ),
 .UNSPECIFIED., .F., .F.,
 ( 4, 2, 2, 2, 4 ),
 ( 0.000000000000000000, 0.0007403986298595417693, 0.001480797259719083539, 0.002221195889578625200, 0.002961594519438167077 ),
 .UNSPECIFIED. ) ;
#23166 = VERTEX_POINT ( 'NONE', #67565 ) ;
#23165 = CARTESIAN_POINT ( 'NONE',  ( -52.34085353736339385, 1379.705649852349779, 249.9538312876250075 ) ) ;
#23167 = ORIENTED_EDGE ( 'NONE', *, *, #107746, .T. ) ;
#23168 = CARTESIAN_POINT ( 'NONE',  ( -2.512417091500000144, 1396.184323656129891, 221.0598646773979965 ) ) ;
#23169 = CARTESIAN_POINT ( 'NONE',  ( -22.32010538089999940, 1411.050761390129992, 213.5142330314379819 ) ) ;
#23170 = EDGE_LOOP ( 'NONE', ( #4830, #35681, #56906, #101887, #71680 ) ) ;
#23171 = CARTESIAN_POINT ( 'NONE',  ( -13.43774386648357400, 1444.332129055663245, 169.3644175787693200 ) ) ;
#23172 = CARTESIAN_POINT ( 'NONE',  ( -0.2612772979118159755, 1416.851343897360039, 227.4677505453099968 ) ) ;
#23173 = CARTESIAN_POINT ( 'NONE',  ( -7.883543530645000352, 1512.115618635729788, 212.0728052921269864 ) ) ;
#23175 = CARTESIAN_POINT ( 'NONE',  ( -13.82025443706379875, 1508.597244210279996, 183.9953287070100032 ) ) ;
#23174 = CARTESIAN_POINT ( 'NONE',  ( 1.514255875599999968, 1444.175298751890068, 200.2744927717990038 ) ) ;
#23176 = CARTESIAN_POINT ( 'NONE',  ( 4.597825173950000455, 1468.702107850830089, 183.5732306118979977 ) ) ;
#23177 = CARTESIAN_POINT ( 'NONE',  ( -3.841809705010690301, 1464.683280171979959, 198.7835890369999845 ) ) ;
#23178 = CARTESIAN_POINT ( 'NONE',  ( -1.971951421069999988, 1423.054295909000075, 191.2999637764989984 ) ) ;
#23179 = FILL_AREA_STYLE_COLOUR ( '', #37813 ) ;
#23180 = CARTESIAN_POINT ( 'NONE',  ( 11.01747428149709940, 1396.297799067110191, 208.0502089956040095 ) ) ;
#23181 = CARTESIAN_POINT ( 'NONE',  ( 1.270728274670000157, 1414.996444518330009, 191.7853923519979844 ) ) ;
#23182 = CARTESIAN_POINT ( 'NONE',  ( 11.48551835569999824, 1426.311945552029783, 147.9218383413980007 ) ) ;
#23183 = CARTESIAN_POINT ( 'NONE',  ( 8.140171433879366703, 1509.197613402637671, 180.9403984144503852 ) ) ;
#23184 = ORIENTED_EDGE ( 'NONE', *, *, #41579, .T. ) ;
#23185 = CARTESIAN_POINT ( 'NONE',  ( 12.92162038170519978, 1434.739176993439969, 149.3060585083890146 ) ) ;
#23186 = DIRECTION ( 'NONE',  ( 1.000000000000000000, 0.000000000000000000, 0.000000000000000000 ) ) ;
#23187 = VERTEX_POINT ( 'NONE', #33930 ) ;
#23188 = ORIENTED_EDGE ( 'NONE', *, *, #15349, .T. ) ;
#23189 = CARTESIAN_POINT ( 'NONE',  ( -18.13595047818949979, 1468.171444148069895, 228.4032209057770046 ) ) ;
#23190 = CARTESIAN_POINT ( 'NONE',  ( -12.70631653080000056, 1462.828418259130103, 230.7343418143979932 ) ) ;
#23191 = AXIS2_PLACEMENT_3D ( 'NONE', #76319, #109921, #110468 ) ;
#23192 = CARTESIAN_POINT ( 'NONE',  ( -107.8944167935766956, 1389.215957491298241, 309.8698152422039698 ) ) ;
#23193 = CARTESIAN_POINT ( 'NONE',  ( 7.331183090945000203, 1516.882217593000178, 216.0635732225570109 ) ) ;
#23194 = CARTESIAN_POINT ( 'NONE',  ( -12.34597593048379949, 1378.750903717820165, 209.0838442145889928 ) ) ;
#23195 = ORIENTED_EDGE ( 'NONE', *, *, #87035, .F. ) ;
#23196 = CARTESIAN_POINT ( 'NONE',  ( -11.71166783339999995, 1503.433515124489986, 208.0502066329989930 ) ) ;
#23197 = CARTESIAN_POINT ( 'NONE',  ( 2.500000000000000000, 1448.208035806090038, 170.3313966091639884 ) ) ;
#23198 = CARTESIAN_POINT ( 'NONE',  ( -50.14839348009999753, 1375.010081756269983, 242.5009839091590038 ) ) ;
#23199 = ORIENTED_EDGE ( 'NONE', *, *, #96638, .T. ) ;
#23200 = CARTESIAN_POINT ( 'NONE',  ( 0.7356989345870019736, 1517.020847257979995, 205.6609797614169963 ) ) ;
#23202 = EDGE_LOOP ( 'NONE', ( #61462, #109854, #77358, #36985 ) ) ;
#23201 = B_SPLINE_CURVE_WITH_KNOTS ( 'NONE', 3,
 ( #4348, #38477, #61505, #18903, #55865, #31178, #14917, #23324, #47449, #56401, #32291, #40134, #74318, #14366, #90533, #100583, #73764, #108448, #31728, #99473, #57517, #107341, #81573 ),
 .UNSPECIFIED., .F., .F.,
 ( 4, 2, 1, 2, 2, 2, 2, 2, 2, 2, 2, 4 ),
 ( 0.000000000000000000, 0.1249999999991294464, 0.1874999999988291033, 0.2187499999987238541, 0.2499999999986186050, 0.3749999999983899546, 0.4374999999980648258, 0.4999999999977396969, 0.6249999999977112752, 0.6874999999976637577, 0.7499999999976162401, 1.000000000000000000 ),
 .UNSPECIFIED. ) ;
#23203 = CARTESIAN_POINT ( 'NONE',  ( 2.873919002525000099, 1516.940252185109784, 209.1085733957019954 ) ) ;
#23204 = VECTOR ( 'NONE', #86362, 1000.000000000000114 ) ;
#23205 = CARTESIAN_POINT ( 'NONE',  ( -7.305485514955160298, 1453.383523734929895, 203.2828978378740032 ) ) ;
#23206 = CARTESIAN_POINT ( 'NONE',  ( -38.91479787275512336, 1429.388299853867238, 269.5915017202312924 ) ) ;
#23207 = CARTESIAN_POINT ( 'NONE',  ( -1.616567575689999980, 1409.474956838429989, 232.6959444083979918 ) ) ;
#23209 = ORIENTED_EDGE ( 'NONE', *, *, #107894, .F. ) ;
#23208 = CARTESIAN_POINT ( 'NONE',  ( -1.239262138312009931, 1414.972329067380088, 226.4897656787760241 ) ) ;
#23210 = CARTESIAN_POINT ( 'NONE',  ( 2.500000000000000000, 1419.382893006970107, 144.1042006977590120 ) ) ;
#23211 = CARTESIAN_POINT ( 'NONE',  ( -34.13585384247240029, 1440.913060389490056, 249.1457226945469756 ) ) ;
#23212 = CARTESIAN_POINT ( 'NONE',  ( -73.68066259569999943, 1383.781794063629832, 298.8244620241590042 ) ) ;
#23213 = CARTESIAN_POINT ( 'NONE',  ( -0.3157405184142340060, 1466.373614858310248, 235.6705076282450193 ) ) ;
#23214 = CARTESIAN_POINT ( 'NONE',  ( 5.035691840050000145, 1407.858053359329915, 270.1320510971980298 ) ) ;
#23215 = CARTESIAN_POINT ( 'NONE',  ( -1.704794841465000044, 1517.096587378560116, 213.7484378375869767 ) ) ;
#23216 = CARTESIAN_POINT ( 'NONE',  ( 23.66166531129999839, 1410.128854677129993, 208.6849955005649804 ) ) ;
#23217 = CARTESIAN_POINT ( 'NONE',  ( -20.15293516530000062, 1508.383239031330049, 189.0805060732980110 ) ) ;
#23218 = CARTESIAN_POINT ( 'NONE',  ( 2.713660715419999647, 1441.511099666689915, 218.6663635638090000 ) ) ;
#23219 = CARTESIAN_POINT ( 'NONE',  ( -7.712247387419390421, 1516.657104395800161, 210.1350615241800028 ) ) ;
#23220 = CARTESIAN_POINT ( 'NONE',  ( -7.323390445344999833, 1516.613712827999962, 210.2512321725070024 ) ) ;
#23221 = CARTESIAN_POINT ( 'NONE',  ( 9.602386435385879437, 1434.766419721330067, 207.2149381967969930 ) ) ;
#23222 = CARTESIAN_POINT ( 'NONE',  ( 0.2576834098190000089, 1419.224531700530179, 184.6439150135979901 ) ) ;
#23223 =( BOUNDED_CURVE ( )  B_SPLINE_CURVE ( 3, ( #89768, #97085, #37173, #47227 ),
 .UNSPECIFIED., .F., .F. ) 
 B_SPLINE_CURVE_WITH_KNOTS ( ( 4, 4 ),
 ( 4.148492618474420190, 5.276285279552140217 ),
 .UNSPECIFIED. ) 
 CURVE ( )  GEOMETRIC_REPRESENTATION_ITEM ( )  RATIONAL_B_SPLINE_CURVE ( ( 1.000000000000000000, 0.8967860053317929792, 0.8967860053317929792, 1.000000000000000000 ) ) 
 REPRESENTATION_ITEM ( '' )  );
#23224 = CARTESIAN_POINT ( 'NONE',  ( 0.6369828065621148117, 1408.970539270458858, 231.8715245986919058 ) ) ;
#23226 = ORIENTED_EDGE ( 'NONE', *, *, #41906, .T. ) ;
#23225 = CARTESIAN_POINT ( 'NONE',  ( -19.25455816879999915, 1386.939098950560037, 220.3202894305590007 ) ) ;
#23227 = CARTESIAN_POINT ( 'NONE',  ( -44.39234662709849744, 1385.156173160149820, 250.3178217652419733 ) ) ;
#23228 = AXIS2_PLACEMENT_3D ( 'NONE', #105018, #59851, #93975 ) ;
#23229 = CARTESIAN_POINT ( 'NONE',  ( 39.02588949829999621, 1459.481874369829939, 266.4772423242980040 ) ) ;
#23230 = DIRECTION ( 'NONE',  ( 0.000000000000000000, 1.000000000000000000, 0.000000000000000000 ) ) ;
#23231 = PRODUCT_DEFINITION_SHAPE ( 'NONE', 'NONE',  #110838 ) ;
#23232 = CARTESIAN_POINT ( 'NONE',  ( -8.768113839085080130, 1509.161991642730072, 236.4477861136639945 ) ) ;
#23233 = AXIS2_PLACEMENT_3D ( 'NONE', #93428, #512, #78294 ) ;
#23234 = CARTESIAN_POINT ( 'NONE',  ( -113.4000000000000057, 1305.913060387289988, 304.2218459572590064 ) ) ;
#23235 = CARTESIAN_POINT ( 'NONE',  ( 12.08449222550000002, 1421.674727768539924, 206.2100432727989983 ) ) ;
#23236 = CARTESIAN_POINT ( 'NONE',  ( 0.3740406207303079711, 1452.976564550639978, 183.2744760995269928 ) ) ;
#23238 = CARTESIAN_POINT ( 'NONE',  ( -8.297571581699999754, 1384.891077973469919, 218.7035731870690256 ) ) ;
#23237 = CARTESIAN_POINT ( 'NONE',  ( 7.717505752974999744, 1516.857914730730045, 216.8393517232070167 ) ) ;
#23239 = DIRECTION ( 'NONE',  ( 0.000000000000000000, 0.000000000000000000, 1.000000000000000000 ) ) ;
#23240 = CARTESIAN_POINT ( 'NONE',  ( 0.6209246841665734262, 1515.589587247402505, 205.1019389779893913 ) ) ;
#23241 = ORIENTED_EDGE ( 'NONE', *, *, #2245, .T. ) ;
#23242 = CARTESIAN_POINT ( 'NONE',  ( 2.290256263724999908, 1517.170721208160103, 202.1706708033170230 ) ) ;
#23243 = CARTESIAN_POINT ( 'NONE',  ( -16.00554747716499904, 1513.636261293280086, 223.8634274198670084 ) ) ;
#23244 = AXIS2_PLACEMENT_3D ( 'NONE', #11623, #104015, #87223 ) ;
#23245 = CARTESIAN_POINT ( 'NONE',  ( 0.3765640108789999885, 1477.420202996130001, 229.8311010043980218 ) ) ;
#23246 = CARTESIAN_POINT ( 'NONE',  ( 20.06336068849999776, 1456.114497556030074, 223.5835209092980165 ) ) ;
#23247 = CARTESIAN_POINT ( 'NONE',  ( 10.94084016961279993, 1461.364874240460040, 209.8155579094599830 ) ) ;
#23248 = CARTESIAN_POINT ( 'NONE',  ( 9.319248534172345444, 1425.257639114323183, 195.5897260868380272 ) ) ;
#23249 = CARTESIAN_POINT ( 'NONE',  ( -0.6891144619180010755, 1443.914159960489997, 218.1634325674289698 ) ) ;
#23250 = CARTESIAN_POINT ( 'NONE',  ( 15.20036750253001756, 1420.718811329341179, 227.8626738659623356 ) ) ;
#23251 = CARTESIAN_POINT ( 'NONE',  ( 38.78625493179519879, 1448.012161950920017, 136.4925098791590017 ) ) ;
#23252 = CARTESIAN_POINT ( 'NONE',  ( -20.33636649369999816, 1427.581624735430069, 223.9337651306980206 ) ) ;
#23253 = CARTESIAN_POINT ( 'NONE',  ( -13.58058603182956148, 1473.584022274761764, 269.5920743625052864 ) ) ;
#23254 = CARTESIAN_POINT ( 'NONE',  ( -108.0517768189999970, 1387.143456978330050, 297.7515165377590165 ) ) ;
#23255 = DIRECTION ( 'NONE',  ( -6.123233995736769734E-17, -1.000000000000000000, -1.124819836996399911E-32 ) ) ;
#23256 = CARTESIAN_POINT ( 'NONE',  ( -106.6767654209999847, 1391.553749469950162, 300.4545537148590029 ) ) ;
#23257 = CARTESIAN_POINT ( 'NONE',  ( -25.36238703422979412, 1465.239872904934600, 269.4273574237397497 ) ) ;
#23258 = VERTEX_POINT ( 'NONE', #41242 ) ;
#23259 = CARTESIAN_POINT ( 'NONE',  ( -24.61293950550089704, 1444.770188684140066, 210.8869336946189890 ) ) ;
#23260 = CARTESIAN_POINT ( 'NONE',  ( -3.909710721586109550, 1517.151704408390060, 197.7672215555029993 ) ) ;
#23261 = EDGE_CURVE ( 'NONE', #41661, #106368, #45097, .T. ) ;
#23262 = CARTESIAN_POINT ( 'NONE',  ( -17.37723644544100310, 1525.394081235439444, 237.0493492034528913 ) ) ;
#23263 = CARTESIAN_POINT ( 'NONE',  ( -12.86224528119999988, 1519.913060387329779, 228.0025448475979886 ) ) ;
#23264 = CIRCLE ( 'NONE', #85869, 7.500000000000000000 ) ;
#23265 = DIRECTION ( 'NONE',  ( -5.980589973904019347E-17, 1.000000000000000000, -1.736889445713099699E-16 ) ) ;
#23266 = CARTESIAN_POINT ( 'NONE',  ( -12.53380580351000084, 1442.773887400870080, 185.9733686700720057 ) ) ;
#23267 = B_SPLINE_SURFACE_WITH_KNOTS ( 'NONE', 5, 5, ( 
 ( #39047, #4909, #3846, #55339, #12767, #89471, #72155, #21687, #106273 ),
 ( #90012, #108477, #64851, #22784, #98961, #29559, #37973, #13289, #72687 ),
 ( #47481, #55894, #21132, #56432, #46945, #90563, #82724, #81604, #38508 ),
 ( #65396, #81064, #39624, #48027, #73792, #99501, #56989, #91120, #14396 ),
 ( #6014, #31760, #65946, #50773, #16578, #24447, #49139, #109583, #6569 ),
 ( #58088, #85453, #7661, #83272, #110126, #110671, #41818, #8751, #92768 ) ),
 .UNSPECIFIED., .F., .F., .F.,
 ( 6, 6 ),
 ( 6, 3, 6 ),
 ( 39.88384216566930007, 42.45432491120000407 ),
 ( 0.000000000000000000, 8.028376878260001348, 16.05675375649999737 ),
 .UNSPECIFIED. ) ;
#23268 = CARTESIAN_POINT ( 'NONE',  ( -9.518234561902950475, 1438.815826527629952, 209.5578901295930052 ) ) ;
#23269 = CARTESIAN_POINT ( 'NONE',  ( 16.55108609117709406, 1524.760046179776054, 180.7894123379967368 ) ) ;
#23270 = CARTESIAN_POINT ( 'NONE',  ( -3.091188561554334413, 1415.773449501390360, 232.7382472471307153 ) ) ;
#23271 = CARTESIAN_POINT ( 'NONE',  ( -14.37435889315949922, 1415.677402204050168, 205.0862553119529821 ) ) ;
#23272 = CARTESIAN_POINT ( 'NONE',  ( 25.03845205760000070, 1436.443508297579911, 137.7838405999980012 ) ) ;
#23273 = CARTESIAN_POINT ( 'NONE',  ( 2.234923043937409926, 1512.341036938790012, 216.7210731156089878 ) ) ;
#23275 = ORIENTED_EDGE ( 'NONE', *, *, #63978, .T. ) ;
#23274 = CARTESIAN_POINT ( 'NONE',  ( -13.98887540559999998, 1409.902971829729950, 226.7724385780979901 ) ) ;
#23276 = AXIS2_PLACEMENT_3D ( 'NONE', #63292, #104158, #97407 ) ;
#23277 = CARTESIAN_POINT ( 'NONE',  ( 1.190628175363690033, 1414.913057834419988, 192.2393642087460250 ) ) ;
#23278 = DIRECTION ( 'NONE',  ( -1.000000000000000000, 0.000000000000000000, 0.000000000000000000 ) ) ;
#23279 = VERTEX_POINT ( 'NONE', #94378 ) ;
#23280 = VERTEX_POINT ( 'NONE', #93821 ) ;
#23281 = CARTESIAN_POINT ( 'NONE',  ( -11.92170027740000116, 1502.281711308889953, 208.9298100184969940 ) ) ;
#23282 = CARTESIAN_POINT ( 'NONE',  ( 6.212573846741591410, 1516.720895353221294, 204.9194608389200596 ) ) ;
#23284 = CARTESIAN_POINT ( 'NONE',  ( 7.760422419640001065E-08, 1460.308496262029848, 216.2848421383880009 ) ) ;
#23283 = CARTESIAN_POINT ( 'NONE',  ( 2.629563630540000307, 1456.337126530590012, 219.4237753482989888 ) ) ;
#23285 = CARTESIAN_POINT ( 'NONE',  ( -2.274880353649999964, 1445.428165552290011, 217.8632208591889992 ) ) ;
#23286 = CARTESIAN_POINT ( 'NONE',  ( -11.89091680820000008, 1433.344382350330079, 150.2411281519979980 ) ) ;
#23287 = DIRECTION ( 'NONE',  ( -0.9455185755993178454, 0.000000000000000000, 0.3255681544571537578 ) ) ;
#23288 = DIRECTION ( 'NONE',  ( 0.0002664982727862750633, -9.558500756205390916E-06, 0.9999999644436521340 ) ) ;
#23289 = CARTESIAN_POINT ( 'NONE',  ( -27.07124288249999822, 1440.503322045070036, 137.2138250103980113 ) ) ;
#23290 = CARTESIAN_POINT ( 'NONE',  ( -24.34163166689999969, 1440.051000972679958, 211.6712235465880099 ) ) ;
#23291 = FACE_BOUND ( 'NONE', #68585, .T. ) ;
#23292 = CARTESIAN_POINT ( 'NONE',  ( 1.603799458759999963, 1450.610278152239971, 181.7139904433980178 ) ) ;
#23293 = CARTESIAN_POINT ( 'NONE',  ( 9.663424421720160140, 1363.752474719036172, 210.6218459616987957 ) ) ;
#23294 = CARTESIAN_POINT ( 'NONE',  ( -9.587247150298686904, 1509.374143047329653, 237.5563645247161162 ) ) ;
#23296 = ORIENTED_EDGE ( 'NONE', *, *, #15225, .T. ) ;
#23295 = CARTESIAN_POINT ( 'NONE',  ( -2.670047520287639767E-10, 1412.356500757170124, 252.5818293650800115 ) ) ;
#23297 = ORIENTED_EDGE ( 'NONE', *, *, #69962, .T. ) ;
#23298 = CARTESIAN_POINT ( 'NONE',  ( -11.85007381715819896, 1431.224519208780066, 149.8691846786930171 ) ) ;
#23299 = EDGE_CURVE ( 'NONE', #42516, #31391, #85109, .T. ) ;
#23300 = EDGE_CURVE ( 'NONE', #97433, #18368, #100978, .T. ) ;
#23301 = CARTESIAN_POINT ( 'NONE',  ( -13.76731767608630008, 1503.460756753999931, 227.5714742811019846 ) ) ;
#23302 = CARTESIAN_POINT ( 'NONE',  ( -3.511242807609999961, 1473.164181487230053, 270.4277067457979911 ) ) ;
#23303 = CARTESIAN_POINT ( 'NONE',  ( -0.1116522590836569045, 1473.547763220521347, 219.3528841741646147 ) ) ;
#23304 = CARTESIAN_POINT ( 'NONE',  ( -125.3156758022999213, 1368.558218059088631, 301.1792744052535227 ) ) ;
#23305 = EDGE_CURVE ( 'NONE', #33810, #76110, #86513, .T. ) ;
#23306 = CARTESIAN_POINT ( 'NONE',  ( 37.14918443920200275, 1450.989562377319999, 134.7272541307739857 ) ) ;
#23308 = EDGE_CURVE ( 'NONE', #714, #42229, #21045, .T. ) ;
#23307 = CARTESIAN_POINT ( 'NONE',  ( 1.590879946458802596, 1526.333389947941896, 239.8456008596616016 ) ) ;
#23309 = CARTESIAN_POINT ( 'NONE',  ( -7.291808457750000194, 1480.410216369889895, 208.6747883837709878 ) ) ;
#23310 = ADVANCED_FACE ( 'NONE', ( #31045 ), #89855, .F. ) ;
#23311 = CARTESIAN_POINT ( 'NONE',  ( -2.472529913803023227, 1523.678648413191695, 175.3762130535718597 ) ) ;
#23312 = CARTESIAN_POINT ( 'NONE',  ( -3.776018960370000066, 1457.468576287289807, 218.0147105414490056 ) ) ;
#23313 = CARTESIAN_POINT ( 'NONE',  ( 12.04322937582876030, 1364.845882714125537, 209.6218459617033432 ) ) ;
#23314 = CARTESIAN_POINT ( 'NONE',  ( -29.06316727068120187, 1413.561815854209954, 267.1797966645490305 ) ) ;
#23315 = VECTOR ( 'NONE', #51822, 1000.000000000000000 ) ;
#23316 = VERTEX_POINT ( 'NONE', #38341 ) ;
#23317 = CARTESIAN_POINT ( 'NONE',  ( -4.327403558811090178, 1515.142896577510101, 209.6457263099750037 ) ) ;
#23318 = VERTEX_POINT ( 'NONE', #29940 ) ;
#23319 = EDGE_LOOP ( 'NONE', ( #65509, #47990, #37406, #19827, #7307, #104488, #66747 ) ) ;
#23320 = CARTESIAN_POINT ( 'NONE',  ( -4.026777524084999449, 1516.718889242609976, 211.4189316860469887 ) ) ;
#23321 = CARTESIAN_POINT ( 'NONE',  ( 16.90742456144258909, 1444.994950788469623, 162.4348202098878744 ) ) ;
#23322 = CARTESIAN_POINT ( 'NONE',  ( 41.54209482800269626, 1444.082802428220020, 136.2297247852750104 ) ) ;
#23324 = CARTESIAN_POINT ( 'NONE',  ( -17.62619653710081025, 1419.739949534606012, 206.8872665010755156 ) ) ;
#23323 = CARTESIAN_POINT ( 'NONE',  ( -7.322709724964999722, 1516.596789218710001, 212.3828531017969965 ) ) ;
#23325 = CARTESIAN_POINT ( 'NONE',  ( -18.01785038329999722, 1455.457996638230043, 190.4178173900980084 ) ) ;
#23326 = AXIS2_PLACEMENT_3D ( 'NONE', #55307, #88889, #80499 ) ;
#23327 = CARTESIAN_POINT ( 'NONE',  ( -11.60004869885203682, 1428.983126981193436, 136.0999999980979851 ) ) ;
#23328 = VERTEX_POINT ( 'NONE', #22613 ) ;
#23329 = CARTESIAN_POINT ( 'NONE',  ( -26.53940720459999980, 1435.424242704579910, 135.2833523932980029 ) ) ;
#23330 = ADVANCED_FACE ( 'NONE', ( #64131 ), #90269, .T. ) ;
#23331 = CARTESIAN_POINT ( 'NONE',  ( 7.328049280255000575, 1516.809497469189864, 202.5664528150769854 ) ) ;
#23332 = CARTESIAN_POINT ( 'NONE',  ( 1.582067810090000045E-15, 1406.443991414029824, 137.0999999980979851 ) ) ;
#23333 = ADVANCED_FACE ( 'NONE', ( #107209 ), #32277, .F. ) ;
#23334 = CARTESIAN_POINT ( 'NONE',  ( -19.84796779067900019, 1384.533059183989963, 201.6437377799259991 ) ) ;
#23335 = CARTESIAN_POINT ( 'NONE',  ( -40.98920041333110476, 1431.365838692129955, 269.8604638295950053 ) ) ;
#23336 = CARTESIAN_POINT ( 'NONE',  ( -17.54330095577449811, 1486.685527788949912, 197.8065059920220108 ) ) ;
#23337 = CARTESIAN_POINT ( 'NONE',  ( -2.562000323739999974, 1397.677063979329887, 196.2741722088979941 ) ) ;
#23339 = EDGE_LOOP ( 'NONE', ( #23144, #109972, #18879, #103793, #46908 ) ) ;
#23338 = CARTESIAN_POINT ( 'NONE',  ( 30.98826378581297192, 1524.599984580802357, 196.4397214278006345 ) ) ;
#23340 = EDGE_LOOP ( 'NONE', ( #105664, #72273, #87727, #5944 ) ) ;
#23342 = EDGE_CURVE ( 'NONE', #45774, #31602, #53394, .T. ) ;
#23341 = CARTESIAN_POINT ( 'NONE',  ( -11.86703214218580094, 1432.405005609789896, 149.9822914483479792 ) ) ;
#23343 = CARTESIAN_POINT ( 'NONE',  ( 32.12914650970602537, 1465.185426907999272, 269.3130570102625825 ) ) ;
#23344 = CARTESIAN_POINT ( 'NONE',  ( -0.007179413344095889743, 1425.548651214390020, 191.0976962420139955 ) ) ;
#23345 = CARTESIAN_POINT ( 'NONE',  ( -12.93021894928120119, 1435.974380371249936, 150.7740590697349887 ) ) ;
#23346 = AXIS2_PLACEMENT_3D ( 'NONE', #12510, #79731, #54547 ) ;
#23347 = CYLINDRICAL_SURFACE ( 'NONE', #77628, 1.000000000000000444 ) ;
#23348 = CARTESIAN_POINT ( 'NONE',  ( -1.700706814495000163, 1516.923170579120097, 211.4225755968969906 ) ) ;
#23349 = CARTESIAN_POINT ( 'NONE',  ( 7.369559949379922870, 1460.670680854289913, 202.8482577992020310 ) ) ;
#23350 = CARTESIAN_POINT ( 'NONE',  ( -0.2055871234762860489, 1452.986193708736664, 183.2455700960801437 ) ) ;
#23351 = CARTESIAN_POINT ( 'NONE',  ( -14.10900654350000138, 1426.825383623629932, 222.2175365666979872 ) ) ;
#23352 = CARTESIAN_POINT ( 'NONE',  ( -13.20846944190000016, 1414.988015876829877, 220.4537675707979929 ) ) ;
#23353 = CARTESIAN_POINT ( 'NONE',  ( 11.74267910810000082, 1446.506701529569909, 187.7371912896979893 ) ) ;
#23354 = CARTESIAN_POINT ( 'NONE',  ( -1.718203501584999904, 1516.898441858519845, 207.4215862561470090 ) ) ;
#23355 = ORIENTED_EDGE ( 'NONE', *, *, #3499, .T. ) ;
#23356 = DIRECTION ( 'NONE',  ( -0.4794255385927466140, -4.329869795923643736E-12, -0.8775825618966315300 ) ) ;
#23357 = CARTESIAN_POINT ( 'NONE',  ( -11.58689981238089928, 1425.690685868059973, 133.5556927527120195 ) ) ;
#23358 = CARTESIAN_POINT ( 'NONE',  ( -20.92280442586893230, 1454.947889300366114, 223.3949133203993540 ) ) ;
#23359 = VERTEX_POINT ( 'NONE', #103780 ) ;
#23361 = VECTOR ( 'NONE', #108641, 1000.000000000000000 ) ;
#23360 = CARTESIAN_POINT ( 'NONE',  ( -28.81652261710059548, 1526.349684470114653, 198.1982547273859154 ) ) ;
#23362 = CARTESIAN_POINT ( 'NONE',  ( -25.17103052259800933, 1509.792535868356936, 224.3142502091264134 ) ) ;
#23363 = CARTESIAN_POINT ( 'NONE',  ( -4.155669664704369382, 1439.704322410719897, 185.4969487652249995 ) ) ;
#23364 = DIRECTION ( 'NONE',  ( -1.000000000000000000, 0.000000000000000000, 0.000000000000000000 ) ) ;
#23365 = CARTESIAN_POINT ( 'NONE',  ( 11.81780673814840021, 1517.051704408389924, 195.5270144474869767 ) ) ;
#23366 = CARTESIAN_POINT ( 'NONE',  ( 3.169329433935653029, 1451.405488132423443, 183.9445329269590559 ) ) ;
#23367 = CARTESIAN_POINT ( 'NONE',  ( 7.003830488220000206, 1486.892509085090069, 200.8568873985890093 ) ) ;
#23368 = CARTESIAN_POINT ( 'NONE',  ( -4.724155950714410857, 1476.228105402329902, 199.9129071112880069 ) ) ;
#23369 = CARTESIAN_POINT ( 'NONE',  ( 4.261545393745459265, 1441.227666458910107, 159.2966476699340035 ) ) ;
#23370 = CARTESIAN_POINT ( 'NONE',  ( -11.94046459599999999, 1438.194204504490017, 147.6340003373980210 ) ) ;
#23371 = CARTESIAN_POINT ( 'NONE',  ( 35.28305654171062855, 1451.608437209524254, 134.6904889284648732 ) ) ;
#23372 = CARTESIAN_POINT ( 'NONE',  ( -6.553524415734999664, 1516.882690742909972, 216.0660777183969969 ) ) ;
#23373 = EDGE_LOOP ( 'NONE', ( #35191, #20300 ) ) ;
#23374 = CARTESIAN_POINT ( 'NONE',  ( 7.709409411809799550, 1516.548727935889929, 207.4433096617889873 ) ) ;
#23375 = CARTESIAN_POINT ( 'NONE',  ( -5.035691841070000230, 1473.968067415529958, 270.1320510969979978 ) ) ;
#23376 = CARTESIAN_POINT ( 'NONE',  ( -17.90910890133720201, 1508.551704408389924, 211.2475455717739976 ) ) ;
#23377 = CARTESIAN_POINT ( 'NONE',  ( -9.061761650477359709, 1423.804865071479753, 133.5339198589369971 ) ) ;
#23378 = CARTESIAN_POINT ( 'NONE',  ( -3.441085532370000255, 1476.342819318190095, 219.6507254485989904 ) ) ;
#23379 = CARTESIAN_POINT ( 'NONE',  ( -7.545163887449800377, 1384.911772596620040, 219.0875992466739888 ) ) ;
#23380 = DIRECTION ( 'NONE',  ( 0.000000000000000000, 1.000000000000000000, 0.000000000000000000 ) ) ;
#23381 = CARTESIAN_POINT ( 'NONE',  ( -3.676556857354845942, 1508.129772564241193, 220.7334657978175017 ) ) ;
#23382 = CIRCLE ( 'NONE', #34100, 1.000000000000000888 ) ;
#23383 = CARTESIAN_POINT ( 'NONE',  ( 0.000000000000000000, 1526.382868172863937, 238.6369021217711577 ) ) ;
#23384 = CARTESIAN_POINT ( 'NONE',  ( 1.480207909756110052, 1456.259238296559943, 198.6472058902120068 ) ) ;
#23385 = DIRECTION ( 'NONE',  ( -1.224646799147350002E-16, 1.836970198721029688E-16, 1.000000000000000000 ) ) ;
#23386 = CARTESIAN_POINT ( 'NONE',  ( 31.24132895666020104, 1440.913060383959873, 242.0645883728159902 ) ) ;
#23388 = CARTESIAN_POINT ( 'NONE',  ( -14.71230246820326393, 1414.913060387329779, 216.6130014222923137 ) ) ;
#23387 = CARTESIAN_POINT ( 'NONE',  ( -10.70956146626689964, 1470.466741431640230, 211.3590706241550095 ) ) ;
#23389 = DIRECTION ( 'NONE',  ( -4.857225732735055447E-14, 0.000000000000000000, 1.000000000000000000 ) ) ;
#23390 = ORIENTED_EDGE ( 'NONE', *, *, #34627, .F. ) ;
#23391 = ORIENTED_EDGE ( 'NONE', *, *, #73439, .T. ) ;
#23392 = CARTESIAN_POINT ( 'NONE',  ( 7.844692007760903252, 1439.683743732501171, 213.0755470696874454 ) ) ;
#23393 = EDGE_CURVE ( 'NONE', #58764, #104774, #34363, .T. ) ;
#23394 = CARTESIAN_POINT ( 'NONE',  ( -19.85899607061380223, 1484.600033915471386, 190.9336331781040883 ) ) ;
#23395 = B_SPLINE_CURVE_WITH_KNOTS ( 'NONE', 3,
 ( #22985, #48228, #91860, #50437, #108105, #22419, #23549, #24088, #7311, #32519, #82910, #33052, #75636, #84010, #99142, #57741, #6201, #56622, #39252, #40353, #6746, #74534, #90757, #67240, #83452, #31954, #101335, #66147, #107562, #16233, #73427, #15135, #57190, #58276, #31401, #24625, #14037, #91314, #48786, #82368, #58822, #108665, #92960, #65581, #49325, #84562, #5667, #15672, #66690, #75085, #30848, #100270, #39814, #40905, #73974, #109235 ),
 .UNSPECIFIED., .F., .F.,
 ( 4, 2, 2, 2, 1, 1, 2, 2, 2, 2, 1, 1, 2, 2, 2, 2, 1, 1, 2, 2, 2, 1, 1, 1, 1, 1, 1, 2, 2, 2, 2, 2, 2, 4 ),
 ( 0.000000000000000000, 0.06250000003649344715, 0.09375000005474017073, 0.1093750000638571834, 0.1171875000684189649, 0.1210937500707053305, 0.1230468750718511778, 0.1250000000729970251, 0.1875000001098633684, 0.2187500001282965401, 0.2343750001375136671, 0.2421875001421222584, 0.2460937501444259434, 0.2500000001467296284, 0.3125000001831972352, 0.3437500002014302058, 0.3593750002105552399, 0.3671875002151185896, 0.3710937502173994318, 0.3750000002196802740, 0.4375000002557568601, 0.4687500002737773341, 0.4843750002828046131, 0.4921875002873182803, 0.4960937502895878537, 0.4980468752907154517, 0.4990234377912663999, 0.4995117190415430120, 0.5000000002918195685, 0.6250000002188711434, 0.7500000001459228294, 0.8750000000729744043, 0.9375000000364872577, 1.000000000000000000 ),
 .UNSPECIFIED. ) ;
#23396 = CARTESIAN_POINT ( 'NONE',  ( -27.68254006319999760, 1507.989615291430027, 210.5775529109679951 ) ) ;
#23397 = CARTESIAN_POINT ( 'NONE',  ( 8.239807433079999299, 1424.467077651120235, 195.8470003964989985 ) ) ;
#23398 = ADVANCED_FACE ( 'NONE', ( #28727 ), #37125, .T. ) ;
#23399 = CARTESIAN_POINT ( 'NONE',  ( 1.440662988484916918, 1507.675818290031202, 236.8848933736155118 ) ) ;
#23400 = AXIS2_PLACEMENT_3D ( 'NONE', #89598, #99635, #38642 ) ;
#23401 = CARTESIAN_POINT ( 'NONE',  ( 9.642184866601970938, 1422.568599004970110, 212.5648991404160029 ) ) ;
#23402 = DIRECTION ( 'NONE',  ( -0.9455185755993178454, 0.000000000000000000, 0.3255681544571537578 ) ) ;
#23403 = CARTESIAN_POINT ( 'NONE',  ( -51.69639516817590419, 1383.809142186679992, 264.8244201884630229 ) ) ;
#23404 = CARTESIAN_POINT ( 'NONE',  ( -3.385713919165000085, 1511.191277613550028, 201.4988854453669944 ) ) ;
#23405 = CARTESIAN_POINT ( 'NONE',  ( 4.500000000000000000, 1411.429641636930000, 137.0999999980979851 ) ) ;
#23406 = CARTESIAN_POINT ( 'NONE',  ( -11.87973986237470037, 1433.324300388509982, 147.6568050210650256 ) ) ;
#23407 = CARTESIAN_POINT ( 'NONE',  ( 11.09105618205479971, 1492.398032610720065, 212.1352801084049986 ) ) ;
#23409 = VERTEX_POINT ( 'NONE', #55602 ) ;
#23408 = CARTESIAN_POINT ( 'NONE',  ( 0.8903357919429990552, 1455.384224998389982, 218.5322622568489805 ) ) ;
#23410 = CARTESIAN_POINT ( 'NONE',  ( 30.51231035492520149, 1526.382868172863937, 218.1578534183718432 ) ) ;
#23411 = ADVANCED_FACE ( 'NONE', ( #72937 ), #30914, .T. ) ;
#23412 = CARTESIAN_POINT ( 'NONE',  ( -8.783909226360000488, 1382.320486701790060, 217.8959194107489736 ) ) ;
#23413 = CARTESIAN_POINT ( 'NONE',  ( -3.603670846500000025, 1475.686176941090025, 199.3076260124989858 ) ) ;
#23414 = ORIENTED_EDGE ( 'NONE', *, *, #33709, .F. ) ;
#23415 = VERTEX_POINT ( 'NONE', #30363 ) ;
#23416 = AXIS2_PLACEMENT_3D ( 'NONE', #62578, #96696, #19967 ) ;
#23417 = DIRECTION ( 'NONE',  ( 1.000000000000000000, 1.810374147724000060E-32, 1.224646799147351975E-16 ) ) ;
#23418 = CARTESIAN_POINT ( 'NONE',  ( -2.329957330370640456, 1515.551704201149960, 205.2926810898260044 ) ) ;
#23420 = CARTESIAN_POINT ( 'NONE',  ( 2.470168521978398424, 1523.382868172864164, 175.3649660270905315 ) ) ;
#23419 = DIRECTION ( 'NONE',  ( -0.4794255386041804123, 0.000000000000000000, 0.8775825618903850822 ) ) ;
#23421 = B_SPLINE_CURVE_WITH_KNOTS ( 'NONE', 5,
 ( #8979, #100820, #15695, #67265, #92421, #86238, #58848, #66714, #93526 ),
 .UNSPECIFIED., .F., .F.,
 ( 6, 3, 6 ),
 ( 0.000000000000000000, 0.5000000000000000000, 1.000000000000000000 ),
 .UNSPECIFIED. ) ;
#23422 = CARTESIAN_POINT ( 'NONE',  ( -9.861036302450001401, 1463.031815716689835, 205.0798590038790223 ) ) ;
#23423 = CARTESIAN_POINT ( 'NONE',  ( -107.1079164160000090, 1379.789533456470053, 299.4362131821590083 ) ) ;
#23424 = CARTESIAN_POINT ( 'NONE',  ( -15.84432591830269743, 1419.853212859319910, 210.7451195136700051 ) ) ;
#23425 = AXIS2_PLACEMENT_3D ( 'NONE', #35244, #41450, #43105 ) ;
#23426 = CARTESIAN_POINT ( 'NONE',  ( -10.30687864337570048, 1508.551704408389924, 218.1317960845860000 ) ) ;
#23427 = CARTESIAN_POINT ( 'NONE',  ( 9.593214614660599437, 1409.248062823570081, 197.6440812670239779 ) ) ;
#23428 = CARTESIAN_POINT ( 'NONE',  ( 18.02088773781200004, 1424.325293679698234, 225.2049038667060188 ) ) ;
#23429 = CARTESIAN_POINT ( 'NONE',  ( 17.91453291880564080, 1458.959407450137860, 216.8828771306792191 ) ) ;
#23430 = CARTESIAN_POINT ( 'NONE',  ( 1.799588937954729850, 1431.296473388759978, 200.2099206183030162 ) ) ;
#23431 = CARTESIAN_POINT ( 'NONE',  ( -3.660095725623159879, 1441.479904334799812, 165.0935399751739965 ) ) ;
#23432 = DIRECTION ( 'NONE',  ( 0.4868800090730913133, -0.8445173987901640755, 0.2230206714761694409 ) ) ;
#23433 = ORIENTED_EDGE ( 'NONE', *, *, #23117, .F. ) ;
#23434 = EDGE_CURVE ( 'NONE', #82045, #84088, #8958, .T. ) ;
#23435 = CARTESIAN_POINT ( 'NONE',  ( 18.88936493758499680, 1456.871008693799922, 227.2529171743470044 ) ) ;
#23436 = EDGE_CURVE ( 'NONE', #88852, #1678, #32199, .T. ) ;
#23437 = CARTESIAN_POINT ( 'NONE',  ( -12.22933646150000087, 1434.134881474460144, 150.1178554876979945 ) ) ;
#23438 = CARTESIAN_POINT ( 'NONE',  ( 3.230487471805439744E-10, 1465.426655107609804, 239.3266822731660000 ) ) ;
#23439 = CARTESIAN_POINT ( 'NONE',  ( -20.45978729620729908, 1503.323240196070174, 190.5211554919499974 ) ) ;
#23440 = CARTESIAN_POINT ( 'NONE',  ( -24.00431565076883444, 1435.335602849082761, 137.4619998928296809 ) ) ;
#23441 = CARTESIAN_POINT ( 'NONE',  ( -109.5835204229999960, 1385.270838993090138, 311.3045831672590111 ) ) ;
#23442 = CARTESIAN_POINT ( 'NONE',  ( -8.469038851160551218, 1511.685732531849681, 215.1092167430809923 ) ) ;
#23443 = CARTESIAN_POINT ( 'NONE',  ( -9.655745333031781286, 1363.739547551595933, 210.6218459616991936 ) ) ;
#23444 = CARTESIAN_POINT ( 'NONE',  ( 4.314829847434388022, 1413.913060387330006, 217.0200890187050504 ) ) ;
#23445 = CARTESIAN_POINT ( 'NONE',  ( -2.500000000000000000, 1439.615672362009946, 183.5288080637979817 ) ) ;
#23446 = CARTESIAN_POINT ( 'NONE',  ( -19.67294290438620052, 1440.103789594400041, 208.5487540470539898 ) ) ;
#23447 = EDGE_CURVE ( 'NONE', #44473, #64662, #29012, .T. ) ;
#23448 = CARTESIAN_POINT ( 'NONE',  ( 6.550870144104999682, 1516.727502608469877, 208.3674577492799926 ) ) ;
#23449 = CARTESIAN_POINT ( 'NONE',  ( 2.751944573164369690, 1408.825585930090028, 223.0235821367669757 ) ) ;
#23450 = CARTESIAN_POINT ( 'NONE',  ( 29.35747451428488830, 1526.382868172571079, 201.0438982057034423 ) ) ;
#23451 = CARTESIAN_POINT ( 'NONE',  ( 11.29523459009999975, 1425.738185348830029, 112.3426556953979940 ) ) ;
#23452 = CARTESIAN_POINT ( 'NONE',  ( 7.502917382035859895, 1425.357894886970143, 212.2409982979840208 ) ) ;
#23453 = VECTOR ( 'NONE', #97324, 1000.000000000000000 ) ;
#23454 = EDGE_CURVE ( 'NONE', #39930, #34471, #13733, .T. ) ;
#23455 = ORIENTED_EDGE ( 'NONE', *, *, #110441, .F. ) ;
#23456 = CARTESIAN_POINT ( 'NONE',  ( 20.00477949819999779, 1428.885732890330019, 217.2611606326379956 ) ) ;
#23457 = DIRECTION ( 'NONE',  ( 0.000000000000000000, 0.7071067811865475727, 0.7071067811865475727 ) ) ;
#23459 = CARTESIAN_POINT ( 'NONE',  ( 24.91017775802731649, 1509.782942962777497, 224.3120645653099245 ) ) ;
#23458 = CARTESIAN_POINT ( 'NONE',  ( 1.456422591599999983, 1499.391639968829850, 181.4501326743979917 ) ) ;
#23460 = CARTESIAN_POINT ( 'NONE',  ( -7.848979634317430509, 1517.151704408390060, 202.2988320601959913 ) ) ;
#23461 = CARTESIAN_POINT ( 'NONE',  ( -21.71651236630000170, 1429.876880566229829, 220.8156635984979914 ) ) ;
#23462 = CARTESIAN_POINT ( 'NONE',  ( -28.55509083404212944, 1509.910676538754842, 202.0965624507188636 ) ) ;
#23463 = CARTESIAN_POINT ( 'NONE',  ( -12.56757494846049994, 1452.474190999480015, 149.3742479200809896 ) ) ;
#23464 = FACE_OUTER_BOUND ( 'NONE', #106259, .T. ) ;
#23465 = ORIENTED_EDGE ( 'NONE', *, *, #95662, .T. ) ;
#23466 = CARTESIAN_POINT ( 'NONE',  ( -2.500000000000000000, 1421.191390850129892, 151.1105839291980146 ) ) ;
#23467 = CARTESIAN_POINT ( 'NONE',  ( -7.848979634317430509, 1522.051704408389924, 202.2988320601959913 ) ) ;
#23468 = CARTESIAN_POINT ( 'NONE',  ( 15.55407252301110077, 1422.604129201769865, 228.8743534404409843 ) ) ;
#23469 = CARTESIAN_POINT ( 'NONE',  ( 0.000000000000000000, 1511.187213306747708, 209.1218459616979999 ) ) ;
#23470 = ORIENTED_EDGE ( 'NONE', *, *, #65180, .F. ) ;
#23471 = EDGE_LOOP ( 'NONE', ( #80999, #90798, #100052, #97238, #82873 ) ) ;
#23472 = EDGE_CURVE ( 'NONE', #76166, #68839, #94418, .T. ) ;
#23473 = CARTESIAN_POINT ( 'NONE',  ( -75.49940225679999628, 1385.016445804960085, 276.6852814938590086 ) ) ;
#23474 = CARTESIAN_POINT ( 'NONE',  ( -23.04342231024600096, 1409.747493226589995, 209.0991873506499985 ) ) ;
#23475 = CARTESIAN_POINT ( 'NONE',  ( -4.146783142809999489, 1426.018316099529784, 186.1121553539979914 ) ) ;
#23476 = CARTESIAN_POINT ( 'NONE',  ( 0.3628711435760000326, 1419.323187844430095, 227.2866819789979900 ) ) ;
#23477 = CARTESIAN_POINT ( 'NONE',  ( -10.18103031238790024, 1517.299312825791731, 184.9292055843397975 ) ) ;
#23478 = ADVANCED_FACE ( 'NONE', ( #91921 ), #65643, .F. ) ;
#23479 = CARTESIAN_POINT ( 'NONE',  ( -4.438764019890000689, 1507.637717467430093, 236.4803969381979982 ) ) ;
#23480 = CARTESIAN_POINT ( 'NONE',  ( -19.40852230999999861, 1415.853157747729938, 222.6427874863980207 ) ) ;
#23481 = ORIENTED_EDGE ( 'NONE', *, *, #62860, .F. ) ;
#23482 = CARTESIAN_POINT ( 'NONE',  ( 45.90364696054209759, 1443.726197624660017, 268.5001126654299810 ) ) ;
#23483 = CARTESIAN_POINT ( 'NONE',  ( -4.556911044178249881, 1508.729442775010057, 205.2988566914049784 ) ) ;
#23484 = CARTESIAN_POINT ( 'NONE',  ( -0.005520699207629999571, 1419.740206832129843, 184.3860476924980105 ) ) ;
#23485 = CARTESIAN_POINT ( 'NONE',  ( -5.010423001364999962, 1516.929569650079884, 205.0907035804270038 ) ) ;
#23486 = AXIS2_PLACEMENT_3D ( 'NONE', #6438, #99369, #49557 ) ;
#23487 = VERTEX_POINT ( 'NONE', #15195 ) ;
#23488 = CARTESIAN_POINT ( 'NONE',  ( 6.445177767125850110, 1483.523613335260052, 219.0471454115900087 ) ) ;
#23489 = CARTESIAN_POINT ( 'NONE',  ( 15.28467102806859934, 1512.548660307890032, 195.8467575762399804 ) ) ;
#23490 = CARTESIAN_POINT ( 'NONE',  ( 8.236825666079377939, 1479.663677487053747, 202.5474313781959950 ) ) ;
#23491 = ORIENTED_EDGE ( 'NONE', *, *, #33357, .T. ) ;
#23492 = CARTESIAN_POINT ( 'NONE',  ( -10.84028572272250024, 1480.780801381620222, 210.8784252212099943 ) ) ;
#23493 = CARTESIAN_POINT ( 'NONE',  ( 26.58146304371889812, 1451.968400311360028, 135.1860841996399927 ) ) ;
#23494 = CARTESIAN_POINT ( 'NONE',  ( -12.53206807815550050, 1512.191474810040063, 194.1217683614299858 ) ) ;
#23495 = CARTESIAN_POINT ( 'NONE',  ( 0.1216143914258819986, 1452.908813519200066, 152.5222040808779980 ) ) ;
#23496 = CARTESIAN_POINT ( 'NONE',  ( 7.431520146699999607, 1422.886000214980186, 195.6153521392990058 ) ) ;
#23497 = CARTESIAN_POINT ( 'NONE',  ( -4.121959999953849874, 1425.947382011577702, 186.1095471754434243 ) ) ;
#23498 = CARTESIAN_POINT ( 'NONE',  ( -11.38101510873019961, 1491.910250263850230, 204.5016764512789962 ) ) ;
#23499 = CARTESIAN_POINT ( 'NONE',  ( 10.76386117010460097, 1478.973846364719975, 205.9615306354030224 ) ) ;
#23500 = CARTESIAN_POINT ( 'NONE',  ( 2.112814772436390154, 1408.986841504970016, 186.9590526398459929 ) ) ;
#23502 = CARTESIAN_POINT ( 'NONE',  ( -18.36927172832351474, 1424.107301416295286, 225.2316973828278890 ) ) ;
#23501 = CARTESIAN_POINT ( 'NONE',  ( -16.97624119622160066, 1420.556660208560061, 191.4662531876780065 ) ) ;
#23503 = CARTESIAN_POINT ( 'NONE',  ( 2.959300169439202044, 1440.912996883657570, 170.5323342380343092 ) ) ;
#23504 = AXIS2_PLACEMENT_3D ( 'NONE', #20944, #81398, #28824 ) ;
#23505 = CARTESIAN_POINT ( 'NONE',  ( -14.01399965579999929, 1379.590355683860025, 211.9184156875489862 ) ) ;
#23506 = CARTESIAN_POINT ( 'NONE',  ( 2.265645423020000049, 1414.246892558129957, 164.3383647881979925 ) ) ;
#23507 = ORIENTED_EDGE ( 'NONE', *, *, #74271, .F. ) ;
#23508 = CARTESIAN_POINT ( 'NONE',  ( 21.37693748330000076, 1438.522492596059919, 224.8635561966979708 ) ) ;
#23509 = CYLINDRICAL_SURFACE ( 'NONE', #39151, 26.50000000000001421 ) ;
#23510 = CARTESIAN_POINT ( 'NONE',  ( -108.8990485207509948, 1384.924713768860101, 311.2645749510550104 ) ) ;
#23511 = CARTESIAN_POINT ( 'NONE',  ( -8.964263409860000920, 1385.771258260049763, 200.0191890160589878 ) ) ;
#23512 = CARTESIAN_POINT ( 'NONE',  ( 10.03585564278080078, 1426.955176195429885, 209.6792063305699969 ) ) ;
#23513 = CARTESIAN_POINT ( 'NONE',  ( 12.16717212215749910, 1426.186041745560033, 202.7890921220440248 ) ) ;
#23514 = CARTESIAN_POINT ( 'NONE',  ( 1.455000209906389896, 1507.073729425429974, 236.7651043255590082 ) ) ;
#23515 = VECTOR ( 'NONE', #87325, 999.9999999999998863 ) ;
#23516 = CARTESIAN_POINT ( 'NONE',  ( -43.50000000000000000, 1440.913060387330006, 271.1218459616979999 ) ) ;
#23517 = CARTESIAN_POINT ( 'NONE',  ( -8.053024569705350189, 1477.121180019175654, 215.6798857060248622 ) ) ;
#23518 = DIRECTION ( 'NONE',  ( -0.7414773880254760252, 0.000000000000000000, -0.6709778558543624261 ) ) ;
#23519 = CARTESIAN_POINT ( 'NONE',  ( 37.18025153319999276, 1449.733372704670273, 265.6112249940979950 ) ) ;
#23520 = FACE_OUTER_BOUND ( 'NONE', #22982, .T. ) ;
#23521 = CARTESIAN_POINT ( 'NONE',  ( -16.80834505000999712, 1420.460051406040066, 203.2687812860760062 ) ) ;
#23522 = CARTESIAN_POINT ( 'NONE',  ( -108.8108081923106596, 1388.207833152419198, 297.7714192390470771 ) ) ;
#23523 = CARTESIAN_POINT ( 'NONE',  ( 5.945385552781929484, 1466.587269241879994, 217.1256145497779926 ) ) ;
#23524 = EDGE_CURVE ( 'NONE', #63875, #43726, #105333, .T. ) ;
#23525 = CARTESIAN_POINT ( 'NONE',  ( -10.01326586723869916, 1481.014341800280135, 205.7823588363200145 ) ) ;
#23526 = CARTESIAN_POINT ( 'NONE',  ( 2.644243049506179943, 1474.633123746480123, 220.2308870144509854 ) ) ;
#23527 = CARTESIAN_POINT ( 'NONE',  ( 3.313501335607582643, 1397.551704408390151, 215.1871694724064810 ) ) ;
#23528 = CIRCLE ( 'NONE', #37863, 1.999999999999998668 ) ;
#23529 = CARTESIAN_POINT ( 'NONE',  ( -7.351095455360000308, 1491.337165262789995, 211.7591980188690002 ) ) ;
#23530 = CARTESIAN_POINT ( 'NONE',  ( -25.42735443440000154, 1450.801672132440217, 137.2052187181979832 ) ) ;
#23531 = CARTESIAN_POINT ( 'NONE',  ( -16.84515702779830093, 1409.666169224270106, 192.5998696085950144 ) ) ;
#23532 = CARTESIAN_POINT ( 'NONE',  ( 12.78690732370000127, 1416.828044896230040, 222.7042044813979942 ) ) ;
#23533 = FACE_OUTER_BOUND ( 'NONE', #30196, .T. ) ;
#23534 =( BOUNDED_CURVE ( )  B_SPLINE_CURVE ( 3, ( #99524, #13864, #73248, #4927 ),
 .UNSPECIFIED., .F., .F. ) 
 B_SPLINE_CURVE_WITH_KNOTS ( ( 4, 4 ),
 ( 4.745561737044720729, 4.756500625272940042 ),
 .UNSPECIFIED. ) 
 CURVE ( )  GEOMETRIC_REPRESENTATION_ITEM ( )  RATIONAL_B_SPLINE_CURVE ( ( 1.000000000000000000, 0.9999900284185523347, 0.9999900284185523347, 1.000000000000000000 ) ) 
 REPRESENTATION_ITEM ( '' )  );
#23535 = CARTESIAN_POINT ( 'NONE',  ( -19.04700355086820096, 1444.155872664750177, 199.5980004632280043 ) ) ;
#23536 = CARTESIAN_POINT ( 'NONE',  ( 1.581901184577762853, 1426.946688134061105, 134.0999999980979851 ) ) ;
#23537 = CARTESIAN_POINT ( 'NONE',  ( 0.2065023403792599910, 1459.318095313439926, 182.9823369938129929 ) ) ;
#23539 = EDGE_LOOP ( 'NONE', ( #91491, #12206 ) ) ;
#23538 = CARTESIAN_POINT ( 'NONE',  ( -6.157363072879999955, 1409.067554757129756, 222.6581951653980127 ) ) ;
#23540 = CARTESIAN_POINT ( 'NONE',  ( -18.43688931543649190, 1444.994950788470533, 161.6100378850031234 ) ) ;
#23541 = EDGE_CURVE ( 'NONE', #15766, #94444, #42484, .T. ) ;
#23542 = CARTESIAN_POINT ( 'NONE',  ( -28.59140520858730028, 1509.720434423589950, 211.2156787647219858 ) ) ;
#23543 = CARTESIAN_POINT ( 'NONE',  ( 12.40430713589999989, 1434.419976112569884, 147.9455075187979674 ) ) ;
#23544 = CARTESIAN_POINT ( 'NONE',  ( -41.65974987178940125, 1443.430997014530021, 134.0999999981650035 ) ) ;
#23545 = CARTESIAN_POINT ( 'NONE',  ( -109.3495745150000005, 1384.893444084359999, 297.1386071063589611 ) ) ;
#23546 = EDGE_LOOP ( 'NONE', ( #87040, #72741, #38695, #94531, #41945, #21689, #110369, #107299, #70612, #17318 ) ) ;
#23547 = CARTESIAN_POINT ( 'NONE',  ( -16.94364159994526986, 1525.231887713386186, 181.3784724611917625 ) ) ;
#23548 = DIRECTION ( 'NONE',  ( 0.000000000000000000, 1.000000000000000000, 0.000000000000000000 ) ) ;
#23549 = CARTESIAN_POINT ( 'NONE',  ( -103.6396175609407351, 1379.933997479830168, 304.9922815699929970 ) ) ;
#23550 = CARTESIAN_POINT ( 'NONE',  ( -10.90040294519999975, 1492.525757351089851, 207.2558712963190146 ) ) ;
#23551 = EDGE_CURVE ( 'NONE', #38761, #13254, #107932, .T. ) ;
#23552 = CARTESIAN_POINT ( 'NONE',  ( 2.123005411769999906, 1469.492284959789913, 189.2609491558989987 ) ) ;
#23553 = CARTESIAN_POINT ( 'NONE',  ( 35.58608576442487248, 1419.490279919586328, 269.2370718515488761 ) ) ;
#23554 = FACE_OUTER_BOUND ( 'NONE', #69817, .T. ) ;
#23555 = CARTESIAN_POINT ( 'NONE',  ( -13.02112344040000025, 1380.010336238359969, 210.3784953617490032 ) ) ;
#23556 = CARTESIAN_POINT ( 'NONE',  ( 32.38601544705583990, 1523.530935881284904, 202.1199691060085968 ) ) ;
#23557 = CARTESIAN_POINT ( 'NONE',  ( -61.13392802363229350, 1385.066938601299853, 246.4491151330799994 ) ) ;
#23558 = CARTESIAN_POINT ( 'NONE',  ( -11.65231821165970061, 1391.913060387289988, 209.9483455405510028 ) ) ;
#23559 = CARTESIAN_POINT ( 'NONE',  ( 11.20703803478759930, 1426.374986909809877, 206.7608603490599819 ) ) ;
#23560 = ORIENTED_EDGE ( 'NONE', *, *, #103486, .T. ) ;
#23561 = CARTESIAN_POINT ( 'NONE',  ( -28.40191814786259883, 1508.834101309289963, 208.8103828110809843 ) ) ;
#23562 = CARTESIAN_POINT ( 'NONE',  ( -16.54489977905999964, 1410.128898629499872, 226.3156677813840076 ) ) ;
#23564 = EDGE_LOOP ( 'NONE', ( #49947, #75689, #100976, #31666 ) ) ;
#23563 = CARTESIAN_POINT ( 'NONE',  ( -2.385013337802742495, 1526.073434386619510, 240.5311849226266645 ) ) ;
#23565 = CARTESIAN_POINT ( 'NONE',  ( 3.790668365970000231, 1474.135722993289846, 219.4689549067989844 ) ) ;
#23566 = CARTESIAN_POINT ( 'NONE',  ( 10.71811212121339807, 1471.486163717210047, 211.4980701100689942 ) ) ;
#23567 = CARTESIAN_POINT ( 'NONE',  ( -20.89012358491003596, 1411.002044536383437, 218.6339710684976581 ) ) ;
#23568 = CARTESIAN_POINT ( 'NONE',  ( -109.9878148690000046, 1384.765614765949977, 311.4533902662590208 ) ) ;
#23569 = CARTESIAN_POINT ( 'NONE',  ( -0.3711878547863939892, 1418.751852236400055, 184.7050034054750256 ) ) ;
#23570 = ADVANCED_FACE ( 'NONE', ( #76232 ), #43072, .T. ) ;
#23571 = CARTESIAN_POINT ( 'NONE',  ( 21.89160165000000191, 1409.841974678430006, 214.9120575694479669 ) ) ;
#23572 = CARTESIAN_POINT ( 'NONE',  ( -2.920701990467229781, 1417.235411609819948, 186.3067063531650263 ) ) ;
#23573 = CARTESIAN_POINT ( 'NONE',  ( -16.67802482740000158, 1423.369746731130135, 229.1820141820979870 ) ) ;
#23574 = CARTESIAN_POINT ( 'NONE',  ( -4.434000058850124937, 1511.410071747451866, 200.7859701086250936 ) ) ;
#23575 = CARTESIAN_POINT ( 'NONE',  ( 9.145064070970001069, 1450.428955669789957, 207.9342079490990045 ) ) ;
#23576 = CARTESIAN_POINT ( 'NONE',  ( -106.3607388212290061, 1309.112692017090239, 308.0674119603681902 ) ) ;
#23577 = EDGE_CURVE ( 'NONE', #35203, #25053, #40243, .T. ) ;
#23578 = CARTESIAN_POINT ( 'NONE',  ( -3.763781937370000108, 1369.097489338550076, 207.6218459616989946 ) ) ;
#23579 = CARTESIAN_POINT ( 'NONE',  ( -30.68434753588525155, 1526.000688113616661, 216.8500914423166819 ) ) ;
#23580 = EDGE_CURVE ( 'NONE', #6969, #75505, #93854, .T. ) ;
#23581 = AXIS2_PLACEMENT_3D ( 'NONE', #93654, #61228, #85830 ) ;
#23582 = CARTESIAN_POINT ( 'NONE',  ( -2.297085753945000253, 1516.718889242609976, 205.0950684461469962 ) ) ;
#23583 = CARTESIAN_POINT ( 'NONE',  ( -12.71625625589999942, 1484.464918063330060, 185.9897890590980012 ) ) ;
#23584 = ORIENTED_EDGE ( 'NONE', *, *, #19347, .F. ) ;
#23585 = CARTESIAN_POINT ( 'NONE',  ( -17.17760814124009983, 1517.051704413129983, 195.4929600000709797 ) ) ;
#23586 = DIRECTION ( 'NONE',  ( -0.6081597637245996779, 0.7938146520356244018, 0.000000000000000000 ) ) ;
#23588 = ORIENTED_EDGE ( 'NONE', *, *, #12007, .T. ) ;
#23587 = CARTESIAN_POINT ( 'NONE',  ( -68.66102733441179851, 1379.747688256459924, 280.2626083829800336 ) ) ;
#23589 = EDGE_CURVE ( 'NONE', #43187, #50508, #63546, .T. ) ;
#23590 = ORIENTED_EDGE ( 'NONE', *, *, #32289, .T. ) ;
#23591 = CARTESIAN_POINT ( 'NONE',  ( -10.49976491246964017, 1379.056602952379990, 215.6293701293769800 ) ) ;
#23592 = ORIENTED_EDGE ( 'NONE', *, *, #44723, .T. ) ;
#23593 = CARTESIAN_POINT ( 'NONE',  ( -0.9396743887285590180, 1486.122836457870108, 220.9886464860670117 ) ) ;
#23594 = CARTESIAN_POINT ( 'NONE',  ( -23.04597175440000001, 1410.910372373229848, 204.9159820316880030 ) ) ;
#23596 = CARTESIAN_POINT ( 'NONE',  ( 15.85178800091950002, 1409.849131890500075, 191.9518116726889900 ) ) ;
#23595 = CARTESIAN_POINT ( 'NONE',  ( -11.15965917747685410, 1425.157781931322461, 144.4782180148434634 ) ) ;
#23597 = CARTESIAN_POINT ( 'NONE',  ( 2.300729626665000360, 1516.923170579120097, 210.8225527465970117 ) ) ;
#23598 = CARTESIAN_POINT ( 'NONE',  ( 41.51359561934580711, 1442.004548209790073, 135.9438258381890137 ) ) ;
#23599 = TOROIDAL_SURFACE ( 'NONE', #62988, 30.13701971169416538, 3.000000000000000000 ) ;
#23600 = CARTESIAN_POINT ( 'NONE',  ( -107.3791820827839985, 1378.913060387289988, 307.6919078974059971 ) ) ;
#23601 = CARTESIAN_POINT ( 'NONE',  ( -3.666694481987490040, 1509.114858341099989, 179.5219341129400163 ) ) ;
#23602 = CARTESIAN_POINT ( 'NONE',  ( 9.783750736287140981, 1464.829832912111442, 232.4492286805421202 ) ) ;
#23603 = DIRECTION ( 'NONE',  ( 1.755985294532464991E-16, -1.000000000000000000, 1.338183447452830017E-16 ) ) ;
#23604 = DIRECTION ( 'NONE',  ( -0.000000000000000000, -1.000000000000000000, -0.000000000000000000 ) ) ;
#23605 = EDGE_LOOP ( 'NONE', ( #46849, #101853, #77887 ) ) ;
#23606 = CARTESIAN_POINT ( 'NONE',  ( -21.51339057090000040, 1505.551704408389924, 209.1218459616989946 ) ) ;
#23607 = ADVANCED_FACE ( 'NONE', ( #86277 ), #100211, .T. ) ;
#23608 = CARTESIAN_POINT ( 'NONE',  ( -3.909710721586120208, 1517.051704408389924, 197.7672215555029993 ) ) ;
#23609 = ORIENTED_EDGE ( 'NONE', *, *, #16496, .T. ) ;
#23610 = ORIENTED_EDGE ( 'NONE', *, *, #81716, .T. ) ;
#23611 = DIRECTION ( 'NONE',  ( 1.000000000000000000, 0.000000000000000000, 0.000000000000000000 ) ) ;
#23612 = CARTESIAN_POINT ( 'NONE',  ( 10.41388400344690091, 1453.143260227160226, 211.1213780663029809 ) ) ;
#23613 = B_SPLINE_CURVE_WITH_KNOTS ( 'NONE', 3,
 ( #95832, #87444, #10739, #54415, #88547, #98023, #63373, #11832, #80134, #12369, #46555, #72308, #70126, #21295, #78489, #1803, #44912, #36477, #48200, #6174, #48756, #31372 ),
 .UNSPECIFIED., .F., .F.,
 ( 4, 2, 2, 2, 2, 2, 2, 2, 2, 2, 4 ),
 ( 0.000000000000000000, 0.0004646859671260076966, 0.0009293719342520153932, 0.001394057901378022981, 0.001626400884941100501, 0.001858743868504178238, 0.002091086852067255974, 0.002323429835630333711, 0.002788115802756573319, 0.003252801769882813360, 0.003717487737009052967 ),
 .UNSPECIFIED. ) ;
#23614 = CARTESIAN_POINT ( 'NONE',  ( -0.008321110301990000332, 1451.173510518130115, 182.5308026085980089 ) ) ;
#23615 = CARTESIAN_POINT ( 'NONE',  ( -2.330134127310790060, 1515.064792882719985, 213.4512947379739956 ) ) ;
#23616 = CARTESIAN_POINT ( 'NONE',  ( -2.500000000000000000, 1439.611175468640113, 167.3041000418980104 ) ) ;
#23617 = ADVANCED_FACE ( 'NONE', ( #28580 ), #42149, .T. ) ;
#23619 = CARTESIAN_POINT ( 'NONE',  ( -30.31940284292426924, 1523.382868172864164, 195.7503880523418616 ) ) ;
#23618 = VECTOR ( 'NONE', #50524, 999.9999999999998863 ) ;
#23620 = CARTESIAN_POINT ( 'NONE',  ( -28.07231162100000077, 1508.101920006030241, 207.7749232119980149 ) ) ;
#23621 = CARTESIAN_POINT ( 'NONE',  ( 36.37832866288330536, 1451.642701157629745, 135.6938360142119961 ) ) ;
#23622 = CARTESIAN_POINT ( 'NONE',  ( -19.96011951328586420, 1485.861506872206974, 214.4463820970520374 ) ) ;
#23623 = CARTESIAN_POINT ( 'NONE',  ( 27.50386082860000059, 1440.425502049640045, 137.1894327424980133 ) ) ;
#23624 = EDGE_CURVE ( 'NONE', #82581, #66323, #108178, .T. ) ;
#23625 = CARTESIAN_POINT ( 'NONE',  ( -10.79387578689999927, 1391.590462314130036, 214.7676431958390140 ) ) ;
#23626 = CARTESIAN_POINT ( 'NONE',  ( -69.45604853682949908, 1384.733805731689927, 264.7784157945660013 ) ) ;
#23627 = VERTEX_POINT ( 'NONE', #102387 ) ;
#23628 = TOROIDAL_SURFACE ( 'NONE', #12834, 1.000000000000000000, 1.000000000000000000 ) ;
#23629 = CARTESIAN_POINT ( 'NONE',  ( 6.553524377605000062, 1516.882690742909972, 202.1776141839370098 ) ) ;
#23630 = CARTESIAN_POINT ( 'NONE',  ( -2.491655763544999846, 1516.977504706749869, 208.3867361609839861 ) ) ;
#23631 = ORIENTED_EDGE ( 'NONE', *, *, #30416, .F. ) ;
#23632 = CARTESIAN_POINT ( 'NONE',  ( 41.78528023106409961, 1440.913060387330006, 269.3547801055810282 ) ) ;
#23633 = CARTESIAN_POINT ( 'NONE',  ( -0.0007848984903239803303, 1451.920411048226470, 154.0000879905409192 ) ) ;
#23634 = VERTEX_POINT ( 'NONE', #78875 ) ;
#23635 = CARTESIAN_POINT ( 'NONE',  ( -14.04614445250000188, 1415.579607678630055, 221.1977299884980255 ) ) ;
#23636 = CARTESIAN_POINT ( 'NONE',  ( -11.65870824634879988, 1432.338283297729959, 150.9211958027459843 ) ) ;
#23637 = CARTESIAN_POINT ( 'NONE',  ( -17.59976141832330043, 1419.797097700060021, 206.6695233765389901 ) ) ;
#23638 = CARTESIAN_POINT ( 'NONE',  ( -9.362058791585690543, 1461.114539333109860, 206.6197382024370199 ) ) ;
#23639 = CARTESIAN_POINT ( 'NONE',  ( -12.88992692469999923, 1429.132124773229862, 222.5285527285979867 ) ) ;
#23640 = CARTESIAN_POINT ( 'NONE',  ( 9.987216885397780075, 1469.109414354970113, 207.4754563298509993 ) ) ;
#23641 = CARTESIAN_POINT ( 'NONE',  ( 7.443246446248299009, 1423.092341332710021, 195.6161848952980051 ) ) ;
#23642 = CARTESIAN_POINT ( 'NONE',  ( -11.94143867729999897, 1433.615104777220040, 147.8551380903979862 ) ) ;
#23643 = CARTESIAN_POINT ( 'NONE',  ( 26.02020593944349969, 1489.081220952810099, 206.2263664854170031 ) ) ;
#23645 = DIRECTION ( 'NONE',  ( 0.000000000000000000, 1.000000000000000000, 0.000000000000000000 ) ) ;
#23644 = CARTESIAN_POINT ( 'NONE',  ( 17.51720238729999934, 1459.587282136729982, 228.3696857288979913 ) ) ;
#23646 = CARTESIAN_POINT ( 'NONE',  ( 19.79329231029999647, 1474.474811148189929, 213.0571447478990024 ) ) ;
#23647 = DIRECTION ( 'NONE',  ( -0.000000000000000000, -1.000000000000000000, -0.000000000000000000 ) ) ;
#23648 = VERTEX_POINT ( 'NONE', #59862 ) ;
#23649 = CARTESIAN_POINT ( 'NONE',  ( -22.71351678742513158, 1409.706230938278395, 208.9920840151032735 ) ) ;
#23650 = CARTESIAN_POINT ( 'NONE',  ( -0.03160925563740960703, 1508.847401064120049, 179.7329215851769959 ) ) ;
#23651 = CARTESIAN_POINT ( 'NONE',  ( 0.8692293861700702839, 1516.691033975803066, 216.8349817968451703 ) ) ;
#23652 = CARTESIAN_POINT ( 'NONE',  ( -4.610938249504999753, 1516.815231249920089, 213.1623732742069990 ) ) ;
#23653 = CARTESIAN_POINT ( 'NONE',  ( 18.46505082730000069, 1509.557874170530113, 187.1463136621979970 ) ) ;
#23654 = CARTESIAN_POINT ( 'NONE',  ( -11.60004869885203505, 1425.163648245827062, 137.9639116245677997 ) ) ;
#23656 = VERTEX_POINT ( 'NONE', #43605 ) ;
#23655 = CARTESIAN_POINT ( 'NONE',  ( 4.678149135874779319, 1508.611352721110052, 212.6094320121750059 ) ) ;
#23657 = CARTESIAN_POINT ( 'NONE',  ( -8.156254201879999499, 1384.896657262430153, 199.6468321548190090 ) ) ;
#23658 = CARTESIAN_POINT ( 'NONE',  ( 2.413234528069999829, 1507.615208039690060, 220.6132374451989904 ) ) ;
#23659 = CARTESIAN_POINT ( 'NONE',  ( -11.85198087010000023, 1431.354781565790063, 149.8962517293980170 ) ) ;
#23660 = FACE_OUTER_BOUND ( 'NONE', #41576, .T. ) ;
#23661 = CARTESIAN_POINT ( 'NONE',  ( -5.618830611241669715, 1441.039434150369743, 202.2715367274489893 ) ) ;
#23662 = CARTESIAN_POINT ( 'NONE',  ( 27.02941372530000308, 1451.801869924330049, 135.6489090826979975 ) ) ;
#23663 = CARTESIAN_POINT ( 'NONE',  ( -4.244126290243009691, 1428.207434869309964, 200.7816286936110259 ) ) ;
#23664 = CARTESIAN_POINT ( 'NONE',  ( -4.999835795559509855, 1447.920857802409955, 212.7698679858029891 ) ) ;
#23666 = CARTESIAN_POINT ( 'NONE',  ( -2.456317400796513173, 1421.792675212155928, 137.0999999980980704 ) ) ;
#23665 = CARTESIAN_POINT ( 'NONE',  ( -25.76221643539999917, 1495.363080995530026, 215.5756636875879906 ) ) ;
#23667 = CARTESIAN_POINT ( 'NONE',  ( -6.121215447810000043, 1471.624333221390089, 212.8646130425990179 ) ) ;
#23668 = ORIENTED_EDGE ( 'NONE', *, *, #10303, .T. ) ;
#23669 = CARTESIAN_POINT ( 'NONE',  ( -0.7574260232259989456, 1516.837969789639828, 205.8660360680970030 ) ) ;
#23670 = CARTESIAN_POINT ( 'NONE',  ( 6.176534431810000392, 1406.368378108629940, 269.0307194043979848 ) ) ;
#23671 = CARTESIAN_POINT ( 'NONE',  ( -2.500000000000000000, 1439.114301494319989, 157.7261950941980331 ) ) ;
#23672 = CARTESIAN_POINT ( 'NONE',  ( 10.90953519108039949, 1489.918727231739922, 208.2510843807270078 ) ) ;
#23673 = CARTESIAN_POINT ( 'NONE',  ( 24.16053673582425176, 1436.344787939296566, 213.4465298597629328 ) ) ;
#23674 = CARTESIAN_POINT ( 'NONE',  ( -7.794443285332278037, 1386.710985943309879, 218.8404340897528186 ) ) ;
#23675 = CARTESIAN_POINT ( 'NONE',  ( -11.41676025498539815, 1482.775671442730072, 205.7339583212410048 ) ) ;
#23676 = DIRECTION ( 'NONE',  ( 0.000000000000000000, 0.000000000000000000, -1.000000000000000000 ) ) ;
#23677 = CARTESIAN_POINT ( 'NONE',  ( -14.58700458240000053, 1416.104883097150150, 204.1284875012190128 ) ) ;
#23678 = CARTESIAN_POINT ( 'NONE',  ( -1.564574781134263626, 1451.289357135363161, 183.8180204487754565 ) ) ;
#23679 = CARTESIAN_POINT ( 'NONE',  ( 1.466050869238679999, 1450.686205474260078, 155.3356453482439861 ) ) ;
#23680 = LINE ( 'NONE', #102030, #8961 ) ;
#23681 = CARTESIAN_POINT ( 'NONE',  ( -4.282693164180000345, 1515.349926011190064, 210.2223588092890054 ) ) ;
#23682 = CARTESIAN_POINT ( 'NONE',  ( -19.00000000000000000, 1438.871025162500018, 209.1218459616979999 ) ) ;
#23683 = CARTESIAN_POINT ( 'NONE',  ( -11.60004869885203682, -0.000000000000000000, 135.5999999980979851 ) ) ;
#23684 = CARTESIAN_POINT ( 'NONE',  ( 4.283856808220000367, 1440.956245581859775, 155.9230798038979913 ) ) ;
#23685 = CARTESIAN_POINT ( 'NONE',  ( -7.055157488669999921, 1475.427864936029891, 266.9413125670979525 ) ) ;
#23686 = CARTESIAN_POINT ( 'NONE',  ( -4.220676207128734703, 1446.230049502166139, 170.5366217123670083 ) ) ;
#23687 = CARTESIAN_POINT ( 'NONE',  ( -12.73368289317676094, 1513.317521358512295, 192.3517865229087533 ) ) ;
#23688 = CARTESIAN_POINT ( 'NONE',  ( 1.770994272916319279, 1526.211528530236592, 240.5584569913896189 ) ) ;
#23689 = CARTESIAN_POINT ( 'NONE',  ( -50.03546363177220968, 1384.739880094399950, 261.8130513971230471 ) ) ;
#23690 = DIRECTION ( 'NONE',  ( -1.755985294532469921E-16, 1.000000000000000000, -1.338183447452831989E-16 ) ) ;
#23691 = AXIS2_PLACEMENT_3D ( 'NONE', #105209, #28497, #29053 ) ;
#23692 = CARTESIAN_POINT ( 'NONE',  ( 16.42420380379999756, 1507.212883763329955, 193.5443561786979956 ) ) ;
#23693 = CARTESIAN_POINT ( 'NONE',  ( -24.61334319966909945, 1444.769530411740107, 210.8865013930089845 ) ) ;
#23694 = CARTESIAN_POINT ( 'NONE',  ( 31.75409331310657990, 1525.055402519452173, 216.6568980277143908 ) ) ;
#23695 = DIRECTION ( 'NONE',  ( -0.3090169943749403458, 0.000000000000000000, 0.9510565162951560847 ) ) ;
#23696 = CARTESIAN_POINT ( 'NONE',  ( -20.44853841340000145, 1410.549219022030002, 198.9863064543980329 ) ) ;
#23697 = CARTESIAN_POINT ( 'NONE',  ( -11.14745452005457871, 1378.905166874835913, 203.8219142046758634 ) ) ;
#23698 = CARTESIAN_POINT ( 'NONE',  ( 12.53106854449860030, 1421.570172124900182, 207.2100616318859920 ) ) ;
#23699 = CARTESIAN_POINT ( 'NONE',  ( 10.10120055931009908, 1480.591734632540010, 206.1129840487050160 ) ) ;
#23700 = ADVANCED_FACE ( 'NONE', ( #86698 ), #25115, .F. ) ;
#23701 = EDGE_LOOP ( 'NONE', ( #66557, #55785, #81306, #56138 ) ) ;
#23702 = CARTESIAN_POINT ( 'NONE',  ( -6.934382790878020231, 1410.528793468874483, 231.1058639361037592 ) ) ;
#23703 = CARTESIAN_POINT ( 'NONE',  ( 13.27254556628637872, 1414.941240495251577, 198.0499574059903694 ) ) ;
#23704 = CARTESIAN_POINT ( 'NONE',  ( 14.43085696104800064, 1426.807557148669957, 195.4949581798340148 ) ) ;
#23706 = FACE_OUTER_BOUND ( 'NONE', #60217, .T. ) ;
#23705 = CARTESIAN_POINT ( 'NONE',  ( 11.13334565089999906, 1425.173446693529968, 142.7648904542980119 ) ) ;
#23707 = LINE ( 'NONE', #27581, #17973 ) ;
#23708 = CARTESIAN_POINT ( 'NONE',  ( -7.326141170133179337, 1517.051704409989952, 204.8440844730560002 ) ) ;
#23709 = CARTESIAN_POINT ( 'NONE',  ( -5.334733590569999073, 1453.182326120890139, 200.0999779489789887 ) ) ;
#23710 = CARTESIAN_POINT ( 'NONE',  ( 3.258474578945000033, 1517.083030555940013, 202.5598499717069956 ) ) ;
#23711 = DIRECTION ( 'NONE',  ( 0.3090169943749582204, 0.000000000000000000, 0.9510565162951499785 ) ) ;
#23712 = CARTESIAN_POINT ( 'NONE',  ( -10.21388636078169299, 1398.215752035679088, 201.0479164178328801 ) ) ;
#23713 = CARTESIAN_POINT ( 'NONE',  ( 16.72999343173500009, 1513.736060322960157, 195.1295000578670056 ) ) ;
#23714 = CARTESIAN_POINT ( 'NONE',  ( -18.61832818047690097, 1419.362210733380152, 205.9667898552229985 ) ) ;
#23715 = DIRECTION ( 'NONE',  ( -0.7071067811870476172, 0.000000000000000000, 0.7071067811860475283 ) ) ;
#23716 = CARTESIAN_POINT ( 'NONE',  ( 4.329791490734999471, 1515.051704408389924, 205.7917117663369879 ) ) ;
#23718 = ORIENTED_EDGE ( 'NONE', *, *, #48220, .F. ) ;
#23717 = CARTESIAN_POINT ( 'NONE',  ( -36.47250856561959864, 1379.658678557460007, 223.7669085669769800 ) ) ;
#23719 = ORIENTED_EDGE ( 'NONE', *, *, #24991, .T. ) ;
#23721 = EDGE_CURVE ( 'NONE', #46101, #49402, #25921, .T. ) ;
#23720 = CARTESIAN_POINT ( 'NONE',  ( 11.29216247361090097, 1434.438968647419870, 151.5554298123269916 ) ) ;
#23722 = CARTESIAN_POINT ( 'NONE',  ( -11.88194722309999918, 1396.505120844730072, 211.3071127478679898 ) ) ;
#23723 = CARTESIAN_POINT ( 'NONE',  ( -20.06921834150000095, 1410.974364727830107, 220.7356942897980048 ) ) ;
#23724 = VERTEX_POINT ( 'NONE', #69936 ) ;
#23725 = CARTESIAN_POINT ( 'NONE',  ( -13.15334649152275404, 1444.754287284761403, 169.3979280245720247 ) ) ;
#23726 = CARTESIAN_POINT ( 'NONE',  ( 22.03874496197475708, 1509.704128133699214, 228.9173456134791991 ) ) ;
#23727 = DIRECTION ( 'NONE',  ( 3.828568698926946970E-16, 0.000000000000000000, -1.000000000000000000 ) ) ;
#23729 = CARTESIAN_POINT ( 'NONE',  ( -13.80442745998849929, 1508.531539859030090, 184.0281800264250194 ) ) ;
#23728 = CARTESIAN_POINT ( 'NONE',  ( 0.2567668993620010331, 1444.957971160790066, 199.0403769168990209 ) ) ;
#23730 = CARTESIAN_POINT ( 'NONE',  ( -0.02449593311879999860, 1468.711357958130066, 182.4995022349980047 ) ) ;
#23731 = CARTESIAN_POINT ( 'NONE',  ( -4.748715079035791042, 1463.075537724480000, 200.5807050376280074 ) ) ;
#23732 = CARTESIAN_POINT ( 'NONE',  ( -17.47648986376090008, 1417.884872443149789, 206.9675092925560023 ) ) ;
#23733 = CARTESIAN_POINT ( 'NONE',  ( 9.951016712660660346, 1396.260557557309994, 204.2881766974590221 ) ) ;
#23734 = CARTESIAN_POINT ( 'NONE',  ( 1.249587849179999877, 1415.128105756529976, 191.3153250033980157 ) ) ;
#23735 = CARTESIAN_POINT ( 'NONE',  ( 10.96803698370000113, 1432.243966832229944, 151.7696189413979937 ) ) ;
#23736 = CARTESIAN_POINT ( 'NONE',  ( 8.229600951721646851, 1509.200675254854787, 180.9700133782839941 ) ) ;
#23737 = VERTEX_POINT ( 'NONE', #27341 ) ;
#23738 = CARTESIAN_POINT ( 'NONE',  ( 13.27369308195070019, 1434.899823491839925, 149.1828079990220033 ) ) ;
#23739 = VERTEX_POINT ( 'NONE', #61527 ) ;
#23740 = ORIENTED_EDGE ( 'NONE', *, *, #64067, .F. ) ;
#23741 = CARTESIAN_POINT ( 'NONE',  ( 12.85075015980074298, 1444.958812780512289, 169.4430788496519824 ) ) ;
#23742 = CARTESIAN_POINT ( 'NONE',  ( -7.139643389570000664, 1463.933016855429969, 236.1633026984980006 ) ) ;
#23743 = CARTESIAN_POINT ( 'NONE',  ( -108.4309645088232088, 1388.536554251156758, 310.3699996483296104 ) ) ;
#23744 = CARTESIAN_POINT ( 'NONE',  ( -0.7391220051939990654, 1517.130100026000036, 216.0715493048870144 ) ) ;
#23745 = CARTESIAN_POINT ( 'NONE',  ( -8.394782641223070385, 1511.398921086017026, 213.7356158315847665 ) ) ;
#23746 = EDGE_CURVE ( 'NONE', #1490, #26765, #16700, .T. ) ;
#23747 = EDGE_LOOP ( 'NONE', ( #11255, #77715, #18240, #106247, #18914, #11264, #100383 ) ) ;
#23748 = CARTESIAN_POINT ( 'NONE',  ( -11.74584741039999969, 1503.658473360889957, 208.1214727982489876 ) ) ;
#23749 = CARTESIAN_POINT ( 'NONE',  ( 5.649719750514999639, 1514.243099272629934, 201.4728115316369781 ) ) ;
#23750 = CARTESIAN_POINT ( 'NONE',  ( -19.16011842089999817, 1379.988729378269909, 208.8610751811399950 ) ) ;
#23751 = EDGE_CURVE ( 'NONE', #59795, #18384, #18265, .T. ) ;
#23752 = ORIENTED_EDGE ( 'NONE', *, *, #37154, .T. ) ;
#23753 = CARTESIAN_POINT ( 'NONE',  ( 5.772403774305000290, 1516.676340709600026, 205.8583240277470168 ) ) ;
#23754 = ORIENTED_EDGE ( 'NONE', *, *, #2233, .F. ) ;
#23755 = CARTESIAN_POINT ( 'NONE',  ( 5.781585778145000631, 1516.939646076049939, 209.1093989964429909 ) ) ;
#23756 = CARTESIAN_POINT ( 'NONE',  ( -20.15452302159999931, 1507.845791376729949, 228.9024215066979764 ) ) ;
#23757 = CARTESIAN_POINT ( 'NONE',  ( -35.91967445428193884, 1425.095412615255555, 269.5444895620009902 ) ) ;
#23758 = CARTESIAN_POINT ( 'NONE',  ( 6.844666213235000463, 1512.637906871319728, 217.0439743110670179 ) ) ;
#23760 = ORIENTED_EDGE ( 'NONE', *, *, #13807, .T. ) ;
#23759 = CARTESIAN_POINT ( 'NONE',  ( -1.032249311085239984, 1415.090956648730071, 226.6967784922329940 ) ) ;
#23761 = CARTESIAN_POINT ( 'NONE',  ( 2.500000000000000000, 1432.302110539269961, 157.4936333739979943 ) ) ;
#23762 = CARTESIAN_POINT ( 'NONE',  ( -28.69268220585919948, 1440.913060387330006, 233.8417140319710086 ) ) ;
#23763 = CARTESIAN_POINT ( 'NONE',  ( -49.59998741779999420, 1384.429563225830179, 260.9046511607589878 ) ) ;
#23764 = CARTESIAN_POINT ( 'NONE',  ( -0.07116624666730259063, 1465.436517331040250, 236.3246395822949921 ) ) ;
#23765 = CARTESIAN_POINT ( 'NONE',  ( 8.194407606919998699, 1409.116459709330002, 270.4215667397979814 ) ) ;
#23766 = CARTESIAN_POINT ( 'NONE',  ( -0.7365612166329978949, 1517.066898074209803, 213.7457380308570123 ) ) ;
#23767 = CARTESIAN_POINT ( 'NONE',  ( 23.95176194079999732, 1410.398731527629934, 209.1804549718790156 ) ) ;
#23768 = DIRECTION ( 'NONE',  ( -1.989939052760000051E-13, -6.949020296389990473E-15, 1.000000000000000000 ) ) ;
#23769 = CYLINDRICAL_SURFACE ( 'NONE', #23486, 1.999999999999991562 ) ;
#23770 = CARTESIAN_POINT ( 'NONE',  ( 21.77174004986088462, 1524.860077346005028, 184.6554692728756777 ) ) ;
#23771 = CARTESIAN_POINT ( 'NONE',  ( -4.028611259245000298, 1516.744381837270112, 210.2562039408269925 ) ) ;
#23772 = CARTESIAN_POINT ( 'NONE',  ( -3.189772444258944351, 1447.442977096462073, 154.8380773011854501 ) ) ;
#23773 = CARTESIAN_POINT ( 'NONE',  ( -9.789290102761340151, 1501.631178984691360, 228.6396138205003012 ) ) ;
#23774 = CARTESIAN_POINT ( 'NONE',  ( -6.420950019901092709, 1485.997607280482725, 182.7091661881264884 ) ) ;
#23776 = EDGE_LOOP ( 'NONE', ( #86067, #83605, #102523, #100752, #19125 ) ) ;
#23775 = CARTESIAN_POINT ( 'NONE',  ( -74.54124110130000247, 1388.281602540309905, 277.2607202525589969 ) ) ;
#23777 = CARTESIAN_POINT ( 'NONE',  ( -38.52179989938650095, 1385.190298941179890, 239.5872078768659890 ) ) ;
#23778 = CARTESIAN_POINT ( 'NONE',  ( 18.95862648649999826, 1416.832348283729971, 210.4638202831779950 ) ) ;
#23779 = CARTESIAN_POINT ( 'NONE',  ( 11.76014171143800091, 1479.338753478690023, 208.6264959333659874 ) ) ;
#23780 = CARTESIAN_POINT ( 'NONE',  ( -11.22085813611739979, 1414.913060387329779, 220.6193216859199993 ) ) ;
#23781 = CARTESIAN_POINT ( 'NONE',  ( 4.957272291311130452, 1484.564628183469949, 219.0507141408710083 ) ) ;
#23782 = CARTESIAN_POINT ( 'NONE',  ( -6.119584447340000288, 1461.516739343589961, 206.9548908960190090 ) ) ;
#23783 = CARTESIAN_POINT ( 'NONE',  ( -7.121584071090000023, 1409.161751583130126, 195.9581075130980139 ) ) ;
#23785 = CARTESIAN_POINT ( 'NONE',  ( -8.861530393209999801, 1384.875119385939797, 218.6849572728390285 ) ) ;
#23784 = CARTESIAN_POINT ( 'NONE',  ( -5.004475612664999851, 1517.026025493960105, 216.8437538584669824 ) ) ;
#23786 = CARTESIAN_POINT ( 'NONE',  ( -25.93754856796245889, 1450.779557423562437, 136.7820379074420600 ) ) ;
#23787 = CARTESIAN_POINT ( 'NONE',  ( -3.348648543330357885, 1523.530935881284904, 176.1572159930114196 ) ) ;
#23788 = VERTEX_POINT ( 'NONE', #91107 ) ;
#23789 = CARTESIAN_POINT ( 'NONE',  ( 4.615017327834999961, 1516.987478262539980, 202.5620478758069964 ) ) ;
#23790 = CARTESIAN_POINT ( 'NONE',  ( -15.46083485256500012, 1513.125294087170005, 223.3378070712669796 ) ) ;
#23791 = CARTESIAN_POINT ( 'NONE',  ( 6.520293663361448111, 1509.032998980578441, 216.3821515562998457 ) ) ;
#23792 = CARTESIAN_POINT ( 'NONE',  ( 19.88559295760000012, 1455.744107332229987, 223.8027299929979961 ) ) ;
#23793 = CARTESIAN_POINT ( 'NONE',  ( 10.92329970540940032, 1461.467203400760127, 210.0859975044730277 ) ) ;
#23794 = CARTESIAN_POINT ( 'NONE',  ( 12.51045652733512981, 1414.677402202029953, 211.4999743317719663 ) ) ;
#23795 = CARTESIAN_POINT ( 'NONE',  ( 26.61844847777970813, 1450.722186606933292, 136.4846925697592042 ) ) ;
#23796 = CARTESIAN_POINT ( 'NONE',  ( 15.25750226104648810, 1420.759466697897551, 227.8319051552381609 ) ) ;
#23797 = CARTESIAN_POINT ( 'NONE',  ( 29.70844085274949720, 1436.010927005220083, 136.4302040973799990 ) ) ;
#23798 = CARTESIAN_POINT ( 'NONE',  ( 39.62454033826469413, 1446.691649570389927, 136.6910118460810111 ) ) ;
#23799 = CARTESIAN_POINT ( 'NONE',  ( 20.25058512361396623, 1506.578946199967277, 217.9834787517386587 ) ) ;
#23800 = CARTESIAN_POINT ( 'NONE',  ( -2.616722072391682197, 1475.048391684631042, 269.6500679664175095 ) ) ;
#23801 = CARTESIAN_POINT ( 'NONE',  ( -106.8356828860000007, 1390.011699867550078, 299.6508205978589672 ) ) ;
#23802 = CARTESIAN_POINT ( 'NONE',  ( -17.52239435150000446, 1415.804866261129973, 225.9435871245979968 ) ) ;
#23803 = CARTESIAN_POINT ( 'NONE',  ( -106.1967435559999871, 1391.345933298020100, 301.1341274642589951 ) ) ;
#23804 = CARTESIAN_POINT ( 'NONE',  ( -16.16453978850797313, 1469.071349536585103, 269.3697744449012816 ) ) ;
#23805 = ORIENTED_EDGE ( 'NONE', *, *, #9200, .F. ) ;
#23806 = CARTESIAN_POINT ( 'NONE',  ( -4.074350933259999502E-15, 1428.579607037230062, 149.5143047311979672 ) ) ;
#23807 = CARTESIAN_POINT ( 'NONE',  ( -27.36442814965441173, 1413.476243666040546, 269.4075121043655372 ) ) ;
#23808 = CARTESIAN_POINT ( 'NONE',  ( -3.861663332592479847, 1508.610718243669908, 213.8016401467760090 ) ) ;
#23809 = CARTESIAN_POINT ( 'NONE',  ( -5.443435778090000454, 1484.664955501689974, 199.0097654132990215 ) ) ;
#23810 = B_SPLINE_CURVE_WITH_KNOTS ( 'NONE', 5,
 ( #23172, #92045, #108293, #33233, #7486, #82552 ),
 .UNSPECIFIED., .F., .F.,
 ( 6, 6 ),
 ( 0.000000000000000000, 1.000000000000000000 ),
 .UNSPECIFIED. ) ;
#23811 = CARTESIAN_POINT ( 'NONE',  ( -14.69331829855070026, 1452.091493848030041, 222.9975758587799817 ) ) ;
#23812 = CARTESIAN_POINT ( 'NONE',  ( -13.09515188823569076, 1443.020675217816461, 186.6586876594417106 ) ) ;
#23813 = CARTESIAN_POINT ( 'NONE',  ( -8.638199857644998758, 1437.437583958759888, 209.7090198132510181 ) ) ;
#23814 = CARTESIAN_POINT ( 'NONE',  ( 16.48487877296681248, 1525.795403383247276, 181.7735843130006685 ) ) ;
#23815 = CARTESIAN_POINT ( 'NONE',  ( -4.958998528701818564, 1416.169772216195270, 232.1515073687287156 ) ) ;
#23816 = CARTESIAN_POINT ( 'NONE',  ( -38.12974907660549917, 1444.894042496500106, 137.0546131931990033 ) ) ;
#23817 = FACE_OUTER_BOUND ( 'NONE', #69412, .T. ) ;
#23818 = CARTESIAN_POINT ( 'NONE',  ( -13.20386921870955632, 1443.121265474914935, 169.3907368431102896 ) ) ;
#23820 = ORIENTED_EDGE ( 'NONE', *, *, #24815, .F. ) ;
#23819 = CARTESIAN_POINT ( 'NONE',  ( -14.81131296149999876, 1410.375311526330051, 226.7082462524979860 ) ) ;
#23821 = B_SPLINE_CURVE_WITH_KNOTS ( 'NONE', 3,
 ( #27794, #71502, #97197, #27244, #87151, #70384, #61425, #3175, #104501, #61981, #53575, #96096 ),
 .UNSPECIFIED., .F., .F.,
 ( 4, 2, 2, 2, 2, 4 ),
 ( -0.08068999410833509189, -0.06416485085002331112, -0.04444643289188129898, -0.02282564341193510371, 0.000000000000000000, 0.0003431288226209555647 ),
 .UNSPECIFIED. ) ;
#23822 = CARTESIAN_POINT ( 'NONE',  ( 0.8265315298475599537, 1415.089948427370018, 191.7561489437229909 ) ) ;
#23823 = CARTESIAN_POINT ( 'NONE',  ( -2.573074615509999941, 1409.002914132830028, 231.1540680731980046 ) ) ;
#23824 = ORIENTED_EDGE ( 'NONE', *, *, #16557, .T. ) ;
#23825 = EDGE_LOOP ( 'NONE', ( #14399, #88659, #79143, #52944, #68196, #33111 ) ) ;
#23826 = CARTESIAN_POINT ( 'NONE',  ( 16.66147553287439820, 1414.913057846380070, 209.9988873639480005 ) ) ;
#23827 = DIRECTION ( 'NONE',  ( -1.755985294532469921E-16, 1.000000000000000000, -1.338183447452831989E-16 ) ) ;
#23829 = CARTESIAN_POINT ( 'NONE',  ( -8.166151876880000771, 1461.469839515129934, 225.2410124208979880 ) ) ;
#23828 = CARTESIAN_POINT ( 'NONE',  ( 2.319193188279999873, 1454.536622715790145, 218.2400033011389837 ) ) ;
#23830 = CARTESIAN_POINT ( 'NONE',  ( -6.605784529800000193, 1446.202031244890122, 215.7107487543390221 ) ) ;
#23831 = CARTESIAN_POINT ( 'NONE',  ( -11.88593578010000051, 1433.200405512929819, 150.0669781585979763 ) ) ;
#23832 = DIRECTION ( 'NONE',  ( 5.980589973904019347E-17, -1.000000000000000000, 1.736889445713099699E-16 ) ) ;
#23833 = CARTESIAN_POINT ( 'NONE',  ( -19.23853081770000273, 1466.576780668189940, 213.8528554934590034 ) ) ;
#23834 = CARTESIAN_POINT ( 'NONE',  ( -2.682480990172567470, 1524.330813522192102, 241.8675070349543716 ) ) ;
#23835 = CARTESIAN_POINT ( 'NONE',  ( -24.35601318819999861, 1440.342902236149939, 211.6694219976479872 ) ) ;
#23836 = FACE_BOUND ( 'NONE', #87008, .T. ) ;
#23837 = CARTESIAN_POINT ( 'NONE',  ( 2.086716510760000087, 1452.155719858229986, 183.6328824817980205 ) ) ;
#23838 = CARTESIAN_POINT ( 'NONE',  ( 9.813910351429941059, 1364.017814053639768, 210.6218459616987957 ) ) ;
#23839 = CARTESIAN_POINT ( 'NONE',  ( -27.55294438350654929, 1509.987280990239697, 197.2544469677627887 ) ) ;
#23841 = ORIENTED_EDGE ( 'NONE', *, *, #13815, .F. ) ;
#23840 = CARTESIAN_POINT ( 'NONE',  ( -2.017359258820280141E-09, 1416.045455530739900, 240.6646644973519926 ) ) ;
#23842 = VERTEX_POINT ( 'NONE', #65933 ) ;
#23843 = EDGE_CURVE ( 'NONE', #32285, #81525, #6275, .T. ) ;
#23844 = CARTESIAN_POINT ( 'NONE',  ( -11.79426874074069964, 1427.973425763779915, 147.8794941013190112 ) ) ;
#23845 = CARTESIAN_POINT ( 'NONE',  ( 24.08466742948269967, 1495.842384968879969, 206.9662854201800144 ) ) ;
#23846 = CARTESIAN_POINT ( 'NONE',  ( -6.215218566849999959, 1471.256776971429872, 269.6190395958980162 ) ) ;
#23847 = CARTESIAN_POINT ( 'NONE',  ( -3.657993755839999750, 1474.872004365689918, 218.7367895275489786 ) ) ;
#23848 = CARTESIAN_POINT ( 'NONE',  ( -107.8722023357835695, 1311.832804576487888, 313.5405874544188123 ) ) ;
#23849 = CARTESIAN_POINT ( 'NONE',  ( 40.76353202841180234, 1447.329558407210016, 136.0508387103639905 ) ) ;
#23850 = CARTESIAN_POINT ( 'NONE',  ( 17.70665509759999878, 1431.113060387329824, 202.1814663873780091 ) ) ;
#23851 = CARTESIAN_POINT ( 'NONE',  ( 19.76122774234984192, 1455.648809305226223, 227.1212724839211603 ) ) ;
#23852 = EDGE_CURVE ( 'NONE', #100324, #107049, #100055, .T. ) ;
#23853 = CARTESIAN_POINT ( 'NONE',  ( 19.66678637211940028, 1517.051704408389924, 202.3500283489059939 ) ) ;
#23854 = FACE_OUTER_BOUND ( 'NONE', #90396, .T. ) ;
#23855 = CARTESIAN_POINT ( 'NONE',  ( 10.57963509885960285, 1366.486042548352543, 207.6218459616987673 ) ) ;
#23856 = CARTESIAN_POINT ( 'NONE',  ( -39.51454461767819737, 1423.024700941120045, 268.9460601137379854 ) ) ;
#23857 = ORIENTED_EDGE ( 'NONE', *, *, #11837, .T. ) ;
#23858 = FACE_OUTER_BOUND ( 'NONE', #8322, .T. ) ;
#23859 = EDGE_LOOP ( 'NONE', ( #68084, #964, #21672, #6819 ) ) ;
#23860 = ORIENTED_EDGE ( 'NONE', *, *, #37130, .T. ) ;
#23861 = CARTESIAN_POINT ( 'NONE',  ( -6.546302780145000000, 1516.577434278289957, 211.6089493897669911 ) ) ;
#23862 = CARTESIAN_POINT ( 'NONE',  ( 4.844982144979842253, 1423.488028581556364, 184.1325588144100891 ) ) ;
#23863 = CARTESIAN_POINT ( 'NONE',  ( -21.54905603439506478, 1524.816548299036867, 183.6628006193895430 ) ) ;
#23865 = CARTESIAN_POINT ( 'NONE',  ( -38.61927355701700293, 1444.188087899089851, 137.1592452686400065 ) ) ;
#23864 = CARTESIAN_POINT ( 'NONE',  ( 5.785582913545000316, 1516.981965530290154, 213.1542438721070027 ) ) ;
#23866 = CARTESIAN_POINT ( 'NONE',  ( -17.85129570129999621, 1455.457398219630250, 190.3057806367980049 ) ) ;
#23867 = CARTESIAN_POINT ( 'NONE',  ( -16.75617669327549919, 1479.756059428050094, 228.8978987931039910 ) ) ;
#23868 = ORIENTED_EDGE ( 'NONE', *, *, #37704, .T. ) ;
#23869 = CARTESIAN_POINT ( 'NONE',  ( -113.4000000000000057, 1391.913060387289988, 304.2218459572590064 ) ) ;
#23870 =( BOUNDED_SURFACE ( )  B_SPLINE_SURFACE ( 3, 2, ( 
 ( #49618, #48520, #5950 ),
 ( #83751, #101085, #99990 ),
 ( #91603, #41205, #65323 ),
 ( #99433, #24383, #6495 ),
 ( #13768, #33334, #75375 ),
 ( #109514, #32790, #83206 ) ),
 .UNSPECIFIED., .F., .F., .F. ) 
 B_SPLINE_SURFACE_WITH_KNOTS ( ( 4, 2, 4 ),
 ( 3, 3 ),
 ( -6.288372600415925717E-17, 0.001312027981647218922, 0.002624055963294500728 ),
 ( 0.000000000000000000, 1.000000000000000000 ),
 .UNSPECIFIED. ) 
 GEOMETRIC_REPRESENTATION_ITEM ( )  RATIONAL_B_SPLINE_SURFACE ( (
 ( 1.000000000000000000, 0.9376006582765932240, 1.000000000000000000),
 ( 1.000000000000000000, 0.9569320108025204386, 1.000000000000000000),
 ( 1.000000000000000000, 0.9725743441615498641, 1.000000000000000000),
 ( 1.000000000000000000, 0.9942095667139038140, 1.000000000000000000),
 ( 1.000000000000000000, 1.000043666450451063, 1.000000000000000000),
 ( 1.000000000000000000, 1.000000000000000000, 1.000000000000000000) ) ) 
 REPRESENTATION_ITEM ( '' )  SURFACE ( )  );
#23871 = CARTESIAN_POINT ( 'NONE',  ( 1.124894050234999998, 1517.194816588360027, 202.1703287997270309 ) ) ;
#23872 = CARTESIAN_POINT ( 'NONE',  ( -33.91369114349999592, 1451.728768196330066, 134.7155300131979914 ) ) ;
#23873 = CARTESIAN_POINT ( 'NONE',  ( -40.26705673720950074, 1384.583644506999917, 213.1675334149419996 ) ) ;
#23874 = CARTESIAN_POINT ( 'NONE',  ( -112.2014361534894817, 1391.413060387289988, 302.0278895525330540 ) ) ;
#23875 = DIRECTION ( 'NONE',  ( 0.9977304882603014180, 0.06733403890946067227, 0.000000000000000000 ) ) ;
#23876 = CARTESIAN_POINT ( 'NONE',  ( -6.016808998109999251, 1396.654460029229995, 198.2004533603980008 ) ) ;
#23878 = ORIENTED_EDGE ( 'NONE', *, *, #96295, .T. ) ;
#23877 = CARTESIAN_POINT ( 'NONE',  ( -3.448830483803564828, 1512.187213306747481, 175.1594891075192209 ) ) ;
#23879 = VERTEX_POINT ( 'NONE', #6555 ) ;
#23880 = FACE_OUTER_BOUND ( 'NONE', #66340, .T. ) ;
#23881 = VECTOR ( 'NONE', #21492, 1000.000000000000114 ) ;
#23882 = CARTESIAN_POINT ( 'NONE',  ( 3.749167825016557654, 1425.488083945166409, 185.1890168411832462 ) ) ;
#23883 = CARTESIAN_POINT ( 'NONE',  ( -2.344512381655610156, 1516.526058395550081, 201.4130302485380071 ) ) ;
#23884 = CARTESIAN_POINT ( 'NONE',  ( -24.31979101810000188, 1435.530147504380011, 137.6066080458979854 ) ) ;
#23885 = CARTESIAN_POINT ( 'NONE',  ( -24.67369719190000055, 1441.458996830729802, 210.7025079082280001 ) ) ;
#23886 = CARTESIAN_POINT ( 'NONE',  ( 0.7578857918350010436, 1516.872851364150165, 211.6022732247369902 ) ) ;
#23887 = CARTESIAN_POINT ( 'NONE',  ( -68.76290618570000390, 1379.747985224000104, 280.1898727115589622 ) ) ;
#23888 = CIRCLE ( 'NONE', #13261, 2.000000000000001776 ) ;
#23889 = CARTESIAN_POINT ( 'NONE',  ( -1.908211845303299903, 1484.244220179899912, 182.9087969337900006 ) ) ;
#23890 = CARTESIAN_POINT ( 'NONE',  ( 3.991339022206620069, 1441.662322080260083, 217.1481258823889959 ) ) ;
#23891 = CARTESIAN_POINT ( 'NONE',  ( -19.59884465730793579, 1526.382868172863937, 237.0995590530540937 ) ) ;
#23892 = CARTESIAN_POINT ( 'NONE',  ( 3.251394362135000105, 1516.757508073510053, 207.4061414411269766 ) ) ;
#23893 = EDGE_LOOP ( 'NONE', ( #44659, #36589, #78964, #42056, #57531, #73336, #33131, #63520, #71829, #104338, #56314 ) ) ;
#23894 = CARTESIAN_POINT ( 'NONE',  ( -2.386210315674730076, 1451.954674705370053, 184.6135196128299754 ) ) ;
#23895 = CARTESIAN_POINT ( 'NONE',  ( -10.13788858020000028, 1473.082980680690071, 207.8827380507390217 ) ) ;
#23896 = CARTESIAN_POINT ( 'NONE',  ( -20.28084755118021576, 1456.032803552603809, 224.6711213126964708 ) ) ;
#23897 = ORIENTED_EDGE ( 'NONE', *, *, #91306, .F. ) ;
#23898 = DIRECTION ( 'NONE',  ( -0.7414773880254701410, -2.572516463827778023E-15, -0.6709778558543689764 ) ) ;
#23899 = CARTESIAN_POINT ( 'NONE',  ( -25.78156655170059608, 1509.813372604039841, 223.1298223243570078 ) ) ;
#23900 = B_SPLINE_SURFACE_WITH_KNOTS ( 'NONE', 5, 1, ( 
 ( #93592, #77375 ),
 ( #67885, #8489 ),
 ( #86865, #10157 ),
 ( #68438, #101995 ),
 ( #43768, #7947 ),
 ( #76264, #52730 ),
 ( #51621, #110412 ),
 ( #25280, #35925 ),
 ( #59481, #60034 ),
 ( #9598, #16868 ),
 ( #84649, #95273 ),
 ( #33691, #26399 ),
 ( #1787, #44332 ),
 ( #42116, #43226 ),
 ( #17423, #76817 ) ),
 .UNSPECIFIED., .F., .F., .F.,
 ( 6, 3, 3, 3, 6 ),
 ( 2, 2 ),
 ( 91.71614156710000998, 91.73016858649999961, 144.2269611950000012, 165.2349012489999893, 166.7810826825559900 ),
 ( -7.070755615892880552E-05, 4.740550787240640496 ),
 .UNSPECIFIED. ) ;
#23901 = CARTESIAN_POINT ( 'NONE',  ( -4.070270494153594321, 1440.756896449854594, 185.1152696589734319 ) ) ;
#23902 = CARTESIAN_POINT ( 'NONE',  ( -9.573074595669998743, 1414.882314128850112, 207.6164979793489920 ) ) ;
#23903 = CARTESIAN_POINT ( 'NONE',  ( -11.39059366553855490, 1425.662989886324112, 138.8619651797782808 ) ) ;
#23904 = CARTESIAN_POINT ( 'NONE',  ( 9.374206578739999074, 1489.420254891390186, 201.2494609442489946 ) ) ;
#23905 = CARTESIAN_POINT ( 'NONE',  ( -3.420065937103660136, 1476.688851773250008, 199.3353256554640041 ) ) ;
#23906 = CARTESIAN_POINT ( 'NONE',  ( 24.25228055134414262, 1445.991220302454849, 214.4993191193233883 ) ) ;
#23907 = CARTESIAN_POINT ( 'NONE',  ( -11.96519809220000141, 1440.444625599219989, 147.6189886498980002 ) ) ;
#23908 = CARTESIAN_POINT ( 'NONE',  ( 16.17523441753503022, 1409.477912220330381, 225.6432943692607296 ) ) ;
#23909 = CARTESIAN_POINT ( 'NONE',  ( -7.328049318385000177, 1516.809497469189864, 215.6772390872569929 ) ) ;
#23910 = VERTEX_POINT ( 'NONE', #107357 ) ;
#23911 = CARTESIAN_POINT ( 'NONE',  ( 7.719201501412129574, 1516.922672751009941, 209.0804826056520085 ) ) ;
#23912 = B_SPLINE_SURFACE_WITH_KNOTS ( 'NONE', 5, 5, ( 
 ( #92793, #22810, #41298, #74372, #23378, #58111 ),
 ( #30686, #64872, #91692, #98980, #48614, #83295 ),
 ( #32879, #39646, #40740, #14968, #58657, #31784 ),
 ( #65975, #73815, #100098, #49162, #6590, #16065 ),
 ( #74916, #50268, #109066, #23916, #107943, #24469 ),
 ( #56453, #66527, #67069, #82187, #100631, #101175 ),
 ( #84398, #92244, #49711, #41843, #7685, #107389 ),
 ( #90588, #13865, #5487, #31235, #65418, #99525 ),
 ( #57017, #91142, #14419, #101730, #93885, #53023 ) ),
 .UNSPECIFIED., .F., .F., .F.,
 ( 6, 3, 6 ),
 ( 6, 6 ),
 ( 4.070471747090000036, 8.034185059020000352, 13.29188982760000037 ),
 ( 0.000000000000000000, 2.000000000000000000 ),
 .UNSPECIFIED. ) ;
#23913 = CARTESIAN_POINT ( 'NONE',  ( -16.61546743539999937, 1420.545275466900193, 203.3817927211090080 ) ) ;
#23914 = CARTESIAN_POINT ( 'NONE',  ( 0.5093327223650000457, 1419.917355073230055, 184.4471483751979974 ) ) ;
#23915 = EDGE_CURVE ( 'NONE', #48999, #9907, #104917, .T. ) ;
#23916 = CARTESIAN_POINT ( 'NONE',  ( -1.100961233750000101, 1475.184615464690069, 219.7712113178990023 ) ) ;
#23917 = DIRECTION ( 'NONE',  ( 0.000000000000000000, 1.000000000000000000, -1.836970198721029688E-16 ) ) ;
#23918 = CARTESIAN_POINT ( 'NONE',  ( -7.545177104707559756, 1384.914515597359923, 219.0875873435799974 ) ) ;
#23919 = CARTESIAN_POINT ( 'NONE',  ( -11.31495002440830078, 1471.132454865509999, 207.6217866740839781 ) ) ;
#23920 = DIRECTION ( 'NONE',  ( 0.000000000000000000, -1.000000000000000000, 0.000000000000000000 ) ) ;
#23921 = CARTESIAN_POINT ( 'NONE',  ( 17.71719970781420628, 1423.378758011100444, 226.1827588889887863 ) ) ;
#23922 = ADVANCED_FACE ( 'NONE', ( #49127 ), #55123, .F. ) ;
#23923 = CARTESIAN_POINT ( 'NONE',  ( 0.5238578764187010739, 1455.924360441900035, 198.5814542928440289 ) ) ;
#23924 = LINE ( 'NONE', #48056, #38012 ) ;
#23926 = EDGE_CURVE ( 'NONE', #61077, #94335, #97477, .T. ) ;
#23925 = CARTESIAN_POINT ( 'NONE',  ( 42.45354694711880228, 1440.913060353240098, 262.5200983195459798 ) ) ;
#23928 = CARTESIAN_POINT ( 'NONE',  ( 4.327230971739109755, 1515.149487411880045, 208.7301753859959774 ) ) ;
#23927 = DIRECTION ( 'NONE',  ( 0.000000000000000000, 1.000000000000000000, 0.000000000000000000 ) ) ;
#23929 = DIRECTION ( 'NONE',  ( 0.9455185755993178454, 0.000000000000000000, -0.3255681544571539243 ) ) ;
#23930 = ORIENTED_EDGE ( 'NONE', *, *, #56503, .F. ) ;
#23931 = ORIENTED_EDGE ( 'NONE', *, *, #5811, .T. ) ;
#23932 = DIRECTION ( 'NONE',  ( 0.000000000000000000, 0.000000000000000000, 1.000000000000000000 ) ) ;
#23933 = CARTESIAN_POINT ( 'NONE',  ( -4.775348822359999801, 1443.097051919790147, 200.2639737031189782 ) ) ;
#23934 = CARTESIAN_POINT ( 'NONE',  ( -1.188177861046854300, 1416.835288266028101, 228.1251897816796941 ) ) ;
#23935 = CARTESIAN_POINT ( 'NONE',  ( 20.70484064406403846, 1525.907212628473644, 233.2025904124105580 ) ) ;
#23936 = LINE ( 'NONE', #41864, #100242 ) ;
#23937 = CARTESIAN_POINT ( 'NONE',  ( -0.6435652335515109623, 1508.551704408389924, 220.0605423497629829 ) ) ;
#23938 = CARTESIAN_POINT ( 'NONE',  ( 17.43739734485520998, 1526.178928173328131, 180.7274168163513082 ) ) ;
#23939 = CARTESIAN_POINT ( 'NONE',  ( -42.01758979030880425, 1383.824999389499908, 245.4151092701270045 ) ) ;
#23940 = CARTESIAN_POINT ( 'NONE',  ( -5.110470226864999965, 1511.399604276809896, 200.8758674234269961 ) ) ;
#23941 = CARTESIAN_POINT ( 'NONE',  ( 2.499945006294769900, 1419.401634877229981, 143.2540554854240042 ) ) ;
#23942 = CARTESIAN_POINT ( 'NONE',  ( -27.43651671978516404, 1509.328400563031892, 212.0833630515228378 ) ) ;
#23943 = CARTESIAN_POINT ( 'NONE',  ( 11.08064054948859933, 1491.588519825060075, 210.5260817967020159 ) ) ;
#23945 = EDGE_LOOP ( 'NONE', ( #11816, #67177, #75040, #110809 ) ) ;
#23944 = CARTESIAN_POINT ( 'NONE',  ( 0.08652916374279870371, 1456.779921165790029, 219.3623944633989993 ) ) ;
#23946 = CARTESIAN_POINT ( 'NONE',  ( 34.68852446352672558, 1522.861859112239927, 218.2490599185861697 ) ) ;
#23947 = CARTESIAN_POINT ( 'NONE',  ( -46.58469234310000218, 1379.055167030529901, 234.6844865969590046 ) ) ;
#23948 = CARTESIAN_POINT ( 'NONE',  ( 19.82859500370260264, 1508.459386330439884, 229.4052108613220184 ) ) ;
#23949 = ORIENTED_EDGE ( 'NONE', *, *, #73711, .T. ) ;
#23950 = ORIENTED_EDGE ( 'NONE', *, *, #71279, .T. ) ;
#23951 = EDGE_CURVE ( 'NONE', #40664, #24247, #39034, .T. ) ;
#23952 = CARTESIAN_POINT ( 'NONE',  ( -7.679213435265119791, 1385.492375165610156, 218.9666595514219978 ) ) ;
#23953 = CARTESIAN_POINT ( 'NONE',  ( -3.778541329980729557, 1515.551842520359969, 205.7532489892629997 ) ) ;
#23955 = DIRECTION ( 'NONE',  ( -0.6736849260863841948, 0.000000000000000000, 0.7390186874254148774 ) ) ;
#23954 = CARTESIAN_POINT ( 'NONE',  ( -11.87761131804900039, 1481.971403308739809, 208.7488170094680129 ) ) ;
#23956 = AXIS2_PLACEMENT_3D ( 'NONE', #47063, #29688, #48720 ) ;
#23957 = CARTESIAN_POINT ( 'NONE',  ( 11.76839603954939939, 1479.635942723670041, 209.6667243029050098 ) ) ;
#23958 = CARTESIAN_POINT ( 'NONE',  ( -107.4881158890000137, 1380.862912516779943, 298.8296354258590100 ) ) ;
#23959 = CYLINDRICAL_SURFACE ( 'NONE', #19552, 2.000000000000001776 ) ;
#23960 = CARTESIAN_POINT ( 'NONE',  ( -30.44526109729619989, 1526.211528530236592, 201.0917145515471987 ) ) ;
#23961 = CARTESIAN_POINT ( 'NONE',  ( -16.16605818406190309, 1508.551704408389924, 213.6368797843010157 ) ) ;
#23962 = CARTESIAN_POINT ( 'NONE',  ( 3.347801439296145709, 1523.456872492435195, 176.1543725841967500 ) ) ;
#23963 = CARTESIAN_POINT ( 'NONE',  ( 0.7287763451100000012, 1409.106502167329836, 185.6933822617980070 ) ) ;
#23964 = CARTESIAN_POINT ( 'NONE',  ( 10.65100542576229437, 1461.074092667963441, 226.0091726112900403 ) ) ;
#23965 = CARTESIAN_POINT ( 'NONE',  ( 1.515247566503459931, 1431.991194283580171, 200.7184132697910002 ) ) ;
#23966 = CARTESIAN_POINT ( 'NONE',  ( 11.57646189039999918, 1432.336252720020184, 151.1966908187980039 ) ) ;
#23967 = CIRCLE ( 'NONE', #86571, 1.999999999999961808 ) ;
#23968 = CARTESIAN_POINT ( 'NONE',  ( -2.513809405447149814, 1451.504177376969892, 184.6655415589659981 ) ) ;
#23969 = VERTEX_POINT ( 'NONE', #6002 ) ;
#23970 = CARTESIAN_POINT ( 'NONE',  ( -22.04556278850142093, 1524.082582765195411, 184.4798054120614665 ) ) ;
#23971 = CARTESIAN_POINT ( 'NONE',  ( 18.71713341259120256, 1457.163765172349940, 229.5372674111999913 ) ) ;
#23972 = CARTESIAN_POINT ( 'NONE',  ( -12.98106087750000093, 1435.572631767780194, 150.6458279223980128 ) ) ;
#23973 = CARTESIAN_POINT ( 'NONE',  ( -1.150230247847569986E-08, 1474.257262691309961, 263.8864222916459994 ) ) ;
#23974 = CARTESIAN_POINT ( 'NONE',  ( -13.08802352330000041, 1503.233211745590097, 208.6735908916250253 ) ) ;
#23975 = EDGE_CURVE ( 'NONE', #38998, #17148, #58164, .T. ) ;
#23976 = CARTESIAN_POINT ( 'NONE',  ( 0.9225549254600009519, 1476.549448786289986, 198.3955259652989866 ) ) ;
#23977 = CARTESIAN_POINT ( 'NONE',  ( -108.1428528709999881, 1386.591709523359896, 310.8553624892590506 ) ) ;
#23978 = CARTESIAN_POINT ( 'NONE',  ( -0.1885928293499999908, 1482.195919647529990, 181.9611671400979844 ) ) ;
#23979 = CARTESIAN_POINT ( 'NONE',  ( -9.832966357653941003, 1364.062280235955768, 210.6218459616991936 ) ) ;
#23980 = CARTESIAN_POINT ( 'NONE',  ( 17.01540922059999872, 1497.106364323189837, 222.9636020297990058 ) ) ;
#23981 = CARTESIAN_POINT ( 'NONE',  ( 2.738034649980079838, 1428.914299196640059, 216.9389116324280167 ) ) ;
#23982 = DIRECTION ( 'NONE',  ( 0.9858563016923833633, 0.000000000000000000, 0.1675928173085483863 ) ) ;
#23983 = CARTESIAN_POINT ( 'NONE',  ( 6.938478784765000462, 1516.719999691880048, 208.3679751968140010 ) ) ;
#23984 = DIRECTION ( 'NONE',  ( -0.6736849260863839728, 0.000000000000000000, 0.7390186874254150995 ) ) ;
#23985 = CARTESIAN_POINT ( 'NONE',  ( 1.478250974131940509, 1424.351089761499907, 227.4175086134767128 ) ) ;
#23986 = CARTESIAN_POINT ( 'NONE',  ( 7.466935644698990515, 1425.252733620679919, 212.3145299656949874 ) ) ;
#23987 = ORIENTED_EDGE ( 'NONE', *, *, #12475, .F. ) ;
#23988 = CARTESIAN_POINT ( 'NONE',  ( 24.93072418010000035, 1437.606125426900235, 217.2956629241979840 ) ) ;
#23990 = CARTESIAN_POINT ( 'NONE',  ( -16.19492410690000384, 1409.478599599030076, 194.0661808922979787 ) ) ;
#23989 = CARTESIAN_POINT ( 'NONE',  ( 1.467228651769999948, 1489.039472797129974, 181.9015832661979744 ) ) ;
#23991 = DIRECTION ( 'NONE',  ( -1.000000000000000000, 0.000000000000000000, 0.000000000000000000 ) ) ;
#23992 = SPHERICAL_SURFACE ( 'NONE', #8549, 2.000000000000000000 ) ;
#23993 = CARTESIAN_POINT ( 'NONE',  ( -28.36433000254718806, 1509.903564542218646, 201.4659584704413930 ) ) ;
#23994 = CARTESIAN_POINT ( 'NONE',  ( -9.826464246318440843, 1452.569912694470077, 150.6692168550179929 ) ) ;
#23995 = DIRECTION ( 'NONE',  ( 0.9455185755993178454, 0.000000000000000000, -0.3255681544571537578 ) ) ;
#23996 = EDGE_LOOP ( 'NONE', ( #64985, #64138, #5480, #7366 ) ) ;
#23997 = DIRECTION ( 'NONE',  ( 0.8672669759446726134, -7.800054970605876826E-15, 0.4978433412588572637 ) ) ;
#23998 = CARTESIAN_POINT ( 'NONE',  ( -0.6192548831692870070, 1407.650904249920131, 270.1377146676910002 ) ) ;
#23999 = CARTESIAN_POINT ( 'NONE',  ( 15.95518007350070100, 1422.893326400530214, 228.6357347565129885 ) ) ;
#24000 = CARTESIAN_POINT ( 'NONE',  ( 9.677596946179999549, 1463.237936564790061, 210.5383604994590030 ) ) ;
#24001 = ORIENTED_EDGE ( 'NONE', *, *, #93987, .F. ) ;
#24002 = ORIENTED_EDGE ( 'NONE', *, *, #77360, .T. ) ;
#24003 = CARTESIAN_POINT ( 'NONE',  ( -46.09372478569999743, 1384.870670475119823, 219.0248111663489965 ) ) ;
#24004 = CARTESIAN_POINT ( 'NONE',  ( -23.74908638290310137, 1410.154450923110062, 208.9152455597699998 ) ) ;
#24005 = EDGE_CURVE ( 'NONE', #110100, #110607, #8741, .T. ) ;
#24006 = CARTESIAN_POINT ( 'NONE',  ( -4.273589427560000154, 1425.970440093729849, 186.1370899423980063 ) ) ;
#24007 = CARTESIAN_POINT ( 'NONE',  ( -12.49103604210455387, 1436.447564085543263, 151.1284240868977520 ) ) ;
#24008 = CARTESIAN_POINT ( 'NONE',  ( -6.861707994109999653, 1428.078401598830169, 112.4493539157979995 ) ) ;
#24009 = EDGE_CURVE ( 'NONE', #82014, #96593, #38271, .T. ) ;
#24010 = CARTESIAN_POINT ( 'NONE',  ( -2.474406870190000163, 1507.640282505830100, 236.9531809319980198 ) ) ;
#24011 = CARTESIAN_POINT ( 'NONE',  ( -19.90339844620000065, 1415.851102572129776, 221.6293417451979906 ) ) ;
#24012 = ORIENTED_EDGE ( 'NONE', *, *, #63496, .T. ) ;
#24013 = CARTESIAN_POINT ( 'NONE',  ( 44.63527855443649628, 1449.973421542959841, 268.2561587561260126 ) ) ;
#24014 = CARTESIAN_POINT ( 'NONE',  ( -10.56579291990400016, 1391.913060387269979, 204.9477986745440319 ) ) ;
#24015 = CARTESIAN_POINT ( 'NONE',  ( -0.05142771962049999535, 1419.751625371630098, 184.3796591070980071 ) ) ;
#24016 = CARTESIAN_POINT ( 'NONE',  ( 2.865911516645000212, 1516.906233342200039, 205.6598507734169914 ) ) ;
#24017 = ORIENTED_EDGE ( 'NONE', *, *, #29949, .F. ) ;
#24018 = CARTESIAN_POINT ( 'NONE',  ( 18.37125585514824166, 1459.035043778956151, 227.7538859344645061 ) ) ;
#24019 = CARTESIAN_POINT ( 'NONE',  ( -0.2511677605985540018, 1444.763459584839893, 199.0663387163230027 ) ) ;
#24020 = DIRECTION ( 'NONE',  ( -0.8023110876747339137, -0.5969061220947440294, 0.000000000000000000 ) ) ;
#24021 = VERTEX_POINT ( 'NONE', #56704 ) ;
#24022 = CARTESIAN_POINT ( 'NONE',  ( 4.987082680427550763, 1508.551704408389924, 205.8487925209399805 ) ) ;
#24023 = CARTESIAN_POINT ( 'NONE',  ( 5.428693282926851715, 1434.565645669088553, 202.5455567000074950 ) ) ;
#24024 = CARTESIAN_POINT ( 'NONE',  ( -12.57832850835009886, 1512.205851781539877, 194.0924024796699996 ) ) ;
#24025 = CARTESIAN_POINT ( 'NONE',  ( 10.06093830045220194, 1503.068099882679917, 216.9326386128159925 ) ) ;
#24026 = CARTESIAN_POINT ( 'NONE',  ( 8.268376058639999471, 1421.225653048179993, 196.1217719269989743 ) ) ;
#24028 = B_SPLINE_SURFACE_WITH_KNOTS ( 'NONE', 5, 5, ( 
 ( #25011, #85469, #8216, #95002, #50262, #110140, #51904, #44053, #33413 ),
 ( #51334, #67061, #68175, #59756, #33980, #17700, #24461, #84391, #59212 ),
 ( #7678, #41834, #75990, #86044, #93331, #18270, #16594, #93877, #110689 ),
 ( #50791, #84923, #43504, #25563, #42381, #8768, #77648, #42949, #77108 ),
 ( #416, #34534, #26677, #68716, #962, #69267, #26115, #103373, #60876 ),
 ( #95548, #78754, #37857, #45729, #35635, #106160, #19372, #72043, #11552 ),
 ( #29437, #63636, #20470, #69829, #96664, #62543, #18821, #36749, #97750 ),
 ( #12650, #19935, #105621, #45172, #46828, #44612, #2069, #2623, #79313 ),
 ( #1504, #79865, #55225, #103946, #10440, #54131, #21021, #89355, #11000 ) ),
 .UNSPECIFIED., .F., .F., .F.,
 ( 6, 3, 6 ),
 ( 6, 3, 6 ),
 ( 1.119759084200000032, 3.314659481400000107, 6.273351219260000278 ),
 ( 0.000000000000000000, 1.000000000000000000, 2.000000000000000000 ),
 .UNSPECIFIED. ) ;
#24027 = LINE ( 'NONE', #16183, #15530 ) ;
#24029 = CARTESIAN_POINT ( 'NONE',  ( -4.855393136690000055, 1495.916459891889872, 198.8750123678989894 ) ) ;
#24030 = CIRCLE ( 'NONE', #59888, 2.000000000000003109 ) ;
#24031 = CARTESIAN_POINT ( 'NONE',  ( 4.577122560907209703, 1409.072897029190017, 187.7508653761969981 ) ) ;
#24033 = FACE_OUTER_BOUND ( 'NONE', #83322, .T. ) ;
#24032 = CARTESIAN_POINT ( 'NONE',  ( -13.78070311828070160, 1434.978583006209874, 148.5586138787649872 ) ) ;
#24034 = CARTESIAN_POINT ( 'NONE',  ( 10.94058267569030107, 1425.550681174790043, 206.5022529322419871 ) ) ;
#24035 = CARTESIAN_POINT ( 'NONE',  ( -11.70763562119999968, 1378.584671346379992, 213.2295515425790029 ) ) ;
#24036 = ADVANCED_FACE ( 'NONE', ( #81885 ), #24071, .T. ) ;
#24037 = AXIS2_PLACEMENT_3D ( 'NONE', #96814, #105210, #20085 ) ;
#24038 = CARTESIAN_POINT ( 'NONE',  ( 11.59417695439999996, 1428.981093279630159, 133.6118001900980232 ) ) ;
#24039 = VERTEX_POINT ( 'NONE', #73518 ) ;
#24040 = CARTESIAN_POINT ( 'NONE',  ( 12.21873817507339943, 1415.431750870119913, 222.0592676625429931 ) ) ;
#24041 = CIRCLE ( 'NONE', #102694, 2.000007000530037882 ) ;
#24042 = CARTESIAN_POINT ( 'NONE',  ( -1.925297170580940076, 1517.151704408390060, 187.5582988486569889 ) ) ;
#24043 = CARTESIAN_POINT ( 'NONE',  ( 13.13561839920527063, 1517.151704408390060, 209.9352119836111683 ) ) ;
#24044 = B_SPLINE_SURFACE_WITH_KNOTS ( 'NONE', 5, 5, ( 
 ( #86376, #67951, #8556, #35426, #102060, #69613 ),
 ( #27034, #95337, #18598, #24784, #58986, #93113 ),
 ( #16384, #25342, #42175, #70177, #56511, #47554 ),
 ( #29095, #78540, #80601, #97393, #104288, #38047 ),
 ( #63280, #20663, #107991, #35989, #4453, #30175 ),
 ( #12832, #10220, #22308, #72224, #44398, #5545 ) ),
 .UNSPECIFIED., .F., .F., .F.,
 ( 6, 6 ),
 ( 6, 6 ),
 ( 5.893388896111249942, 9.819930328988748514 ),
 ( -0.0002947352087483990084, 0.5000000000000000000 ),
 .UNSPECIFIED. ) ;
#24045 = EDGE_CURVE ( 'NONE', #68144, #26609, #95581, .T. ) ;
#24046 = CARTESIAN_POINT ( 'NONE',  ( -11.98665338999999896, 1391.172375739130075, 205.5831304284690191 ) ) ;
#24047 = CARTESIAN_POINT ( 'NONE',  ( 9.996610684277881020, 1422.882004021880221, 210.0220379297240072 ) ) ;
#24048 = CARTESIAN_POINT ( 'NONE',  ( 10.95736455730619952, 1423.486173266069954, 203.2510385470160088 ) ) ;
#24049 = EDGE_CURVE ( 'NONE', #96085, #50916, #52974, .T. ) ;
#24050 = CARTESIAN_POINT ( 'NONE',  ( -10.94864045059309987, 1462.689136093790239, 207.6212922226960131 ) ) ;
#24051 = CARTESIAN_POINT ( 'NONE',  ( -34.97756117329999626, 1449.243413927999882, 262.6648722463980334 ) ) ;
#24052 = CARTESIAN_POINT ( 'NONE',  ( -21.38849015939615583, 1509.000358152776244, 191.8600543660001279 ) ) ;
#24053 = CARTESIAN_POINT ( 'NONE',  ( -12.78752272590105932, 1416.843574538714392, 195.5392800691490152 ) ) ;
#24054 = CARTESIAN_POINT ( 'NONE',  ( 34.84383450159999285, 1453.969943368129861, 265.6112250856980381 ) ) ;
#24055 = B_SPLINE_SURFACE_WITH_KNOTS ( 'NONE', 5, 5, ( 
 ( #65863, #17472, #14872, #49064, #49610, #6487 ),
 ( #7039, #41197, #51673, #725, #34855, #69044 ),
 ( #26447, #73719, #107842, #79644, #70164, #103718 ),
 ( #105943, #19135, #10774, #77965, #54453, #60641 ),
 ( #61209, #86916, #104276, #2401, #86363, #1273 ),
 ( #27563, #70712, #104826, #87487, #35412, #1839 ),
 ( #53339, #61747, #9644, #96430, #43819, #62303 ),
 ( #95869, #44946, #69600, #79093, #78528, #71823 ),
 ( #27020, #52780, #36519, #28112, #11872, #95323 ) ),
 .UNSPECIFIED., .F., .F., .F.,
 ( 6, 3, 6 ),
 ( 6, 6 ),
 ( 24.00348385615980007, 27.60499227840000103, 32.18191237814389893 ),
 ( -0.008403786540223459611, 2.000000000000000000 ),
 .UNSPECIFIED. ) ;
#24057 = ADVANCED_FACE ( 'NONE', ( #107096 ), #5753, .F. ) ;
#24056 = CARTESIAN_POINT ( 'NONE',  ( 12.82280136232900070, 1414.971993471380074, 197.7189074864900249 ) ) ;
#24058 = CARTESIAN_POINT ( 'NONE',  ( 0.4435541702111918672, 1467.106087704137963, 235.5928625124542179 ) ) ;
#24059 = CARTESIAN_POINT ( 'NONE',  ( 0.1144963318970000088, 1419.768049673130008, 184.3728032279979914 ) ) ;
#24060 = CARTESIAN_POINT ( 'NONE',  ( 0.000000000000000000, 1512.187213306747481, 209.1218459616979999 ) ) ;
#24061 = ADVANCED_FACE ( 'NONE', ( #64576 ), #65114, .F. ) ;
#24062 = CARTESIAN_POINT ( 'NONE',  ( -19.01829945129999899, 1486.473597083029972, 189.2492686670979936 ) ) ;
#24063 = CARTESIAN_POINT ( 'NONE',  ( -1.376928043298434101, 1517.051704408389924, 226.4861182474958525 ) ) ;
#24064 = CARTESIAN_POINT ( 'NONE',  ( -17.68901833540000013, 1410.027722936829832, 224.9019810024979904 ) ) ;
#24065 = CARTESIAN_POINT ( 'NONE',  ( 23.04597175290000166, 1410.910372357130200, 213.3277098939479686 ) ) ;
#24066 = EDGE_CURVE ( 'NONE', #90388, #58309, #5918, .T. ) ;
#24067 = CARTESIAN_POINT ( 'NONE',  ( -26.69006509299999763, 1449.954382144920146, 136.5854975036980079 ) ) ;
#24068 = CARTESIAN_POINT ( 'NONE',  ( 4.806901123144410257E-05, 1416.181292948460168, 209.1218310849390036 ) ) ;
#24069 = CARTESIAN_POINT ( 'NONE',  ( 0.7508624519860009894, 1515.469918561890154, 204.9042454670689892 ) ) ;
#24070 = CARTESIAN_POINT ( 'NONE',  ( -2.686147501205827570, 1526.329757971589515, 176.3936480404082374 ) ) ;
#24071 = CONICAL_SURFACE ( 'NONE', #11709, 26.99999999999998934, 0.2186689458740001812 ) ;
#24072 = CARTESIAN_POINT ( 'NONE',  ( 20.10528725740779876, 1430.878053006679920, 215.1856555508250040 ) ) ;
#24074 = EDGE_CURVE ( 'NONE', #51033, #76907, #56406, .T. ) ;
#24073 = CARTESIAN_POINT ( 'NONE',  ( -12.37274144529999909, 1415.932840167130053, 221.9815654478979923 ) ) ;
#24075 = AXIS2_PLACEMENT_3D ( 'NONE', #23234, #41152, #75861 ) ;
#24076 = CARTESIAN_POINT ( 'NONE',  ( 0.1705841116430650006, 1479.986583045490079, 182.0949671867700204 ) ) ;
#24078 = ORIENTED_EDGE ( 'NONE', *, *, #87815, .T. ) ;
#24077 = CARTESIAN_POINT ( 'NONE',  ( 0.01096404850135499973, 1407.225809182730018, 222.1218459625830235 ) ) ;
#24079 = CARTESIAN_POINT ( 'NONE',  ( -20.75326766870000128, 1444.324653571829913, 176.0807405191980024 ) ) ;
#24080 = CYLINDRICAL_SURFACE ( 'NONE', #53341, 1.500000000000001332 ) ;
#24081 = CARTESIAN_POINT ( 'NONE',  ( 12.06088154280000069, 1433.903722001979986, 149.6992425274980008 ) ) ;
#24082 = CARTESIAN_POINT ( 'NONE',  ( -41.37151551560999962, 1441.555306591699946, 134.0999999980749919 ) ) ;
#24083 = CARTESIAN_POINT ( 'NONE',  ( -110.0629570050000012, 1384.907242112629774, 296.9512948280589626 ) ) ;
#24084 = ORIENTED_EDGE ( 'NONE', *, *, #53583, .F. ) ;
#24086 = EDGE_CURVE ( 'NONE', #19741, #16403, #82456, .T. ) ;
#24085 = CARTESIAN_POINT ( 'NONE',  ( -1.119918677100000037, 1484.477289159689917, 198.4557079161989748 ) ) ;
#24087 = CARTESIAN_POINT ( 'NONE',  ( -113.4000000000000057, 1391.413060387289988, 304.2218459572590064 ) ) ;
#24088 = CARTESIAN_POINT ( 'NONE',  ( -103.6552259873821100, 1379.945806083001571, 305.1021558360112635 ) ) ;
#24089 = EDGE_CURVE ( 'NONE', #41219, #101100, #6128, .T. ) ;
#24090 = CARTESIAN_POINT ( 'NONE',  ( 6.768931428559999297, 1468.810414616219987, 208.2491176692980162 ) ) ;
#24091 = CARTESIAN_POINT ( 'NONE',  ( -108.3926162938884801, 1381.231319549018281, 310.3369704220332892 ) ) ;
#24092 = CARTESIAN_POINT ( 'NONE',  ( 22.16059216520000419, 1489.466620110430085, 210.4454289069080062 ) ) ;
#24093 = LINE ( 'NONE', #66696, #18145 ) ;
#24094 = CARTESIAN_POINT ( 'NONE',  ( -57.85475636940380184, 1385.051150463449858, 239.4744903710780193 ) ) ;
#24095 = CARTESIAN_POINT ( 'NONE',  ( -11.57078835683859985, 1391.913060387289988, 210.5928294217469841 ) ) ;
#24096 = CARTESIAN_POINT ( 'NONE',  ( 12.35725348643379995, 1421.674275332549996, 207.8249747856479814 ) ) ;
#24097 = EDGE_CURVE ( 'NONE', #68962, #37552, #39463, .T. ) ;
#24098 = CARTESIAN_POINT ( 'NONE',  ( 11.87502392341400004, 1433.007271648830056, 149.9804723818110119 ) ) ;
#24099 = CARTESIAN_POINT ( 'NONE',  ( -16.61545066670979764, 1410.583136789100081, 226.4812420948509839 ) ) ;
#24101 = ORIENTED_EDGE ( 'NONE', *, *, #24941, .T. ) ;
#24100 = CARTESIAN_POINT ( 'NONE',  ( 10.11781796957937551, 1428.435797280887527, 134.0999999980966777 ) ) ;
#24102 = FACE_OUTER_BOUND ( 'NONE', #43455, .T. ) ;
#24103 = CARTESIAN_POINT ( 'NONE',  ( 18.20623948849710061, 1429.807643283219932, 209.5135666361939855 ) ) ;
#24104 = CARTESIAN_POINT ( 'NONE',  ( -109.9744337340000016, 1384.497115240790208, 311.4392815102590362 ) ) ;
#24105 = CARTESIAN_POINT ( 'NONE',  ( -2.664535259099999805E-15, 1424.786834349990158, 209.1218459616989946 ) ) ;
#24106 = DIRECTION ( 'NONE',  ( 0.000000000000000000, 0.000000000000000000, -1.000000000000000000 ) ) ;
#24107 = CARTESIAN_POINT ( 'NONE',  ( -11.60004870196338445, 1428.704565730935656, 134.1356168154925967 ) ) ;
#24108 = CARTESIAN_POINT ( 'NONE',  ( -17.20364854680000377, 1422.328583322830127, 226.7282386093980051 ) ) ;
#24109 = CARTESIAN_POINT ( 'NONE',  ( -2.983385501069631740, 1512.076650117638792, 201.2296962218204328 ) ) ;
#24110 = DIRECTION ( 'NONE',  ( 0.8809280347472114858, -0.3866361631380628161, 0.2729070811655368578 ) ) ;
#24111 = CARTESIAN_POINT ( 'NONE',  ( -120.4682768577266927, 1368.558218059088176, 292.3061701549587497 ) ) ;
#24112 = CARTESIAN_POINT ( 'NONE',  ( 14.59882275810000074, 1475.513060387329915, 225.1032622602980098 ) ) ;
#24113 = AXIS2_PLACEMENT_3D ( 'NONE', #69939, #52568, #36853 ) ;
#24114 = CARTESIAN_POINT ( 'NONE',  ( -1.491852088959999989, 1457.030208651289740, 199.7005471962389720 ) ) ;
#24115 = CARTESIAN_POINT ( 'NONE',  ( 2.865588684285000021, 1516.890356958860139, 205.8536102114670143 ) ) ;
#24116 = CARTESIAN_POINT ( 'NONE',  ( 2.707337067620000148, 1447.195466848630076, 162.7581449801980114 ) ) ;
#24117 = ORIENTED_EDGE ( 'NONE', *, *, #95878, .F. ) ;
#24118 = AXIS2_PLACEMENT_3D ( 'NONE', #20232, #89644, #54433 ) ;
#24119 = CARTESIAN_POINT ( 'NONE',  ( -109.1329681763050132, 1384.757089681630077, 311.2614977992300282 ) ) ;
#24121 = B_SPLINE_CURVE_WITH_KNOTS ( 'NONE', 5,
 ( #9578, #58902, #102524, #101976, #85185, #7928 ),
 .UNSPECIFIED., .F., .F.,
 ( 6, 6 ),
 ( 171.9180602750000162, 176.6690472260000035 ),
 .UNSPECIFIED. ) ;
#24120 = CARTESIAN_POINT ( 'NONE',  ( -0.1681676274470000065, 1420.473121337229941, 182.7663689088979879 ) ) ;
#24123 = ORIENTED_EDGE ( 'NONE', *, *, #17086, .F. ) ;
#24122 = CARTESIAN_POINT ( 'NONE',  ( -68.53711315337859844, 1379.747442305619870, 280.1339386914270335 ) ) ;
#24124 = CARTESIAN_POINT ( 'NONE',  ( -8.564985822174367769, 1381.538787820967173, 218.1048692684619539 ) ) ;
#24125 = ORIENTED_EDGE ( 'NONE', *, *, #80371, .F. ) ;
#24126 = CARTESIAN_POINT ( 'NONE',  ( -16.78503329099363839, 1513.553906385462142, 222.3493531866972148 ) ) ;
#24127 = CARTESIAN_POINT ( 'NONE',  ( 12.68801089449999964, 1500.413651719489962, 208.6561537547790124 ) ) ;
#24129 = CARTESIAN_POINT ( 'NONE',  ( 15.79865788131630211, 1409.472960598209966, 192.7589945538530003 ) ) ;
#24128 = CARTESIAN_POINT ( 'NONE',  ( -8.623178441291070584, 1441.178012937099993, 153.8582158015130119 ) ) ;
#24130 = CARTESIAN_POINT ( 'NONE',  ( -3.251394400264999707, 1516.757508073510053, 210.8375504612070017 ) ) ;
#24131 = EDGE_CURVE ( 'NONE', #84814, #17947, #45710, .T. ) ;
#24132 = CARTESIAN_POINT ( 'NONE',  ( 39.44884039036110579, 1439.526606209990177, 136.6633719441740027 ) ) ;
#24133 = B_SPLINE_SURFACE_WITH_KNOTS ( 'NONE', 5, 5, ( 
 ( #72942, #45008, #46109, #80240, #71330, #107080 ),
 ( #55056, #28732, #61813, #53971, #45562, #97049 ),
 ( #20312, #3559, #71886, #108175, #108734, #65648 ),
 ( #66760, #92466, #40972, #99764, #57262, #74046 ),
 ( #100333, #109299, #15737, #74598, #98677, #30918 ),
 ( #32025, #49938, #13549, #73501, #32584, #91390 ) ),
 .UNSPECIFIED., .F., .F., .F.,
 ( 6, 6 ),
 ( 6, 6 ),
 ( 0.000000000000000000, 0.5294136330519999545 ),
 ( 0.000000000000000000, 2.000000000000000000 ),
 .UNSPECIFIED. ) ;
#24134 = CARTESIAN_POINT ( 'NONE',  ( 33.91369110979999846, 1435.681798629080049, 135.0664268281979901 ) ) ;
#24135 = CARTESIAN_POINT ( 'NONE',  ( -3.829620088063210748, 1515.551704408389696, 212.3304832847908017 ) ) ;
#24136 = CARTESIAN_POINT ( 'NONE',  ( 16.99003759221664467, 1460.417638315011573, 228.7506697972868039 ) ) ;
#24137 = APPLICATION_PROTOCOL_DEFINITION ( 'draft international standard', 'automotive_design', 1998, #70655 ) ;
#24138 = CARTESIAN_POINT ( 'NONE',  ( 4.983582722859440040, 1508.551704408389924, 211.7624053699070146 ) ) ;
#24139 = DIRECTION ( 'NONE',  ( 0.000000000000000000, 0.000000000000000000, -1.000000000000000000 ) ) ;
#24140 = ORIENTED_EDGE ( 'NONE', *, *, #67197, .T. ) ;
#24141 = CARTESIAN_POINT ( 'NONE',  ( 19.12715434829999950, 1496.834837384790035, 222.0421819495990121 ) ) ;
#24142 = DIRECTION ( 'NONE',  ( -0.9455185755993178454, 0.000000000000000000, 0.3255681544571539243 ) ) ;
#24143 = ORIENTED_EDGE ( 'NONE', *, *, #78062, .F. ) ;
#24144 = VERTEX_POINT ( 'NONE', #84090 ) ;
#24145 = CARTESIAN_POINT ( 'NONE',  ( -29.49847430838659079, 1509.954514606188013, 211.0666888197964397 ) ) ;
#24146 = CARTESIAN_POINT ( 'NONE',  ( 13.42479616400980014, 1453.338203267170002, 224.7140346886050111 ) ) ;
#24147 = EDGE_CURVE ( 'NONE', #85990, #96481, #103721, .T. ) ;
#24148 = CARTESIAN_POINT ( 'NONE',  ( -5.943657091278290672, 1507.986285603529950, 220.5847158657419982 ) ) ;
#24149 = CARTESIAN_POINT ( 'NONE',  ( -18.42841025093079921, 1508.451658788899977, 209.8501139522570043 ) ) ;
#24150 = CARTESIAN_POINT ( 'NONE',  ( 4.261736551909999449, 1515.372048949689997, 210.9648081929590262 ) ) ;
#24151 = CARTESIAN_POINT ( 'NONE',  ( -27.69670323179999727, 1508.056852025029912, 205.9292566894080210 ) ) ;
#24152 = CARTESIAN_POINT ( 'NONE',  ( 42.60628464300240381, 1443.705283383309961, 135.3769922593340027 ) ) ;
#24153 = CARTESIAN_POINT ( 'NONE',  ( 12.78776258895000062, 1416.851343899079893, 222.7045348340550106 ) ) ;
#24154 = AXIS2_PLACEMENT_3D ( 'NONE', #86481, #9776, #43943 ) ;
#24155 = CARTESIAN_POINT ( 'NONE',  ( 25.58202537360000051, 1438.616865385849906, 137.7521160916980136 ) ) ;
#24156 = CARTESIAN_POINT ( 'NONE',  ( -11.50315952000000053, 1391.841514381249908, 212.6496336906789963 ) ) ;
#24157 = CARTESIAN_POINT ( 'NONE',  ( -85.15111601059649615, 1384.818475995900144, 288.8775456395259766 ) ) ;
#24158 = ORIENTED_EDGE ( 'NONE', *, *, #83473, .F. ) ;
#24159 = CARTESIAN_POINT ( 'NONE',  ( -6.554764199395000546, 1516.786099423779888, 201.4062207291269999 ) ) ;
#24160 = CARTESIAN_POINT ( 'NONE',  ( 7.326072144144999854, 1516.714320817460020, 208.3685457967989976 ) ) ;
#24161 = ORIENTED_EDGE ( 'NONE', *, *, #39751, .T. ) ;
#24162 = CARTESIAN_POINT ( 'NONE',  ( 11.82387352787750068, 1429.526484542929893, 149.2201243832210196 ) ) ;
#24163 = EDGE_CURVE ( 'NONE', #63442, #15989, #102309, .T. ) ;
#24164 = CARTESIAN_POINT ( 'NONE',  ( 3.294745913766051082, 1511.738168994502985, 217.0981794534744722 ) ) ;
#24165 = EDGE_LOOP ( 'NONE', ( #89231, #102520, #108476, #65526 ) ) ;
#24166 = CARTESIAN_POINT ( 'NONE',  ( -13.20846943169999932, 1414.988017870030035, 220.4537675474979892 ) ) ;
#24167 = CARTESIAN_POINT ( 'NONE',  ( -11.24996134802339931, 1432.343754011389819, 151.5214230697959863 ) ) ;
#24168 = CARTESIAN_POINT ( 'NONE',  ( -2.382436964801009083, 1426.901689560119166, 137.0999999980979567 ) ) ;
#24169 = CIRCLE ( 'NONE', #86772, 7.500000000000000000 ) ;
#24170 = CARTESIAN_POINT ( 'NONE',  ( -9.957211913627739719, 1462.411460094509948, 206.9659526157329879 ) ) ;
#24171 = CARTESIAN_POINT ( 'NONE',  ( -12.80774462770000000, 1422.978431755830115, 222.2455730111979904 ) ) ;
#24172 = EDGE_CURVE ( 'NONE', #87558, #3107, #31362, .T. ) ;
#24173 = CYLINDRICAL_SURFACE ( 'NONE', #63860, 9.999999999999992895 ) ;
#24174 = CARTESIAN_POINT ( 'NONE',  ( -10.03141690779999884, 1472.765117886789994, 207.2972482850190090 ) ) ;
#24175 = CARTESIAN_POINT ( 'NONE',  ( 7.459255098270000772, 1492.932273812890116, 217.3740738590289823 ) ) ;
#24176 = CARTESIAN_POINT ( 'NONE',  ( -60.00250937820000274, 1379.736434133900048, 261.8124847885590043 ) ) ;
#24177 = CARTESIAN_POINT ( 'NONE',  ( 24.64805363261919879, 1458.278292896679886, 206.2167562891609975 ) ) ;
#24179 = CARTESIAN_POINT ( 'NONE',  ( -13.72981806390609805, 1507.304744983219962, 190.9530748769740285 ) ) ;
#24178 = CARTESIAN_POINT ( 'NONE',  ( 12.05130385160000017, 1461.808810158830056, 233.1312125915980005 ) ) ;
#24180 = LINE ( 'NONE', #57288, #23618 ) ;
#24181 = B_SPLINE_SURFACE_WITH_KNOTS ( 'NONE', 5, 5, ( 
 ( #45560, #88650, #3556, #61810, #70226, #38220 ),
 ( #27624, #53396, #36576, #19767, #95932, #62362 ),
 ( #97047, #87545, #37128, #29275, #11927, #45005 ),
 ( #79149, #80236, #4095, #3006, #29820, #2460 ),
 ( #46657, #78583, #105999, #72402, #46107, #64009 ),
 ( #79701, #97586, #70774, #104885, #89181, #98120 ) ),
 .UNSPECIFIED., .F., .F., .F.,
 ( 6, 6 ),
 ( 6, 6 ),
 ( 0.9325643087039999779, 1.051317469700000062 ),
 ( 0.000000000000000000, 2.000000000000000000 ),
 .UNSPECIFIED. ) ;
#24182 = CARTESIAN_POINT ( 'NONE',  ( 4.616861508414999093, 1516.666407245520077, 216.8343369232169948 ) ) ;
#24183 = ORIENTED_EDGE ( 'NONE', *, *, #44668, .F. ) ;
#24184 = CARTESIAN_POINT ( 'NONE',  ( -22.67879459162747224, 1409.704991073136853, 209.2849360770794362 ) ) ;
#24185 = CYLINDRICAL_SURFACE ( 'NONE', #58942, 33.13701971169416538 ) ;
#24186 = CARTESIAN_POINT ( 'NONE',  ( 0.6913041155385422076, 1516.736466343139227, 216.8361714852529190 ) ) ;
#24187 = CARTESIAN_POINT ( 'NONE',  ( 2.296124850935000072, 1516.677239312369920, 213.7299927514870319 ) ) ;
#24188 = EDGE_CURVE ( 'NONE', #88662, #35462, #27566, .T. ) ;
#24189 = CARTESIAN_POINT ( 'NONE',  ( 4.020407408656390125, 1515.375307573260216, 212.6641671072679856 ) ) ;
#24190 =( BOUNDED_SURFACE ( )  B_SPLINE_SURFACE ( 3, 2, ( 
 ( #106107, #29384, #4204 ),
 ( #20424, #63049, #22060 ),
 ( #46228, #80361, #90385 ),
 ( #13664, #47853, #81987 ),
 ( #37805, #22607, #3677 ),
 ( #71451, #107756, #31039 ) ),
 .UNSPECIFIED., .F., .F., .F. ) 
 B_SPLINE_SURFACE_WITH_KNOTS ( ( 4, 2, 4 ),
 ( 3, 3 ),
 ( -2.168404344971008868E-17, 0.001312027981647318452, 0.002624055963294658587 ),
 ( 0.000000000000000000, 1.000000000000000000 ),
 .UNSPECIFIED. ) 
 GEOMETRIC_REPRESENTATION_ITEM ( )  RATIONAL_B_SPLINE_SURFACE ( (
 ( 1.000000000000000000, 0.9376006582765917807, 1.000000000000000000),
 ( 1.000000000000000000, 0.9569320108023516847, 1.000000000000000000),
 ( 1.000000000000000000, 0.9725743441617671348, 1.000000000000000000),
 ( 1.000000000000000000, 0.9942095667136823245, 1.000000000000000000),
 ( 1.000000000000000000, 1.000043666450618485, 1.000000000000000000),
 ( 1.000000000000000000, 1.000000000000000000, 1.000000000000000000) ) ) 
 REPRESENTATION_ITEM ( '' )  SURFACE ( )  );
#24191 = CARTESIAN_POINT ( 'NONE',  ( -11.19085206853407399, 1425.281374859042899, 138.5667630678716762 ) ) ;
#24193 = ORIENTED_EDGE ( 'NONE', *, *, #108, .T. ) ;
#24192 = CARTESIAN_POINT ( 'NONE',  ( -12.39813691047029920, 1501.849957302749999, 211.5949719684760169 ) ) ;
#24194 = CARTESIAN_POINT ( 'NONE',  ( -15.59626543754127859, 1415.697927852701469, 209.6280133318726371 ) ) ;
#24195 = CARTESIAN_POINT ( 'NONE',  ( -15.52481283598960005, 1507.483738429079949, 192.3367673041059902 ) ) ;
#24196 = EDGE_CURVE ( 'NONE', #39431, #66581, #100876, .T. ) ;
#24197 = CARTESIAN_POINT ( 'NONE',  ( -11.72037271900000022, 1428.748239199529962, 149.7340254384980085 ) ) ;
#24198 = CARTESIAN_POINT ( 'NONE',  ( 3.335053448420000066, 1435.130189762789996, 227.2785100434990113 ) ) ;
#24199 = CARTESIAN_POINT ( 'NONE',  ( -109.7733655239769917, 1383.592504427309905, 311.3137736610110551 ) ) ;
#24200 = CARTESIAN_POINT ( 'NONE',  ( -18.31482527320000031, 1445.278739201789904, 204.5307550449689984 ) ) ;
#24201 = CARTESIAN_POINT ( 'NONE',  ( -8.214410069903289369, 1425.179819099440010, 204.7529498726069903 ) ) ;
#24202 = CARTESIAN_POINT ( 'NONE',  ( 4.989246313819999834, 1471.909539260290103, 189.7082128665990126 ) ) ;
#24203 = EDGE_CURVE ( 'NONE', #8701, #15055, #6356, .T. ) ;
#24205 = CARTESIAN_POINT ( 'NONE',  ( -11.49997733492739904, 1482.708633644570000, 206.0163858927470244 ) ) ;
#24204 = CARTESIAN_POINT ( 'NONE',  ( -20.38765208069999701, 1482.730053243030170, 226.6937557411979753 ) ) ;
#24206 = CARTESIAN_POINT ( 'NONE',  ( -1.725662463189999940, 1484.236887840130066, 182.7463278878979906 ) ) ;
#24207 = EDGE_LOOP ( 'NONE', ( #1683, #59032, #94516, #12132 ) ) ;
#24208 = CARTESIAN_POINT ( 'NONE',  ( 4.609673241434999902, 1516.754149861460064, 205.8564388142570181 ) ) ;
#24209 = CARTESIAN_POINT ( 'NONE',  ( 12.67286678700000024, 1407.348457837030082, 268.9829868799980090 ) ) ;
#24210 = CARTESIAN_POINT ( 'NONE',  ( -32.38845792001066570, 1523.456924617338927, 216.1254071227721170 ) ) ;
#24211 = CARTESIAN_POINT ( 'NONE',  ( 22.58665416150000027, 1410.868456648429856, 206.5931427415680162 ) ) ;
#24212 = EDGE_CURVE ( 'NONE', #25949, #108859, #25989, .T. ) ;
#24213 = CARTESIAN_POINT ( 'NONE',  ( 6.121052152493825282, 1506.452631422901959, 230.2562301517164656 ) ) ;
#24214 = VECTOR ( 'NONE', #8813, 1000.000000000000000 ) ;
#24215 = CARTESIAN_POINT ( 'NONE',  ( 3.782892722810800468, 1454.105688421529976, 217.7082469129449862 ) ) ;
#24216 = CARTESIAN_POINT ( 'NONE',  ( -1.835536234179999893, 1450.383119663930074, 182.7750508583980036 ) ) ;
#24217 = CARTESIAN_POINT ( 'NONE',  ( -19.16951723229999871, 1456.627470220629903, 228.8719212425980061 ) ) ;
#24218 = CARTESIAN_POINT ( 'NONE',  ( -10.76610293753739889, 1461.751116445120033, 211.3389343603909936 ) ) ;
#24219 = CARTESIAN_POINT ( 'NONE',  ( -13.59113641329999922, 1444.764193666879919, 188.0077009021979961 ) ) ;
#24220 = CARTESIAN_POINT ( 'NONE',  ( -13.92102725570000032, 1408.913060387329779, 221.6645303301980050 ) ) ;
#24221 = CARTESIAN_POINT ( 'NONE',  ( -8.644357649085678830, 1437.214323335709878, 209.1429500785100117 ) ) ;
#24222 = CARTESIAN_POINT ( 'NONE',  ( -5.363702833240000523, 1497.797094973989942, 219.9207493420989863 ) ) ;
#24223 = CARTESIAN_POINT ( 'NONE',  ( 1.459768879727899815, 1496.155829132160079, 181.5912509448299943 ) ) ;
#24224 = DIRECTION ( 'NONE',  ( -1.643460219210440075E-32, 1.000000000000000000, -6.123233995736769734E-17 ) ) ;
#24225 = EDGE_CURVE ( 'NONE', #69831, #20553, #110245, .T. ) ;
#24226 = CARTESIAN_POINT ( 'NONE',  ( 11.36285630521358136, 1425.645385257877024, 138.6334011581851087 ) ) ;
#24227 = CARTESIAN_POINT ( 'NONE',  ( 34.18677586421187442, 1524.726013923371283, 219.7932833225211482 ) ) ;
#24228 = CARTESIAN_POINT ( 'NONE',  ( -3.767832703549999884, 1475.866516295129941, 267.2290101134979636 ) ) ;
#24229 = B_SPLINE_CURVE_WITH_KNOTS ( 'NONE', 5,
 ( #40597, #84790, #16468, #49021, #74768, #93197 ),
 .UNSPECIFIED., .F., .F.,
 ( 6, 6 ),
 ( -84.90067530929999862, -19.14976305689999947 ),
 .UNSPECIFIED. ) ;
#24230 = CARTESIAN_POINT ( 'NONE',  ( -4.240954185389510300, 1446.390260568540043, 162.6730374057570145 ) ) ;
#24231 = CARTESIAN_POINT ( 'NONE',  ( -14.30569713659541620, 1514.201165865805024, 192.5944094235600801 ) ) ;
#24232 = EDGE_CURVE ( 'NONE', #27509, #63858, #96992, .T. ) ;
#24233 = DIRECTION ( 'NONE',  ( -0.6736849260863841948, 0.000000000000000000, 0.7390186874254148774 ) ) ;
#24234 = CARTESIAN_POINT ( 'NONE',  ( -51.53422708892170334, 1384.732738490049996, 264.8871901791150094 ) ) ;
#24235 = CARTESIAN_POINT ( 'NONE',  ( -106.8411176217500014, 1391.913060387289988, 302.0741137023289298 ) ) ;
#24236 = CARTESIAN_POINT ( 'NONE',  ( 12.12507211432840037, 1416.051481377749951, 223.4385051997479934 ) ) ;
#24237 = FACE_OUTER_BOUND ( 'NONE', #61136, .T. ) ;
#24238 = CARTESIAN_POINT ( 'NONE',  ( -18.66420869458074705, 1526.382868172864164, 185.4599087859683095 ) ) ;
#24239 = FACE_OUTER_BOUND ( 'NONE', #80929, .T. ) ;
#24240 = AXIS2_PLACEMENT_3D ( 'NONE', #39423, #96585, #46201 ) ;
#24241 = CARTESIAN_POINT ( 'NONE',  ( -16.87240674950000141, 1409.502257814230006, 196.1298176688979993 ) ) ;
#24242 = B_SPLINE_CURVE_WITH_KNOTS ( 'NONE', 5,
 ( #38554, #80023, #3344, #12254, #47529, #81650 ),
 .UNSPECIFIED., .F., .F.,
 ( 6, 6 ),
 ( 0.000000000000000000, 1.000000000000000000 ),
 .UNSPECIFIED. ) ;
#24243 = CARTESIAN_POINT ( 'NONE',  ( -8.536583043757159928, 1382.467666485138807, 200.0783688444290362 ) ) ;
#24244 = CARTESIAN_POINT ( 'NONE',  ( -15.08289094651999918, 1422.396364341253729, 228.4054957403699859 ) ) ;
#24245 = CARTESIAN_POINT ( 'NONE',  ( -40.43468551219999796, 1425.927552745930143, 269.7751466411979777 ) ) ;
#24246 = B_SPLINE_CURVE_WITH_KNOTS ( 'NONE', 3,
 ( #40178, #25977, #34404, #76969, #60176, #94293, #68577, #31770, #103237, #32336, #66516, #100082, #25423, #51771, #18684, #17571, #78060, #23366, #8633, #85907, #91679, #94864, #69133, #65957, #83281, #108487, #9212, #74902, #57556, #43372, #61303, #6579, #27118 ),
 .UNSPECIFIED., .F., .F.,
 ( 4, 2, 2, 2, 1, 1, 2, 2, 1, 2, 2, 2, 2, 2, 1, 1, 2, 2, 4 ),
 ( 0.000000000000000000, 0.1249999999959629515, 0.2499999999919259031, 0.3124999999898815939, 0.3203124999895942127, 0.3242187499894761404, 0.3261718749894179648, 0.3281249999893598446, 0.3437499999896028724, 0.3749999999900890391, 0.4999999999921616034, 0.5624999999931965533, 0.5703124999933014694, 0.5742187499933539829, 0.5781249999934063855, 0.5937499999936258765, 0.6249999999940646367, 0.7499999999959944263, 1.000000000000000000 ),
 .UNSPECIFIED. ) ;
#24247 = VERTEX_POINT ( 'NONE', #52717 ) ;
#24248 = CARTESIAN_POINT ( 'NONE',  ( -4.304798037349998904E-15, 1432.353341358199941, 150.3995506339979897 ) ) ;
#24249 = CARTESIAN_POINT ( 'NONE',  ( -17.44087122180000193, 1443.080660932889941, 219.4520116906990097 ) ) ;
#24250 = CARTESIAN_POINT ( 'NONE',  ( 13.12775437374511078, 1414.913060581095351, 198.1894658563514895 ) ) ;
#24251 = AXIS2_PLACEMENT_3D ( 'NONE', #39596, #73769, #31185 ) ;
#24252 = CARTESIAN_POINT ( 'NONE',  ( -9.104803454178981070, 1421.479062530849887, 192.1853131694120123 ) ) ;
#24254 = CARTESIAN_POINT ( 'NONE',  ( -2.487935098691028912, 1508.731359868551181, 204.5668839584545537 ) ) ;
#24253 = CARTESIAN_POINT ( 'NONE',  ( 11.41672989679999972, 1425.493523444330094, 142.7646581281979934 ) ) ;
#24255 = CARTESIAN_POINT ( 'NONE',  ( 17.19739463999655982, 1525.960063244516959, 236.2603809477409698 ) ) ;
#24256 = DIRECTION ( 'NONE',  ( 2.491197269910784929E-47, 1.000000000000000000, -1.836970198721029688E-16 ) ) ;
#24257 = CARTESIAN_POINT ( 'NONE',  ( 10.23405869452090045, 1451.409005433660013, 206.7712507236010140 ) ) ;
#24258 = B_SPLINE_CURVE_WITH_KNOTS ( 'NONE', 3,
 ( #73695, #88270, #37870, #90457, #97761, #107266, #21033, #64751, #63110, #98862, #22126, #11563, #47919, #82054, #97209, #5360, #107821, #31109, #45739, #20482, #88818, #12104, #14299, #75343, #91576, #5920, #83717, #76422, #99955, #42272, #109484, #23796, #40066, #65838, #74245, #100518, #23250, #110576, #67497, #110026, #66944, #58537, #31657, #57448, #14849, #92662, #49040, #83176, #49586, #84267, #50673, #56879, #33302, #6466, #33861, #84806, #32761, #48488, #24885, #40615, #108375, #101601, #93215, #16484 ),
 .UNSPECIFIED., .F., .F.,
 ( 4, 2, 2, 1, 1, 1, 1, 1, 2, 2, 2, 2, 2, 1, 1, 1, 2, 2, 2, 2, 1, 1, 2, 2, 2, 2, 2, 2, 1, 1, 1, 2, 2, 2, 1, 1, 1, 2, 2, 4 ),
 ( 0.000000000000000000, 0.03124999999978876619, 0.04687499999969505643, 0.05468749999965903663, 0.05859374999963078839, 0.06054687499962693037, 0.06152343749961597386, 0.06201171874962137232, 0.06225585937461416280, 0.06249999999960695329, 0.09374999999852183519, 0.1093749999979896359, 0.1171874999977146059, 0.1210937499975777709, 0.1230468749975153486, 0.1240234374974771847, 0.1245117187474644865, 0.1249999999974517884, 0.1406249999974463760, 0.1484374999974328035, 0.1523437499974131804, 0.1542968749974160114, 0.1552734374974319986, 0.1562499999974480136, 0.1874999999975305587, 0.2187499999976131315, 0.2499999999976956766, 0.3749999999979625742, 0.4374999999980880294, 0.4687499999981594723, 0.4843749999981943888, 0.4921874999982117638, 0.4999999999982291943, 0.6249999999985961230, 0.6874999999987861932, 0.7187499999988812283, 0.7343749999989280797, 0.7421874999989571675, 0.7499999999989861443, 1.000000000000000000 ),
 .UNSPECIFIED. ) ;
#24259 = CARTESIAN_POINT ( 'NONE',  ( -11.83466398157531962, 1519.551704408389924, 228.0588040458438286 ) ) ;
#24260 = CARTESIAN_POINT ( 'NONE',  ( -3.457266643525000127, 1516.691414181030041, 203.3491180233569935 ) ) ;
#24261 = CARTESIAN_POINT ( 'NONE',  ( -18.51436573157398513, 1512.187213306747481, 181.1015051776554969 ) ) ;
#24262 = CARTESIAN_POINT ( 'NONE',  ( -11.89217588495976230, 1398.265670798425390, 203.8704783742946063 ) ) ;
#24263 = CARTESIAN_POINT ( 'NONE',  ( 16.20130417443500193, 1512.842772631639946, 197.8702892259670136 ) ) ;
#24264 = CARTESIAN_POINT ( 'NONE',  ( -22.52609270459879909, 1509.699688878229836, 190.3921826462719764 ) ) ;
#24265 = CARTESIAN_POINT ( 'NONE',  ( -7.468813707570000737, 1377.075590846060095, 211.4935550762889989 ) ) ;
#24266 = CARTESIAN_POINT ( 'NONE',  ( 20.67662342439280110, 1509.571223683380140, 229.8561361637509890 ) ) ;
#24268 = ORIENTED_EDGE ( 'NONE', *, *, #80073, .F. ) ;
#24267 = CARTESIAN_POINT ( 'NONE',  ( -52.29426375968220242, 1379.697094711749969, 249.9767541960729886 ) ) ;
#24269 = VERTEX_POINT ( 'NONE', #9584 ) ;
#24270 = CARTESIAN_POINT ( 'NONE',  ( 11.44586080288440044, 1434.091157437989978, 151.3988925854559966 ) ) ;
#24271 = CARTESIAN_POINT ( 'NONE',  ( -2.609101932360000209, 1396.541851151430137, 221.5905290407980033 ) ) ;
#24272 = ORIENTED_EDGE ( 'NONE', *, *, #48064, .T. ) ;
#24273 = CARTESIAN_POINT ( 'NONE',  ( -105.5253899740000065, 1379.039621664339847, 305.7477329845589793 ) ) ;
#24274 = CARTESIAN_POINT ( 'NONE',  ( -27.34571021120000012, 1509.867993630230103, 198.7006099054979700 ) ) ;
#24275 = CARTESIAN_POINT ( 'NONE',  ( 4.082778200585179817, 1515.071394777460000, 205.5355244017910081 ) ) ;
#24277 = CARTESIAN_POINT ( 'NONE',  ( 17.01314077800000035, 1421.695136730729928, 226.8095292698980074 ) ) ;
#24276 = CARTESIAN_POINT ( 'NONE',  ( 0.2645265605250010088, 1443.121736177289904, 200.2023345980989859 ) ) ;
#24278 = CARTESIAN_POINT ( 'NONE',  ( 19.68479608726639896, 1507.817797212230062, 229.3453755810369898 ) ) ;
#24279 = CARTESIAN_POINT ( 'NONE',  ( 13.95127933429999878, 1449.229478364299894, 189.0411395998980311 ) ) ;
#24280 = CARTESIAN_POINT ( 'NONE',  ( -12.16691017849999845, 1415.934222461130048, 194.8513043958980120 ) ) ;
#24281 = CARTESIAN_POINT ( 'NONE',  ( 42.28244370419900378, 1440.913053795810129, 269.8809842699980095 ) ) ;
#24282 =( LENGTH_UNIT ( ) NAMED_UNIT ( * ) SI_UNIT ( .MILLI., .METRE. ) );
#24283 = B_SPLINE_CURVE_WITH_KNOTS ( 'NONE', 3,
 ( #51623, #86316, #61160, #109870, #76821, #34258, #101997, #26401, #93594, #9058, #16870, #9600, #43770, #60594, #85203, #679, #43229, #41569, #49968, #42664, #17425, #68440, #95277, #69551, #103672 ),
 .UNSPECIFIED., .F., .F.,
 ( 4, 3, 3, 3, 3, 3, 3, 3, 4 ),
 ( -1.000000000000000000, -0.7382082361762160039, -0.4751161948289650550, -0.2112166304481060131, 0.05257943943730047920, 0.3138547044834778532, 0.5710709172084329488, 0.8195866995882130634, 1.000000000000000000 ),
 .UNSPECIFIED. ) ;
#24284 = CARTESIAN_POINT ( 'NONE',  ( 2.723978590149899848, 1396.008183815759821, 198.4466560475439962 ) ) ;
#24285 = CARTESIAN_POINT ( 'NONE',  ( 1.433831019619999925, 1415.263254653229978, 191.0530033739979956 ) ) ;
#24286 = CARTESIAN_POINT ( 'NONE',  ( 10.95713523929999944, 1431.451756866380038, 151.7157163214980073 ) ) ;
#24287 = CARTESIAN_POINT ( 'NONE',  ( 8.429098512467547266, 1509.207532371149455, 181.0372478593424148 ) ) ;
#24288 = VERTEX_POINT ( 'NONE', #10709 ) ;
#24289 = CARTESIAN_POINT ( 'NONE',  ( 13.08462178706889922, 1434.901236159169912, 149.6929169018040113 ) ) ;
#24290 = EDGE_LOOP ( 'NONE', ( #60287, #108769 ) ) ;
#24291 = ORIENTED_EDGE ( 'NONE', *, *, #21895, .T. ) ;
#24292 = CARTESIAN_POINT ( 'NONE',  ( 13.29125253233012849, 1444.599725294718382, 169.3795554700696755 ) ) ;
#24293 = CARTESIAN_POINT ( 'NONE',  ( -12.54330649829999977, 1461.761650172629743, 231.4481574644979958 ) ) ;
#24294 = CARTESIAN_POINT ( 'NONE',  ( -107.6660152849997587, 1389.491633112957743, 309.6288604638345419 ) ) ;
#24295 = CARTESIAN_POINT ( 'NONE',  ( -2.871580426725000024, 1517.129577905929864, 216.0720609035170128 ) ) ;
#24296 = CARTESIAN_POINT ( 'NONE',  ( -8.510911714697881436, 1511.398736650778574, 214.0857784337908356 ) ) ;
#24297 = B_SPLINE_CURVE_WITH_KNOTS ( 'NONE', 5,
 ( #71250, #88037, #17042, #20786, #26010, #60207, #105373, #94326, #33877 ),
 .UNSPECIFIED., .F., .F.,
 ( 6, 3, 6 ),
 ( 0.000000000000000000, 0.4555160169310293328, 1.000000000000000000 ),
 .UNSPECIFIED. ) ;
#24298 = VERTEX_POINT ( 'NONE', #44880 ) ;
#24299 = CARTESIAN_POINT ( 'NONE',  ( -11.92597359959999892, 1502.382029717889964, 208.7016622767430079 ) ) ;
#24300 = CARTESIAN_POINT ( 'NONE',  ( 13.86092937120069912, 1410.765486813650114, 191.1266627561969926 ) ) ;
#24301 = CARTESIAN_POINT ( 'NONE',  ( -7.543040680839999901, 1380.366160257679894, 209.1218465795010104 ) ) ;
#24302 = VECTOR ( 'NONE', #40705, 1000.000000000000000 ) ;
#24303 = VECTOR ( 'NONE', #29921, 1000.000000000000000 ) ;
#24304 = VERTEX_POINT ( 'NONE', #70094 ) ;
#24305 = CARTESIAN_POINT ( 'NONE',  ( -6.561995998525000040, 1517.083030555940013, 205.8633713531569924 ) ) ;
#24306 = ORIENTED_EDGE ( 'NONE', *, *, #94927, .F. ) ;
#24307 = CARTESIAN_POINT ( 'NONE',  ( -1.906501101195560124E-08, 1517.020990152690047, 209.1218459511669892 ) ) ;
#24308 = CARTESIAN_POINT ( 'NONE',  ( -20.07277539240000053, 1508.598349472430073, 229.2502111213980243 ) ) ;
#24309 = CARTESIAN_POINT ( 'NONE',  ( -4.246424122129999645, 1409.061348784629899, 187.8200628337979765 ) ) ;
#24310 = CARTESIAN_POINT ( 'NONE',  ( -0.8350686643532178044, 1524.382868172863937, 240.9330574173806951 ) ) ;
#24312 = ORIENTED_EDGE ( 'NONE', *, *, #107681, .T. ) ;
#24311 = CARTESIAN_POINT ( 'NONE',  ( -0.8770414022454380287, 1414.913057846380070, 225.7833214945719931 ) ) ;
#24313 = CARTESIAN_POINT ( 'NONE',  ( 24.26322120380000058, 1437.059134594650232, 214.0566016570280112 ) ) ;
#24314 = CARTESIAN_POINT ( 'NONE',  ( -15.89125153416810043, 1508.551704408389924, 210.3764243748509841 ) ) ;
#24315 = CARTESIAN_POINT ( 'NONE',  ( -76.10119759110000359, 1384.646775243249976, 301.2182732922589707 ) ) ;
#24316 = DIRECTION ( 'NONE',  ( 0.000000000000000000, 1.000000000000000000, 0.000000000000000000 ) ) ;
#24317 = CARTESIAN_POINT ( 'NONE',  ( 14.72001629658930000, 1412.288675752429981, 269.3627518331180113 ) ) ;
#24318 = CARTESIAN_POINT ( 'NONE',  ( 3.458526497885000328, 1516.742629295279812, 214.1194197574270106 ) ) ;
#24319 = CARTESIAN_POINT ( 'NONE',  ( 24.11835951289999969, 1410.845629426529968, 209.1806383628220090 ) ) ;
#24320 = CIRCLE ( 'NONE', #24397, 1.999999999999998668 ) ;
#24321 = DIRECTION ( 'NONE',  ( -0.7414773880254761362, 0.000000000000000000, -0.6709778558543624261 ) ) ;
#24322 = CARTESIAN_POINT ( 'NONE',  ( 2.833473913299999758, 1441.452951622389946, 218.6297931320189889 ) ) ;
#24323 = DIRECTION ( 'NONE',  ( 0.000000000000000000, 0.000000000000000000, -1.000000000000000000 ) ) ;
#24324 = CARTESIAN_POINT ( 'NONE',  ( -4.608417544644999531, 1516.691389976299888, 211.6120918846570191 ) ) ;
#24325 = CARTESIAN_POINT ( 'NONE',  ( 9.477234549875239722, 1434.583635821490134, 206.7094033099960200 ) ) ;
#24326 = CARTESIAN_POINT ( 'NONE',  ( 17.55396644409023210, 1524.816548299036867, 180.7601981288415800 ) ) ;
#24327 = DIRECTION ( 'NONE',  ( 0.000000000000000000, -1.000000000000000000, 1.836970198721029688E-16 ) ) ;
#24329 = ORIENTED_EDGE ( 'NONE', *, *, #49553, .F. ) ;
#24328 = CARTESIAN_POINT ( 'NONE',  ( -55.00753619759999680, 1390.789904819489948, 252.7470035923590217 ) ) ;
#24330 = CARTESIAN_POINT ( 'NONE',  ( -49.49710368664120352, 1385.125075197469869, 260.6903207721879312 ) ) ;
#24331 = EDGE_CURVE ( 'NONE', #94097, #57348, #101047, .T. ) ;
#24332 = CARTESIAN_POINT ( 'NONE',  ( 36.81313714009999671, 1443.228346759079841, 254.5659540772979881 ) ) ;
#24333 = EDGE_CURVE ( 'NONE', #5019, #36878, #56928, .T. ) ;
#24334 = CARTESIAN_POINT ( 'NONE',  ( -4.457338102780003197, 1370.468904865611648, 209.2786786533806946 ) ) ;
#24335 =( BOUNDED_SURFACE ( )  B_SPLINE_SURFACE ( 3, 2, ( 
 ( #3857, #81614, #29569 ),
 ( #38518, #30675, #39634 ),
 ( #97867, #46409, #72697 ),
 ( #98426, #3303, #13852 ) ),
 .UNSPECIFIED., .F., .F., .F. ) 
 B_SPLINE_SURFACE_WITH_KNOTS ( ( 4, 4 ),
 ( 3, 3 ),
 ( 0.000000000000000000, 0.0002960034161023843515 ),
 ( 0.000000000000000000, 1.000000000000000000 ),
 .UNSPECIFIED. ) 
 GEOMETRIC_REPRESENTATION_ITEM ( )  RATIONAL_B_SPLINE_SURFACE ( (
 ( 1.000000000000000000, 0.8072480644198151145, 1.000000000000000000),
 ( 1.000000000000000000, 0.8072480346917711991, 1.000000000000000000),
 ( 1.000000000000000000, 0.8071723757218373096, 1.000000000000000000),
 ( 1.000000000000000000, 0.8070209408749986491, 1.000000000000000000) ) ) 
 REPRESENTATION_ITEM ( '' )  SURFACE ( )  );
#24336 = CARTESIAN_POINT ( 'NONE',  ( -1.334110822913096461, 1494.791028558611742, 220.2012359351212183 ) ) ;
#24337 = CARTESIAN_POINT ( 'NONE',  ( 6.140260223881050194, 1484.047191686760016, 218.4413122911290088 ) ) ;
#24338 = CARTESIAN_POINT ( 'NONE',  ( -2.896892187767880156, 1484.263391075600111, 183.3160938869699805 ) ) ;
#24339 = CARTESIAN_POINT ( 'NONE',  ( -1.073559340110749938, 1444.993510080170154, 218.0402162255370229 ) ) ;
#24341 = CARTESIAN_POINT ( 'NONE',  ( -7.545020166129999595, 1384.905783835959937, 219.0876432053290159 ) ) ;
#24340 = FACE_OUTER_BOUND ( 'NONE', #94915, .T. ) ;
#24342 = CARTESIAN_POINT ( 'NONE',  ( -9.134223394739478863, 1449.159919330089906, 209.9164564190560043 ) ) ;
#24343 = CARTESIAN_POINT ( 'NONE',  ( -9.196349486490200675, 1522.051704408389924, 203.7768694350468195 ) ) ;
#24344 = ORIENTED_EDGE ( 'NONE', *, *, #10750, .F. ) ;
#24345 = CARTESIAN_POINT ( 'NONE',  ( -6.944231786295000042, 1516.882690742909972, 202.5683215544970039 ) ) ;
#24346 = CARTESIAN_POINT ( 'NONE',  ( 7.112123167431945170, 1509.032357809081304, 215.8638901911494941 ) ) ;
#24347 = EDGE_CURVE ( 'NONE', #98527, #64698, #42090, .T. ) ;
#24348 = CARTESIAN_POINT ( 'NONE',  ( 23.15697666530000021, 1449.648812153099925, 217.7024929164979881 ) ) ;
#24349 = CARTESIAN_POINT ( 'NONE',  ( 10.95484118540970009, 1461.213211890040157, 209.4073241984519882 ) ) ;
#24350 = CARTESIAN_POINT ( 'NONE',  ( 4.653713395369999617, 1466.070346627889876, 218.6934685164889913 ) ) ;
#24351 = CARTESIAN_POINT ( 'NONE',  ( 3.920879176457659820, 1439.701872010520219, 184.6839060028229937 ) ) ;
#24352 = CARTESIAN_POINT ( 'NONE',  ( 29.18245906658470190, 1435.992869682629816, 136.4456868839280048 ) ) ;
#24353 = CARTESIAN_POINT ( 'NONE',  ( 40.23461572603999059, 1444.564027027749944, 137.0370437261450149 ) ) ;
#24354 = CARTESIAN_POINT ( 'NONE',  ( -23.26537802140000011, 1433.866345638330131, 213.9181200823180120 ) ) ;
#24355 = CARTESIAN_POINT ( 'NONE',  ( -41.51616159369314829, 1455.119240858822195, 269.0887759631816607 ) ) ;
#24356 = CARTESIAN_POINT ( 'NONE',  ( -109.0713608260000029, 1386.631206999619735, 297.4104235875589666 ) ) ;
#24357 = CARTESIAN_POINT ( 'NONE',  ( 10.82611846040000003, 1509.291116774529883, 182.2978684798979998 ) ) ;
#24358 = CARTESIAN_POINT ( 'NONE',  ( 4.449447964721140458, 1507.123567759500020, 219.9414455400390125 ) ) ;
#24359 = CARTESIAN_POINT ( 'NONE',  ( -15.04391461419485054, 1469.400883903268323, 269.3648501238604922 ) ) ;
#24360 = ORIENTED_EDGE ( 'NONE', *, *, #41288, .F. ) ;
#24361 = CARTESIAN_POINT ( 'NONE',  ( -9.526144281750038800, 1440.436505751970117, 205.9995517796429851 ) ) ;
#24362 = CARTESIAN_POINT ( 'NONE',  ( 5.456719627610000067, 1455.595244131089885, 218.2350948550090095 ) ) ;
#24363 = LINE ( 'NONE', #25457, #98558 ) ;
#24364 = CARTESIAN_POINT ( 'NONE',  ( 15.89604526242030147, 1474.706294885379975, 189.1248889691710247 ) ) ;
#24365 = CARTESIAN_POINT ( 'NONE',  ( -0.009098396902059999528, 1417.355061407530002, 235.2087950155979854 ) ) ;
#24366 = CARTESIAN_POINT ( 'NONE',  ( -29.75012120250000081, 1509.993914124430148, 208.5595671623779879 ) ) ;
#24367 = ADVANCED_FACE ( 'NONE', ( #44317 ), #52029, .F. ) ;
#24368 = CARTESIAN_POINT ( 'NONE',  ( -8.674200344734190438, 1437.754171787169980, 209.1145358281810047 ) ) ;
#24369 = CARTESIAN_POINT ( 'NONE',  ( -3.982959088878220033, 1515.551843419129909, 211.9714090624810012 ) ) ;
#24370 = PRODUCT_DEFINITION_FORMATION_WITH_SPECIFIED_SOURCE ( 'ANY', '', #104493, .NOT_KNOWN. ) ;
#24371 = CARTESIAN_POINT ( 'NONE',  ( 2.500000000000000000, 1432.302110539269961, 157.4936333739979943 ) ) ;
#24372 = CARTESIAN_POINT ( 'NONE',  ( -5.943685272961615418, 1451.459285800949601, 153.4774835117595160 ) ) ;
#24373 = CARTESIAN_POINT ( 'NONE',  ( 25.21503096769999885, 1435.882664665889934, 137.0280311863980103 ) ) ;
#24375 = EDGE_CURVE ( 'NONE', #15354, #68835, #51563, .T. ) ;
#24374 = CARTESIAN_POINT ( 'NONE',  ( 2.258825551794999775, 1511.942942747529969, 216.7106486523369995 ) ) ;
#24377 = ORIENTED_EDGE ( 'NONE', *, *, #69694, .T. ) ;
#24376 = CARTESIAN_POINT ( 'NONE',  ( -14.80327112760000041, 1409.939845700729848, 226.5217252883980166 ) ) ;
#24378 = CARTESIAN_POINT ( 'NONE',  ( 1.674829163898249984, 1414.913060387399810, 192.1894932412249943 ) ) ;
#24379 = DIRECTION ( 'NONE',  ( -6.922360974429999144E-17, -1.000000000000000000, 2.302693041820029802E-16 ) ) ;
#24380 = ORIENTED_EDGE ( 'NONE', *, *, #80990, .F. ) ;
#24381 = ORIENTED_EDGE ( 'NONE', *, *, #103611, .F. ) ;
#24382 = CARTESIAN_POINT ( 'NONE',  ( -12.78943350980000027, 1502.708798922290043, 209.0180533589250160 ) ) ;
#24383 = CARTESIAN_POINT ( 'NONE',  ( -19.34601893677120898, 1526.333389948038530, 233.0427900344768091 ) ) ;
#24385 = CARTESIAN_POINT ( 'NONE',  ( -21.72443950929999801, 1451.953218211529929, 220.8606415680980035 ) ) ;
#24384 = CARTESIAN_POINT ( 'NONE',  ( 4.035142546699999500, 1455.426291782089947, 218.0958705512090035 ) ) ;
#24386 = B_SPLINE_CURVE_WITH_KNOTS ( 'NONE', 5,
 ( #91909, #84606, #57789, #33102, #16280, #49373, #65633, #99194, #56674 ),
 .UNSPECIFIED., .F., .F.,
 ( 6, 3, 6 ),
 ( 0.000000000000000000, 0.4999999999999998335, 1.000000000000000000 ),
 .UNSPECIFIED. ) ;
#24387 = CARTESIAN_POINT ( 'NONE',  ( -7.550047457009999796, 1446.700195908890009, 214.6466464486289851 ) ) ;
#24388 = CARTESIAN_POINT ( 'NONE',  ( -11.48286129179999904, 1433.329274650220214, 151.2855545196979961 ) ) ;
#24389 = CARTESIAN_POINT ( 'NONE',  ( -12.30975638026900043, 1378.376095226579992, 209.8073264528339905 ) ) ;
#24390 = CARTESIAN_POINT ( 'NONE',  ( 9.717824533310780666, 1463.678478211699939, 210.3770741684630252 ) ) ;
#24391 = CARTESIAN_POINT ( 'NONE',  ( 7.911464481230000345, 1423.187191425399988, 213.2893462354790017 ) ) ;
#24392 = CARTESIAN_POINT ( 'NONE',  ( -24.28094609940000126, 1438.198944389940152, 211.0663462535580095 ) ) ;
#24393 = FACE_BOUND ( 'NONE', #87405, .T. ) ;
#24394 = CARTESIAN_POINT ( 'NONE',  ( -2.923521517025829741, 1410.394928878200062, 186.6127595807840009 ) ) ;
#24395 = CARTESIAN_POINT ( 'NONE',  ( 7.893629640421917948, 1363.336479960825272, 207.6218459616988241 ) ) ;
#24396 = CARTESIAN_POINT ( 'NONE',  ( -29.52699855556750208, 1510.054681897895989, 203.5615033681672230 ) ) ;
#24397 = AXIS2_PLACEMENT_3D ( 'NONE', #44921, #67494, #44356 ) ;
#24399 = VERTEX_POINT ( 'NONE', #39189 ) ;
#24398 = CARTESIAN_POINT ( 'NONE',  ( -1.238275708498259911E-09, 1416.572336828779953, 238.6617246227660019 ) ) ;
#24400 = ORIENTED_EDGE ( 'NONE', *, *, #62050, .F. ) ;
#24401 = CARTESIAN_POINT ( 'NONE',  ( -11.74192897671919944, 1426.699235643070097, 144.5141135958380119 ) ) ;
#24402 = CARTESIAN_POINT ( 'NONE',  ( 0.1080666684629969926, 1502.828674633789888, 233.2928853222989858 ) ) ;
#24403 = CARTESIAN_POINT ( 'NONE',  ( -7.520399231549999008, 1473.125808901829942, 270.3839821968980459 ) ) ;
#24404 = CARTESIAN_POINT ( 'NONE',  ( -1.556370157619999972, 1414.996444526030018, 226.5294865527980051 ) ) ;
#24405 = CARTESIAN_POINT ( 'NONE',  ( -124.1837824924000557, 1366.350733876290406, 301.4682942176205529 ) ) ;
#24406 = CARTESIAN_POINT ( 'NONE',  ( -8.157610789389998729, 1384.622758710029984, 199.6574702203289746 ) ) ;
#24407 = CARTESIAN_POINT ( 'NONE',  ( 18.00963447456260269, 1431.117864245919918, 206.0875853561470024 ) ) ;
#24408 = DIRECTION ( 'NONE',  ( 0.2902388374169100338, -0.1068831630355692452, -0.9509665644566018816 ) ) ;
#24409 = CARTESIAN_POINT ( 'NONE',  ( 9.925983360900000108, 1364.303202023270160, 207.6218459616989946 ) ) ;
#24410 = CARTESIAN_POINT ( 'NONE',  ( -9.077803069467520913, 1448.962985536510132, 210.3449884047199987 ) ) ;
#24411 = CARTESIAN_POINT ( 'NONE',  ( -10.65372266856249972, 1406.685601047840009, 268.4360227182569929 ) ) ;
#24412 = CIRCLE ( 'NONE', #87013, 0.9999999999999955591 ) ;
#24413 = CARTESIAN_POINT ( 'NONE',  ( -13.42238899811910002, 1434.957430979650098, 149.2077055965390002 ) ) ;
#24414 = VERTEX_POINT ( 'NONE', #38643 ) ;
#24415 = DIRECTION ( 'NONE',  ( 0.9109019969992648846, -0.3842787907060009056, -0.1502909274583290045 ) ) ;
#24416 = ORIENTED_EDGE ( 'NONE', *, *, #881, .F. ) ;
#24417 = ORIENTED_EDGE ( 'NONE', *, *, #3542, .T. ) ;
#24418 = CARTESIAN_POINT ( 'NONE',  ( 4.868531005982084103, 1422.373029460236467, 184.3158709850344508 ) ) ;
#24419 = CARTESIAN_POINT ( 'NONE',  ( 9.297632061492119959, 1425.336027861749926, 195.2545234328350148 ) ) ;
#24421 = CARTESIAN_POINT ( 'NONE',  ( 31.23437356469435144, 1512.187213306747481, 197.3468678195113739 ) ) ;
#24420 = CARTESIAN_POINT ( 'NONE',  ( 0.01327404799950150129, 1516.939877939420057, 212.5773418040870126 ) ) ;
#24422 = CARTESIAN_POINT ( 'NONE',  ( 5.381311975764999644, 1511.468585915670019, 217.4468093916769931 ) ) ;
#24423 = CARTESIAN_POINT ( 'NONE',  ( -16.85472157044729968, 1498.343964390320025, 229.6923633532749989 ) ) ;
#24424 = VERTEX_POINT ( 'NONE', #29153 ) ;
#24425 = DIRECTION ( 'NONE',  ( -0.6736849260863839728, 0.000000000000000000, 0.7390186874254150995 ) ) ;
#24426 = CARTESIAN_POINT ( 'NONE',  ( -7.331183129075000693, 1516.882217593000178, 202.1801186797769674 ) ) ;
#24427 = CARTESIAN_POINT ( 'NONE',  ( -4.363122561674769528, 1421.971318449149976, 184.5104913919989826 ) ) ;
#24428 = CARTESIAN_POINT ( 'NONE',  ( -32.14450299649809750, 1384.561384632279896, 206.8209701602499990 ) ) ;
#24429 = CARTESIAN_POINT ( 'NONE',  ( -1.430117442880000089, 1408.963001188930093, 194.1218459369979996 ) ) ;
#24430 = FACE_OUTER_BOUND ( 'NONE', #85309, .T. ) ;
#24432 = ORIENTED_EDGE ( 'NONE', *, *, #4394, .T. ) ;
#24431 = CARTESIAN_POINT ( 'NONE',  ( -37.88774006571790665, 1442.824633575369944, 137.1073183462600014 ) ) ;
#24433 = CARTESIAN_POINT ( 'NONE',  ( -23.55026106900000116, 1411.110742672429751, 210.4800087176980128 ) ) ;
#24434 = CARTESIAN_POINT ( 'NONE',  ( 28.18850436520000358, 1508.134789600230079, 209.7835208149050175 ) ) ;
#24435 = CARTESIAN_POINT ( 'NONE',  ( 13.77266209894789917, 1522.051704408389924, 201.2043266506040027 ) ) ;
#24436 = CARTESIAN_POINT ( 'NONE',  ( 0.8756585369989179357, 1425.746450835400083, 191.1126529878390272 ) ) ;
#24437 = CARTESIAN_POINT ( 'NONE',  ( -24.03198776159999994, 1435.355284493859926, 137.0425515896980073 ) ) ;
#24438 = CARTESIAN_POINT ( 'NONE',  ( -24.34268549840000162, 1442.549315796029759, 212.2035716145279878 ) ) ;
#24439 = CARTESIAN_POINT ( 'NONE',  ( 5.012938863775000087, 1517.051603658920158, 211.6026598552170128 ) ) ;
#24440 = CARTESIAN_POINT ( 'NONE',  ( 1.145290945507940084, 1458.110487998910003, 199.6352770989870180 ) ) ;
#24441 = CARTESIAN_POINT ( 'NONE',  ( -2.896892187767880156, 1484.263391075600111, 183.3160938869699805 ) ) ;
#24442 = CIRCLE ( 'NONE', #58447, 7.513264357030008611 ) ;
#24443 = CARTESIAN_POINT ( 'NONE',  ( -14.00253459870000228, 1430.158944055929851, 222.3204534089979916 ) ) ;
#24444 = LINE ( 'NONE', #58632, #77145 ) ;
#24445 = CARTESIAN_POINT ( 'NONE',  ( -3.269984819434999856, 1516.999105586269934, 207.4194399470370058 ) ) ;
#24446 = ORIENTED_EDGE ( 'NONE', *, *, #89048, .F. ) ;
#24447 = CARTESIAN_POINT ( 'NONE',  ( -40.71747596959829707, 1438.773003713930166, 134.4203395907470053 ) ) ;
#24448 = CARTESIAN_POINT ( 'NONE',  ( -10.16826309620000224, 1472.406893517490062, 208.4967702181029665 ) ) ;
#24449 = CARTESIAN_POINT ( 'NONE',  ( -19.54853263967898158, 1457.140775842711719, 225.9785477345730271 ) ) ;
#24450 = ORIENTED_EDGE ( 'NONE', *, *, #62279, .T. ) ;
#24451 = CARTESIAN_POINT ( 'NONE',  ( -29.86461515634926656, 1525.960063244517187, 197.2746849027940925 ) ) ;
#24452 = CARTESIAN_POINT ( 'NONE',  ( 12.72351525216199875, 1435.772547898509856, 150.8350212812320024 ) ) ;
#24453 = CARTESIAN_POINT ( 'NONE',  ( -4.116135330806149462, 1441.427949229778278, 184.2827671596340906 ) ) ;
#24454 = CARTESIAN_POINT ( 'NONE',  ( -4.119767774860000564, 1413.537972784140266, 207.3346887680889949 ) ) ;
#24455 = CARTESIAN_POINT ( 'NONE',  ( 2.471608048749999842, 1438.194204504490017, 150.4833623973980252 ) ) ;
#24456 = CARTESIAN_POINT ( 'NONE',  ( 4.989613516749999533, 1487.671035670790161, 198.1975016566989893 ) ) ;
#24457 = CARTESIAN_POINT ( 'NONE',  ( 2.356294384139039799, 1431.021013722109956, 218.3169074369490090 ) ) ;
#24458 = PLANE ( 'NONE',  #59453 ) ;
#24460 = CARTESIAN_POINT ( 'NONE',  ( -11.88140585900000090, 1433.447543843229823, 147.6490162021979984 ) ) ;
#24459 = CARTESIAN_POINT ( 'NONE',  ( -4.999456428534999830, 1516.830644417779922, 213.7431138541670066 ) ) ;
#24461 = CARTESIAN_POINT ( 'NONE',  ( 20.11539126239999931, 1508.359231766530002, 189.1805378999980007 ) ) ;
#24462 = CARTESIAN_POINT ( 'NONE',  ( 3.261635932824999973, 1516.613881697390070, 216.0569793506570022 ) ) ;
#24463 = CIRCLE ( 'NONE', #29906, 5.499916801759985319 ) ;
#24464 = ORIENTED_EDGE ( 'NONE', *, *, #57993, .T. ) ;
#24465 = FACE_OUTER_BOUND ( 'NONE', #9037, .T. ) ;
#24466 = CARTESIAN_POINT ( 'NONE',  ( -16.76646998270000211, 1420.451233668469968, 203.6167452475490052 ) ) ;
#24467 = CARTESIAN_POINT ( 'NONE',  ( 2.412180996239999597, 1419.421713268930034, 185.1536642287979930 ) ) ;
#24468 = ADVANCED_FACE ( 'NONE', ( #105872 ), #168, .T. ) ;
#24469 = CARTESIAN_POINT ( 'NONE',  ( -1.062402653849999989, 1475.637717254689960, 220.5408259888989733 ) ) ;
#24470 = CARTESIAN_POINT ( 'NONE',  ( -105.0631825244292372, 1390.534411153809060, 304.1916690124131719 ) ) ;
#24471 = UNCERTAINTY_MEASURE_WITH_UNIT (LENGTH_MEASURE( 1.000000000000000082E-05 ), #64675, 'distance_accuracy_value', 'NONE');
#24472 = CARTESIAN_POINT ( 'NONE',  ( 1.133338450661860008, 1423.755929587430046, 191.2144893514050068 ) ) ;
#24473 = CARTESIAN_POINT ( 'NONE',  ( -11.39934036035690035, 1470.872822770500079, 208.6597014105470294 ) ) ;
#24474 = CARTESIAN_POINT ( 'NONE',  ( -5.382670666700607676, 1508.259648345004507, 220.3115702328250336 ) ) ;
#24475 = DIRECTION ( 'NONE',  ( 0.1403901532130676921, 0.9900962604114871279, 1.240732444514164729E-15 ) ) ;
#24476 = CARTESIAN_POINT ( 'NONE',  ( 18.25964269232630599, 1425.332953396113226, 224.8491606838273356 ) ) ;
#24477 = ADVANCED_FACE ( 'NONE', ( #30135 ), #20619, .T. ) ;
#24478 = CARTESIAN_POINT ( 'NONE',  ( -8.335430188334420131E-07, 1408.657067462929945, 223.1089253223800313 ) ) ;
#24479 = CARTESIAN_POINT ( 'NONE',  ( 27.50547257934209711, 1446.424453580260206, 137.1666655437190059 ) ) ;
#24480 = B_SPLINE_CURVE_WITH_KNOTS ( 'NONE', 3,
 ( #61353, #41752, #94344, #68091, #69185, #42306, #103869, #67533, #102203, #93786, #59132, #75911, #334, #34460, #17062, #68637, #94921, #102737, #26598, #18194, #52391, #86514, #27169, #101633, #95473, #18740, #24922, #85392, #33895, #50709, #84840, #8140, #96018, #71967, #20397, #1990, #97128, #63558, #3647, #19290, #106078, #2546, #97673 ),
 .UNSPECIFIED., .F., .F.,
 ( 4, 3, 3, 3, 3, 3, 3, 3, 3, 3, 3, 3, 3, 3, 4 ),
 ( -2.000000000000000000, -1.920433884135369862, -1.776779042643749973, -1.631085684125360036, -1.484142407439499989, -1.335324404072970150, -1.185565806898190022, -1.035185577921500011, -0.8845459646997599901, -0.7342798813318649476, -0.5847724199270629697, -0.4363642902088080699, -0.2893200053190718712, -0.1438262832493450993, 0.000000000000000000 ),
 .UNSPECIFIED. ) ;
#24482 = DIRECTION ( 'NONE',  ( -0.03489950421557262011, 0.9993908267567336301, 7.330759870573984416E-09 ) ) ;
#24481 = CARTESIAN_POINT ( 'NONE',  ( -10.54622137524750158, 1471.119434090909863, 209.8143280353739897 ) ) ;
#24483 = CARTESIAN_POINT ( 'NONE',  ( 12.88130326439999784, 1419.881202692929946, 222.3734530188980045 ) ) ;
#24484 = VERTEX_POINT ( 'NONE', #13873 ) ;
#24485 = ORIENTED_EDGE ( 'NONE', *, *, #61170, .T. ) ;
#24486 = DIRECTION ( 'NONE',  ( -0.1070030146457386366, 0.000000000000000000, -0.9942586961433749204 ) ) ;
#24487 = CARTESIAN_POINT ( 'NONE',  ( -19.66847414439826380, 1485.263780816827648, 190.3137200183769551 ) ) ;
#24488 = AXIS2_PLACEMENT_3D ( 'NONE', #28607, #103087, #62807 ) ;
#24489 = CARTESIAN_POINT ( 'NONE',  ( -28.66995855460000087, 1509.914237400329966, 211.4901977112579914 ) ) ;
#24490 = CARTESIAN_POINT ( 'NONE',  ( -12.87618670773889917, 1416.835419214280137, 221.9337012713420165 ) ) ;
#24491 = LINE ( 'NONE', #93359, #102063 ) ;
#24492 = CARTESIAN_POINT ( 'NONE',  ( -2.074768463076620328, 1486.986234437389840, 220.1251915955149911 ) ) ;
#24493 = CARTESIAN_POINT ( 'NONE',  ( -4.015749066599999750, 1515.588778490289997, 208.3687103823360189 ) ) ;
#24494 = CARTESIAN_POINT ( 'NONE',  ( -73.02464777688889797, 1383.782474506479957, 297.9868448762199478 ) ) ;
#24495 = CARTESIAN_POINT ( 'NONE',  ( 10.89003754610000030, 1451.711500069930025, 152.2142025596980091 ) ) ;
#24496 = LINE ( 'NONE', #75497, #8890 ) ;
#24497 = CARTESIAN_POINT ( 'NONE',  ( 10.95202006776319870, 1490.978190374230053, 210.0828909271359919 ) ) ;
#24499 = VERTEX_POINT ( 'NONE', #46428 ) ;
#24498 = CARTESIAN_POINT ( 'NONE',  ( -2.788614694270000083, 1456.607942948890013, 218.2023089652089993 ) ) ;
#24500 = CARTESIAN_POINT ( 'NONE',  ( 33.45065857237933216, 1524.841055067848629, 219.4656524796220367 ) ) ;
#24501 = CARTESIAN_POINT ( 'NONE',  ( -72.24957631569999705, 1381.775758148160094, 272.8158467630589712 ) ) ;
#24502 = CARTESIAN_POINT ( 'NONE',  ( 19.78518508183620028, 1508.106391392640035, 229.3111777015780035 ) ) ;
#24503 = ORIENTED_EDGE ( 'NONE', *, *, #87963, .F. ) ;
#24504 = VERTEX_POINT ( 'NONE', #88946 ) ;
#24505 = CARTESIAN_POINT ( 'NONE',  ( -8.508204430222377823, 1386.516060600280071, 218.4508996449510221 ) ) ;
#24506 = CARTESIAN_POINT ( 'NONE',  ( 38.59693733168150231, 1439.219610169110183, 136.6571113115409730 ) ) ;
#24508 = CARTESIAN_POINT ( 'NONE',  ( 1.161830502209999949, 1469.358622120289965, 189.0813358120989847 ) ) ;
#24507 = DIRECTION ( 'NONE',  ( 1.000000000000000000, 0.000000000000000000, 0.000000000000000000 ) ) ;
#24509 = CARTESIAN_POINT ( 'NONE',  ( -6.973120769980000411, 1462.078774314090197, 202.2276825251889818 ) ) ;
#24510 = AXIS2_PLACEMENT_3D ( 'NONE', #59626, #103244, #49575 ) ;
#24511 = CARTESIAN_POINT ( 'NONE',  ( -105.6757023109999949, 1378.000557810240025, 302.9257663873589763 ) ) ;
#24512 = CARTESIAN_POINT ( 'NONE',  ( -12.02002121700249937, 1447.120365805550136, 187.5076542713389927 ) ) ;
#24513 = CARTESIAN_POINT ( 'NONE',  ( -11.92890078398071552, 1435.343914765019463, 151.2188616800775094 ) ) ;
#24514 = LINE ( 'NONE', #58703, #44216 ) ;
#24515 = CARTESIAN_POINT ( 'NONE',  ( 13.74310390781900004, 1517.151704408390060, 217.0905615615409943 ) ) ;
#24516 = CARTESIAN_POINT ( 'NONE',  ( 1.031770593039999850, 1409.117028087930066, 185.7659931841980097 ) ) ;
#24517 = CARTESIAN_POINT ( 'NONE',  ( 4.359264906129999950, 1423.889211762329978, 184.2836487311979852 ) ) ;
#24518 = CARTESIAN_POINT ( 'NONE',  ( 6.050886996877059332, 1433.308159904890090, 202.4648030222659827 ) ) ;
#24519 = CARTESIAN_POINT ( 'NONE',  ( -2.499999999849909837, 1439.824763698960169, 159.3159658887090018 ) ) ;
#24520 = AXIS2_PLACEMENT_3D ( 'NONE', #98479, #21747, #96852 ) ;
#24521 = CARTESIAN_POINT ( 'NONE',  ( 11.86590139589999815, 1432.348266868109931, 151.0567667964980103 ) ) ;
#24522 = VERTEX_POINT ( 'NONE', #38540 ) ;
#24523 = CARTESIAN_POINT ( 'NONE',  ( -0.8141018274779999730, 1430.453334911130241, 150.3332009510979788 ) ) ;
#24524 = CARTESIAN_POINT ( 'NONE',  ( -3.949444845858078867, 1427.113443899376762, 134.0999999980980135 ) ) ;
#24525 =( BOUNDED_CURVE ( )  B_SPLINE_CURVE ( 3, ( #98855, #46290, #47912, #82047 ),
 .UNSPECIFIED., .F., .F. ) 
 B_SPLINE_CURVE_WITH_KNOTS ( ( 4, 4 ),
 ( 1.036083073916405750, 2.105411660058823298 ),
 .UNSPECIFIED. ) 
 CURVE ( )  GEOMETRIC_REPRESENTATION_ITEM ( )  RATIONAL_B_SPLINE_CURVE ( ( 1.000000000000000000, 0.9069598253101942564, 0.9069598253101942564, 1.000000000000000000 ) ) 
 REPRESENTATION_ITEM ( '' )  );
#24526 = CARTESIAN_POINT ( 'NONE',  ( 15.42454884180000008, 1430.140040983930021, 190.9214399110979912 ) ) ;
#24527 = CARTESIAN_POINT ( 'NONE',  ( -8.328873504844570907E-09, 1475.098823578779957, 265.5557250396390145 ) ) ;
#24528 = CARTESIAN_POINT ( 'NONE',  ( 20.48353907805949703, 1436.444560210333520, 144.9117583361570780 ) ) ;
#24529 = FACE_OUTER_BOUND ( 'NONE', #55449, .T. ) ;
#24530 = FACE_OUTER_BOUND ( 'NONE', #95588, .T. ) ;
#24531 = CARTESIAN_POINT ( 'NONE',  ( -107.1491673510000027, 1387.396471041590075, 310.3410155632590204 ) ) ;
#24532 = CARTESIAN_POINT ( 'NONE',  ( -0.06018024750005197820, 1486.202617829743531, 181.8162541669730103 ) ) ;
#24533 = CARTESIAN_POINT ( 'NONE',  ( -8.454776581079805453, 1360.296086664740642, 208.3718459617010978 ) ) ;
#24534 = CARTESIAN_POINT ( 'NONE',  ( -46.01983168967480253, 1438.258892378159771, 268.2089072814339943 ) ) ;
#24535 = CARTESIAN_POINT ( 'NONE',  ( -2.499999999859999988, 1439.640830480200293, 184.0873493999980042 ) ) ;
#24536 = CARTESIAN_POINT ( 'NONE',  ( -8.700499408960000736, 1424.079320566130036, 207.5589903581490034 ) ) ;
#24537 = CARTESIAN_POINT ( 'NONE',  ( -3.460866208815000178, 1517.020847257979995, 208.3861469975149987 ) ) ;
#24538 = CARTESIAN_POINT ( 'NONE',  ( -5.386101783710000035, 1432.347042943159977, 154.6076477470979853 ) ) ;
#24539 = CARTESIAN_POINT ( 'NONE',  ( -14.34470072367650140, 1379.595425982329971, 208.0071153785060005 ) ) ;
#24540 = CARTESIAN_POINT ( 'NONE',  ( 7.354254828809129840, 1426.340165684199974, 212.6766371994280007 ) ) ;
#24541 = CARTESIAN_POINT ( 'NONE',  ( -25.18522889079570248, 1452.033591493209769, 135.3780775317339931 ) ) ;
#24542 = ORIENTED_EDGE ( 'NONE', *, *, #7637, .F. ) ;
#24543 = CARTESIAN_POINT ( 'NONE',  ( 7.587264836529999279, 1421.907226632029960, 217.1547583186280121 ) ) ;
#24545 = CARTESIAN_POINT ( 'NONE',  ( -14.82736039673160100, 1512.135905030570029, 221.4210449998400065 ) ) ;
#24544 = CARTESIAN_POINT ( 'NONE',  ( -2.273033093151270556, 1525.821544997590308, 177.3097463090896326 ) ) ;
#24546 = CARTESIAN_POINT ( 'NONE',  ( -0.9691334048877314755, 1488.056577045728773, 219.9420655526842552 ) ) ;
#24547 = CARTESIAN_POINT ( 'NONE',  ( -15.52964687406499955, 1451.324136384999974, 222.4830579234560162 ) ) ;
#24548 = CARTESIAN_POINT ( 'NONE',  ( 17.04532911661896932, 1519.551704408389924, 221.2898363890541589 ) ) ;
#24549 = CARTESIAN_POINT ( 'NONE',  ( 3.401541474470889614, 1468.225229937070026, 218.5224292273400124 ) ) ;
#24550 = CARTESIAN_POINT ( 'NONE',  ( 18.19476890929999868, 1429.544292015390056, 208.2833220268470029 ) ) ;
#24551 = ORIENTED_EDGE ( 'NONE', *, *, #19277, .T. ) ;
#24552 = CARTESIAN_POINT ( 'NONE',  ( 1.600048698852036821, 1411.254281879943164, 135.5999999980979851 ) ) ;
#24553 = CARTESIAN_POINT ( 'NONE',  ( 16.03409403789510179, 1422.997244933739921, 228.9049390009139984 ) ) ;
#24554 = CARTESIAN_POINT ( 'NONE',  ( 9.808373588480000294, 1462.684821613489930, 210.4841290881089719 ) ) ;
#24555 = ORIENTED_EDGE ( 'NONE', *, *, #41136, .F. ) ;
#24556 = ORIENTED_EDGE ( 'NONE', *, *, #62414, .T. ) ;
#24557 = CARTESIAN_POINT ( 'NONE',  ( -23.81602722030639896, 1410.419941936439955, 209.8068453827619919 ) ) ;
#24558 = ORIENTED_EDGE ( 'NONE', *, *, #87183, .F. ) ;
#24559 = DIRECTION ( 'NONE',  ( 0.000000000000000000, -1.000000000000000000, 0.000000000000000000 ) ) ;
#24560 = CIRCLE ( 'NONE', #87177, 2.000000000000003109 ) ;
#24561 = CARTESIAN_POINT ( 'NONE',  ( -8.968501251859999357, 1428.602659895330135, 101.8807690336980016 ) ) ;
#24562 = CARTESIAN_POINT ( 'NONE',  ( -1.919144336779999849, 1507.641079666230098, 237.0664109672979976 ) ) ;
#24563 = CARTESIAN_POINT ( 'NONE',  ( -18.99570766729999960, 1410.874976135429733, 222.9834657993979761 ) ) ;
#24564 = CARTESIAN_POINT ( 'NONE',  ( 40.83400096486530373, 1456.643151761250010, 266.3273196274960242 ) ) ;
#24565 = CARTESIAN_POINT ( 'NONE',  ( -11.01364452973389874, 1391.913060387030100, 206.0332053900289964 ) ) ;
#24566 = B_SPLINE_CURVE_WITH_KNOTS ( 'NONE', 3,
 ( #12785, #31783, #57016, #91690, #13307, #91141, #14418, #48611, #82744, #14967, #6037, #74370, #65974, #49161, #72177, #76415, #85920, #34960, #17019, #95433, #9224, #51218, #85349, #290, #51782, #43382, #70270, #68045, #17582, #10313, #59630, #104379, #36085, #33854, #102155, #77531, #25435 ),
 .UNSPECIFIED., .F., .F.,
 ( 4, 3, 3, 3, 3, 3, 3, 3, 3, 3, 3, 3, 4 ),
 ( -77.98062027567270604, -77.28570685305760435, -75.84252669430900085, -74.37770857730430407, -72.90452813415019762, -71.43163176466710240, -69.96926794057800691, -68.52392561414599470, -67.09989659765190595, -66.56132197703499287, -65.17789798084180575, -63.76799573968669677, -62.33963421229999824 ),
 .UNSPECIFIED. ) ;
#24567 = CARTESIAN_POINT ( 'NONE',  ( -17.12001958753553765, 1422.219426602513295, 226.7452668728065248 ) ) ;
#24568 = CARTESIAN_POINT ( 'NONE',  ( -7.722536802824999214, 1517.050041317280147, 204.5049460973469877 ) ) ;
#24569 = ORIENTED_EDGE ( 'NONE', *, *, #56222, .F. ) ;
#24570 = CARTESIAN_POINT ( 'NONE',  ( 18.73173501632924953, 1458.223697907665837, 227.3016765217417401 ) ) ;
#24571 = CARTESIAN_POINT ( 'NONE',  ( -0.6532060423541629079, 1444.609809648689861, 199.0872701831330005 ) ) ;
#24572 = CARTESIAN_POINT ( 'NONE',  ( 4.069411599699999549, 1427.113643276370112, 212.3578269758590125 ) ) ;
#24573 = ORIENTED_EDGE ( 'NONE', *, *, #33659, .F. ) ;
#24574 = CARTESIAN_POINT ( 'NONE',  ( -11.31803579276679983, 1481.249050730999897, 210.4920860573550101 ) ) ;
#24575 = CARTESIAN_POINT ( 'NONE',  ( 5.380056979554551866, 1434.542470706314134, 202.5070600846412106 ) ) ;
#24576 = CARTESIAN_POINT ( 'NONE',  ( -15.74021840828143404, 1517.051704408389924, 221.9061614121420973 ) ) ;
#24577 = CARTESIAN_POINT ( 'NONE',  ( 11.69850812630680004, 1502.052734125200232, 214.1386926423620025 ) ) ;
#24578 = CARTESIAN_POINT ( 'NONE',  ( 7.758184319229999737, 1421.576654411539948, 195.8091089427989857 ) ) ;
#24579 = CARTESIAN_POINT ( 'NONE',  ( 22.27637251949999708, 1409.690968457230156, 211.0033668272880050 ) ) ;
#24580 = CARTESIAN_POINT ( 'NONE',  ( 10.11567626329839875, 1479.961683375350049, 205.9716079530940078 ) ) ;
#24581 = CARTESIAN_POINT ( 'NONE',  ( 2.570960541213360262, 1409.002840307820179, 187.0877483113689834 ) ) ;
#24583 = DIRECTION ( 'NONE',  ( 0.02978939777567089775, 0.9648997004021163670, 0.2609236668914279300 ) ) ;
#24582 = CARTESIAN_POINT ( 'NONE',  ( 30.60461244942475645, 1523.621879633029039, 196.4204177336139878 ) ) ;
#24584 = AXIS2_PLACEMENT_3D ( 'NONE', #71246, #3479, #103705 ) ;
#24585 = CARTESIAN_POINT ( 'NONE',  ( 1.530059654846469996, 1452.704397329589938, 183.4894956925679992 ) ) ;
#24586 = CARTESIAN_POINT ( 'NONE',  ( -11.92968414179999925, 1378.045929578360074, 212.2475929956690095 ) ) ;
#24587 = CARTESIAN_POINT ( 'NONE',  ( 16.19464330292652932, 1423.010950068178090, 229.4833128991568287 ) ) ;
#24588 = ORIENTED_EDGE ( 'NONE', *, *, #54213, .F. ) ;
#24589 = LINE ( 'NONE', #68310, #94541 ) ;
#24590 = AXIS2_PLACEMENT_3D ( 'NONE', #27696, #55677, #79219 ) ;
#24591 = CARTESIAN_POINT ( 'NONE',  ( 17.21411468017923596, 1414.941240534613826, 210.6779454605140813 ) ) ;
#24592 = CARTESIAN_POINT ( 'NONE',  ( -12.22845464540000116, 1392.111545638959797, 206.8354075410990163 ) ) ;
#24593 = CARTESIAN_POINT ( 'NONE',  ( 10.39728290242030084, 1427.483012415709936, 210.1624185323059919 ) ) ;
#24594 = CARTESIAN_POINT ( 'NONE',  ( 10.94186774115649996, 1423.753146808589918, 203.2164765458729789 ) ) ;
#24595 = CARTESIAN_POINT ( 'NONE',  ( 13.15804437931859994, 1421.151500651059905, 221.7660300441250172 ) ) ;
#24596 = CARTESIAN_POINT ( 'NONE',  ( -20.14739811709999984, 1469.497636830730016, 271.1218459616979999 ) ) ;
#24597 = CARTESIAN_POINT ( 'NONE',  ( -8.860260194638639675, 1384.841874547059888, 218.6844059295819989 ) ) ;
#24598 = CARTESIAN_POINT ( 'NONE',  ( 11.84937012939999867, 1433.469328321039939, 150.5730835599980253 ) ) ;
#24599 = CARTESIAN_POINT ( 'NONE',  ( 26.42894384599999924, 1460.505561531929970, 262.6648722511980054 ) ) ;
#24600 = CARTESIAN_POINT ( 'NONE',  ( 12.13987205295800109, 1415.426207913209964, 196.5375152356580202 ) ) ;
#24601 = CARTESIAN_POINT ( 'NONE',  ( 1.420259601960000229, 1466.712985171129958, 235.0376566307980113 ) ) ;
#24602 = CARTESIAN_POINT ( 'NONE',  ( 9.031927925652290412, 1421.291943124229874, 197.0056667342660148 ) ) ;
#24603 = CARTESIAN_POINT ( 'NONE',  ( -15.06279480623459222, 1422.388301958798820, 229.4662111127462651 ) ) ;
#24604 = CARTESIAN_POINT ( 'NONE',  ( -19.36475817619999873, 1485.943425245129902, 190.1135902501980013 ) ) ;
#24605 = CARTESIAN_POINT ( 'NONE',  ( 12.84736500079448440, 1398.293695667951624, 211.5699839868841252 ) ) ;
#24606 = CARTESIAN_POINT ( 'NONE',  ( 18.63578313170000200, 1416.568813547830132, 209.6898099495820134 ) ) ;
#24607 = AXIS2_PLACEMENT_3D ( 'NONE', #55384, #12807, #30149 ) ;
#24608 = CARTESIAN_POINT ( 'NONE',  ( 22.14275666300000012, 1410.906117087829898, 215.7312451241079998 ) ) ;
#24609 = DIRECTION ( 'NONE',  ( 0.000000000000000000, 0.000000000000000000, -1.000000000000000000 ) ) ;
#24610 = DIRECTION ( 'NONE',  ( -0.9948834766775035421, -0.000000000000000000, -0.1010290445074252669 ) ) ;
#24611 = CARTESIAN_POINT ( 'NONE',  ( -14.58219550427210010, 1383.858962634210002, 219.1768149639169962 ) ) ;
#24612 = CARTESIAN_POINT ( 'NONE',  ( -19.86464710103360076, 1441.435714288719964, 212.6459465483729900 ) ) ;
#24613 = CARTESIAN_POINT ( 'NONE',  ( -19.30744623537299987, 1418.880101625140014, 208.8299352253080201 ) ) ;
#24614 = CARTESIAN_POINT ( 'NONE',  ( 0.1692191542157840123, 1480.788586062970126, 182.0605159988109847 ) ) ;
#24616 = ORIENTED_EDGE ( 'NONE', *, *, #69977, .T. ) ;
#24615 = CARTESIAN_POINT ( 'NONE',  ( 0.06764665397380001388, 1408.848989337130206, 223.4935224561980078 ) ) ;
#24617 = CARTESIAN_POINT ( 'NONE',  ( -18.64337105059427913, 1444.324653571828549, 162.1710875046049694 ) ) ;
#24618 = FACE_OUTER_BOUND ( 'NONE', #4353, .T. ) ;
#24619 = DIRECTION ( 'NONE',  ( -0.6736849260863841948, 0.000000000000000000, 0.7390186874254148774 ) ) ;
#24620 = CARTESIAN_POINT ( 'NONE',  ( -41.61795676491179563, 1442.846609225109887, 134.0999999981039821 ) ) ;
#24621 = PLANE ( 'NONE',  #31800 ) ;
#24622 = EDGE_LOOP ( 'NONE', ( #84202, #6530, #61817, #95762, #89023 ) ) ;
#24623 = CARTESIAN_POINT ( 'NONE',  ( -17.62867182259884302, 1524.547873515804895, 180.6301120142637728 ) ) ;
#24624 = CARTESIAN_POINT ( 'NONE',  ( 10.84148007940000014, 1478.843050295790135, 205.9629258051089948 ) ) ;
#24625 = CARTESIAN_POINT ( 'NONE',  ( -104.9411529111025487, 1380.860630878966958, 308.2816869617895463 ) ) ;
#24626 = CARTESIAN_POINT ( 'NONE',  ( -19.59053950279439960, 1486.265866315750145, 189.8955481462990065 ) ) ;
#24627 = ADVANCED_FACE ( 'NONE', ( #64326, #21717 ), #71653, .F. ) ;
#24628 = CARTESIAN_POINT ( 'NONE',  ( -5.666956068895039778, 1433.164882934490151, 215.5009249933730189 ) ) ;
#24629 = AXIS2_PLACEMENT_3D ( 'NONE', #95063, #27859, #18330 ) ;
#24630 = CARTESIAN_POINT ( 'NONE',  ( 0.4720966309508138892, 1418.692307282306956, 184.7100086785088138 ) ) ;
#24631 = DIRECTION ( 'NONE',  ( -1.987380029059999976E-13, 6.832419524060000430E-15, 1.000000000000000000 ) ) ;
#24632 = CARTESIAN_POINT ( 'NONE',  ( 7.121584085660000341, 1409.161751583630121, 222.2855843900980233 ) ) ;
#24633 = CARTESIAN_POINT ( 'NONE',  ( 3.429372500519999978, 1436.958971107729894, 184.6577026058980096 ) ) ;
#24634 = CARTESIAN_POINT ( 'NONE',  ( -67.47041654031760061, 1385.099433479379968, 260.5101198769480106 ) ) ;
#24635 = CARTESIAN_POINT ( 'NONE',  ( -11.64091994802049790, 1391.913060387289988, 210.0754932155269898 ) ) ;
#24636 = CARTESIAN_POINT ( 'NONE',  ( 12.14434402762229936, 1421.782244358430034, 208.4503354109049837 ) ) ;
#24637 = ORIENTED_EDGE ( 'NONE', *, *, #110571, .F. ) ;
#24638 = CARTESIAN_POINT ( 'NONE',  ( 11.89922653334599012, 1433.329005341657876, 149.9506340396733890 ) ) ;
#24639 = CARTESIAN_POINT ( 'NONE',  ( 12.29654148988069373, 1442.773887286368335, 164.4841150006940325 ) ) ;
#24641 = ORIENTED_EDGE ( 'NONE', *, *, #93320, .F. ) ;
#24640 = CARTESIAN_POINT ( 'NONE',  ( 3.454899550169740152, 1437.151257404700118, 227.3279159481639908 ) ) ;
#24642 = CARTESIAN_POINT ( 'NONE',  ( 4.134276593080000062, 1473.270938484690078, 218.6199709919989971 ) ) ;
#24643 = DIRECTION ( 'NONE',  ( 0.7384854939282339270, -4.128709092058508552E-17, -0.6742693640212139572 ) ) ;
#24644 = CARTESIAN_POINT ( 'NONE',  ( -7.173827098650000345, 1361.757975858899954, 207.6218459616989946 ) ) ;
#24645 = CARTESIAN_POINT ( 'NONE',  ( -10.81171726419999857, 1492.479041299990058, 205.9913540356689907 ) ) ;
#24646 = CARTESIAN_POINT ( 'NONE',  ( 41.71654787359375405, 1444.824798330285603, 269.6421161746990265 ) ) ;
#24647 = FACE_OUTER_BOUND ( 'NONE', #39695, .T. ) ;
#24648 = CARTESIAN_POINT ( 'NONE',  ( 15.51696353740144296, 1431.230679900481618, 219.3923223260254645 ) ) ;
#24649 = CARTESIAN_POINT ( 'NONE',  ( 1776.370103581280091, 5181.793945261120825, -8870.008376233501622 ) ) ;
#24650 = CARTESIAN_POINT ( 'NONE',  ( 8.343671689369999811, 1449.263932163490153, 204.8140308564489942 ) ) ;
#24651 = CARTESIAN_POINT ( 'NONE',  ( -21.48880489289999929, 1507.176470023590127, 211.5094435469989946 ) ) ;
#24652 = CARTESIAN_POINT ( 'NONE',  ( -4.987078435459999071, 1509.051704408389924, 209.1218459616989946 ) ) ;
#24653 = CIRCLE ( 'NONE', #96235, 3.993878626057317582 ) ;
#24654 = CARTESIAN_POINT ( 'NONE',  ( -30.79916350761092048, 1526.104292489148747, 217.1177548920758795 ) ) ;
#24655 = CARTESIAN_POINT ( 'NONE',  ( -4.042729840925000317, 1516.919782530640077, 205.8674445284970034 ) ) ;
#24656 = CIRCLE ( 'NONE', #94449, 33.13701971169416538 ) ;
#24657 = CARTESIAN_POINT ( 'NONE',  ( 3.116758655549999979, 1446.591766555970025, 170.5446539970980098 ) ) ;
#24658 = ORIENTED_EDGE ( 'NONE', *, *, #102990, .F. ) ;
#24659 = CARTESIAN_POINT ( 'NONE',  ( -109.1646618499602397, 1384.891810334096363, 297.1326802748606610 ) ) ;
#24660 = CARTESIAN_POINT ( 'NONE',  ( 14.45771163620000088, 1416.835808384130132, 196.8517379759979917 ) ) ;
#24662 = VERTEX_POINT ( 'NONE', #55921 ) ;
#24661 = CARTESIAN_POINT ( 'NONE',  ( -68.44952925478749250, 1379.747226849109893, 280.0582246923240177 ) ) ;
#24663 = CARTESIAN_POINT ( 'NONE',  ( -9.668563137246193762, 1379.991352563589089, 216.8468033706864730 ) ) ;
#24664 = ORIENTED_EDGE ( 'NONE', *, *, #21486, .T. ) ;
#24665 = AXIS2_PLACEMENT_3D ( 'NONE', #42326, #78693, #76480 ) ;
#24666 = CARTESIAN_POINT ( 'NONE',  ( -16.67556694314024668, 1513.118420038618069, 221.3657088474023169 ) ) ;
#24667 = ADVANCED_FACE ( 'NONE', ( #73260 ), #29589, .F. ) ;
#24668 = CARTESIAN_POINT ( 'NONE',  ( -23.30790377659999990, 1410.912174224829869, 205.7308725902679782 ) ) ;
#24670 = CARTESIAN_POINT ( 'NONE',  ( 15.78650398947750055, 1409.847271299810018, 191.9459370198140107 ) ) ;
#24669 = CARTESIAN_POINT ( 'NONE',  ( -11.34647335060000017, 1426.876719822230143, 115.9728140669979979 ) ) ;
#24671 = EDGE_CURVE ( 'NONE', #39549, #22340, #106294, .T. ) ;
#24672 = CARTESIAN_POINT ( 'NONE',  ( -0.7351098092479989576, 1516.977504706749869, 211.6135016956469883 ) ) ;
#24673 = CARTESIAN_POINT ( 'NONE',  ( 41.44218962868909983, 1442.560172593170137, 136.4421865476589915 ) ) ;
#24674 = EDGE_CURVE ( 'NONE', #86208, #50172, #105212, .T. ) ;
#24675 = CARTESIAN_POINT ( 'NONE',  ( -33.67851661499999949, 1421.560016960630037, 261.9077615516980586 ) ) ;
#24676 = CARTESIAN_POINT ( 'NONE',  ( -0.2678627835216980113, 1508.980470044890126, 179.3639230931030113 ) ) ;
#24677 = ADVANCED_FACE ( 'NONE', ( #48059 ), #50201, .F. ) ;
#24678 = CARTESIAN_POINT ( 'NONE',  ( 16.47155471125729420, 1460.849993040709023, 229.0965666438152937 ) ) ;
#24679 = ITEM_DEFINED_TRANSFORMATION ( 'NONE', 'NONE', #57330,  #21632 ) ;
#24680 = ADVANCED_FACE ( 'NONE', ( #41310 ), #14978, .T. ) ;
#24681 = CARTESIAN_POINT ( 'NONE',  ( 4.902792406504040024, 1508.551704408389924, 212.2587853230709811 ) ) ;
#24682 = CARTESIAN_POINT ( 'NONE',  ( -36.78701199996249471, 1437.792136250990097, 136.5523556798590050 ) ) ;
#24683 = ORIENTED_EDGE ( 'NONE', *, *, #27042, .F. ) ;
#24684 = CARTESIAN_POINT ( 'NONE',  ( -18.32377786700000399, 1464.077817829789865, 217.4721512913189940 ) ) ;
#24685 = CARTESIAN_POINT ( 'NONE',  ( -18.62496937760000293, 1457.110903083630092, 228.9008583485980353 ) ) ;
#24686 = EDGE_LOOP ( 'NONE', ( #84345, #12999, #35640 ) ) ;
#24687 = ORIENTED_EDGE ( 'NONE', *, *, #107537, .F. ) ;
#24688 = CARTESIAN_POINT ( 'NONE',  ( 1.332267629549999902E-15, 1412.913060387329779, 209.1218459616989946 ) ) ;
#24689 = CARTESIAN_POINT ( 'NONE',  ( 10.55962377587460033, 1452.696006162120057, 209.8459794650469803 ) ) ;
#24690 = CARTESIAN_POINT ( 'NONE',  ( -6.487810219224459551, 1508.114173656130106, 220.3031569931239915 ) ) ;
#24691 = VECTOR ( 'NONE', #35719, 1000.000000000000000 ) ;
#24692 = FACE_OUTER_BOUND ( 'NONE', #10970, .T. ) ;
#24693 = CARTESIAN_POINT ( 'NONE',  ( 4.201139955930000447, 1515.456931311890003, 210.2329862578490065 ) ) ;
#24694 = DIRECTION ( 'NONE',  ( 0.000000000000000000, 0.000000000000000000, 1.000000000000000000 ) ) ;
#24695 = CARTESIAN_POINT ( 'NONE',  ( 40.71747596959940552, 1438.773003713930166, 134.4205483767809994 ) ) ;
#24696 = CARTESIAN_POINT ( 'NONE',  ( 3.724929213431543484, 1516.669760784861410, 215.6322040485396485 ) ) ;
#24697 = CARTESIAN_POINT ( 'NONE',  ( 25.47948162479999823, 1436.582469785759940, 137.1757940733980092 ) ) ;
#24698 = CARTESIAN_POINT ( 'NONE',  ( -11.40910167059999836, 1391.913060387289988, 211.4454899872289957 ) ) ;
#24699 = EDGE_CURVE ( 'NONE', #92620, #110694, #17021, .T. ) ;
#24700 = CARTESIAN_POINT ( 'NONE',  ( -103.0456467999559891, 1384.883686176350011, 296.7218882600220127 ) ) ;
#24701 = ORIENTED_EDGE ( 'NONE', *, *, #92741, .F. ) ;
#24702 = CARTESIAN_POINT ( 'NONE',  ( -0.7533001734329990429, 1516.714320817460020, 201.7957737879569891 ) ) ;
#24703 = CARTESIAN_POINT ( 'NONE',  ( -7.719640941135000212, 1516.939452820819952, 209.1319487995289705 ) ) ;
#24704 = ORIENTED_EDGE ( 'NONE', *, *, #70951, .F. ) ;
#24705 = CARTESIAN_POINT ( 'NONE',  ( 11.79866176452289928, 1428.170196302150089, 148.1141846266930031 ) ) ;
#24706 = CARTESIAN_POINT ( 'NONE',  ( 2.994315780531499271, 1512.053483454412799, 217.0162803964337854 ) ) ;
#24707 = ORIENTED_EDGE ( 'NONE', *, *, #21296, .T. ) ;
#24708 = CARTESIAN_POINT ( 'NONE',  ( -14.35445997400000095, 1416.822690122629865, 221.5782749823979998 ) ) ;
#24709 = CARTESIAN_POINT ( 'NONE',  ( -11.69294445086449841, 1432.337845643199898, 150.8474197947550124 ) ) ;
#24710 = CARTESIAN_POINT ( 'NONE',  ( 22.08327125186944428, 1523.604703353109699, 233.8169256665487694 ) ) ;
#24711 = EDGE_CURVE ( 'NONE', #76707, #15508, #49173, .T. ) ;
#24712 = CARTESIAN_POINT ( 'NONE',  ( -2.844617774716496239, 1488.558558072584219, 219.6378750350716587 ) ) ;
#24713 = CARTESIAN_POINT ( 'NONE',  ( 21.84956437405869778, 1409.868736151659959, 206.3073818229169945 ) ) ;
#24714 = CARTESIAN_POINT ( 'NONE',  ( 9.905242068095489572, 1468.560492227489931, 207.6656469818879884 ) ) ;
#24715 = FACE_OUTER_BOUND ( 'NONE', #103097, .T. ) ;
#24716 = EDGE_CURVE ( 'NONE', #68013, #24247, #47454, .T. ) ;
#24717 = CARTESIAN_POINT ( 'NONE',  ( -7.272433915116270242, 1410.543391134071953, 187.5337605366746629 ) ) ;
#24718 = CARTESIAN_POINT ( 'NONE',  ( -63.91816553489999819, 1379.742600501299876, 270.3198227003589977 ) ) ;
#24719 = FACE_OUTER_BOUND ( 'NONE', #63119, .T. ) ;
#24721 = CARTESIAN_POINT ( 'NONE',  ( 7.578766088578010596, 1467.899149354640031, 200.9046483899009843 ) ) ;
#24720 = CARTESIAN_POINT ( 'NONE',  ( -21.63156322749999916, 1505.770867997990081, 209.2235208569570091 ) ) ;
#24722 = CARTESIAN_POINT ( 'NONE',  ( 6.753961865179999968, 1469.830701748189995, 210.2167338168290200 ) ) ;
#24723 = CARTESIAN_POINT ( 'NONE',  ( 1.708092266164999984, 1516.523379810429788, 216.8305916180169959 ) ) ;
#24724 = ORIENTED_EDGE ( 'NONE', *, *, #97273, .T. ) ;
#24725 = EDGE_CURVE ( 'NONE', #106056, #2195, #74927, .T. ) ;
#24726 = CARTESIAN_POINT ( 'NONE',  ( 32.37018134260406299, 1512.187213306747481, 218.0712926453362002 ) ) ;
#24727 = CARTESIAN_POINT ( 'NONE',  ( 0.9839655838812769728, 1516.663585454903341, 216.8342630320297246 ) ) ;
#24728 = CARTESIAN_POINT ( 'NONE',  ( -0.7365612166329978949, 1517.066898074209803, 213.7457380308570123 ) ) ;
#24729 = CARTESIAN_POINT ( 'NONE',  ( -2.945604300558919864, 1485.274571919582741, 182.9922692145212864 ) ) ;
#24730 = CARTESIAN_POINT ( 'NONE',  ( -11.60004869885203505, 1426.083046513046838, 138.9256368688967314 ) ) ;
#24732 = ORIENTED_EDGE ( 'NONE', *, *, #86267, .T. ) ;
#24731 = CARTESIAN_POINT ( 'NONE',  ( 4.987080938901260474, 1508.551704408389924, 213.0804906078760155 ) ) ;
#24733 = CARTESIAN_POINT ( 'NONE',  ( -8.604799066060000001, 1384.909923716469848, 199.8686514356990074 ) ) ;
#24734 = CARTESIAN_POINT ( 'NONE',  ( 1.699897556570000079, 1508.551704408389924, 219.7511403508990213 ) ) ;
#24735 = CARTESIAN_POINT ( 'NONE',  ( -11.54217015299999893, 1429.750359027530067, 150.6915807595979970 ) ) ;
#24736 = CARTESIAN_POINT ( 'NONE',  ( 19.05886514166099843, 1456.926298666380035, 225.3128034416440073 ) ) ;
#24737 = CARTESIAN_POINT ( 'NONE',  ( -5.930039503890000674, 1441.838256304279867, 183.8171696374980115 ) ) ;
#24738 = CARTESIAN_POINT ( 'NONE',  ( 9.298374091227790572, 1424.634616539950230, 149.7551418246100070 ) ) ;
#24739 = CARTESIAN_POINT ( 'NONE',  ( -4.663088608516360978, 1427.954664977100038, 201.0136482515530076 ) ) ;
#24740 = CARTESIAN_POINT ( 'NONE',  ( -2.488082932330000219, 1441.600846913620217, 150.5962877614979902 ) ) ;
#24742 = CARTESIAN_POINT ( 'NONE',  ( -21.50400446119279962, 1505.467562055609960, 209.6175409707290100 ) ) ;
#24741 = CARTESIAN_POINT ( 'NONE',  ( -22.76497971890000116, 1482.723760643630158, 222.4289363302980007 ) ) ;
#24743 = CARTESIAN_POINT ( 'NONE',  ( -16.00058974059999883, 1465.442699635990039, 221.9149816820990111 ) ) ;
#24744 = ORIENTED_EDGE ( 'NONE', *, *, #54202, .T. ) ;
#24745 = CARTESIAN_POINT ( 'NONE',  ( 5.772403774305000290, 1516.676340709600026, 205.8583240277470168 ) ) ;
#24746 = CARTESIAN_POINT ( 'NONE',  ( 23.72605694800000009, 1410.650267468229913, 267.6119861631980257 ) ) ;
#24747 = CARTESIAN_POINT ( 'NONE',  ( -32.86470156657983210, 1523.580204110581917, 217.2021180770848616 ) ) ;
#24748 = AXIS2_PLACEMENT_3D ( 'NONE', #70060, #71153, #94663 ) ;
#24749 = CARTESIAN_POINT ( 'NONE',  ( 17.85928734389999661, 1430.310748820929803, 191.7175708229979705 ) ) ;
#24750 = AXIS2_PLACEMENT_3D ( 'NONE', #104753, #44876, #96356 ) ;
#24751 = CARTESIAN_POINT ( 'NONE',  ( -0.08548173663637460840, 1507.632698406310283, 237.3720899768290167 ) ) ;
#24752 = CARTESIAN_POINT ( 'NONE',  ( -8.062121734079813251, 1387.317230855839398, 218.5919200099478701 ) ) ;
#24753 = CARTESIAN_POINT ( 'NONE',  ( -1.442473716300000097, 1451.217997451130032, 183.7279619786979765 ) ) ;
#24754 = CARTESIAN_POINT ( 'NONE',  ( -9.822264486677861081E-06, 1450.913060148159957, 181.2410907034809782 ) ) ;
#24755 = CARTESIAN_POINT ( 'NONE',  ( -15.35926873949999916, 1415.632233529220002, 207.7221835180689880 ) ) ;
#24756 = CARTESIAN_POINT ( 'NONE',  ( -14.34064213879999983, 1445.290870928000004, 188.7064315755980033 ) ) ;
#24757 = CARTESIAN_POINT ( 'NONE',  ( -21.45452449210000267, 1497.713060387329961, 213.1853964382480058 ) ) ;
#24758 = CARTESIAN_POINT ( 'NONE',  ( -16.30759486957349580, 1419.707542479528001, 209.7289770706684351 ) ) ;
#24759 = CARTESIAN_POINT ( 'NONE',  ( -7.402577614759999314, 1497.624368088290112, 217.8806385702189914 ) ) ;
#24760 = CARTESIAN_POINT ( 'NONE',  ( -0.7270621067209990240, 1477.679265261989940, 201.4865919325389996 ) ) ;
#24761 = FACE_OUTER_BOUND ( 'NONE', #49649, .T. ) ;
#24762 = EDGE_CURVE ( 'NONE', #7882, #7907, #58122, .T. ) ;
#24763 = DIRECTION ( 'NONE',  ( -0.01668530547203130737, -0.7071067811868645414, 0.7069098956591685079 ) ) ;
#24764 = CARTESIAN_POINT ( 'NONE',  ( -7.233415693649337008, 1421.233009521309668, 193.8023935178989916 ) ) ;
#24765 = CARTESIAN_POINT ( 'NONE',  ( -7.031059539510000178, 1475.166475290029894, 269.2761626991979824 ) ) ;
#24767 = STYLED_ITEM ( 'NONE', ( #61234 ), #82338 ) ;
#24766 = CARTESIAN_POINT ( 'NONE',  ( -30.12442103005642124, 1524.524650307258753, 195.8615354049555322 ) ) ;
#24768 = CARTESIAN_POINT ( 'NONE',  ( -14.79463505727891004, 1514.566409480255743, 192.8705245058147568 ) ) ;
#24769 = DIRECTION ( 'NONE',  ( 0.4035202328300511176, 0.000000000000000000, 0.9149707217702551798 ) ) ;
#24770 = CARTESIAN_POINT ( 'NONE',  ( -47.91296898077749944, 1384.750118820870057, 257.4434400084929848 ) ) ;
#24771 = CARTESIAN_POINT ( 'NONE',  ( -106.4020803887899973, 1391.913060387289988, 304.0987531970990290 ) ) ;
#24772 = CARTESIAN_POINT ( 'NONE',  ( 11.34486003903470142, 1415.059973078959956, 222.6680858266069833 ) ) ;
#24773 = CARTESIAN_POINT ( 'NONE',  ( -107.4477388159999975, 1379.886884385820167, 299.0757729400589824 ) ) ;
#24774 = CARTESIAN_POINT ( 'NONE',  ( 4.873735476160000246, 1472.089320948289924, 218.0431589096889695 ) ) ;
#24775 = CYLINDRICAL_SURFACE ( 'NONE', #73318, 1.455175085940062507 ) ;
#24776 = CARTESIAN_POINT ( 'NONE',  ( -17.99954287939999986, 1410.904693930530129, 195.2564708288979887 ) ) ;
#24777 = B_SPLINE_CURVE_WITH_KNOTS ( 'NONE', 3,
 ( #18045, #83597, #84153, #75770, #16375, #50573, #34860, #32658, #93104, #85814 ),
 .UNSPECIFIED., .F., .F.,
 ( 4, 2, 2, 2, 4 ),
 ( 0.000000000000000000, 0.0007189769279726063861, 0.001437953855945212772, 0.002156930783917819158, 0.002875907711890425544 ),
 .UNSPECIFIED. ) ;
#24778 = CARTESIAN_POINT ( 'NONE',  ( -11.93976775657317013, 1378.024740770806602, 206.0762735010970061 ) ) ;
#24779 = CARTESIAN_POINT ( 'NONE',  ( 3.675002922379999593, 1484.816058337290087, 219.9704011141990350 ) ) ;
#24780 = EDGE_CURVE ( 'NONE', #52522, #84750, #55544, .T. ) ;
#24781 = CARTESIAN_POINT ( 'NONE',  ( 11.49453118813409880, 1478.838340461310054, 206.6810620774099903 ) ) ;
#24782 = CARTESIAN_POINT ( 'NONE',  ( -3.968827103576990201, 1519.551704408389924, 229.5396913781519856 ) ) ;
#24783 = CARTESIAN_POINT ( 'NONE',  ( 11.82788503319999940, 1436.101494931290063, 225.5825002257989809 ) ) ;
#24784 = CARTESIAN_POINT ( 'NONE',  ( -6.120117913879710159, 1508.729257035799947, 216.5649250963629981 ) ) ;
#24785 = CARTESIAN_POINT ( 'NONE',  ( -13.67844807081490011, 1504.250361896059985, 227.6838271028410077 ) ) ;
#24787 = CARTESIAN_POINT ( 'NONE',  ( -15.00364260096500146, 1514.335759350750095, 193.0073477423669885 ) ) ;
#24786 = CARTESIAN_POINT ( 'NONE',  ( -22.04779405809999915, 1409.847308038730034, 211.6317860905479904 ) ) ;
#24788 = CARTESIAN_POINT ( 'NONE',  ( 11.73663431677760016, 1426.696239189569951, 144.1418624741639860 ) ) ;
#24789 = CARTESIAN_POINT ( 'NONE',  ( 17.05900707844048014, 1524.678872986498845, 237.1958236346374633 ) ) ;
#24790 = DIRECTION ( 'NONE',  ( 2.343158368729999945E-19, 1.387778780780000088E-15, -1.000000000000000000 ) ) ;
#24791 = LINE ( 'NONE', #76333, #62461 ) ;
#24792 = CARTESIAN_POINT ( 'NONE',  ( -0.05087723766931040448, 1408.368774909099784, 222.6640242851099742 ) ) ;
#24793 = CARTESIAN_POINT ( 'NONE',  ( -7.720650173434999708, 1516.977993847330026, 203.3422188780170075 ) ) ;
#24794 = CARTESIAN_POINT ( 'NONE',  ( 5.864566082395450408, 1517.151704408390060, 226.1537825710409777 ) ) ;
#24795 = CARTESIAN_POINT ( 'NONE',  ( -12.78681252341862340, 1398.292084349547167, 211.4732289992830374 ) ) ;
#24796 = CARTESIAN_POINT ( 'NONE',  ( 15.87603342113500027, 1512.359593911809952, 198.0975645610670028 ) ) ;
#24797 = FACE_BOUND ( 'NONE', #56701, .T. ) ;
#24798 = CARTESIAN_POINT ( 'NONE',  ( -24.42450952024000088, 1377.857503279539969, 215.6133220620030215 ) ) ;
#24799 = CARTESIAN_POINT ( 'NONE',  ( 20.30811166882689989, 1509.558778732829978, 230.1713494956079842 ) ) ;
#24800 = CIRCLE ( 'NONE', #82049, 1.000000000000015099 ) ;
#24802 = ORIENTED_EDGE ( 'NONE', *, *, #68911, .F. ) ;
#24801 = CARTESIAN_POINT ( 'NONE',  ( -48.15636025208650040, 1379.711680487519970, 241.4636575790609925 ) ) ;
#24803 = ORIENTED_EDGE ( 'NONE', *, *, #36340, .T. ) ;
#24804 = CARTESIAN_POINT ( 'NONE',  ( 12.00598652703259894, 1433.712414975789898, 150.0453429833439998 ) ) ;
#24805 = CARTESIAN_POINT ( 'NONE',  ( -13.31360989399999895, 1398.307674596630022, 207.3550467807280029 ) ) ;
#24806 = ORIENTED_EDGE ( 'NONE', *, *, #23721, .F. ) ;
#24807 = CARTESIAN_POINT ( 'NONE',  ( -105.9298767669999961, 1379.081211923699811, 306.7609391451590000 ) ) ;
#24808 = EDGE_CURVE ( 'NONE', #6602, #56560, #57027, .T. ) ;
#24809 = CARTESIAN_POINT ( 'NONE',  ( -3.487592467065000257, 1509.038615934169911, 213.6090957241370063 ) ) ;
#24810 = DIRECTION ( 'NONE',  ( -1.000000000000000000, 0.000000000000000000, 0.000000000000000000 ) ) ;
#24812 = CARTESIAN_POINT ( 'NONE',  ( -13.73987724751260053, 1508.184446304589983, 184.1670646690170088 ) ) ;
#24811 = CARTESIAN_POINT ( 'NONE',  ( 3.375977098360000372, 1446.395221917490062, 199.5681764228489783 ) ) ;
#24813 = CARTESIAN_POINT ( 'NONE',  ( 18.89293537649999877, 1507.815827870629846, 229.9105837539979973 ) ) ;
#24814 = CARTESIAN_POINT ( 'NONE',  ( 2.377993551410000350, 1468.705613521729902, 182.9807957255980000 ) ) ;
#24815 = EDGE_CURVE ( 'NONE', #77110, #24021, #84409, .T. ) ;
#24816 = CARTESIAN_POINT ( 'NONE',  ( -5.281923854050000422, 1415.931391677429929, 191.9559905162979874 ) ) ;
#24817 = CARTESIAN_POINT ( 'NONE',  ( 2.738491091690000268, 1419.583501618159971, 204.7124688696490011 ) ) ;
#24818 = B_SPLINE_SURFACE_WITH_KNOTS ( 'NONE', 5, 5, ( 
 ( #75338, #110021, #99394, #22673, #61316, #42822 ),
 ( #17583, #69711, #52894, #18698, #93742, #26560 ),
 ( #85350, #43927, #78073, #1376, #10885, #10314 ),
 ( #34961, #1949, #25437, #53452, #69145, #103249 ),
 ( #8647, #76984, #68589, #59631, #17020, #9226 ),
 ( #291, #27678, #94305, #18153, #834, #51783 ) ),
 .UNSPECIFIED., .F., .F., .F.,
 ( 6, 6 ),
 ( 6, 6 ),
 ( 4.770714915030000114, 5.109858025250000324 ),
 ( 0.000000000000000000, 2.000000000000000000 ),
 .UNSPECIFIED. ) ;
#24819 = CARTESIAN_POINT ( 'NONE',  ( -17.17241001986523941, 1523.382868172864164, 179.6185504016046082 ) ) ;
#24820 = CARTESIAN_POINT ( 'NONE',  ( 2.500020115319840031, 1419.382923540379807, 144.1035841389490031 ) ) ;
#24821 = CARTESIAN_POINT ( 'NONE',  ( 11.75937283610000073, 1431.557362424269968, 150.7646243546980145 ) ) ;
#24822 = CARTESIAN_POINT ( 'NONE',  ( 5.818574454934999807, 1514.487275757750012, 201.4289454835769959 ) ) ;
#24823 = ORIENTED_EDGE ( 'NONE', *, *, #104271, .F. ) ;
#24824 = CARTESIAN_POINT ( 'NONE',  ( 13.04096353016549870, 1435.727353653040154, 150.6338561105279723 ) ) ;
#24825 = ORIENTED_EDGE ( 'NONE', *, *, #75427, .T. ) ;
#24826 = ORIENTED_EDGE ( 'NONE', *, *, #15487, .T. ) ;
#24827 = EDGE_CURVE ( 'NONE', #21719, #8025, #90345, .T. ) ;
#24828 = CARTESIAN_POINT ( 'NONE',  ( 13.36968693692587706, 1444.477217224934293, 169.3716362414181162 ) ) ;
#24829 = CARTESIAN_POINT ( 'NONE',  ( -8.255467981419998935, 1463.782943827829968, 233.8280712257979985 ) ) ;
#24830 = AXIS2_PLACEMENT_3D ( 'NONE', #105644, #106717, #64198 ) ;
#24831 = CARTESIAN_POINT ( 'NONE',  ( -9.922940940763762541, 1473.528715622569734, 206.4586403660501901 ) ) ;
#24832 = CARTESIAN_POINT ( 'NONE',  ( 4.616861508414999093, 1516.666407245520077, 216.8343369232169948 ) ) ;
#24833 = CARTESIAN_POINT ( 'NONE',  ( -7.924515700752487568, 1511.889608912520998, 212.2345484715577584 ) ) ;
#24834 = B_SPLINE_SURFACE_WITH_KNOTS ( 'NONE', 5, 5, ( 
 ( #94360, #104993, #69200, #61919, #87086, #54074 ),
 ( #10938, #43991, #103307, #1430, #2564, #10370 ),
 ( #27184, #18208, #88200, #52951, #86528, #78126 ),
 ( #60811, #17641, #52405, #45669, #70881, #28284 ),
 ( #96599, #19870, #11494, #44544, #102753, #61367 ),
 ( #51842, #9279, #95487, #43439, #78689, #77590 ) ),
 .UNSPECIFIED., .F., .F., .F.,
 ( 6, 6 ),
 ( 6, 6 ),
 ( 7.590234162189999800, 19.60754526079999849 ),
 ( 0.1222658846940000016, 0.5999999999999999778 ),
 .UNSPECIFIED. ) ;
#24835 = AXIS2_PLACEMENT_3D ( 'NONE', #19502, #53704, #87845 ) ;
#24836 = EDGE_CURVE ( 'NONE', #56666, #98856, #62308, .T. ) ;
#24837 = CARTESIAN_POINT ( 'NONE',  ( 11.19147557906589974, 1422.145537183640045, 210.4506353095700035 ) ) ;
#24838 = CARTESIAN_POINT ( 'NONE',  ( 2.500000000000000000, 1448.231796796869958, 166.4378714439059763 ) ) ;
#24839 = CARTESIAN_POINT ( 'NONE',  ( -3.771520291289999882, 1375.697147833719782, 207.5503167614189977 ) ) ;
#24840 =( BOUNDED_CURVE ( )  B_SPLINE_CURVE ( 3, ( #85130, #36391, #86794, #77851 ),
 .UNSPECIFIED., .F., .F. ) 
 B_SPLINE_CURVE_WITH_KNOTS ( ( 4, 4 ),
 ( 1.953429545882020113, 2.601599304719214967 ),
 .UNSPECIFIED. ) 
 CURVE ( )  GEOMETRIC_REPRESENTATION_ITEM ( )  RATIONAL_B_SPLINE_CURVE ( ( 1.000000000000000000, 0.9652950237418777002, 0.9652950237418777002, 1.000000000000000000 ) ) 
 REPRESENTATION_ITEM ( '' )  );
#24841 = ORIENTED_EDGE ( 'NONE', *, *, #53684, .T. ) ;
#24842 = CARTESIAN_POINT ( 'NONE',  ( 4.028307740155000261, 1516.797038924770050, 205.8554964580370097 ) ) ;
#24843 = ORIENTED_EDGE ( 'NONE', *, *, #43925, .F. ) ;
#24844 = CARTESIAN_POINT ( 'NONE',  ( 20.57595172751539891, 1440.913060387330006, 219.9584118754960116 ) ) ;
#24845 = CARTESIAN_POINT ( 'NONE',  ( -18.68654022859999841, 1509.565608751230002, 231.3997216384979936 ) ) ;
#24846 = CARTESIAN_POINT ( 'NONE',  ( -12.92009008149999971, 1409.866466474230037, 189.8912044915980175 ) ) ;
#24847 = CARTESIAN_POINT ( 'NONE',  ( 8.126234247455000670, 1514.923664147150021, 215.2485921136969864 ) ) ;
#24849 = ORIENTED_EDGE ( 'NONE', *, *, #46735, .T. ) ;
#24848 = CARTESIAN_POINT ( 'NONE',  ( 0.09392264341561619434, 1415.426561690370136, 226.6233626858019932 ) ) ;
#24850 = CARTESIAN_POINT ( 'NONE',  ( 21.66194437680000107, 1429.187467587929859, 218.7319503095280027 ) ) ;
#24851 = CARTESIAN_POINT ( 'NONE',  ( -3.897009773373953490, 1519.551704408389924, 187.2231132105589211 ) ) ;
#24852 = EDGE_CURVE ( 'NONE', #53780, #73756, #15284, .T. ) ;
#24853 = CARTESIAN_POINT ( 'NONE',  ( -106.4241660069999966, 1383.759861017009825, 311.1380007012590454 ) ) ;
#24854 = CARTESIAN_POINT ( 'NONE',  ( 0.0007013484591967420129, 1465.026770150519951, 237.7732560087259799 ) ) ;
#24855 = VECTOR ( 'NONE', #34631, 1000.000000000000114 ) ;
#24856 = EDGE_CURVE ( 'NONE', #74077, #72398, #58695, .T. ) ;
#24857 = CARTESIAN_POINT ( 'NONE',  ( -6.548821979184999975, 1516.688761843659904, 213.1592242262869945 ) ) ;
#24858 = CARTESIAN_POINT ( 'NONE',  ( 1.491506560153233352, 1511.187213306747708, 242.6732489767341576 ) ) ;
#24859 = CYLINDRICAL_SURFACE ( 'NONE', #82101, 1.999999999999981348 ) ;
#24860 = CARTESIAN_POINT ( 'NONE',  ( -7.722579826676089887, 1517.051704428850144, 208.6871515679729896 ) ) ;
#24861 = CARTESIAN_POINT ( 'NONE',  ( -5.771149113014999443, 1516.616791731099966, 211.6102065995370083 ) ) ;
#24862 = CARTESIAN_POINT ( 'NONE',  ( -20.91563430996852091, 1525.795403621571268, 233.2509748519915718 ) ) ;
#24863 = CARTESIAN_POINT ( 'NONE',  ( 13.55937162340000057, 1409.552479690230030, 191.5919554294980003 ) ) ;
#24864 = CARTESIAN_POINT ( 'NONE',  ( -9.140833745038642988, 1486.006228221076299, 183.5277714374079778 ) ) ;
#24866 = ORIENTED_EDGE ( 'NONE', *, *, #65604, .T. ) ;
#24865 = CARTESIAN_POINT ( 'NONE',  ( -59.30951814779999864, 1386.658176173940092, 279.8843003692589946 ) ) ;
#24867 = CARTESIAN_POINT ( 'NONE',  ( -52.91940571912499536, 1385.104601948549998, 267.6864206406419839 ) ) ;
#24868 = CARTESIAN_POINT ( 'NONE',  ( 33.66409353290000439, 1447.474031022650252, 250.0355534076980177 ) ) ;
#24869 = CARTESIAN_POINT ( 'NONE',  ( 8.800000000000002487, 1412.913060387329779, 209.1218459616989946 ) ) ;
#24870 = CARTESIAN_POINT ( 'NONE',  ( -3.393167906721693328, 1495.486076169147736, 219.7910603749398604 ) ) ;
#24871 = CARTESIAN_POINT ( 'NONE',  ( 12.55935747509999878, 1421.555442417790118, 207.1258153896989995 ) ) ;
#24872 = CARTESIAN_POINT ( 'NONE',  ( 11.46842531143500032, 1512.169992403149990, 225.2408885909669891 ) ) ;
#24874 = DIRECTION ( 'NONE',  ( -1.755985294532469921E-16, 1.000000000000000000, -1.338183447452831989E-16 ) ) ;
#24873 = CARTESIAN_POINT ( 'NONE',  ( -4.219439023932549659, 1446.230224804030058, 183.1418048969109975 ) ) ;
#24875 = DIRECTION ( 'NONE',  ( 1.000000000000000000, 6.438966932878399974E-12, 0.000000000000000000 ) ) ;
#24876 = CARTESIAN_POINT ( 'NONE',  ( -106.2815139762350043, 1381.801306631560010, 309.7257556431679859 ) ) ;
#24877 = VERTEX_POINT ( 'NONE', #70404 ) ;
#24878 = CARTESIAN_POINT ( 'NONE',  ( 2.483322453895000059, 1517.139039350860003, 202.5585910412470128 ) ) ;
#24879 = CARTESIAN_POINT ( 'NONE',  ( 0.2302825872959999853, 1467.622811642030001, 229.4111514478979927 ) ) ;
#24880 = B_SPLINE_SURFACE_WITH_KNOTS ( 'NONE', 5, 1, ( 
 ( #104401, #61882 ),
 ( #3077, #45076 ),
 ( #19267, #37204 ),
 ( #53470, #12547 ),
 ( #95998, #71948 ),
 ( #37756, #46726 ) ),
 .UNSPECIFIED., .F., .F., .F.,
 ( 6, 6 ),
 ( 2, 2 ),
 ( 0.000000000000000000, 17.60720389089999927 ),
 ( 0.000000000000000000, 14.00000000000000000 ),
 .UNSPECIFIED. ) ;
#24881 = CARTESIAN_POINT ( 'NONE',  ( -4.194822514691770311E-06, 1471.586156170330014, 269.6149383081970541 ) ) ;
#24882 = CARTESIAN_POINT ( 'NONE',  ( -33.52308185467848034, 1525.402221411349728, 217.5800527287189539 ) ) ;
#24883 = LINE ( 'NONE', #66942, #91375 ) ;
#24884 = CARTESIAN_POINT ( 'NONE',  ( 4.244807866439999522, 1467.382213863189918, 218.1353146091890096 ) ) ;
#24885 = CARTESIAN_POINT ( 'NONE',  ( 7.092997891250118592, 1416.799648712304588, 231.0433554185687512 ) ) ;
#24886 = CARTESIAN_POINT ( 'NONE',  ( 32.03033759198009278, 1435.776089609319797, 136.0024512530590073 ) ) ;
#24887 = CIRCLE ( 'NONE', #33863, 1.000000000000000888 ) ;
#24888 = CARTESIAN_POINT ( 'NONE',  ( 38.97393047930350463, 1447.767677101680192, 136.5281119700379975 ) ) ;
#24889 = CARTESIAN_POINT ( 'NONE',  ( -4.038220123662581429, 1450.278798041637629, 185.0006713385352839 ) ) ;
#24890 = CARTESIAN_POINT ( 'NONE',  ( -109.2614022059999996, 1385.672371935979982, 297.1866512157590705 ) ) ;
#24891 = CARTESIAN_POINT ( 'NONE',  ( 14.23428072729999982, 1509.239486858130022, 184.7798516627979666 ) ) ;
#24892 = CARTESIAN_POINT ( 'NONE',  ( 19.38211899476434041, 1526.344110814219221, 185.3185741806024112 ) ) ;
#24893 = DIRECTION ( 'NONE',  ( -0.000000000000000000, -1.000000000000000000, -0.000000000000000000 ) ) ;
#24894 = ORIENTED_EDGE ( 'NONE', *, *, #91338, .T. ) ;
#24895 = CARTESIAN_POINT ( 'NONE',  ( 12.39573405564622988, 1517.151704408390060, 218.5685989363918225 ) ) ;
#24896 = CARTESIAN_POINT ( 'NONE',  ( -2.802202849542238638, 1406.777768078013423, 269.6500898821890928 ) ) ;
#24897 = EDGE_CURVE ( 'NONE', #77481, #31705, #81387, .T. ) ;
#24898 = CARTESIAN_POINT ( 'NONE',  ( -4.237005615526038937, 1508.610336687640029, 213.6558473927679813 ) ) ;
#24899 = DIRECTION ( 'NONE',  ( -1.000000000000000000, 0.000000000000000000, 0.000000000000000000 ) ) ;
#24900 = CARTESIAN_POINT ( 'NONE',  ( 10.98324908544952727, 1424.969403672227372, 138.3333100251041401 ) ) ;
#24901 = CARTESIAN_POINT ( 'NONE',  ( 11.79936509490000063, 1501.494630616190079, 210.6141959002089834 ) ) ;
#24902 = CARTESIAN_POINT ( 'NONE',  ( -12.89480376717877341, 1444.937738581603526, 186.1394114880380926 ) ) ;
#24903 = CARTESIAN_POINT ( 'NONE',  ( 13.89942583313499824, 1515.383078152259941, 193.2773559084670012 ) ) ;
#24904 = CARTESIAN_POINT ( 'NONE',  ( 16.66231036550703593, 1523.604703353109699, 180.4882076302513099 ) ) ;
#24905 = AXIS2_PLACEMENT_3D ( 'NONE', #94177, #10183, #44357 ) ;
#24906 = CARTESIAN_POINT ( 'NONE',  ( 3.394586470828380165, 1484.752177860970050, 220.4731790445629827 ) ) ;
#24907 = CARTESIAN_POINT ( 'NONE',  ( -7.859519671404137320, 1451.394139414346682, 152.9865962971728663 ) ) ;
#24908 = CARTESIAN_POINT ( 'NONE',  ( -7.135977434860000024, 1484.469329130889946, 199.5068056354589885 ) ) ;
#24909 = CARTESIAN_POINT ( 'NONE',  ( 24.88936805819999876, 1435.366663778739849, 135.7839653261980004 ) ) ;
#24910 = CARTESIAN_POINT ( 'NONE',  ( -12.93237811294222439, 1442.909190189631317, 169.4316757962859299 ) ) ;
#24911 = ORIENTED_EDGE ( 'NONE', *, *, #44245, .T. ) ;
#24912 = EDGE_CURVE ( 'NONE', #40123, #19916, #16811, .T. ) ;
#24913 = CARTESIAN_POINT ( 'NONE',  ( 0.5259141656908821183, 1414.913057855109855, 192.6235218337679953 ) ) ;
#24914 = CARTESIAN_POINT ( 'NONE',  ( -2.820494496349999825, 1409.011554225530062, 231.0801550522980108 ) ) ;
#24915 = ORIENTED_EDGE ( 'NONE', *, *, #65232, .F. ) ;
#24916 = ORIENTED_EDGE ( 'NONE', *, *, #28118, .F. ) ;
#24917 = CARTESIAN_POINT ( 'NONE',  ( 0.07780472814651649693, 1435.826791670900093, 227.5930969672339756 ) ) ;
#24918 = CARTESIAN_POINT ( 'NONE',  ( -15.37131439997841120, 1416.019838768163936, 206.9134041253344662 ) ) ;
#24920 = CARTESIAN_POINT ( 'NONE',  ( -10.70690149680000047, 1457.973036634730079, 211.8464313850780059 ) ) ;
#24919 = CARTESIAN_POINT ( 'NONE',  ( 2.254281109099999902, 1456.426090434989874, 219.5085644225989938 ) ) ;
#24921 = CARTESIAN_POINT ( 'NONE',  ( -8.920901164470000921, 1446.486419407289986, 213.5435801750889766 ) ) ;
#24922 = CARTESIAN_POINT ( 'NONE',  ( 4.151090981929720591, 1424.289371950179884, 184.6289891318990044 ) ) ;
#24923 = CARTESIAN_POINT ( 'NONE',  ( -12.29749543468789952, 1378.326909674530043, 209.9820058553110016 ) ) ;
#24924 = CONICAL_SURFACE ( 'NONE', #33828, 1.000000000000009104, 0.7853981633970000820 ) ;
#24925 = CARTESIAN_POINT ( 'NONE',  ( -2.502901717667406434, 1421.086235556830388, 185.1090482811913489 ) ) ;
#24926 = CARTESIAN_POINT ( 'NONE',  ( 6.917355500260000234, 1424.874072686129921, 213.3478120366190183 ) ) ;
#24927 = CARTESIAN_POINT ( 'NONE',  ( -24.82841969249999892, 1439.350353960880057, 210.4303024200779930 ) ) ;
#24928 = CARTESIAN_POINT ( 'NONE',  ( -3.402680045398430053, 1454.224139754760017, 199.2091369326260235 ) ) ;
#24929 = CARTESIAN_POINT ( 'NONE',  ( 9.090771158884999537, 1511.924334870729808, 220.7486671641670171 ) ) ;
#24930 = CARTESIAN_POINT ( 'NONE',  ( 7.871876822161247844, 1364.664245783809292, 209.6218459617148824 ) ) ;
#24931 = CARTESIAN_POINT ( 'NONE',  ( -21.85598295049956619, 1509.793014696267164, 229.6769293903243749 ) ) ;
#24933 = ORIENTED_EDGE ( 'NONE', *, *, #53214, .F. ) ;
#24932 = CARTESIAN_POINT ( 'NONE',  ( 3.902836639019999776, 1495.323243335989901, 220.8767694861990094 ) ) ;
#24934 = EDGE_LOOP ( 'NONE', ( #98640, #82453, #35888, #110222, #37312 ) ) ;
#24935 = CARTESIAN_POINT ( 'NONE',  ( -11.80507841927059864, 1428.482117788079904, 148.4348042808990158 ) ) ;
#24936 = DIRECTION ( 'NONE',  ( -3.828588921590000582E-16, 0.000000000000000000, 1.000000000000000000 ) ) ;
#24937 = CARTESIAN_POINT ( 'NONE',  ( -7.932950196699999346, 1470.889844930330128, 269.3427102504979871 ) ) ;
#24938 = DIRECTION ( 'NONE',  ( 0.2113515706023409990, -1.466546124833963756E-15, 0.9774101051267701790 ) ) ;
#24939 = CARTESIAN_POINT ( 'NONE',  ( -125.3156758022999924, 1368.558218059089995, 304.2218459572590064 ) ) ;
#24940 = CARTESIAN_POINT ( 'NONE',  ( 22.44565107540000071, 1519.913060387329779, 204.8661566055479852 ) ) ;
#24941 = EDGE_CURVE ( 'NONE', #21200, #82793, #26148, .T. ) ;
#24942 = CARTESIAN_POINT ( 'NONE',  ( -8.862552377930001057, 1384.556343050050145, 199.9458714445790122 ) ) ;
#24943 = SHAPE_REPRESENTATION_RELATIONSHIP ( 'NONE' , 'NONE' ,  #83713, #110798 ) ;
#24944 = CARTESIAN_POINT ( 'NONE',  ( -19.68294476550000027, 1431.113060387329824, 208.1462084707240194 ) ) ;
#24945 = CARTESIAN_POINT ( 'NONE',  ( 9.663829730717637290, 1367.635736277483147, 207.6218459616987673 ) ) ;
#24946 = CARTESIAN_POINT ( 'NONE',  ( -15.36549428884569934, 1420.414141511310163, 227.0219848988409979 ) ) ;
#24947 = CARTESIAN_POINT ( 'NONE',  ( -8.405094409318110138, 1406.273497697349967, 267.8245351791679809 ) ) ;
#24948 = EDGE_CURVE ( 'NONE', #53542, #44160, #78775, .T. ) ;
#24949 = B_SPLINE_CURVE_WITH_KNOTS ( 'NONE', 3,
 ( #28710, #88081, #21917, #97566, #104863, #28151, #19746, #72383, #80767, #87523 ),
 .UNSPECIFIED., .F., .F.,
 ( 4, 2, 2, 2, 4 ),
 ( 0.000000000000000000, 0.2500000000000000000, 0.5000000000000000000, 0.7500000000000000000, 1.000000000000000000 ),
 .UNSPECIFIED. ) ;
#24950 = CARTESIAN_POINT ( 'NONE',  ( -13.19292672295799917, 1435.822704715800000, 150.5785168366210200 ) ) ;
#24951 = ORIENTED_EDGE ( 'NONE', *, *, #40680, .T. ) ;
#24952 = CARTESIAN_POINT ( 'NONE',  ( -4.328706393743980030, 1515.093143318830244, 210.3280110370420175 ) ) ;
#24953 = CARTESIAN_POINT ( 'NONE',  ( 14.11724807090000056, 1444.027138891239929, 189.4625475421979957 ) ) ;
#24954 = ORIENTED_EDGE ( 'NONE', *, *, #66624, .F. ) ;
#24955 = ORIENTED_EDGE ( 'NONE', *, *, #86680, .T. ) ;
#24956 = ADVANCED_FACE ( 'NONE', ( #77669 ), #83100, .T. ) ;
#24957 = CARTESIAN_POINT ( 'NONE',  ( -22.01621720485236011, 1506.474306125368003, 209.2841005374792758 ) ) ;
#24958 = CARTESIAN_POINT ( 'NONE',  ( 5.441863932033339069, 1424.278296144239903, 193.3859063792879738 ) ) ;
#24959 = CARTESIAN_POINT ( 'NONE',  ( 0.7568986996720019622, 1516.805675336850072, 213.1530147380969993 ) ) ;
#24960 = CARTESIAN_POINT ( 'NONE',  ( 5.551188673975000043, 1510.480349266450048, 216.6723492941569873 ) ) ;
#24961 = EDGE_CURVE ( 'NONE', #51991, #48892, #20801, .T. ) ;
#24962 = CARTESIAN_POINT ( 'NONE',  ( -10.93162295028230169, 1470.132889486390013, 212.2376398131100075 ) ) ;
#24963 = B_SPLINE_SURFACE_WITH_KNOTS ( 'NONE', 4, 5, ( 
 ( #72444, #98165, #56172, #71924, #64047, #21437 ),
 ( #62403, #106575, #2498, #96531, #80282, #106037 ),
 ( #19805, #62973, #45599, #54010, #97086, #29314 ),
 ( #88141, #90311, #11429, #20898, #89224, #79740 ),
 ( #70816, #81354, #98720, #13589, #55648, #3597 ) ),
 .UNSPECIFIED., .F., .F., .F.,
 ( 5, 5 ),
 ( 6, 6 ),
 ( 6.493025399899999606, 14.36013212639999992 ),
 ( -4.440892098500000003E-16, 2.000000000000000000 ),
 .UNSPECIFIED. ) ;
#24964 = ORIENTED_EDGE ( 'NONE', *, *, #94018, .F. ) ;
#24965 = CARTESIAN_POINT ( 'NONE',  ( -113.4000000000000057, 1378.483856714079820, 302.0293834673589686 ) ) ;
#24966 = CARTESIAN_POINT ( 'NONE',  ( 6.939219482805000005, 1516.783701990830195, 203.3409846960470020 ) ) ;
#24967 = CIRCLE ( 'NONE', #87602, 2.000212125018253406 ) ;
#24968 = CARTESIAN_POINT ( 'NONE',  ( -28.40019560849999891, 1509.157491137930037, 208.4293195043489675 ) ) ;
#24969 = B_SPLINE_SURFACE_WITH_KNOTS ( 'NONE', 5, 5, ( 
 ( #29456, #3197, #37324, #61444, #11570, #70961 ),
 ( #95568, #45747, #105076, #54148, #2088, #63652 ),
 ( #27818, #61998, #28365, #19955, #79884, #12110 ),
 ( #71520, #105640, #28925, #97216, #20488, #31115 ),
 ( #72585, #30567, #91016, #56332, #90464, #14305 ),
 ( #49046, #4805, #57455, #81503, #99964, #106713 ) ),
 .UNSPECIFIED., .F., .F., .F.,
 ( 6, 6 ),
 ( 6, 6 ),
 ( 6.267575576645930013, 7.848944788839999909 ),
 ( 0.000000000000000000, 1.444929468818969998 ),
 .UNSPECIFIED. ) ;
#24970 = CARTESIAN_POINT ( 'NONE',  ( -0.4151546846821903003, 1512.187213306747481, 173.3106345060153046 ) ) ;
#24971 = CARTESIAN_POINT ( 'NONE',  ( -42.50641556133220433, 1384.590798579960165, 215.4612014908259710 ) ) ;
#24972 =( BOUNDED_SURFACE ( )  B_SPLINE_SURFACE ( 5, 2, ( 
 ( #91066, #64807, #98915, #107324, #82679, #56385, #106226 ),
 ( #13792, #47976, #82116, #5415, #39574, #46352, #40115 ),
 ( #73747, #12715, #21092, #107871, #38462, #99457, #22735 ),
 ( #65897, #5970, #100014, #54747, #88877, #37930, #72112 ),
 ( #29510, #63703, #46899, #55295, #97813, #89425, #81023 ),
 ( #4332, #23304, #24939, #34477, #108987, #59151, #109536 ),
 ( #32810, #24405, #15448, #93804, #58039, #66995, #76477 ),
 ( #7614, #93272, #8707, #16535, #350, #83227, #85408 ),
 ( #50726, #15995, #49639, #84323, #101105, #41227, #75397 ),
 ( #17081, #6517, #25502, #67550, #50197, #40670, #42885 ),
 ( #83776, #84857, #92177, #57499, #41770, #75927, #58589 ),
 ( #8157, #32272, #42324, #7070, #14900, #66454, #74843 ),
 ( #92719, #91624, #77042, #59692, #110080, #33356, #101652 ),
 ( #51276, #110630, #100567, #33913, #68107, #23848, #102222 ),
 ( #68652, #49092, #2006, #103884, #37242, #96036, #36141 ),
 ( #104438, #35572, #19307, #35021, #3113, #79254, #26048 ) ),
 .UNSPECIFIED., .F., .F., .F. ) 
 B_SPLINE_SURFACE_WITH_KNOTS ( ( 6, 3, 3, 1, 3, 6 ),
 ( 3, 2, 2, 3 ),
 ( 0.4214913904879999951, 6.500000000000000000, 18.08975840989999995, 46.86861349480000172, 60.45619974110000072, 75.86994138869999915 ),
 ( 2.628620570832299830, 3.141592653589790007, 4.712388980384689674, 5.770213224422659160 ),
 .UNSPECIFIED. ) 
 GEOMETRIC_REPRESENTATION_ITEM ( )  RATIONAL_B_SPLINE_SURFACE ( (
 ( 0.8711730262222689980, 0.9043503973638329363, 1.000000000000000000, 0.7071067811865480168, 1.000000000000000000, 0.8027563838226099424, 0.8711730262223420507),
 ( 0.8711730262222689980, 0.9043503973638329363, 1.000000000000000000, 0.7071067811865480168, 1.000000000000000000, 0.8027563838226099424, 0.8711730262223420507),
 ( 0.8711730262222689980, 0.9043503973638329363, 1.000000000000000000, 0.7071067811865480168, 1.000000000000000000, 0.8027563838226099424, 0.8711730262223420507),
 ( 0.8711730262222689980, 0.9043503973638329363, 1.000000000000000000, 0.7071067811865480168, 1.000000000000000000, 0.8027563838226099424, 0.8711730262223420507),
 ( 0.8711730262222689980, 0.9043503973638329363, 1.000000000000000000, 0.7071067811865480168, 1.000000000000000000, 0.8027563838226099424, 0.8711730262223420507),
 ( 0.8711730262222689980, 0.9043503973638329363, 1.000000000000000000, 0.7071067811865480168, 1.000000000000000000, 0.8027563838226099424, 0.8711730262223420507),
 ( 0.8711730262222689980, 0.9043503973638329363, 1.000000000000000000, 0.7071067811865480168, 1.000000000000000000, 0.8027563838226099424, 0.8711730262223420507),
 ( 0.8711730262222689980, 0.9043503973638329363, 1.000000000000000000, 0.7071067811865480168, 1.000000000000000000, 0.8027563838226099424, 0.8711730262223420507),
 ( 0.8711730262222689980, 0.9043503973638329363, 1.000000000000000000, 0.7071067811865480168, 1.000000000000000000, 0.8027563838226099424, 0.8711730262223420507),
 ( 0.8711730262222689980, 0.9043503973638329363, 1.000000000000000000, 0.7071067811865480168, 1.000000000000000000, 0.8027563838226099424, 0.8711730262223420507),
 ( 0.8711730262222689980, 0.9043503973638329363, 1.000000000000000000, 0.7071067811865480168, 1.000000000000000000, 0.8027563838226099424, 0.8711730262223420507),
 ( 0.8711730262222689980, 0.9043503973638329363, 1.000000000000000000, 0.7071067811865480168, 1.000000000000000000, 0.8027563838226099424, 0.8711730262223420507),
 ( 0.8711730262222689980, 0.9043503973638329363, 1.000000000000000000, 0.7071067811865480168, 1.000000000000000000, 0.8027563838226099424, 0.8711730262223420507),
 ( 0.8711730262222689980, 0.9043503973638329363, 1.000000000000000000, 0.7071067811865480168, 1.000000000000000000, 0.8027563838226099424, 0.8711730262223420507),
 ( 0.8711730262222689980, 0.9043503973638329363, 1.000000000000000000, 0.7071067811865480168, 1.000000000000000000, 0.8027563838226099424, 0.8711730262223420507),
 ( 0.8711730262222689980, 0.9043503973638329363, 1.000000000000000000, 0.7071067811865480168, 1.000000000000000000, 0.8027563838226099424, 0.8711730262223420507) ) ) 
 REPRESENTATION_ITEM ( '' )  SURFACE ( )  );
#24973 = CARTESIAN_POINT ( 'NONE',  ( -2.605301666119999915, 1407.938395048229950, 196.0967308190980134 ) ) ;
#24974 = CARTESIAN_POINT ( 'NONE',  ( -33.28034951413921760, 1512.187213306747481, 217.4407153818824838 ) ) ;
#24975 = CIRCLE ( 'NONE', #51797, 1.999999999999998668 ) ;
#24977 = VERTEX_POINT ( 'NONE', #29458 ) ;
#24976 = CARTESIAN_POINT ( 'NONE',  ( 15.53981991842809585, 1506.512156833535528, 193.4804600942033801 ) ) ;
#24978 = CARTESIAN_POINT ( 'NONE',  ( 3.973077635731362633, 1441.765784966813499, 217.0264645807230011 ) ) ;
#24979 = CARTESIAN_POINT ( 'NONE',  ( 27.25446695569999989, 1488.690170597129736, 210.3317447754679961 ) ) ;
#24980 = CARTESIAN_POINT ( 'NONE',  ( -67.28024477550941640, 1379.744889785224586, 278.5190817744257856 ) ) ;
#24981 = CARTESIAN_POINT ( 'NONE',  ( 1.491506560153238015, 1511.187213306747708, 175.5704429466618421 ) ) ;
#24982 = CARTESIAN_POINT ( 'NONE',  ( -4.987078451384999944, 1508.551704408389924, 205.1631965221770031 ) ) ;
#24983 = B_SPLINE_CURVE_WITH_KNOTS ( 'NONE', 3,
 ( #106030, #46690, #29306, #29854, #12511, #90301 ),
 .UNSPECIFIED., .F., .F.,
 ( 4, 2, 4 ),
 ( 2.168404344971008868E-18, 0.003924659484584390456, 0.007849318969168777443 ),
 .UNSPECIFIED. ) ;
#24984 = ADVANCED_FACE ( 'NONE', ( #12669 ), #13192, .T. ) ;
#24986 = CARTESIAN_POINT ( 'NONE',  ( -5.770883602015000058, 1516.603620185149794, 211.4160555996369908 ) ) ;
#24985 = VECTOR ( 'NONE', #13481, 1000.000000000000227 ) ;
#24987 = CARTESIAN_POINT ( 'NONE',  ( -68.74238773750001030, 1379.747863086420011, 280.1036906554590473 ) ) ;
#24988 = CARTESIAN_POINT ( 'NONE',  ( -6.016757112579999678, 1449.943096111989917, 209.5823369759550019 ) ) ;
#24989 = CARTESIAN_POINT ( 'NONE',  ( 18.80368967275888181, 1425.915424793447983, 225.1658295344082603 ) ) ;
#24990 = CARTESIAN_POINT ( 'NONE',  ( 4.612671339784999880, 1516.783665406140017, 208.3654117178780041 ) ) ;
#24991 = EDGE_CURVE ( 'NONE', #96085, #83875, #20630, .T. ) ;
#24992 = ORIENTED_EDGE ( 'NONE', *, *, #10317, .F. ) ;
#24993 = CARTESIAN_POINT ( 'NONE',  ( -1.906499758064230099E-08, 1516.051704408390151, 209.1218459511669892 ) ) ;
#24994 = B_SPLINE_CURVE_WITH_KNOTS ( 'NONE', 5,
 ( #40086, #92144, #30020, #47400, #65860, #81522, #49061, #14870, #107840 ),
 .UNSPECIFIED., .F., .F.,
 ( 6, 3, 6 ),
 ( 0.000000000000000000, 0.4402423755028501695, 1.000000000000000000 ),
 .UNSPECIFIED. ) ;
#24995 = CARTESIAN_POINT ( 'NONE',  ( -10.17795364999999919, 1472.274701162789825, 208.9856853541390080 ) ) ;
#24996 = CARTESIAN_POINT ( 'NONE',  ( -18.72407526530000155, 1458.246115540929850, 227.3156487912980026 ) ) ;
#24997 = ORIENTED_EDGE ( 'NONE', *, *, #60815, .F. ) ;
#24999 = B_SPLINE_CURVE_WITH_KNOTS ( 'NONE', 3,
 ( #88792, #45155, #18802, #27227, #10981, #44590, #63082, #96645, #53554, #37839, #20455, #36183, #19354, #19914, #54664, #27775, #96079, #80395, #2606, #88243, #61407, #11536, #3159, #95530, #104482, #60857, #94982, #45711 ),
 .UNSPECIFIED., .F., .F.,
 ( 4, 2, 2, 1, 2, 2, 2, 1, 1, 1, 1, 1, 2, 2, 2, 2, 4 ),
 ( 0.000000000000000000, 0.2499999999999414912, 0.3749999999999151234, 0.4374999999999019118, 0.4687499999998977485, 0.4999999999998935296, 0.6249999999998722133, 0.6874999999998615552, 0.7187499999998566702, 0.7343749999998538946, 0.7421874999998498978, 0.7460937499998477884, 0.7480468749998462341, 0.7499999999998446798, 0.8749999999999199529, 0.9374999999999600320, 1.000000000000000000 ),
 .UNSPECIFIED. ) ;
#24998 = CARTESIAN_POINT ( 'NONE',  ( -3.059311260596259352, 1525.343710797494396, 241.3958505225228066 ) ) ;
#25000 = CARTESIAN_POINT ( 'NONE',  ( 12.87808539635419969, 1435.336471212810011, 150.5288829532699992 ) ) ;
#25001 = CARTESIAN_POINT ( 'NONE',  ( 12.94866893597960100, 1469.001480463319922, 231.3866629679569940 ) ) ;
#25002 = CARTESIAN_POINT ( 'NONE',  ( -4.218809310280000169, 1413.234397187750119, 207.6255014893789905 ) ) ;
#25003 = CARTESIAN_POINT ( 'NONE',  ( 12.77587743780000018, 1416.568813547830132, 222.7009457741980327 ) ) ;
#25004 = B_SPLINE_CURVE_WITH_KNOTS ( 'NONE', 3,
 ( #88757, #44549, #71446, #10376, #11500, #3672 ),
 .UNSPECIFIED., .F., .F.,
 ( 4, 2, 4 ),
 ( 0.000000000000000000, 0.5000000000000000000, 1.000000000000000000 ),
 .UNSPECIFIED. ) ;
#25005 = CARTESIAN_POINT ( 'NONE',  ( 5.387574631020000560, 1487.707168882490123, 198.8464060204989892 ) ) ;
#25006 = DIRECTION ( 'NONE',  ( -1.836970198721029688E-16, -1.000000000000000000, 0.000000000000000000 ) ) ;
#25007 = CARTESIAN_POINT ( 'NONE',  ( 4.221851273025380102, 1441.601972411079942, 170.0739392326869961 ) ) ;
#25008 = VECTOR ( 'NONE', #16923, 1000.000000000000114 ) ;
#25010 = CARTESIAN_POINT ( 'NONE',  ( 41.66134420550000073, 1443.796851579070108, 135.6885409488979803 ) ) ;
#25009 = CARTESIAN_POINT ( 'NONE',  ( -2.286446363765000100, 1517.042661899400173, 213.7475398352470108 ) ) ;
#25011 = CARTESIAN_POINT ( 'NONE',  ( 21.39772446809999806, 1509.704964749530063, 188.4542719777979869 ) ) ;
#25012 = CARTESIAN_POINT ( 'NONE',  ( 5.005071008295000290, 1516.710692850270107, 216.4473877573669824 ) ) ;
#25013 = ORIENTED_EDGE ( 'NONE', *, *, #47009, .F. ) ;
#25014 = DIRECTION ( 'NONE',  ( 1.755985294532469921E-16, -1.000000000000000000, 1.338183447452831989E-16 ) ) ;
#25015 = CARTESIAN_POINT ( 'NONE',  ( -17.13546891859999732, 1420.255476167079905, 203.8193908791089939 ) ) ;
#25016 = VERTEX_POINT ( 'NONE', #19957 ) ;
#25017 = CARTESIAN_POINT ( 'NONE',  ( 0.6025240147529998813, 1420.628247535429864, 182.8370771391979872 ) ) ;
#25018 = CARTESIAN_POINT ( 'NONE',  ( -17.13806402160000175, 1505.874291994889973, 209.1215054657809844 ) ) ;
#25019 = CARTESIAN_POINT ( 'NONE',  ( 3.355802132529028370, 1523.843271061949054, 176.1812215589180539 ) ) ;
#25020 = CARTESIAN_POINT ( 'NONE',  ( 9829.078716723830439, 2833.596074015639715, -1083.720023828199828 ) ) ;
#25021 = CARTESIAN_POINT ( 'NONE',  ( -11.20494725878380038, 1471.318229655669938, 206.9400762973899930 ) ) ;
#25022 = CARTESIAN_POINT ( 'NONE',  ( -5.036431363644181758, 1508.232884704754269, 220.4119323058353928 ) ) ;
#25023 = AXIS2_PLACEMENT_3D ( 'NONE', #73060, #29933, #20972 ) ;
#25024 = CARTESIAN_POINT ( 'NONE',  ( 18.88752285780000051, 1416.568813549730066, 210.6689649478780098 ) ) ;
#25025 = CARTESIAN_POINT ( 'NONE',  ( 18.03158832033268411, 1424.671894330125269, 224.6703068079623051 ) ) ;
#25026 = DIRECTION ( 'NONE',  ( 3.828588921590000582E-16, 0.000000000000000000, 1.000000000000000000 ) ) ;
#25027 = CARTESIAN_POINT ( 'NONE',  ( -4.989973902650000070, 1442.756953654919926, 150.3769280849980134 ) ) ;
#25028 = CARTESIAN_POINT ( 'NONE',  ( 44.98655287106430478, 1440.913060372329937, 265.4537301890219965 ) ) ;
#25030 = CARTESIAN_POINT ( 'NONE',  ( 11.41971426342585261, 1507.432269439749689, 184.3360310533326185 ) ) ;
#25029 = CARTESIAN_POINT ( 'NONE',  ( -13.42843082903999985, 1417.384064304789945, 201.4800834699910297 ) ) ;
#25031 = CARTESIAN_POINT ( 'NONE',  ( 33.42844755917195698, 1501.977400791986611, 222.1271778627166213 ) ) ;
#25032 = ORIENTED_EDGE ( 'NONE', *, *, #93122, .F. ) ;
#25033 = ORIENTED_EDGE ( 'NONE', *, *, #94906, .F. ) ;
#25034 = CARTESIAN_POINT ( 'NONE',  ( 1.547519921729459957, 1416.512142023790148, 190.2622265145609788 ) ) ;
#25035 = CARTESIAN_POINT ( 'NONE',  ( -18.44417578049999662, 1443.022497311789948, 205.4505639164189859 ) ) ;
#25036 = CARTESIAN_POINT ( 'NONE',  ( -27.72858371599999927, 1508.599279862329922, 210.5587065999479819 ) ) ;
#25037 = DIRECTION ( 'NONE',  ( -1.755985294532469921E-16, 1.000000000000000000, -1.338183447452831989E-16 ) ) ;
#25038 = CARTESIAN_POINT ( 'NONE',  ( 6.680091234600673111, 1440.117289966305634, 185.5007468843921004 ) ) ;
#25039 = DIRECTION ( 'NONE',  ( -0.9958668876188416785, 0.000000000000000000, 0.09082478816029017354 ) ) ;
#25040 = DIRECTION ( 'NONE',  ( -0.7414773880254689198, 0.000000000000000000, 0.6709778558543705307 ) ) ;
#25041 = CARTESIAN_POINT ( 'NONE',  ( 12.98226561589999939, 1414.913060387329779, 198.3280246956980193 ) ) ;
#25042 = CARTESIAN_POINT ( 'NONE',  ( -68.92988442230469559, 1383.786281746080022, 293.5620293669300054 ) ) ;
#25043 = CARTESIAN_POINT ( 'NONE',  ( -0.02753319299389999850, 1452.474300611429953, 153.7510437628980071 ) ) ;
#25044 = DIRECTION ( 'NONE',  ( -0.05481995565582255259, -0.1266070825601602612, -0.9904369839154324451 ) ) ;
#25045 = CARTESIAN_POINT ( 'NONE',  ( 11.13874570262469987, 1491.363259792560029, 209.7171445221170245 ) ) ;
#25047 = EDGE_LOOP ( 'NONE', ( #24002, #24823, #102925 ) ) ;
#25046 = CARTESIAN_POINT ( 'NONE',  ( 0.5688480841909990815, 1456.339328993690060, 218.9825356867290225 ) ) ;
#25048 = CYLINDRICAL_SURFACE ( 'NONE', #77177, 1.999999999999912514 ) ;
#25049 = B_SPLINE_SURFACE_WITH_KNOTS ( 'NONE', 5, 1, ( 
 ( #100736, #60431 ),
 ( #109712, #15073 ),
 ( #58218, #50915 ),
 ( #49269, #75023 ),
 ( #15615, #7252 ),
 ( #83396, #101836 ),
 ( #24572, #85046 ),
 ( #6694, #109174 ),
 ( #32460, #66635 ) ),
 .UNSPECIFIED., .F., .F., .F.,
 ( 6, 3, 6 ),
 ( 2, 2 ),
 ( 0.000000000000000000, 7.657578151330000082, 15.28728567399999960 ),
 ( 0.000000000000000000, 14.00000771804140065 ),
 .UNSPECIFIED. ) ;
#25050 = CARTESIAN_POINT ( 'NONE',  ( -51.40360984529999655, 1380.961789557690054, 260.0749407918589782 ) ) ;
#25051 = CARTESIAN_POINT ( 'NONE',  ( -2.418973636230000057, 1431.127469431690088, 217.1544448978289950 ) ) ;
#25052 = ORIENTED_EDGE ( 'NONE', *, *, #55754, .F. ) ;
#25053 = VERTEX_POINT ( 'NONE', #12112 ) ;
#25054 = CARTESIAN_POINT ( 'NONE',  ( 18.96841931012820126, 1508.814919057110046, 230.1294357287169987 ) ) ;
#25055 = LINE ( 'NONE', #83328, #2764 ) ;
#25056 = CARTESIAN_POINT ( 'NONE',  ( 40.27297052727078608, 1443.533075565821719, 137.1070167546214122 ) ) ;
#25058 = FACE_OUTER_BOUND ( 'NONE', #67611, .T. ) ;
#25057 = CARTESIAN_POINT ( 'NONE',  ( -11.71103087170000023, 1438.058396846869982, 147.7520216503980066 ) ) ;
#25059 = CIRCLE ( 'NONE', #69798, 2.000000000000001776 ) ;
#25060 = CARTESIAN_POINT ( 'NONE',  ( -10.17701436070000121, 1462.839837603090018, 206.1633447294989878 ) ) ;
#25061 = CARTESIAN_POINT ( 'NONE',  ( -109.1959892269999983, 1382.683563420089968, 297.4542923961590191 ) ) ;
#25062 = CARTESIAN_POINT ( 'NONE',  ( -22.08523867432794674, 1523.530870145311610, 233.8225105631221084 ) ) ;
#25063 = FACE_OUTER_BOUND ( 'NONE', #43188, .T. ) ;
#25064 = CARTESIAN_POINT ( 'NONE',  ( -14.07384742208520123, 1508.551704408389924, 215.7439646766590045 ) ) ;
#25065 = CARTESIAN_POINT ( 'NONE',  ( 4.276093308640000146, 1410.438556067529817, 186.1213257426980192 ) ) ;
#25066 = FACE_OUTER_BOUND ( 'NONE', #78960, .T. ) ;
#25067 = CARTESIAN_POINT ( 'NONE',  ( -8.104522071583946996, 1514.095142040220935, 201.7913770512302563 ) ) ;
#25068 = CARTESIAN_POINT ( 'NONE',  ( 10.96966797059999799, 1432.360037085230033, 151.7701368415980028 ) ) ;
#25069 = VECTOR ( 'NONE', #105572, 1000.000000000000114 ) ;
#25070 = CARTESIAN_POINT ( 'NONE',  ( -23.39765034550000067, 1451.953609269630078, 140.1874901743979933 ) ) ;
#25071 = CARTESIAN_POINT ( 'NONE',  ( 0.7760999072929999354, 1465.000431637629845, 237.6961790583980019 ) ) ;
#25072 = VERTEX_POINT ( 'NONE', #3199 ) ;
#25073 = CARTESIAN_POINT ( 'NONE',  ( 22.26425649109999938, 1476.353502809590054, 209.6940367010219859 ) ) ;
#25074 = CARTESIAN_POINT ( 'NONE',  ( 5.015673624609470416, 1509.218235651550003, 238.8061437059149910 ) ) ;
#25075 = FACE_OUTER_BOUND ( 'NONE', #55392, .T. ) ;
#25076 = DIRECTION ( 'NONE',  ( -0.000000000000000000, -1.000000000000000000, -0.000000000000000000 ) ) ;
#25077 = CARTESIAN_POINT ( 'NONE',  ( 14.48064082319999812, 1430.158253430729928, 190.5189584202980200 ) ) ;
#25078 = CARTESIAN_POINT ( 'NONE',  ( -5.849681485717489748E-09, 1472.204232032089976, 259.4648360949830135 ) ) ;
#25079 = EDGE_CURVE ( 'NONE', #17806, #75555, #54286, .T. ) ;
#25080 = CARTESIAN_POINT ( 'NONE',  ( 9.326420915248059273, 1460.944044860930035, 206.0389257843339976 ) ) ;
#25081 = CARTESIAN_POINT ( 'NONE',  ( -1.124394188919999982, 1416.535385209630022, 228.0704250668979682 ) ) ;
#25082 = CARTESIAN_POINT ( 'NONE',  ( -19.14812029890000034, 1505.318613837190014, 209.0594768593419985 ) ) ;
#25083 = CARTESIAN_POINT ( 'NONE',  ( -1.756482616760000059, 1475.875686602589894, 198.5418275763989868 ) ) ;
#25084 = CARTESIAN_POINT ( 'NONE',  ( -106.9425809150000077, 1387.746739512440172, 310.0310650472589487 ) ) ;
#25085 = CARTESIAN_POINT ( 'NONE',  ( -7.679927622135040544, 1511.009256124219974, 214.7417639624250114 ) ) ;
#25086 = CARTESIAN_POINT ( 'NONE',  ( -0.8025614321512887228, 1359.202926620322387, 210.6218459617030021 ) ) ;
#25087 = CARTESIAN_POINT ( 'NONE',  ( -45.77496015592539891, 1438.861072743580053, 268.7587536533030175 ) ) ;
#25088 = CARTESIAN_POINT ( 'NONE',  ( 13.47402130151080080, 1508.487106454680088, 233.3457994875830082 ) ) ;
#25089 = CARTESIAN_POINT ( 'NONE',  ( -9.148257661150001496, 1423.748799908730007, 207.7944249153989915 ) ) ;
#25090 = CARTESIAN_POINT ( 'NONE',  ( -1.127928371535000140, 1516.989863902050047, 209.1319708558790182 ) ) ;
#25091 = AXIS2_PLACEMENT_3D ( 'NONE', #43823, #105388, #10212 ) ;
#25092 = CARTESIAN_POINT ( 'NONE',  ( -5.451417714189999764, 1437.905383210109903, 154.7243314242980148 ) ) ;
#25093 = B_SPLINE_SURFACE_WITH_KNOTS ( 'NONE', 5, 5, ( 
 ( #75316, #32738, #66918, #59064, #42249, #93187, #33836, #59608, #95275 ),
 ( #18537, #52732, #53291, #79588, #96375, #80119, #89067, #44334, #11817 ),
 ( #20202, #87429, #46542, #37569, #2893, #97473, #37011, #71204, #70110 ),
 ( #29709, #72292, #10159, #71770, #63894, #19654, #96934, #44897, #61697 ),
 ( #54400, #88533, #105886, #36460, #45987, #105325, #28618, #86867, #10725 ),
 ( #79046, #27510, #53858, #95819, #63356, #45446, #98009, #62821, #12352 ),
 ( #19087, #1789, #3438, #28060, #29167, #20743, #87995, #35927, #54938 ),
 ( #80677, #3989, #38114, #70659, #78476, #106425, #2348, #21280, #62250 ),
 ( #104775, #11282, #104223, #64445, #48741, #98562, #49286, #23508, #6158 ),
 ( #55488, #31912, #21830, #40313, #30808, #56029, #47626, #99102, #22380 ),
 ( #82866, #90154, #83415, #57700, #74496, #108624, #90713, #4525, #64986 ),
 ( #66101, #13436, #81208, #100228, #75041, #38659, #56580, #99651, #22942 ) ),
 .UNSPECIFIED., .F., .F., .F.,
 ( 6, 3, 3, 6 ),
 ( 6, 3, 6 ),
 ( 0.000000000000000000, 17.84603210599999912, 40.51038747020000130, 67.03953034199999195 ),
 ( 253.0908261149999987, 295.2726304679999885, 337.4544348200000172 ),
 .UNSPECIFIED. ) ;
#25094 = DIRECTION ( 'NONE',  ( 0.000000000000000000, 0.000000000000000000, 1.000000000000000000 ) ) ;
#25095 = CARTESIAN_POINT ( 'NONE',  ( 7.438626391280539707, 1426.170359921889940, 212.4786103371660033 ) ) ;
#25096 = CARTESIAN_POINT ( 'NONE',  ( -25.64740235160000026, 1451.776718248130010, 136.1276997542979927 ) ) ;
#25097 = EDGE_LOOP ( 'NONE', ( #62548, #90127, #26359, #98115 ) ) ;
#25098 = EDGE_CURVE ( 'NONE', #5750, #64661, #93940, .T. ) ;
#25099 = CARTESIAN_POINT ( 'NONE',  ( 16.11555329659999813, 1425.418868056930023, 217.2236249432280033 ) ) ;
#25101 = CARTESIAN_POINT ( 'NONE',  ( -15.23581460173349988, 1513.231391186749988, 223.2758740717220007 ) ) ;
#25100 = CARTESIAN_POINT ( 'NONE',  ( -2.340423001224519517, 1525.425686270222059, 176.3541592074136872 ) ) ;
#25102 = CARTESIAN_POINT ( 'NONE',  ( -1.836122418284559910, 1419.498329967660084, 185.6833343230359787 ) ) ;
#25103 = VECTOR ( 'NONE', #67057, 1000.000000000000000 ) ;
#25104 = DIRECTION ( 'NONE',  ( 0.5450600352768949497, -0.8383970168982891602, 0.000000000000000000 ) ) ;
#25105 = CARTESIAN_POINT ( 'NONE',  ( 3.165859372309999920, 1420.089904188009996, 205.0081603533590169 ) ) ;
#25106 = ADVANCED_FACE ( 'NONE', ( #46848 ), #80977, .T. ) ;
#25107 = CARTESIAN_POINT ( 'NONE',  ( -17.74177080272650997, 1410.893628021574614, 194.9094938642074339 ) ) ;
#25108 = DIRECTION ( 'NONE',  ( 1.755985294532464991E-16, -1.000000000000000000, 1.338183447452830017E-16 ) ) ;
#25109 = ORIENTED_EDGE ( 'NONE', *, *, #100767, .F. ) ;
#25110 = CARTESIAN_POINT ( 'NONE',  ( -4.375893703611340335, 1407.803658742089965, 270.1335120727630397 ) ) ;
#25111 = CARTESIAN_POINT ( 'NONE',  ( 8.985183074850001006, 1417.398376849329907, 230.5159961331980014 ) ) ;
#25112 = CARTESIAN_POINT ( 'NONE',  ( -2.701663630316083697, 1448.935076026784827, 184.0154241898988232 ) ) ;
#25113 = EDGE_LOOP ( 'NONE', ( #50777, #84559, #73723, #43139 ) ) ;
#25114 = ORIENTED_EDGE ( 'NONE', *, *, #39849, .F. ) ;
#25115 = PLANE ( 'NONE',  #74240 ) ;
#25116 = CARTESIAN_POINT ( 'NONE',  ( 0.01764073193947529941, 1409.855412122559983, 185.0387969038189908 ) ) ;
#25117 = FACE_OUTER_BOUND ( 'NONE', #44094, .T. ) ;
#25118 = CARTESIAN_POINT ( 'NONE',  ( 29.30029655192931770, 1525.907212628473872, 221.3719603026171114 ) ) ;
#25119 = CARTESIAN_POINT ( 'NONE',  ( -19.92563280199049913, 1472.425994622909911, 193.2981305741199947 ) ) ;
#25120 = CARTESIAN_POINT ( 'NONE',  ( 4.491284065468319930, 1508.884228858900087, 211.6097700378190041 ) ) ;
#25121 = ORIENTED_EDGE ( 'NONE', *, *, #72708, .T. ) ;
#25122 = CARTESIAN_POINT ( 'NONE',  ( 32.98914153328620102, 1465.411049489700190, 266.7912572958550186 ) ) ;
#25123 = CARTESIAN_POINT ( 'NONE',  ( -10.37958022962100024, 1391.913060387289988, 204.5402316943800258 ) ) ;
#25124 = DIRECTION ( 'NONE',  ( -1.987898964669120000E-13, 0.000000000000000000, 1.000000000000000000 ) ) ;
#25125 = CARTESIAN_POINT ( 'NONE',  ( -4.623788007495000407, 1516.947419719950176, 205.6726967363569827 ) ) ;
#25126 = EDGE_CURVE ( 'NONE', #32742, #77650, #14179, .T. ) ;
#25127 = ORIENTED_EDGE ( 'NONE', *, *, #68595, .T. ) ;
#25128 = CARTESIAN_POINT ( 'NONE',  ( 18.46594417149771417, 1458.839898657651474, 227.6586181968465041 ) ) ;
#25129 = CARTESIAN_POINT ( 'NONE',  ( 15.22870587831669908, 1512.406412988020065, 196.0902778419350057 ) ) ;
#25130 = VECTOR ( 'NONE', #71564, 1000.000000000000000 ) ;
#25131 = CARTESIAN_POINT ( 'NONE',  ( -12.84239665067440050, 1435.935719077439899, 150.8114796122480072 ) ) ;
#25132 = ORIENTED_EDGE ( 'NONE', *, *, #57524, .T. ) ;
#25133 = CARTESIAN_POINT ( 'NONE',  ( 4.554948924558070544, 1508.731372610989865, 206.6339222123599768 ) ) ;
#25134 = CARTESIAN_POINT ( 'NONE',  ( 4.755330316939417656, 1434.245644035614077, 202.0163905304680441 ) ) ;
#25135 = CARTESIAN_POINT ( 'NONE',  ( -4.554659022055290052, 1508.551704408389924, 213.0139469008600202 ) ) ;
#25136 = CARTESIAN_POINT ( 'NONE',  ( -9.852819229099999632, 1386.608977785310117, 199.8799424390689978 ) ) ;
#25137 = CARTESIAN_POINT ( 'NONE',  ( 7.450392350589999602, 1422.132270461650251, 195.6329181414990046 ) ) ;
#25138 = CARTESIAN_POINT ( 'NONE',  ( 22.70509004431190192, 1409.705939603270053, 209.2982552845940063 ) ) ;
#25139 = CARTESIAN_POINT ( 'NONE',  ( 10.81956120968489898, 1478.925883878960121, 205.9529814458820169 ) ) ;
#25140 = CARTESIAN_POINT ( 'NONE',  ( 8.591778955288280173, 1409.213091919750013, 189.5189649568119989 ) ) ;
#25142 = CARTESIAN_POINT ( 'NONE',  ( 28.54400548274967520, 1526.382868172863482, 219.8019517411713082 ) ) ;
#25141 = CARTESIAN_POINT ( 'NONE',  ( 30.31052258194585036, 1523.604703353109926, 195.7506062427367794 ) ) ;
#25143 = CARTESIAN_POINT ( 'NONE',  ( -16.55212241054000089, 1524.756004293092019, 180.7964624130805191 ) ) ;
#25144 = CARTESIAN_POINT ( 'NONE',  ( -12.97372998250000009, 1379.811305717160167, 213.3571419713289856 ) ) ;
#25145 = CARTESIAN_POINT ( 'NONE',  ( 2.389876875773846887, 1525.253972588464876, 242.0501992864865883 ) ) ;
#25146 = ORIENTED_EDGE ( 'NONE', *, *, #80204, .F. ) ;
#25147 = CARTESIAN_POINT ( 'NONE',  ( 12.33030208333319955, 1415.427621830080170, 221.6250288674360149 ) ) ;
#25148 = CONICAL_SURFACE ( 'NONE', #23400, 12.49999999999999467, 0.02617993877989872875 ) ;
#25149 = CARTESIAN_POINT ( 'NONE',  ( 5.257080573758883268, 1517.051704408389924, 218.9984329930441902 ) ) ;
#25150 = DIRECTION ( 'NONE',  ( -1.755985294532469921E-16, 1.000000000000000000, -1.338183447452831989E-16 ) ) ;
#25151 = CARTESIAN_POINT ( 'NONE',  ( -11.20689792730000001, 1390.718236914620093, 203.7291915516989889 ) ) ;
#25152 =( BOUNDED_SURFACE ( )  B_SPLINE_SURFACE ( 3, 2, ( 
 ( #39187, #3422, #22922 ),
 ( #48169, #31343, #47067 ),
 ( #47609, #29692, #21814 ),
 ( #63337, #55470, #89597 ),
 ( #20725, #4508, #80102 ),
 ( #71753, #81191, #63876 ),
 ( #3974, #56013, #38098 ),
 ( #13420, #12889, #72275 ),
 ( #11799, #73918, #29150 ),
 ( #38641, #72817, #54921 ) ),
 .UNSPECIFIED., .F., .F., .F. ) 
 B_SPLINE_SURFACE_WITH_KNOTS ( ( 4, 2, 2, 2, 4 ),
 ( 3, 3 ),
 ( 0.000000000000000000, 0.3926990816987241395, 0.7853981633974482790, 1.178097245096172418, 1.570796326794896558 ),
 ( 0.000000000000000000, 1.000000000000000000 ),
 .UNSPECIFIED. ) 
 GEOMETRIC_REPRESENTATION_ITEM ( )  RATIONAL_B_SPLINE_SURFACE ( (
 ( 1.000000000000000000, 0.7763623250684303922, 1.000000000000000000),
 ( 1.000000000000000000, 0.7763684247035209651, 1.000000000000000000),
 ( 1.000000000000000000, 0.7746454561797311289, 1.000000000000000000),
 ( 1.000000000000000000, 0.7679730451973156846, 1.000000000000000000),
 ( 1.000000000000000000, 0.7630177051950561840, 1.000000000000000000),
 ( 1.000000000000000000, 0.7504512394524429642, 1.000000000000000000),
 ( 1.000000000000000000, 0.7428408967926065642, 1.000000000000000000),
 ( 1.000000000000000000, 0.7259222650911398844, 1.000000000000000000),
 ( 1.000000000000000000, 0.7166207884818885931, 1.000000000000000000),
 ( 1.000000000000000000, 0.7071067811865857644, 1.000000000000000000) ) ) 
 REPRESENTATION_ITEM ( '' )  SURFACE ( )  );
#25153 = CARTESIAN_POINT ( 'NONE',  ( 8.877746755106400656, 1422.885059916349974, 212.4210226277380116 ) ) ;
#25154 = CARTESIAN_POINT ( 'NONE',  ( 10.94861482359589999, 1423.583840232799957, 203.2386481640710088 ) ) ;
#25155 = CARTESIAN_POINT ( 'NONE',  ( 13.34862394727499968, 1427.267748017370195, 221.9543608694049794 ) ) ;
#25156 = CARTESIAN_POINT ( 'NONE',  ( 1.176836406099999899E-14, 1468.063065667029832, 262.6648722463980334 ) ) ;
#25157 = CARTESIAN_POINT ( 'NONE',  ( -9.025258063816389509, 1384.071087798369945, 218.5842451692199973 ) ) ;
#25158 = CARTESIAN_POINT ( 'NONE',  ( 11.15583049490000001, 1433.756731305959875, 151.6440224492980064 ) ) ;
#25159 = CARTESIAN_POINT ( 'NONE',  ( 3.804422478559999821, 1458.952956299430070, 234.3916895697979612 ) ) ;
#25160 = CARTESIAN_POINT ( 'NONE',  ( -10.53669503535969909, 1461.974058373740036, 209.9839194512770177 ) ) ;
#25161 = CIRCLE ( 'NONE', #41337, 12.50000000000001066 ) ;
#25162 = CARTESIAN_POINT ( 'NONE',  ( -1.636741614903409969, 1469.777368438049962, 219.0527109355280118 ) ) ;
#25163 = CARTESIAN_POINT ( 'NONE',  ( 5.896221088274059774, 1466.153673113790092, 217.3008473279559780 ) ) ;
#25164 = CARTESIAN_POINT ( 'NONE',  ( 12.93261306534300026, 1416.826860677879949, 221.7400780573829877 ) ) ;
#25165 = CIRCLE ( 'NONE', #23346, 29.84605316875909153 ) ;
#25166 = CARTESIAN_POINT ( 'NONE',  ( -13.92276408390000064, 1412.700534325730132, 227.1776661936980020 ) ) ;
#25167 = CARTESIAN_POINT ( 'NONE',  ( 0.05083158678110080014, 1508.992420415059996, 238.9842585609989953 ) ) ;
#25168 = CARTESIAN_POINT ( 'NONE',  ( 23.61553526439999828, 1410.914738107329867, 211.4616251689280091 ) ) ;
#25169 = CARTESIAN_POINT ( 'NONE',  ( 1.107190807272493860, 1477.934341428328935, 198.7592707807304748 ) ) ;
#25170 = CARTESIAN_POINT ( 'NONE',  ( 25.83285470672302253, 1436.659813480326420, 137.0377997444614380 ) ) ;
#25171 = CARTESIAN_POINT ( 'NONE',  ( -19.09790268268400126, 1508.458003811930212, 210.0050661408479868 ) ) ;
#25172 = CARTESIAN_POINT ( 'NONE',  ( 12.72754940664999879, 1426.782577209239889, 204.7399120111390118 ) ) ;
#25173 = CARTESIAN_POINT ( 'NONE',  ( -2.775555772024459689, 1468.867611297260055, 187.4507004145660005 ) ) ;
#25174 = CARTESIAN_POINT ( 'NONE',  ( -1.703779643355000095, 1517.057265928030120, 213.1670284501570052 ) ) ;
#25176 =( BOUNDED_CURVE ( )  B_SPLINE_CURVE ( 3, ( #47091, #30263, #63902, #29718 ),
 .UNSPECIFIED., .F., .F. ) 
 B_SPLINE_CURVE_WITH_KNOTS ( ( 4, 4 ),
 ( 0.9158457003869029389, 2.225909800249735060 ),
 .UNSPECIFIED. ) 
 CURVE ( )  GEOMETRIC_REPRESENTATION_ITEM ( )  RATIONAL_B_SPLINE_CURVE ( ( 1.000000000000000000, 0.8620189361215893076, 0.8620189361215893076, 1.000000000000000000 ) ) 
 REPRESENTATION_ITEM ( '' )  );
#25175 = CARTESIAN_POINT ( 'NONE',  ( -18.35007156173510268, 1419.478779913980134, 206.0032569124829820 ) ) ;
#25177 = CARTESIAN_POINT ( 'NONE',  ( 0.1729020573706560038, 1478.627309218569962, 182.1533541099630042 ) ) ;
#25179 = ORIENTED_EDGE ( 'NONE', *, *, #37977, .T. ) ;
#25178 = DIRECTION ( 'NONE',  ( -0.000000000000000000, -1.000000000000000000, -0.000000000000000000 ) ) ;
#25180 = CARTESIAN_POINT ( 'NONE',  ( -17.11714625305222981, 1444.740067931810927, 162.7561045841209193 ) ) ;
#25181 = AXIS2_PLACEMENT_3D ( 'NONE', #2910, #37028, #62839 ) ;
#25182 = CARTESIAN_POINT ( 'NONE',  ( 33.23571934791666393, 1512.187213306747481, 198.7594255952494677 ) ) ;
#25183 = CARTESIAN_POINT ( 'NONE',  ( 13.80510066409999936, 1434.979587830419860, 149.7893444102980141 ) ) ;
#25184 = CARTESIAN_POINT ( 'NONE',  ( -40.27155789729510360, 1448.225093239489979, 134.0999999982899737 ) ) ;
#25185 = FACE_OUTER_BOUND ( 'NONE', #85757, .T. ) ;
#25186 = EDGE_LOOP ( 'NONE', ( #53374, #107799, #104200, #31874 ) ) ;
#25187 = CARTESIAN_POINT ( 'NONE',  ( -10.16565329039999988, 1472.147622277889923, 209.4747181525780206 ) ) ;
#25188 = DIRECTION ( 'NONE',  ( 0.000000000000000000, 0.000000000000000000, 1.000000000000000000 ) ) ;
#25189 = CARTESIAN_POINT ( 'NONE',  ( -16.81460427359999699, 1415.425433635630043, 214.3135839119680099 ) ) ;
#25190 = DIRECTION ( 'NONE',  ( 1.755985294532469921E-16, -1.000000000000000000, 1.338183447452831989E-16 ) ) ;
#25191 = CARTESIAN_POINT ( 'NONE',  ( -7.873917804663410180, 1436.018178901780175, 213.0668616092210073 ) ) ;
#25192 = CARTESIAN_POINT ( 'NONE',  ( -0.8265242355799999885, 1408.941923249630008, 187.0792671738979891 ) ) ;
#25193 = CARTESIAN_POINT ( 'NONE',  ( -15.66177877319999823, 1418.090152389999957, 210.6205366076489724 ) ) ;
#25194 = CARTESIAN_POINT ( 'NONE',  ( 8.196706623898419863, 1409.199295689860037, 221.6385046391639833 ) ) ;
#25195 = CARTESIAN_POINT ( 'NONE',  ( -11.62395736679999914, 1391.913060387289988, 208.2888796421599977 ) ) ;
#25196 = CARTESIAN_POINT ( 'NONE',  ( -68.09493305640410199, 1385.102643623660015, 261.8663954522849622 ) ) ;
#25197 = CARTESIAN_POINT ( 'NONE',  ( -10.76416396095310013, 1391.913060387289988, 213.0502257285290284 ) ) ;
#25198 = CARTESIAN_POINT ( 'NONE',  ( 12.22179537434220009, 1427.254335307449992, 207.6012072736810126 ) ) ;
#25199 = EDGE_LOOP ( 'NONE', ( #53404, #1526, #83088, #54067 ) ) ;
#25200 = CARTESIAN_POINT ( 'NONE',  ( -29.31937758650000347, 1451.433528204029926, 136.0808240385979957 ) ) ;
#25201 = CARTESIAN_POINT ( 'NONE',  ( -15.80996491931430015, 1410.569114994490064, 226.6997803613269866 ) ) ;
#25203 = EDGE_LOOP ( 'NONE', ( #4625, #14791, #59998, #52364, #22941 ) ) ;
#25202 = DIRECTION ( 'NONE',  ( -0.8164965809278522668, -0.5773502691894472072, 0.000000000000000000 ) ) ;
#25204 = CARTESIAN_POINT ( 'NONE',  ( 1.498516750899999916, 1473.533416210889982, 219.2408104862990115 ) ) ;
#25205 = CARTESIAN_POINT ( 'NONE',  ( 18.15402009115259929, 1430.058659865889922, 210.6865277441139881 ) ) ;
#25206 = CARTESIAN_POINT ( 'NONE',  ( -7.891625280017878552, 1364.691779921422949, 209.6218459617148824 ) ) ;
#25207 = DIRECTION ( 'NONE',  ( -0.6736849260863841948, 0.000000000000000000, 0.7390186874254148774 ) ) ;
#25208 = CARTESIAN_POINT ( 'NONE',  ( 32.86802468386292730, 1512.187213306747481, 217.2040256693915410 ) ) ;
#25209 = FACE_OUTER_BOUND ( 'NONE', #56483, .T. ) ;
#25210 = CARTESIAN_POINT ( 'NONE',  ( 17.93831527589803443, 1434.889764120619475, 215.4602619631652942 ) ) ;
#25211 = CARTESIAN_POINT ( 'NONE',  ( 1.362396098649999887, 1416.437840611730053, 232.9004600697980152 ) ) ;
#25212 = CARTESIAN_POINT ( 'NONE',  ( 9.014216207049999596, 1449.483768445589931, 207.1212598930990225 ) ) ;
#25213 = CARTESIAN_POINT ( 'NONE',  ( -113.4000000000000057, 1309.112692017090239, 296.2006505458990091 ) ) ;
#25214 = CARTESIAN_POINT ( 'NONE',  ( 22.64728419264357129, 1509.725303465448860, 190.0246945496440105 ) ) ;
#25215 = B_SPLINE_CURVE_WITH_KNOTS ( 'NONE', 5,
 ( #70509, #37428, #11135, #62103, #44181, #54253 ),
 .UNSPECIFIED., .F., .F.,
 ( 6, 6 ),
 ( 0.000000000000000000, 1.000000000000000000 ),
 .UNSPECIFIED. ) ;
#25216 = CARTESIAN_POINT ( 'NONE',  ( -1.042889439659999917, 1455.537194040490022, 199.0056471502989837 ) ) ;
#25217 = CARTESIAN_POINT ( 'NONE',  ( -0.7576635715699989726, 1516.855632454399938, 206.2537338009369989 ) ) ;
#25218 = CARTESIAN_POINT ( 'NONE',  ( 2.500000000000000000, 1448.555989962169861, 159.6014785455980132 ) ) ;
#25219 = CARTESIAN_POINT ( 'NONE',  ( -2.500000000000000000, 1439.114301494319989, 157.7261950941980331 ) ) ;
#25220 = CARTESIAN_POINT ( 'NONE',  ( -2.443439238509999889, 1496.401426496290014, 197.7599957902989729 ) ) ;
#25222 = ORIENTED_EDGE ( 'NONE', *, *, #89125, .F. ) ;
#25221 = CARTESIAN_POINT ( 'NONE',  ( -68.55949274003370419, 1379.747596899770087, 280.1521097459560110 ) ) ;
#25223 = CARTESIAN_POINT ( 'NONE',  ( 40.76710640913900363, 1444.185691436559864, 136.9913394050109900 ) ) ;
#25224 = ORIENTED_EDGE ( 'NONE', *, *, #78940, .T. ) ;
#25225 = EDGE_CURVE ( 'NONE', #88502, #39623, #61785, .T. ) ;
#25226 = CARTESIAN_POINT ( 'NONE',  ( -16.78766067578666465, 1513.436209035151933, 222.1126914816819635 ) ) ;
#25227 = CARTESIAN_POINT ( 'NONE',  ( -23.70212955649999742, 1410.915617643129963, 207.1033590604579899 ) ) ;
#25229 = CARTESIAN_POINT ( 'NONE',  ( 17.33016647839879809, 1410.462159060319891, 192.5037184876999845 ) ) ;
#25228 = CARTESIAN_POINT ( 'NONE',  ( -10.52497800899770120, 1425.367411924009957, 103.8987780947440029 ) ) ;
#25230 = CARTESIAN_POINT ( 'NONE',  ( 7.726331925474999807, 1517.194972660189933, 211.4133602680070112 ) ) ;
#25231 = CIRCLE ( 'NONE', #73562, 2.000000000000003553 ) ;
#25232 = CARTESIAN_POINT ( 'NONE',  ( 18.39508751440705225, 1509.674679010870705, 185.4233143434903468 ) ) ;
#25233 = CARTESIAN_POINT ( 'NONE',  ( -18.96350828799999988, 1416.837080254430020, 208.0006277515079773 ) ) ;
#25234 = CARTESIAN_POINT ( 'NONE',  ( -44.59182306800000362, 1432.587450657589898, 266.2372469040980150 ) ) ;
#25235 = CARTESIAN_POINT ( 'NONE',  ( -12.45166823054470129, 1378.738365027170175, 209.0955970008419911 ) ) ;
#25236 = CARTESIAN_POINT ( 'NONE',  ( 12.69299105715940001, 1500.682136716359992, 209.6945769240809909 ) ) ;
#25237 = EDGE_CURVE ( 'NONE', #7508, #10122, #87589, .T. ) ;
#25238 = CARTESIAN_POINT ( 'NONE',  ( 4.626410093743990259, 1508.551704408389924, 212.9021791863180226 ) ) ;
#25239 = DIRECTION ( 'NONE',  ( -1.000000000000000000, 6.123233995736769734E-17, 0.000000000000000000 ) ) ;
#25240 = ORIENTED_EDGE ( 'NONE', *, *, #30975, .T. ) ;
#25241 = CARTESIAN_POINT ( 'NONE',  ( 9.933598901150000771, 1396.438403817630160, 201.0717090587579889 ) ) ;
#25242 = CARTESIAN_POINT ( 'NONE',  ( 10.10890582563189888, 1461.386743975740046, 208.4428558525590063 ) ) ;
#25243 = DIRECTION ( 'NONE',  ( 0.9998780035959986545, 0.000000000000000000, -0.01561979272846077127 ) ) ;
#25244 = ORIENTED_EDGE ( 'NONE', *, *, #51843, .T. ) ;
#25245 = VERTEX_POINT ( 'NONE', #9238 ) ;
#25246 = CARTESIAN_POINT ( 'NONE',  ( -29.53763760329688637, 1509.959418432381881, 210.9330277046395565 ) ) ;
#25247 = CARTESIAN_POINT ( 'NONE',  ( 10.51591518309250084, 1452.897324824680254, 210.4058924105359836 ) ) ;
#25248 = AXIS2_PLACEMENT_3D ( 'NONE', #82644, #315, #61337 ) ;
#25249 = CARTESIAN_POINT ( 'NONE',  ( -14.19917317546740065, 1380.177169543179843, 210.7455613943569972 ) ) ;
#25250 = CARTESIAN_POINT ( 'NONE',  ( -10.95001104760099331, 1417.929106870156829, 198.2904426808065352 ) ) ;
#25251 = CARTESIAN_POINT ( 'NONE',  ( 4.226426730560000067, 1515.477082009289916, 209.1218459616539747 ) ) ;
#25252 = CARTESIAN_POINT ( 'NONE',  ( -4.726277182027989632, 1455.252851925170035, 200.9609556798399979 ) ) ;
#25253 = CARTESIAN_POINT ( 'NONE',  ( 12.65750243759436877, 1420.218673000053741, 200.3470716195499790 ) ) ;
#25254 = DIRECTION ( 'NONE',  ( -0.9455185755993178454, 0.000000000000000000, 0.3255681544571537578 ) ) ;
#25255 = CARTESIAN_POINT ( 'NONE',  ( 25.18950438009999715, 1436.599308748099929, 137.5297815331979905 ) ) ;
#25256 = CARTESIAN_POINT ( 'NONE',  ( -119.3423021147300034, 1306.483669372790018, 300.9755515165790030 ) ) ;
#25257 = CARTESIAN_POINT ( 'NONE',  ( -87.73050061784429943, 1384.829504049740081, 291.0308553036180115 ) ) ;
#25258 = EDGE_LOOP ( 'NONE', ( #85123, #108442, #40089, #9747 ) ) ;
#25259 = CARTESIAN_POINT ( 'NONE',  ( -7.717505791104999346, 1516.857914730730045, 201.4043401791270185 ) ) ;
#25260 = CARTESIAN_POINT ( 'NONE',  ( -1.127928371535000140, 1516.989863902050047, 209.1319708558790182 ) ) ;
#25261 = ORIENTED_EDGE ( 'NONE', *, *, #62416, .T. ) ;
#25262 = CARTESIAN_POINT ( 'NONE',  ( 11.78205866055090034, 1427.489864168300073, 147.1792652955979861 ) ) ;
#25263 = VECTOR ( 'NONE', #76389, 1000.000000000000000 ) ;
#25264 = CARTESIAN_POINT ( 'NONE',  ( 3.806606270525944247, 1511.520894735526781, 217.2557709082670101 ) ) ;
#25265 = ORIENTED_EDGE ( 'NONE', *, *, #18672, .T. ) ;
#25266 = CARTESIAN_POINT ( 'NONE',  ( -13.31050682230000071, 1414.983773854429955, 220.3937082794980142 ) ) ;
#25267 = CARTESIAN_POINT ( 'NONE',  ( -11.74913059853910013, 1432.337153556749854, 150.6947011568290122 ) ) ;
#25268 = CARTESIAN_POINT ( 'NONE',  ( -1.590050350630178855, 1426.843352158476364, 137.0999999982234385 ) ) ;
#25269 = CIRCLE ( 'NONE', #94995, 1.500000000000001332 ) ;
#25270 = CARTESIAN_POINT ( 'NONE',  ( -11.01150942929239918, 1462.569953727359916, 208.1811703706719925 ) ) ;
#25271 = CARTESIAN_POINT ( 'NONE',  ( -4.519015011720000530, 1423.889711422029904, 184.9853378348980186 ) ) ;
#25272 = CARTESIAN_POINT ( 'NONE',  ( 10.09433608495039891, 1469.369659831060062, 207.3742786837029826 ) ) ;
#25273 = CARTESIAN_POINT ( 'NONE',  ( -10.93162295028230169, 1470.132889486390013, 212.2376398131100075 ) ) ;
#25274 = CARTESIAN_POINT ( 'NONE',  ( -5.482624842517240360, 1410.482164323645065, 187.0654721365125397 ) ) ;
#25275 = CARTESIAN_POINT ( 'NONE',  ( -52.00740111290000556, 1379.696047019589969, 243.6069664339590020 ) ) ;
#25276 = CARTESIAN_POINT ( 'NONE',  ( -16.48551040579999949, 1496.366555713729895, 224.3141742696979861 ) ) ;
#25278 = DIRECTION ( 'NONE',  ( 0.000000000000000000, 0.000000000000000000, 1.000000000000000000 ) ) ;
#25277 = CARTESIAN_POINT ( 'NONE',  ( 17.87794079920000101, 1458.605263598229840, 228.2755591389980054 ) ) ;
#25279 = CARTESIAN_POINT ( 'NONE',  ( -4.904257884871542572, 1423.393875679067833, 184.6729318142273826 ) ) ;
#25280 = CARTESIAN_POINT ( 'NONE',  ( -2.499954588792669963, 1419.918889429339970, 111.3715765239870024 ) ) ;
#25281 = ORIENTED_EDGE ( 'NONE', *, *, #68688, .T. ) ;
#25282 = VECTOR ( 'NONE', #90481, 1000.000000000000000 ) ;
#25283 = CARTESIAN_POINT ( 'NONE',  ( -4.364191719525152280, 1509.032014410905276, 205.0059630720760140 ) ) ;
#25284 = CARTESIAN_POINT ( 'NONE',  ( -21.66432897272838431, 1525.042412244734578, 233.5340606467491966 ) ) ;
#25285 = CARTESIAN_POINT ( 'NONE',  ( -2.898871272187721004, 1484.376110530463620, 183.3081109901478669 ) ) ;
#25286 = CARTESIAN_POINT ( 'NONE',  ( -14.77610201870000139, 1416.023439710309958, 213.5223809413389802 ) ) ;
#25288 = ORIENTED_EDGE ( 'NONE', *, *, #47457, .F. ) ;
#25287 = CARTESIAN_POINT ( 'NONE',  ( 4.554954796684620000, 1508.731366863229823, 212.6094326720719891 ) ) ;
#25289 = CARTESIAN_POINT ( 'NONE',  ( 1.525925909070000142, 1471.311257370530029, 187.8077771315979874 ) ) ;
#25290 = CARTESIAN_POINT ( 'NONE',  ( -11.80475977109999874, 1428.187072569730162, 148.7521081752979910 ) ) ;
#25291 = CARTESIAN_POINT ( 'NONE',  ( -10.94851406893937096, 1430.816032392971692, 151.6584449855879768 ) ) ;
#25292 = CARTESIAN_POINT ( 'NONE',  ( -11.03695077974730054, 1462.414655202809854, 208.8602946956429776 ) ) ;
#25293 = CARTESIAN_POINT ( 'NONE',  ( -5.343479917770609156, 1396.099658817820000, 199.4684377796870081 ) ) ;
#25294 = CARTESIAN_POINT ( 'NONE',  ( -5.266928095709999980, 1427.575715857079786, 201.4004753664689815 ) ) ;
#25295 = CARTESIAN_POINT ( 'NONE',  ( -2.451271202390000070, 1433.447543843880112, 150.3250444719979839 ) ) ;
#25297 = CARTESIAN_POINT ( 'NONE',  ( -11.36422223541920040, 1482.111961209009905, 207.7636347213490069 ) ) ;
#25296 = CARTESIAN_POINT ( 'NONE',  ( -25.31266740589999742, 1495.362868818529932, 217.3509689723979932 ) ) ;
#25298 = CARTESIAN_POINT ( 'NONE',  ( -16.13327988281299952, 1459.077551211970103, 230.3615990537609832 ) ) ;
#25299 = VERTEX_POINT ( 'NONE', #93756 ) ;
#25300 = CARTESIAN_POINT ( 'NONE',  ( 7.709681268295000223, 1516.559109716219837, 206.2491454149069909 ) ) ;
#25301 = CARTESIAN_POINT ( 'NONE',  ( 35.80076753759999519, 1418.783835402329942, 268.8110194917979925 ) ) ;
#25302 = DIRECTION ( 'NONE',  ( 0.000000000000000000, 0.000000000000000000, -1.000000000000000000 ) ) ;
#25303 = B_SPLINE_CURVE_WITH_KNOTS ( 'NONE', 3,
 ( #40119, #7075, #30625, #58592, #100019, #99461, #39580, #101111, #90521, #73752, #64812, #22191, #14355, #48547, #22739, #58044 ),
 .UNSPECIFIED., .F., .F.,
 ( 4, 3, 3, 3, 3, 4 ),
 ( -7.456423346589999390, -6.951387445693330669, -5.975502946654870584, -5.002829108848499295, -4.031542647132239310, -3.062118867579999737 ),
 .UNSPECIFIED. ) ;
#25304 = CARTESIAN_POINT ( 'NONE',  ( 20.53761168180000141, 1449.728047012690013, 194.5965259811979990 ) ) ;
#25305 = EDGE_CURVE ( 'NONE', #110638, #80871, #304, .T. ) ;
#25306 = CARTESIAN_POINT ( 'NONE',  ( 0.06657943191975031205, 1508.845581504609981, 238.3754151068810074 ) ) ;
#25307 = ADVANCED_FACE ( 'NONE', ( #85364 ), #94891, .T. ) ;
#25308 = DIRECTION ( 'NONE',  ( 0.000000000000000000, 1.000000000000000000, 0.000000000000000000 ) ) ;
#25309 = CARTESIAN_POINT ( 'NONE',  ( 4.687651746879999415, 1478.378160227390254, 228.9010599218989910 ) ) ;
#25310 = PLANE ( 'NONE',  #60392 ) ;
#25311 = CARTESIAN_POINT ( 'NONE',  ( -15.18421651749999945, 1416.713354283420131, 205.6620439543090129 ) ) ;
#25312 = CARTESIAN_POINT ( 'NONE',  ( -13.40404449519999908, 1444.440855884700113, 187.1602913364980054 ) ) ;
#25313 = EDGE_CURVE ( 'NONE', #60042, #45216, #74188, .T. ) ;
#25314 = CARTESIAN_POINT ( 'NONE',  ( -19.60393592299999810, 1475.513060387329915, 216.8351853114679955 ) ) ;
#25315 = EDGE_CURVE ( 'NONE', #54321, #73940, #93225, .T. ) ;
#25316 = CARTESIAN_POINT ( 'NONE',  ( -8.588755447433969792, 1437.818850531529961, 207.9413692731380081 ) ) ;
#25317 = CARTESIAN_POINT ( 'NONE',  ( -4.712600100240000423, 1496.928403841490081, 219.5050635169990016 ) ) ;
#25318 = VERTEX_POINT ( 'NONE', #1389 ) ;
#25319 = CARTESIAN_POINT ( 'NONE',  ( -1.758949987490000089, 1470.986537992489957, 189.1593042989989897 ) ) ;
#25320 = CARTESIAN_POINT ( 'NONE',  ( -14.39277900435820001, 1409.415667305270063, 205.1427022228000112 ) ) ;
#25321 = CARTESIAN_POINT ( 'NONE',  ( 2.562340869413361588, 1522.051704408389924, 221.9545077427458182 ) ) ;
#25322 = DIRECTION ( 'NONE',  ( -1.224646799147353947E-16, 1.836970198721029688E-16, 1.000000000000000000 ) ) ;
#25323 = CIRCLE ( 'NONE', #367, 2.000000000000003553 ) ;
#25324 = CARTESIAN_POINT ( 'NONE',  ( -14.40881992470000128, 1473.360613499030023, 269.5837026295979513 ) ) ;
#25325 = CARTESIAN_POINT ( 'NONE',  ( -30.04653961080366287, 1524.739915903616748, 195.9294070843147892 ) ) ;
#25326 = CARTESIAN_POINT ( 'NONE',  ( -11.44054303565944686, 1391.153937848091800, 213.9067438120043221 ) ) ;
#25327 = CARTESIAN_POINT ( 'NONE',  ( -24.09045629887435069, 1444.422250552413971, 211.8863943959888161 ) ) ;
#25328 = CARTESIAN_POINT ( 'NONE',  ( -57.60540916714719373, 1384.705479994730013, 276.7345517628079961 ) ) ;
#25329 = CARTESIAN_POINT ( 'NONE',  ( -19.85270156754270232, 1384.950477623580127, 201.6204297621999899 ) ) ;
#25330 = CARTESIAN_POINT ( 'NONE',  ( 12.20493293904160126, 1416.321686232750153, 223.5163099168240137 ) ) ;
#25331 = CARTESIAN_POINT ( 'NONE',  ( -107.8626300280000123, 1378.913060387289988, 300.1243669462589878 ) ) ;
#25332 = CARTESIAN_POINT ( 'NONE',  ( 7.034613962576056423, 1471.361440081786668, 216.4463950981275673 ) ) ;
#25333 = CARTESIAN_POINT ( 'NONE',  ( 11.39903768489999969, 1471.112746669390162, 209.6182361446229834 ) ) ;
#25334 = CARTESIAN_POINT ( 'NONE',  ( -22.77843419010000048, 1410.203593476030164, 204.7359747443179856 ) ) ;
#25335 = EDGE_CURVE ( 'NONE', #1907, #40693, #59623, .T. ) ;
#25336 = CARTESIAN_POINT ( 'NONE',  ( -9.211456433762755580, 1381.302692241149771, 200.8120824927987087 ) ) ;
#25337 = VECTOR ( 'NONE', #47638, 1000.000000000000000 ) ;
#25338 = CARTESIAN_POINT ( 'NONE',  ( 4.167208771420000346, 1485.303719113790066, 219.1667848572990067 ) ) ;
#25339 = CARTESIAN_POINT ( 'NONE',  ( 16.66094735743510213, 1410.867388111209948, 226.5061907891179942 ) ) ;
#25340 = CARTESIAN_POINT ( 'NONE',  ( -15.24384917251130034, 1447.147816755560143, 196.6853903820460232 ) ) ;
#25341 = CARTESIAN_POINT ( 'NONE',  ( -19.10748961539120216, 1444.545920780599999, 199.6793401393300087 ) ) ;
#25343 = EDGE_CURVE ( 'NONE', #61158, #47444, #92198, .T. ) ;
#25342 = CARTESIAN_POINT ( 'NONE',  ( -6.551899188738270041, 1508.551566291330118, 216.0836886511409887 ) ) ;
#25344 = DIRECTION ( 'NONE',  ( 0.01393861230742109505, 0.01013783823313249566, -0.9998514586291816775 ) ) ;
#25346 = FACE_OUTER_BOUND ( 'NONE', #75485, .T. ) ;
#25345 = CARTESIAN_POINT ( 'NONE',  ( -22.51991132370000059, 1410.619212249830071, 212.0399852714280087 ) ) ;
#25347 = CARTESIAN_POINT ( 'NONE',  ( 11.71642830186019957, 1426.709184726649937, 142.6946108399700108 ) ) ;
#25348 = CARTESIAN_POINT ( 'NONE',  ( 9.798333899899640542, 1435.847786354059963, 209.9101837937189998 ) ) ;
#25349 = CARTESIAN_POINT ( 'NONE',  ( -127.3242238164999947, 1328.501055712589960, 296.6150078171390305 ) ) ;
#25350 = EDGE_CURVE ( 'NONE', #106884, #7587, #95446, .T. ) ;
#25351 = CARTESIAN_POINT ( 'NONE',  ( 6.385148413900250119, 1448.088845170490004, 201.0945304462800038 ) ) ;
#25352 = CARTESIAN_POINT ( 'NONE',  ( -10.98592888573429960, 1414.913372219064740, 196.0727560459370693 ) ) ;
#25353 = CARTESIAN_POINT ( 'NONE',  ( -4.620008245204999753, 1516.777260590120022, 203.3472363101570011 ) ) ;
#25354 = CARTESIAN_POINT ( 'NONE',  ( -12.26707230937048365, 1398.276752517840350, 213.6251289080058484 ) ) ;
#25355 = CARTESIAN_POINT ( 'NONE',  ( 31.34137657934019927, 1512.187213306747481, 221.9025654077410081 ) ) ;
#25356 = FACE_BOUND ( 'NONE', #91217, .T. ) ;
#25357 = CARTESIAN_POINT ( 'NONE',  ( 1.401686974080000203, 1507.677644781729896, 236.8428152670980182 ) ) ;
#25358 = CIRCLE ( 'NONE', #5736, 32.72294243206279418 ) ;
#25359 = CARTESIAN_POINT ( 'NONE',  ( 20.59997055523719922, 1508.349664204210058, 227.9987446602079899 ) ) ;
#25361 = ORIENTED_EDGE ( 'NONE', *, *, #17925, .T. ) ;
#25360 = CARTESIAN_POINT ( 'NONE',  ( -56.97967810409669909, 1379.730140100299877, 259.4601704726770208 ) ) ;
#25362 = ORIENTED_EDGE ( 'NONE', *, *, #30897, .F. ) ;
#25363 = CARTESIAN_POINT ( 'NONE',  ( 12.02659948205739937, 1433.794953934120031, 150.1257855643209780 ) ) ;
#25364 = CARTESIAN_POINT ( 'NONE',  ( 0.04898382733899999536, 1396.985963199630305, 221.9366346537979950 ) ) ;
#25365 = ORIENTED_EDGE ( 'NONE', *, *, #45891, .F. ) ;
#25366 = CARTESIAN_POINT ( 'NONE',  ( -105.1200804420000026, 1379.260731124600170, 305.2465900763589843 ) ) ;
#25367 = CARTESIAN_POINT ( 'NONE',  ( -22.59253512340000114, 1509.026248158530052, 193.6920252460979839 ) ) ;
#25368 = CARTESIAN_POINT ( 'NONE',  ( 4.329448802513499395, 1515.064791340959800, 206.7919475944040073 ) ) ;
#25370 = CARTESIAN_POINT ( 'NONE',  ( -13.94340296021099945, 1508.954224554140183, 183.7492702217640215 ) ) ;
#25369 = DIRECTION ( 'NONE',  ( 1.755985294532464991E-16, -1.000000000000000000, 1.338183447452830017E-16 ) ) ;
#25371 = CARTESIAN_POINT ( 'NONE',  ( 19.14360834932719868, 1488.414938085379845, 228.7258892975569893 ) ) ;
#25372 = CIRCLE ( 'NONE', #70116, 1.999999999999999556 ) ;
#25373 = CARTESIAN_POINT ( 'NONE',  ( 11.10982621349999988, 1449.228537578660053, 187.2287387423980078 ) ) ;
#25374 = CARTESIAN_POINT ( 'NONE',  ( 2.356138219550000024, 1466.787411483390088, 219.9406446673989990 ) ) ;
#25375 = CARTESIAN_POINT ( 'NONE',  ( -24.19014952379989936, 1444.790439640009936, 211.5093900478289868 ) ) ;
#25376 = ADVANCED_FACE ( 'NONE', ( #61328 ), #50681, .F. ) ;
#25377 = CARTESIAN_POINT ( 'NONE',  ( 0.4151546846821903003, 1511.187213306747708, 174.3106345060153046 ) ) ;
#25378 = CARTESIAN_POINT ( 'NONE',  ( 37.46849106787850303, 1436.652236075190103, 134.0999999968449856 ) ) ;
#25379 = CARTESIAN_POINT ( 'NONE',  ( 11.85834799300000064, 1431.766924987119864, 150.3709389535979994 ) ) ;
#25380 = CARTESIAN_POINT ( 'NONE',  ( 5.649719750514999639, 1514.243099272629934, 201.4728115316369781 ) ) ;
#25381 = ORIENTED_EDGE ( 'NONE', *, *, #46840, .F. ) ;
#25382 = CARTESIAN_POINT ( 'NONE',  ( 13.49389551315819880, 1436.020594185369873, 150.4744559408089799 ) ) ;
#25383 = ORIENTED_EDGE ( 'NONE', *, *, #33530, .T. ) ;
#25384 = ORIENTED_EDGE ( 'NONE', *, *, #39751, .F. ) ;
#25385 = CARTESIAN_POINT ( 'NONE',  ( 7.006565492904999637, 1516.551704408390151, 221.0781589314669873 ) ) ;
#25386 = CARTESIAN_POINT ( 'NONE',  ( -4.082666824149999485, 1466.262580571829858, 234.7294175710979971 ) ) ;
#25387 = CARTESIAN_POINT ( 'NONE',  ( -12.34781077223220080, 1407.409374063429823, 203.9011771819639876 ) ) ;
#25388 = CARTESIAN_POINT ( 'NONE',  ( -5.778999811904999895, 1516.955859323880077, 216.4549161051170074 ) ) ;
#25389 = CARTESIAN_POINT ( 'NONE',  ( -8.053242336889125497, 1511.610022726261377, 212.6696535251155069 ) ) ;
#25390 = PRODUCT_DEFINITION ( 'UNKNOWN', '', #69102, #60314 ) ;
#25391 = CARTESIAN_POINT ( 'NONE',  ( -19.07790034667103285, 1442.172555339580185, 210.4727050325287223 ) ) ;
#25392 = CARTESIAN_POINT ( 'NONE',  ( 7.098162965876308128, 1512.239113741298070, 201.9714854511515796 ) ) ;
#25393 = CARTESIAN_POINT ( 'NONE',  ( 1.079600664838949807E-13, 1377.913060387289988, 206.3143084471490170 ) ) ;
#25394 = ORIENTED_EDGE ( 'NONE', *, *, #61267, .F. ) ;
#25395 = CARTESIAN_POINT ( 'NONE',  ( 3.252530615595000452, 1516.827328999679821, 206.2418890071470230 ) ) ;
#25396 = EDGE_LOOP ( 'NONE', ( #10828, #80506, #11636, #28296 ) ) ;
#25397 = CARTESIAN_POINT ( 'NONE',  ( 22.08278260508789970, 1440.913060387330006, 227.7515003150190012 ) ) ;
#25398 = CARTESIAN_POINT ( 'NONE',  ( -19.28393528680000202, 1507.737928445829994, 229.5896611176980002 ) ) ;
#25399 = CARTESIAN_POINT ( 'NONE',  ( -7.248290715579999599, 1409.670137264329924, 187.6984399624980142 ) ) ;
#25400 = CARTESIAN_POINT ( 'NONE',  ( 7.653848867554999380, 1514.071098020780028, 215.6856573818370180 ) ) ;
#25402 = ORIENTED_EDGE ( 'NONE', *, *, #84660, .T. ) ;
#25401 = CARTESIAN_POINT ( 'NONE',  ( 0.3610913073109310312, 1416.520646088589956, 227.1639887257210262 ) ) ;
#25403 = CARTESIAN_POINT ( 'NONE',  ( 24.43361483890000230, 1438.270030349950048, 213.2447553941780143 ) ) ;
#25404 = DIRECTION ( 'NONE',  ( -0.6736849260863841948, 0.000000000000000000, 0.7390186874254148774 ) ) ;
#25406 = ADVANCED_FACE ( 'NONE', ( #8113 ), #103261, .T. ) ;
#25405 = DIRECTION ( 'NONE',  ( 0.5161917810414575758, -0.8564730265368828421, 0.000000000000000000 ) ) ;
#25407 = CARTESIAN_POINT ( 'NONE',  ( 21.71247731329033215, 1523.982201850120191, 183.5488543797099226 ) ) ;
#25408 = EDGE_CURVE ( 'NONE', #43960, #23910, #9866, .T. ) ;
#25409 = CARTESIAN_POINT ( 'NONE',  ( -4.031142389804999837, 1516.929569650079884, 214.1322689334670031 ) ) ;
#25410 = CARTESIAN_POINT ( 'NONE',  ( -2.897185018188709993, 1428.978219621640164, 200.2122387005069868 ) ) ;
#25411 = CARTESIAN_POINT ( 'NONE',  ( 23.28443123535648240, 1409.830905082309982, 209.4348622450964115 ) ) ;
#25412 = CARTESIAN_POINT ( 'NONE',  ( 6.961842680912760706, 1508.551566291330118, 215.6737451208340133 ) ) ;
#25413 = CARTESIAN_POINT ( 'NONE',  ( -1.118353254094999860, 1516.977201124959947, 211.6155430111569729 ) ) ;
#25414 = CARTESIAN_POINT ( 'NONE',  ( -20.70484064406366187, 1525.907212628473644, 233.2025904124108706 ) ) ;
#25415 = CARTESIAN_POINT ( 'NONE',  ( 13.82592919020000011, 1409.562390515329980, 191.7841888639979970 ) ) ;
#25416 = CARTESIAN_POINT ( 'NONE',  ( 30.31052258194597471, 1523.604703353109699, 222.4930856806589929 ) ) ;
#25418 = VERTEX_POINT ( 'NONE', #78646 ) ;
#25417 = CARTESIAN_POINT ( 'NONE',  ( -55.17517041340000361, 1388.273123790759882, 269.8705547383589760 ) ) ;
#25420 = VECTOR ( 'NONE', #9915, 999.9999999999998863 ) ;
#25419 = CARTESIAN_POINT ( 'NONE',  ( -70.15791120722559526, 1385.023615900659934, 295.2473282410489901 ) ) ;
#25421 = EDGE_CURVE ( 'NONE', #87307, #78370, #22467, .T. ) ;
#25422 = CARTESIAN_POINT ( 'NONE',  ( 10.82132307070000010, 1467.865346125029873, 250.5360043798979746 ) ) ;
#25423 = CARTESIAN_POINT ( 'NONE',  ( 2.838593810556235386, 1451.798153998362523, 183.8400884881581874 ) ) ;
#25424 = CARTESIAN_POINT ( 'NONE',  ( -26.72684354202990065, 1509.846382329900280, 221.2472112117080201 ) ) ;
#25425 = CARTESIAN_POINT ( 'NONE',  ( -5.276082853953459662, 1507.211509375310015, 236.2464089988909848 ) ) ;
#25426 = CARTESIAN_POINT ( 'NONE',  ( -23.30326309200000168, 1448.852050024469918, 216.7100016161180065 ) ) ;
#25427 = CARTESIAN_POINT ( 'NONE',  ( 2.798741256952680168, 1509.010794585639815, 238.1786444310339732 ) ) ;
#25429 = CARTESIAN_POINT ( 'NONE',  ( 17.67624996012689920, 1409.941488227490026, 222.7221753460849811 ) ) ;
#25428 = CARTESIAN_POINT ( 'NONE',  ( 20.64978683589999875, 1464.413060387330006, 209.6104161236400216 ) ) ;
#25430 = FACE_OUTER_BOUND ( 'NONE', #21974, .T. ) ;
#25431 = CARTESIAN_POINT ( 'NONE',  ( -107.4010429502839941, 1381.980278631019701, 310.0687908842899674 ) ) ;
#25432 = ORIENTED_EDGE ( 'NONE', *, *, #8893, .F. ) ;
#25433 = CARTESIAN_POINT ( 'NONE',  ( 4.032397901875000024, 1516.981965530290154, 203.3362630185569913 ) ) ;
#25434 = EDGE_CURVE ( 'NONE', #87976, #12155, #8177, .T. ) ;
#25435 = CARTESIAN_POINT ( 'NONE',  ( -7.756928808066270165, 1508.430203411700177, 219.4938965895260026 ) ) ;
#25436 = AXIS2_PLACEMENT_3D ( 'NONE', #13719, #82612, #14284 ) ;
#25437 = CARTESIAN_POINT ( 'NONE',  ( 28.23788172209999559, 1509.669894706129980, 207.1691932934379849 ) ) ;
#25438 = EDGE_CURVE ( 'NONE', #76524, #90041, #11786, .T. ) ;
#25439 = CARTESIAN_POINT ( 'NONE',  ( 24.59648532329999782, 1442.354039869650023, 212.9848133149079956 ) ) ;
#25440 = CARTESIAN_POINT ( 'NONE',  ( 38.12974907732069596, 1444.894042496080147, 137.0546131932600247 ) ) ;
#25441 = CARTESIAN_POINT ( 'NONE',  ( -7.532310163755457033, 1461.903255937187396, 202.9766630830429506 ) ) ;
#25442 = CARTESIAN_POINT ( 'NONE',  ( -1.591560612370000127, 1443.444047302290073, 218.6175903739389810 ) ) ;
#25443 = CARTESIAN_POINT ( 'NONE',  ( 1.681169524081967515, 1468.860615669657591, 219.0052562536231733 ) ) ;
#25444 = EDGE_CURVE ( 'NONE', #10869, #2857, #51125, .T. ) ;
#25445 = CARTESIAN_POINT ( 'NONE',  ( 27.33350507148860231, 1435.453172591590146, 135.7066127169290155 ) ) ;
#25446 = CARTESIAN_POINT ( 'NONE',  ( -105.8185367562990251, 1391.163754585894822, 301.8502271879565910 ) ) ;
#25447 = CARTESIAN_POINT ( 'NONE',  ( 3.644234494419170032E-15, 1459.964720571249927, 238.3189299478169971 ) ) ;
#25448 = CARTESIAN_POINT ( 'NONE',  ( -109.3474494770000121, 1386.224464844990280, 297.2624775481590405 ) ) ;
#25449 = CARTESIAN_POINT ( 'NONE',  ( -16.63719475160000272, 1415.804827907129948, 226.7776979096980199 ) ) ;
#25450 = CARTESIAN_POINT ( 'NONE',  ( 4.789673499540000101, 1465.867933640490037, 219.0700355186390027 ) ) ;
#25451 = CARTESIAN_POINT ( 'NONE',  ( -20.53760542139810852, 1525.821544997590308, 184.7213720461156470 ) ) ;
#25452 = CARTESIAN_POINT ( 'NONE',  ( -9.604690719327259566E-16, 1522.051704408389924, 209.1218459616989946 ) ) ;
#25453 = ORIENTED_EDGE ( 'NONE', *, *, #86405, .T. ) ;
#25454 = CARTESIAN_POINT ( 'NONE',  ( -25.18033061374759995, 1457.455288673970017, 210.8733860127310038 ) ) ;
#25455 = CARTESIAN_POINT ( 'NONE',  ( 2.258742332965870236, 1456.424467550069949, 219.5015882959719988 ) ) ;
#25456 = EDGE_CURVE ( 'NONE', #67122, #105161, #81785, .T. ) ;
#25457 = CARTESIAN_POINT ( 'NONE',  ( -16.43158760069999857, 1420.644935630790087, 203.2808212549290090 ) ) ;
#25458 = CARTESIAN_POINT ( 'NONE',  ( 16.61028814131559983, 1497.249999798759973, 188.4200016273640017 ) ) ;
#25459 = CARTESIAN_POINT ( 'NONE',  ( -0.4792323294310000259, 1416.456882655430036, 233.6761913835979954 ) ) ;
#25461 = CARTESIAN_POINT ( 'NONE',  ( 33.42844755916640764, 1522.861859112239927, 196.1165140606936745 ) ) ;
#25460 = CARTESIAN_POINT ( 'NONE',  ( 11.71837906060000023, 1501.675020862189967, 211.1788615571589958 ) ) ;
#25462 = CARTESIAN_POINT ( 'NONE',  ( -28.27265633500000064, 1508.146186371529893, 208.9956447143910054 ) ) ;
#25463 = CARTESIAN_POINT ( 'NONE',  ( 8.458662811369999091, 1427.983063278090185, 212.5922379039890018 ) ) ;
#25464 = CARTESIAN_POINT ( 'NONE',  ( 16.51111913633373263, 1525.159196711359755, 181.0518213589280947 ) ) ;
#25465 = EDGE_CURVE ( 'NONE', #46523, #101208, #99370, .T. ) ;
#25466 = DIRECTION ( 'NONE',  ( -0.006760929966149412801, 0.9987475664841024559, -0.04957406850437492268 ) ) ;
#25467 = CARTESIAN_POINT ( 'NONE',  ( -12.39869315161027785, 1451.240234666110155, 151.2148383238678946 ) ) ;
#25468 = CARTESIAN_POINT ( 'NONE',  ( -16.98743823132990016, 1415.088136167450102, 209.0991636084750098 ) ) ;
#25469 = CARTESIAN_POINT ( 'NONE',  ( 25.73103649876719956, 1435.396100992830043, 135.5026723454229796 ) ) ;
#25470 = LINE ( 'NONE', #78661, #45794 ) ;
#25471 = EDGE_LOOP ( 'NONE', ( #31271, #54757, #21065, #59977 ) ) ;
#25472 = B_SPLINE_CURVE_WITH_KNOTS ( 'NONE', 3,
 ( #98553, #89605, #11809, #71762, #54391, #107510, #98000, #21822, #105878, #80668, #30800, #80111, #3430, #56021, #90145, #5050, #4517 ),
 .UNSPECIFIED., .F., .F.,
 ( 4, 2, 2, 2, 2, 1, 2, 2, 4 ),
 ( 0.000000000000000000, 0.2499999999999752420, 0.3749999999999543698, 0.4999999999999334976, 0.6249999999999126254, 0.6874999999999087397, 0.7187499999999126254, 0.7499999999999165112, 1.000000000000000000 ),
 .UNSPECIFIED. ) ;
#25473 = DIRECTION ( 'NONE',  ( -0.6736849260863839728, 0.000000000000000000, 0.7390186874254150995 ) ) ;
#25474 = CARTESIAN_POINT ( 'NONE',  ( -12.24671249752945812, 1378.552623650818987, 211.6779590916783036 ) ) ;
#25475 = ORIENTED_EDGE ( 'NONE', *, *, #105774, .F. ) ;
#25476 = ORIENTED_EDGE ( 'NONE', *, *, #35626, .T. ) ;
#25477 = CARTESIAN_POINT ( 'NONE',  ( 3.822819546398629864, 1435.023558107709960, 227.1593522666110232 ) ) ;
#25479 = EDGE_CURVE ( 'NONE', #80100, #61056, #110378, .T. ) ;
#25478 = CARTESIAN_POINT ( 'NONE',  ( -15.55291268160981666, 1415.973418256078048, 207.8029067794451805 ) ) ;
#25481 = CARTESIAN_POINT ( 'NONE',  ( -24.41186846940000166, 1442.526119375989992, 212.0284777859579890 ) ) ;
#25480 = CARTESIAN_POINT ( 'NONE',  ( 10.42064607629999884, 1425.390417346130107, 97.30158504869778824 ) ) ;
#25482 = CARTESIAN_POINT ( 'NONE',  ( -1.937821456590000047, 1444.357003194489835, 218.0146419597290048 ) ) ;
#25483 = EDGE_CURVE ( 'NONE', #87765, #89963, #99647, .T. ) ;
#25484 = CARTESIAN_POINT ( 'NONE',  ( -11.86957566529999930, 1433.007102185709755, 150.1775624469979675 ) ) ;
#25485 = CARTESIAN_POINT ( 'NONE',  ( -12.29128949743470045, 1378.278888474700125, 210.0499278134209931 ) ) ;
#25486 = CARTESIAN_POINT ( 'NONE',  ( -2.561666046165639532, 1420.747219518938664, 185.5912888495579125 ) ) ;
#25487 = CARTESIAN_POINT ( 'NONE',  ( 7.153413542260000924, 1423.448481430999891, 213.6996531375289976 ) ) ;
#25488 = CARTESIAN_POINT ( 'NONE',  ( -24.14541275720000257, 1438.310581897909969, 211.7943488613079808 ) ) ;
#25489 = CARTESIAN_POINT ( 'NONE',  ( 3.082439592801790006E-16, 1517.051704408389924, 209.1218459616989946 ) ) ;
#25490 = CARTESIAN_POINT ( 'NONE',  ( 2.612625988760000073, 1449.170853583729922, 183.0936082360980208 ) ) ;
#25491 = EDGE_CURVE ( 'NONE', #86033, #61245, #3383, .T. ) ;
#25492 = CARTESIAN_POINT ( 'NONE',  ( 8.159621828281631295, 1363.533245305855644, 207.6218459616988241 ) ) ;
#25493 = CARTESIAN_POINT ( 'NONE',  ( -26.93976879576212013, 1509.966348417776089, 195.8375140788211866 ) ) ;
#25495 = ORIENTED_EDGE ( 'NONE', *, *, #54284, .F. ) ;
#25494 = CARTESIAN_POINT ( 'NONE',  ( -10.47043688597563182, 1522.051704408389924, 221.2386401010601844 ) ) ;
#25496 = ORIENTED_EDGE ( 'NONE', *, *, #921, .T. ) ;
#25497 = CARTESIAN_POINT ( 'NONE',  ( -11.74917500098110068, 1426.744637973110230, 145.0199627760420071 ) ) ;
#25498 = CARTESIAN_POINT ( 'NONE',  ( -21.63861185800000086, 1508.509217846390129, 209.6249585502670243 ) ) ;
#25499 = CARTESIAN_POINT ( 'NONE',  ( -3.113156797959999889, 1472.539629439029795, 270.3710789736979905 ) ) ;
#25500 = CARTESIAN_POINT ( 'NONE',  ( 12.67183603418154370, 1434.580315194757077, 147.1853303393423573 ) ) ;
#25501 =( BOUNDED_CURVE ( )  B_SPLINE_CURVE ( 3, ( #110489, #61772, #43300, #102609 ),
 .UNSPECIFIED., .F., .F. ) 
 B_SPLINE_CURVE_WITH_KNOTS ( ( 4, 4 ),
 ( 1.268017778269938001, 1.928411133669210020 ),
 .UNSPECIFIED. ) 
 CURVE ( )  GEOMETRIC_REPRESENTATION_ITEM ( )  RATIONAL_B_SPLINE_CURVE ( ( 1.000000000000000000, 0.9639857287959530119, 0.9639857287959530119, 1.000000000000000000 ) ) 
 REPRESENTATION_ITEM ( '' )  );
#25502 = CARTESIAN_POINT ( 'NONE',  ( -130.6584559203110132, 1340.114449826970031, 304.2218459572590064 ) ) ;
#25503 = CARTESIAN_POINT ( 'NONE',  ( 21.50121674829999918, 1519.913060387329779, 200.6355468375280111 ) ) ;
#25504 = CARTESIAN_POINT ( 'NONE',  ( 14.55374896642978300, 1435.825240606026000, 149.7846887453127920 ) ) ;
#25505 = CARTESIAN_POINT ( 'NONE',  ( -20.26030320659999617, 1497.713060387329961, 200.3164169727579917 ) ) ;
#25506 = CARTESIAN_POINT ( 'NONE',  ( 4.938621453790089433, 1370.910692062234148, 209.6218459617033432 ) ) ;
#25507 = CARTESIAN_POINT ( 'NONE',  ( 11.15120484727999894, 1522.051704408389924, 220.1441346914401720 ) ) ;
#25508 = CARTESIAN_POINT ( 'NONE',  ( -15.35891919189770150, 1408.417119347609969, 269.4168528522860129 ) ) ;
#25509 = CARTESIAN_POINT ( 'NONE',  ( -14.05872192255859865, 1435.084336612359948, 149.0797200086629744 ) ) ;
#25510 = CARTESIAN_POINT ( 'NONE',  ( -4.328426199472169777, 1515.103843506339899, 210.1872473502739922 ) ) ;
#25511 = CARTESIAN_POINT ( 'NONE',  ( 13.98344342490000081, 1443.270835250810023, 189.4072587568979884 ) ) ;
#25512 = ORIENTED_EDGE ( 'NONE', *, *, #174, .F. ) ;
#25513 = ORIENTED_EDGE ( 'NONE', *, *, #58995, .F. ) ;
#25514 = CARTESIAN_POINT ( 'NONE',  ( -22.03054413770898279, 1506.491018781362527, 209.2384929680489449 ) ) ;
#25515 = CARTESIAN_POINT ( 'NONE',  ( 5.568562089822329142, 1424.311407511700054, 193.4294382966939736 ) ) ;
#25516 = CARTESIAN_POINT ( 'NONE',  ( 1.713317409674999903, 1516.660388280709867, 213.7298676393670291 ) ) ;
#25517 = CARTESIAN_POINT ( 'NONE',  ( -10.31210393940000003, 1470.461415509729932, 185.6553077399979941 ) ) ;
#25518 = B_SPLINE_SURFACE_WITH_KNOTS ( 'NONE', 5, 5, ( 
 ( #45578, #20331, #45026, #28750, #94845, #11410, #18121, #18665, #79720 ),
 ( #54535, #88669, #11947, #46128, #52317, #86440, #9731, #78039, #21958 ),
 ( #81334, #4648, #108197, #23075, #12495, #65666, #38786, #108752, #6294 ),
 ( #64027, #89749, #65117, #21415, #97609, #47753, #90287, #98698, #81888 ),
 ( #13568, #89202, #48318, #13021, #55626, #46677, #5191, #47208, #80809 ),
 ( #40441, #29841, #83001, #39346, #64579, #72962, #74617, #107100, #30941 ) ),
 .UNSPECIFIED., .F., .F., .F.,
 ( 6, 6 ),
 ( 6, 3, 6 ),
 ( 4.238752792103120726, 5.659133035216879826 ),
 ( 0.000000000000000000, 0.5000000000000000000, 1.002061266616879998 ),
 .UNSPECIFIED. ) ;
#25519 = B_SPLINE_CURVE_WITH_KNOTS ( 'NONE', 3,
 ( #69110, #7517, #61278, #110529, #9183, #85312, #68552, #102118, #67452, #101551, #24844, #33813, #9723, #18112, #103211, #26517, #252, #52308, #95394, #50091, #59046, #84764, #68007, #25397, #59589, #8607, #25952, #60147, #86432, #17544, #51746, #43888, #1340, #35479, #62945, #97056, #70783, #62371, #64019, #4106, #45016, #44450, #2469, #3017, #95943, #79162, #36586, #29285, #96497, #18658, #19776, #89192, #80800, #54526, #1910, #11937, #38230, #10844, #28185, #20320, #28740, #53978, #61820, #20870, #88111, #46667, #55065, #63481, #88660, #97599, #72414, #19203, #11400, #45569, #37689, #104896, #80248, #12485, #79710, #46117, #53405, #52856, #106544, #29833, #3566, #86984, #10273, #37140, #71893, #71337, #105451, #106009, #36048, #78594, #70235, #104341, #27634, #87556, #48866, #23064, #90835, #47745, #99775, #5747, #82450, #98131, #21949, #90278, #56142, #38778, #107647, #72954, #74609, #56699, #75162, #74057, #100343, #48309, #57814, #108744, #32035, #89740, #14118, #82992, #108186, #30379, #13559, #107091, #57274, #91938, #39890, #21406, #64569, #14679, #91401, #31477, #6284, #40432, #23632, #66224, #65658, #15212 ),
 .UNSPECIFIED., .F., .F.,
 ( 4, 3, 3, 3, 3, 3, 3, 3, 3, 3, 3, 3, 3, 3, 3, 3, 3, 3, 3, 3, 3, 3, 3, 3, 3, 3, 3, 3, 3, 3, 3, 3, 3, 3, 3, 3, 3, 3, 3, 3, 3, 3, 3, 3, 3, 3, 3, 4 ),
 ( -30.13994748849999894, -27.96748203595269899, -25.55492730130620060, -23.23438917604190124, -21.17793478234460025, -19.26470382119120117, -17.45260263486330032, -15.71699118168050013, -14.04216480072339834, -12.41738884950610000, -10.85332760853319911, -9.318777413941120358, -7.823271649228651370, -6.990622299191308286, -5.769753512368222204, -4.532961737479141107, -3.269848154182920297, -1.988543521522920798, -0.6878283704175984781, 0.6335739646309974660, 1.976953695996598981, 3.343532765747298185, 4.734321904188007579, 6.162678800765782228, 7.613445470389912373, 9.084622672767892482, 10.57254921413640147, 12.07472987505940409, 13.57779603196559748, 15.07203997055130174, 15.67373306504680386, 16.67002730872509630, 17.62945801330110385, 18.59514990580159832, 19.56632240333010486, 20.54202186413169784, 21.52113328980640006, 22.50240755822210303, 23.48450375772200260, 24.50074590849419565, 25.47886455692250252, 26.45346006570139963, 27.42358464403170615, 28.38842521988249956, 29.34425801996059846, 30.29438266051279527, 31.23569288928990062, 31.61444096390000880 ),
 .UNSPECIFIED. ) ;
#25520 = B_SPLINE_CURVE_WITH_KNOTS ( 'NONE', 3,
 ( #109292, #84616, #100856, #32577, #75690, #66753, #7910, #42081, #76231, #67848, #84070, #102510, #25246, #24145, #58335, #59449, #92460, #68959, #9562, #61120, #87955, #9017, #61657, #43733, #78438, #104185, #77885, #643, #10123, #105287, #17948 ),
 .UNSPECIFIED., .F., .F.,
 ( 4, 2, 2, 2, 2, 2, 2, 2, 2, 2, 2, 2, 1, 2, 2, 4 ),
 ( 0.000000000000000000, 0.2499999999999730216, 0.3749999999999462652, 0.4999999999999195088, 0.6249999999998928635, 0.6874999999998921973, 0.7499999999998915312, 0.8124999999998908651, 0.8749999999998903100, 0.9374999999998896438, 0.9687499999998898659, 0.9843749999998919753, 0.9882812499999029665, 0.9902343749999205080, 0.9921874999999381606, 1.000000000000000000 ),
 .UNSPECIFIED. ) ;
#25522 = ADVANCED_FACE ( 'NONE', ( #97904 ), #65440, .T. ) ;
#25521 = CARTESIAN_POINT ( 'NONE',  ( -16.05668068212990107, 1479.766884033080032, 229.2771335141849818 ) ) ;
#25523 = ORIENTED_EDGE ( 'NONE', *, *, #12558, .T. ) ;
#25524 = DIRECTION ( 'NONE',  ( 9.341989762165448955E-47, -1.000000000000000000, 1.836970198721029688E-16 ) ) ;
#25525 = ADVANCED_FACE ( 'NONE', ( #106856 ), #26052, .F. ) ;
#25526 = CARTESIAN_POINT ( 'NONE',  ( -0.01289782690309849988, 1516.939723362869927, 204.1155860834069813 ) ) ;
#25527 = CARTESIAN_POINT ( 'NONE',  ( -28.65017519560000281, 1509.591492519529993, 207.6322003284180084 ) ) ;
#25528 = CARTESIAN_POINT ( 'NONE',  ( -19.53786426059057746, 1511.187213306747708, 181.5239794925695946 ) ) ;
#25529 = CARTESIAN_POINT ( 'NONE',  ( -43.36595167702599696, 1384.593702623199988, 216.4150399315160200 ) ) ;
#25530 = CARTESIAN_POINT ( 'NONE',  ( -4.398770489489999491, 1409.066668837629777, 194.6843272123980171 ) ) ;
#25531 = CARTESIAN_POINT ( 'NONE',  ( -108.2808028870000072, 1386.465776205880047, 310.9170304772590043 ) ) ;
#25533 = EDGE_LOOP ( 'NONE', ( #21164, #78724, #11922, #99357 ) ) ;
#25532 = CARTESIAN_POINT ( 'NONE',  ( -112.8797039767867432, 1392.913060387289988, 305.0758319338584101 ) ) ;
#25534 = CARTESIAN_POINT ( 'NONE',  ( -25.68353141812590223, 1449.916372628639920, 209.9058930103780085 ) ) ;
#25535 = CARTESIAN_POINT ( 'NONE',  ( 27.39000294680000280, 1488.691910935229998, 209.5725694969789856 ) ) ;
#25536 = CARTESIAN_POINT ( 'NONE',  ( -39.57835122609379397, 1379.656430289635182, 228.3944668109967040 ) ) ;
#25537 = CARTESIAN_POINT ( 'NONE',  ( 19.44143630828250124, 1456.941519871360015, 224.4536055326989867 ) ) ;
#25538 = EDGE_CURVE ( 'NONE', #88339, #32688, #29682, .T. ) ;
#25539 = CARTESIAN_POINT ( 'NONE',  ( -12.20279397044791381, 1516.551704399887512, 191.9693043941118731 ) ) ;
#25540 = CARTESIAN_POINT ( 'NONE',  ( 7.725990161824999980, 1517.181921232829836, 211.6070516194370157 ) ) ;
#25541 = CARTESIAN_POINT ( 'NONE',  ( -68.68489780340000550, 1379.748151576980035, 279.9908545622590168 ) ) ;
#25542 = CARTESIAN_POINT ( 'NONE',  ( -6.049104812149999510, 1450.166793888889970, 209.2893785837540293 ) ) ;
#25543 = CARTESIAN_POINT ( 'NONE',  ( -29.41653895341162439, 1525.790286462514587, 221.5659762852381505 ) ) ;
#25544 = CARTESIAN_POINT ( 'NONE',  ( 6.938478784765000462, 1516.719999691880048, 208.3679751968140010 ) ) ;
#25545 = EDGE_LOOP ( 'NONE', ( #49673, #103234, #13123, #103899 ) ) ;
#25546 = CARTESIAN_POINT ( 'NONE',  ( -2.199032837542779895, 1451.950542369889945, 184.5219133347679872 ) ) ;
#25547 = CARTESIAN_POINT ( 'NONE',  ( -13.95687920409999982, 1412.831204937729808, 227.1595039112980317 ) ) ;
#25548 = CARTESIAN_POINT ( 'NONE',  ( -20.03142830927689388, 1456.423548895029626, 225.1316417485375325 ) ) ;
#25549 = VERTEX_POINT ( 'NONE', #41328 ) ;
#25550 = CARTESIAN_POINT ( 'NONE',  ( 21.54116136303161966, 1523.462669333490112, 234.3126182784851039 ) ) ;
#25551 = ADVANCED_FACE ( 'NONE', ( #15540 ), #9093, .T. ) ;
#25552 = CARTESIAN_POINT ( 'NONE',  ( -11.96603475488899981, 1491.247197521090129, 206.3905183836859862 ) ) ;
#25553 = CARTESIAN_POINT ( 'NONE',  ( 12.32474167489190009, 1434.386220826949966, 150.2103707558300130 ) ) ;
#25554 = CARTESIAN_POINT ( 'NONE',  ( -4.085282425029218345, 1440.421590206651899, 185.3116467681438451 ) ) ;
#25555 = CARTESIAN_POINT ( 'NONE',  ( -6.654072516460000308, 1414.646055428690033, 206.6656543076690014 ) ) ;
#25556 = CARTESIAN_POINT ( 'NONE',  ( -17.44952998132148281, 1525.163457223743990, 237.2403228777125150 ) ) ;
#25557 = EDGE_CURVE ( 'NONE', #12956, #58921, #88443, .T. ) ;
#25558 = CARTESIAN_POINT ( 'NONE',  ( 4.290424513729999667, 1486.223672784390146, 199.2226467242190040 ) ) ;
#25559 = FACE_OUTER_BOUND ( 'NONE', #73648, .T. ) ;
#25560 = DIRECTION ( 'NONE',  ( -0.000000000000000000, -1.000000000000000000, -0.000000000000000000 ) ) ;
#25562 = DIRECTION ( 'NONE',  ( -1.272749556696019889E-16, 0.000000000000000000, 1.000000000000000000 ) ) ;
#25561 = CARTESIAN_POINT ( 'NONE',  ( -2.868433836634999512, 1517.020727862619879, 214.1341630384669941 ) ) ;
#25563 = CARTESIAN_POINT ( 'NONE',  ( 20.35503613270000045, 1509.384884480429946, 188.3699781667980062 ) ) ;
#25564 = DIRECTION ( 'NONE',  ( -5.980589973904019347E-17, 1.000000000000000000, -1.736889445713099699E-16 ) ) ;
#25565 = ORIENTED_EDGE ( 'NONE', *, *, #46890, .T. ) ;
#25566 = CARTESIAN_POINT ( 'NONE',  ( -12.22219588455560135, 1415.434635989099888, 195.9645815201980099 ) ) ;
#25567 = CARTESIAN_POINT ( 'NONE',  ( 15.78266869743918654, 1409.464195827833919, 192.9576493168518709 ) ) ;
#25568 = ORIENTED_EDGE ( 'NONE', *, *, #82556, .F. ) ;
#25569 = CARTESIAN_POINT ( 'NONE',  ( -17.50570382702689898, 1508.551704408389924, 211.8647386576619738 ) ) ;
#25570 = CARTESIAN_POINT ( 'NONE',  ( -31.32995031131182628, 1523.678648413191695, 221.9013357025048947 ) ) ;
#25571 = CARTESIAN_POINT ( 'NONE',  ( 2.485125933802709852, 1524.547873515805350, 175.7096756841900458 ) ) ;
#25572 = UNCERTAINTY_MEASURE_WITH_UNIT (LENGTH_MEASURE( 1.000000000000000082E-05 ), #80901, 'distance_accuracy_value', 'NONE');
#25573 = CARTESIAN_POINT ( 'NONE',  ( 8576.261851438324811, 2833.596074015641989, -10892.29874055200526 ) ) ;
#25574 = CARTESIAN_POINT ( 'NONE',  ( -11.39518164335769868, 1470.898556086270219, 208.5524656631309881 ) ) ;
#25575 = CARTESIAN_POINT ( 'NONE',  ( -6.941072381584187490, 1508.373530314580194, 219.7906263800470583 ) ) ;
#25576 = CARTESIAN_POINT ( 'NONE',  ( 17.74965683759114299, 1423.452220005456184, 226.1321863275825876 ) ) ;
#25578 = ADVANCED_FACE ( 'NONE', ( #68210 ), #77972, .T. ) ;
#25577 = CARTESIAN_POINT ( 'NONE',  ( 13.37406854550570046, 1507.496451373729997, 233.0472692220099873 ) ) ;
#25579 = DIRECTION ( 'NONE',  ( 0.8236474686107853049, 0.5669078173018522460, 0.01484500364079610613 ) ) ;
#25580 = CARTESIAN_POINT ( 'NONE',  ( -7.346057189749999772, 1434.541746329560056, 149.5958201245979922 ) ) ;
#25581 = CARTESIAN_POINT ( 'NONE',  ( 45.67177343720949523, 1440.913060382069943, 266.1885934449759930 ) ) ;
#25583 = CARTESIAN_POINT ( 'NONE',  ( -18.89959486414000267, 1416.839692127460012, 207.5749783441650038 ) ) ;
#25582 = CARTESIAN_POINT ( 'NONE',  ( -6.792894082628190944, 1420.761421989889868, 194.5362997547140083 ) ) ;
#25584 = CARTESIAN_POINT ( 'NONE',  ( 2.582675909241441747, 1526.178928173327677, 242.3428666835334298 ) ) ;
#25585 = ORIENTED_EDGE ( 'NONE', *, *, #17290, .T. ) ;
#25586 = EDGE_CURVE ( 'NONE', #70446, #92411, #19536, .T. ) ;
#25587 = ORIENTED_EDGE ( 'NONE', *, *, #22808, .T. ) ;
#25588 = CARTESIAN_POINT ( 'NONE',  ( -19.05930086066416962, 1519.551704408389924, 223.0490131529958262 ) ) ;
#25589 = ADVANCED_FACE ( 'NONE', ( #87189 ), #18306, .F. ) ;
#25590 = CARTESIAN_POINT ( 'NONE',  ( 2.157536728406360904, 1378.913060387289988, 207.9431782750411912 ) ) ;
#25591 = CARTESIAN_POINT ( 'NONE',  ( -24.41227777330000137, 1441.083062867809986, 212.0377087122379862 ) ) ;
#25592 = CARTESIAN_POINT ( 'NONE',  ( 4.154679781990096465, 1410.434442818600701, 186.0820931863378860 ) ) ;
#25593 = CARTESIAN_POINT ( 'NONE',  ( 4.977085520756839188, 1423.895666356600032, 194.0366106666719759 ) ) ;
#25594 = CARTESIAN_POINT ( 'NONE',  ( -7.789308819770000447, 1507.432058219530063, 181.7020214070979875 ) ) ;
#25595 = EDGE_CURVE ( 'NONE', #36972, #88847, #26070, .T. ) ;
#25596 = CARTESIAN_POINT ( 'NONE',  ( 2.985527909515199863, 1508.551704408389924, 219.4114903352459862 ) ) ;
#25597 = FACE_OUTER_BOUND ( 'NONE', #45406, .T. ) ;
#25598 = CARTESIAN_POINT ( 'NONE',  ( -64.48517748775938685, 1383.791068212090067, 287.7044658124170269 ) ) ;
#25599 = CARTESIAN_POINT ( 'NONE',  ( 3.639705460830000128, 1451.958765405729991, 154.0211597684979949 ) ) ;
#25600 = DIRECTION ( 'NONE',  ( 0.9455185755993178454, 0.000000000000000000, -0.3255681544571537578 ) ) ;
#25601 = CARTESIAN_POINT ( 'NONE',  ( -1.274602950971519988, 1516.603953730839976, 201.4109903819569922 ) ) ;
#25603 = VERTEX_POINT ( 'NONE', #104539 ) ;
#25602 = CARTESIAN_POINT ( 'NONE',  ( 10.56891618719440018, 1452.605324780220144, 209.6008627037060137 ) ) ;
#25604 = CARTESIAN_POINT ( 'NONE',  ( 19.02974267272306719, 1522.051704408389924, 211.0809136819971741 ) ) ;
#25605 = CARTESIAN_POINT ( 'NONE',  ( -35.50363208510000135, 1379.896902233160063, 227.2934423945590083 ) ) ;
#25606 = CARTESIAN_POINT ( 'NONE',  ( 19.79774116257700101, 1508.248996258070065, 229.3423194934649700 ) ) ;
#25607 = ORIENTED_EDGE ( 'NONE', *, *, #48788, .T. ) ;
#25608 = ORIENTED_EDGE ( 'NONE', *, *, #41875, .T. ) ;
#25609 = DIRECTION ( 'NONE',  ( 0.000000000000000000, 1.000000000000000000, 0.000000000000000000 ) ) ;
#25610 = CARTESIAN_POINT ( 'NONE',  ( -12.74986059157959950, 1462.837634083790135, 224.9935237458099948 ) ) ;
#25611 = CARTESIAN_POINT ( 'NONE',  ( 38.69602499724199873, 1439.330795836810012, 136.6667434724849954 ) ) ;
#25613 = FACE_OUTER_BOUND ( 'NONE', #53941, .T. ) ;
#25612 = FACE_OUTER_BOUND ( 'NONE', #21431, .T. ) ;
#25614 = EDGE_CURVE ( 'NONE', #59443, #63161, #12892, .T. ) ;
#25615 = CARTESIAN_POINT ( 'NONE',  ( 11.73451145560060027, 1479.801820424849893, 210.2140368403210005 ) ) ;
#25616 = CARTESIAN_POINT ( 'NONE',  ( -107.0843635519999992, 1382.329134876569924, 298.0462323021590691 ) ) ;
#25617 = FACE_OUTER_BOUND ( 'NONE', #52288, .T. ) ;
#25618 = CARTESIAN_POINT ( 'NONE',  ( -0.3166280365204529046, 1452.331784132522216, 183.2228567542290989 ) ) ;
#25619 = CARTESIAN_POINT ( 'NONE',  ( -20.15452302159999931, 1507.845791376729949, 228.9024215066979764 ) ) ;
#25620 = CARTESIAN_POINT ( 'NONE',  ( 1.834053397919999995, 1410.355893698830187, 185.3938420458979977 ) ) ;
#25621 = CARTESIAN_POINT ( 'NONE',  ( -0.7527848377683918901, 1485.932384399170132, 197.2449775714050020 ) ) ;
#25623 = EDGE_CURVE ( 'NONE', #18936, #84966, #63611, .T. ) ;
#25622 = CARTESIAN_POINT ( 'NONE',  ( 10.58843039633059924, 1471.621789236399991, 212.0273906003420166 ) ) ;
#25624 = CARTESIAN_POINT ( 'NONE',  ( 4.249059288160469627, 1433.039579511759939, 201.5637155983669970 ) ) ;
#25625 = CARTESIAN_POINT ( 'NONE',  ( -2.500000000000000000, 1439.072262259579929, 157.1874756602519767 ) ) ;
#25626 = CARTESIAN_POINT ( 'NONE',  ( 11.79165749935659946, 1429.416858706420044, 146.4064136026630081 ) ) ;
#25627 = CARTESIAN_POINT ( 'NONE',  ( 0.4604323351460000158, 1465.011193676930134, 237.3689745248979932 ) ) ;
#25628 = ORIENTED_EDGE ( 'NONE', *, *, #35575, .T. ) ;
#25629 = CARTESIAN_POINT ( 'NONE',  ( -13.46445246340000068, 1470.514529015489870, 192.0392451277990062 ) ) ;
#25630 = CARTESIAN_POINT ( 'NONE',  ( -43.99260286630000394, 1444.142798274959887, 270.2177640581980427 ) ) ;
#25631 = DIRECTION ( 'NONE',  ( 0.000000000000000000, -1.000000000000000000, 6.123233995736769734E-17 ) ) ;
#25632 = CARTESIAN_POINT ( 'NONE',  ( 22.19805589962659553, 1506.691119430664912, 209.3127852580865067 ) ) ;
#25633 = CARTESIAN_POINT ( 'NONE',  ( 16.93884302589999891, 1507.634939823729837, 188.0954313829980151 ) ) ;
#25634 = CARTESIAN_POINT ( 'NONE',  ( -1.081760175521900104E-08, 1473.331368512430117, 261.9578586066839421 ) ) ;
#25635 = CARTESIAN_POINT ( 'NONE',  ( 9.611939569861299049, 1460.529529387680213, 206.0552052590290089 ) ) ;
#25636 = CARTESIAN_POINT ( 'NONE',  ( -1.433831019619999925, 1415.263254653229978, 227.1906885494979917 ) ) ;
#25637 = CARTESIAN_POINT ( 'NONE',  ( -8.185464237450000624, 1418.160221195129907, 231.1370887997979935 ) ) ;
#25638 = CARTESIAN_POINT ( 'NONE',  ( 0.06163407857050130084, 1477.698269665189855, 198.6861886841990099 ) ) ;
#25639 = CARTESIAN_POINT ( 'NONE',  ( -104.4869036590000064, 1389.270867165570053, 307.8650956148590012 ) ) ;
#25640 =( BOUNDED_CURVE ( )  B_SPLINE_CURVE ( 3, ( #97690, #63039, #3666, #54619 ),
 .UNSPECIFIED., .F., .F. ) 
 B_SPLINE_CURVE_WITH_KNOTS ( ( 4, 4 ),
 ( 1.268017769446416088, 1.928411124454499914 ),
 .UNSPECIFIED. ) 
 CURVE ( )  GEOMETRIC_REPRESENTATION_ITEM ( )  RATIONAL_B_SPLINE_CURVE ( ( 1.000000000000000000, 0.9639857288382313039, 0.9639857288382313039, 1.000000000000000000 ) ) 
 REPRESENTATION_ITEM ( '' )  );
#25641 = CARTESIAN_POINT ( 'NONE',  ( -0.6429601867158417638, 1485.414621978292644, 181.9392741304039305 ) ) ;
#25642 = CARTESIAN_POINT ( 'NONE',  ( 6.171356481870118316, 1359.214203302260557, 209.6218459617033432 ) ) ;
#25643 = CARTESIAN_POINT ( 'NONE',  ( -46.03855999566639667, 1438.451647596259818, 268.2082775289269989 ) ) ;
#25644 = CARTESIAN_POINT ( 'NONE',  ( 3.611741757648789797, 1428.548660076119859, 216.5582848978089885 ) ) ;
#25645 = CARTESIAN_POINT ( 'NONE',  ( -7.887122863889999280, 1426.208111655430002, 206.9861596317290093 ) ) ;
#25646 = VECTOR ( 'NONE', #105649, 1000.000000000000000 ) ;
#25647 = ORIENTED_EDGE ( 'NONE', *, *, #13471, .T. ) ;
#25648 = CARTESIAN_POINT ( 'NONE',  ( -1.906501101195560124E-08, 1517.020990152690047, 209.1218459511669892 ) ) ;
#25649 = CARTESIAN_POINT ( 'NONE',  ( -2.478941618209999920, 1432.378565395950091, 157.5169325447980100 ) ) ;
#25650 = CARTESIAN_POINT ( 'NONE',  ( -15.90990259576500065, 1516.814170398969964, 224.3246417466669982 ) ) ;
#25651 = CARTESIAN_POINT ( 'NONE',  ( 7.532152985507379661, 1425.792267630160040, 212.2199176514089913 ) ) ;
#25652 = CARTESIAN_POINT ( 'NONE',  ( -26.68850062112660027, 1451.728563988709993, 135.8012203878940056 ) ) ;
#25653 = ORIENTED_EDGE ( 'NONE', *, *, #30579, .T. ) ;
#25654 = CARTESIAN_POINT ( 'NONE',  ( 23.18116579810000033, 1432.896189078000134, 217.2884692092180217 ) ) ;
#25656 = CARTESIAN_POINT ( 'NONE',  ( -15.03014123622689979, 1513.722010161890012, 223.7517583984009946 ) ) ;
#25655 = CARTESIAN_POINT ( 'NONE',  ( -11.34466715848219920, 1491.663308851389957, 206.9207944444179930 ) ) ;
#25657 = CARTESIAN_POINT ( 'NONE',  ( 11.60004869885203682, 1425.894332500278097, 137.5113157688821275 ) ) ;
#25658 = CARTESIAN_POINT ( 'NONE',  ( -3.269259737218870310, 1476.740802116999930, 199.2818558394819775 ) ) ;
#25659 = CARTESIAN_POINT ( 'NONE',  ( 2.738491027449999837, 1419.583501809659765, 204.7124689335390144 ) ) ;
#25660 = CARTESIAN_POINT ( 'NONE',  ( -13.74310390781900004, 1517.151704408390060, 201.1531303618569950 ) ) ;
#25661 = DIRECTION ( 'NONE',  ( 0.3255681544571546460, 0.000000000000000000, 0.9455185755993176233 ) ) ;
#25662 = ORIENTED_EDGE ( 'NONE', *, *, #54341, .F. ) ;
#25663 = CARTESIAN_POINT ( 'NONE',  ( -4.950908079962929698, 1408.434846368340004, 270.3888801776009814 ) ) ;
#25664 = CARTESIAN_POINT ( 'NONE',  ( 4.685675373058309390, 1417.752609642629977, 232.3318985854729988 ) ) ;
#25665 = CARTESIAN_POINT ( 'NONE',  ( -0.4228489488307095034, 1508.822448670140602, 238.3614536558768577 ) ) ;
#25667 = VERTEX_POINT ( 'NONE', #21059 ) ;
#25666 = CARTESIAN_POINT ( 'NONE',  ( -2.500000000000000000, 1439.481493142219961, 163.2933147462130137 ) ) ;
#25668 = ORIENTED_EDGE ( 'NONE', *, *, #832, .F. ) ;
#25669 = CARTESIAN_POINT ( 'NONE',  ( -23.81374637684410089, 1410.984159143959914, 210.1595746859130145 ) ) ;
#25670 = CARTESIAN_POINT ( 'NONE',  ( -0.0001149583598519999974, 1408.913064401730026, 186.4639625088979926 ) ) ;
#25671 = CARTESIAN_POINT ( 'NONE',  ( -109.9854347995050006, 1384.902532624669902, 311.4562314680339910 ) ) ;
#25672 = CARTESIAN_POINT ( 'NONE',  ( -45.63203486222421645, 1439.443257688872563, 266.1896917324526726 ) ) ;
#25673 = B_SPLINE_CURVE_WITH_KNOTS ( 'NONE', 3,
 ( #103454, #7210, #51416, #26760, #93954, #58720, #60949, #84463, #50869, #101232, #487, #24532, #9414, #34610, #42456, #101795, #50338, #68796, #102897, #59289, #102357, #7750, #86120, #76615, #76071, #84999, #110767, #34057, #25641, #17220, #95076, #85547, #26195, #43576, #60383, #41368, #3806, #1581, #35716, #96179, #104019, #97819, #21097, #71579, #44133, #106232, #69905, #19454, #20013, #28983, #18894, #79385, #29518, #72117, #2149, #63709 ),
 .UNSPECIFIED., .F., .F.,
 ( 4, 2, 1, 1, 1, 1, 2, 2, 2, 2, 1, 1, 1, 2, 2, 2, 2, 1, 2, 2, 2, 1, 1, 1, 2, 2, 2, 2, 1, 2, 2, 2, 2, 4 ),
 ( 0.000000000000000000, 0.06250000000058465732, 0.09375000000078338724, 0.1093750000008827661, 0.1171875000010262624, 0.1210937500010046269, 0.1230468750009933304, 0.1250000000009820478, 0.1875000000034836301, 0.2187500000048276938, 0.2343750000054989624, 0.2421875000058345828, 0.2460937500060023930, 0.2480468750060855210, 0.2500000000061686212, 0.3750000000050800475, 0.4375000000045334847, 0.4687500000042576498, 0.4843750000041224801, 0.5000000000039872550, 0.6250000000038240522, 0.6875000000037424508, 0.7187500000036169956, 0.7343750000035543790, 0.7421875000034289238, 0.7500000000033034686, 0.8125000000023775426, 0.8437500000019949598, 0.8593750000017285062, 0.8671875000015897283, 0.8750000000014510615, 0.9062500000010844659, 0.9375000000007178702, 1.000000000000000000 ),
 .UNSPECIFIED. ) ;
#25674 = CARTESIAN_POINT ( 'NONE',  ( -20.90394540422069980, 1503.716088646810022, 192.3069530248390038 ) ) ;
#25675 = CARTESIAN_POINT ( 'NONE',  ( -17.94945718479999996, 1425.820490840630100, 226.0414718358979940 ) ) ;
#25676 = CARTESIAN_POINT ( 'NONE',  ( 30.14929311095689712, 1467.662589780429926, 268.0960305645629660 ) ) ;
#25677 = CARTESIAN_POINT ( 'NONE',  ( -11.60429320023880173, 1391.913060387170162, 208.2952356049119658 ) ) ;
#25678 = CARTESIAN_POINT ( 'NONE',  ( -17.10883999351027995, 1422.201703527962763, 226.7517257450004990 ) ) ;
#25679 = CARTESIAN_POINT ( 'NONE',  ( -1.715704529104999931, 1516.757508073510053, 205.8704515699670026 ) ) ;
#25680 = VERTEX_POINT ( 'NONE', #55264 ) ;
#25681 = CARTESIAN_POINT ( 'NONE',  ( 18.29456550085305722, 1459.185740094880657, 227.8225150847868576 ) ) ;
#25682 = CARTESIAN_POINT ( 'NONE',  ( -1.430539248151910137, 1444.328264662749916, 199.1703804428329931 ) ) ;
#25683 = CARTESIAN_POINT ( 'NONE',  ( 1.984413551915469975, 1517.051704408389924, 198.9129232538419956 ) ) ;
#25684 = EDGE_LOOP ( 'NONE', ( #34785, #54051, #19187, #74443, #103440, #21951, #47235, #101996, #14452, #91089, #94861, #61313, #103988, #10077 ) ) ;
#25685 = CARTESIAN_POINT ( 'NONE',  ( 2.994691737410000165, 1448.276535293540064, 183.8510770426980230 ) ) ;
#25686 = CARTESIAN_POINT ( 'NONE',  ( 26.90457551740000142, 1451.808372585929874, 135.6460129701980009 ) ) ;
#25687 = CARTESIAN_POINT ( 'NONE',  ( 2.487935123032368967, 1508.783371655767951, 204.5758637342562452 ) ) ;
#25688 = CARTESIAN_POINT ( 'NONE',  ( -1.545842073307790221, 1419.284905465829979, 228.1300558533139906 ) ) ;
#25689 = CARTESIAN_POINT ( 'NONE',  ( 7.377575598780000021, 1422.796019154259966, 195.5835889348989838 ) ) ;
#25690 = FACE_OUTER_BOUND ( 'NONE', #31721, .T. ) ;
#25691 = CARTESIAN_POINT ( 'NONE',  ( 17.22592482065188335, 1444.324653571828321, 162.9227486220069352 ) ) ;
#25692 = CARTESIAN_POINT ( 'NONE',  ( 0.8431686273640290885, 1408.942504484590017, 186.6283956538120208 ) ) ;
#25694 = DIRECTION ( 'NONE',  ( 0.3282391760791590340, 0.000000000000000000, 0.9445946449598763284 ) ) ;
#25693 = CARTESIAN_POINT ( 'NONE',  ( 30.57065064345538374, 1523.844782250838307, 196.3873375281003177 ) ) ;
#25695 = CARTESIAN_POINT ( 'NONE',  ( 5.558638042260000134, 1409.107172305129779, 229.7071683781979914 ) ) ;
#25696 = CARTESIAN_POINT ( 'NONE',  ( -12.00298711920000017, 1378.730876743509953, 212.7098913336589874 ) ) ;
#25697 = CARTESIAN_POINT ( 'NONE',  ( 13.38476763809124392, 1421.175358059063910, 231.0590627358187987 ) ) ;
#25698 = ORIENTED_EDGE ( 'NONE', *, *, #65850, .T. ) ;
#25699 = CARTESIAN_POINT ( 'NONE',  ( -1.484142863822457858, 1526.349689584397083, 178.3401621312602572 ) ) ;
#25700 = CARTESIAN_POINT ( 'NONE',  ( 11.69294537312310212, 1432.337845730949994, 150.8474185596319899 ) ) ;
#25701 = CARTESIAN_POINT ( 'NONE',  ( 16.81223453394349932, 1414.913060391199906, 210.6693087035600058 ) ) ;
#25702 = CARTESIAN_POINT ( 'NONE',  ( -10.22564300610000032, 1389.880884843570129, 202.1309545629490003 ) ) ;
#25703 = CARTESIAN_POINT ( 'NONE',  ( 8.576574437940319484, 1426.670950778500128, 211.0879220285609961 ) ) ;
#25704 = CARTESIAN_POINT ( 'NONE',  ( -35.36897276635060194, 1450.220808574710190, 136.2318720995220076 ) ) ;
#25705 = CARTESIAN_POINT ( 'NONE',  ( -10.99440994877370059, 1462.600064137660183, 208.0385998618030214 ) ) ;
#25706 = ADVANCED_FACE ( 'NONE', ( #56353 ), #15268, .T. ) ;
#25707 = CARTESIAN_POINT ( 'NONE',  ( -12.15345572500000060, 1468.554006641229989, 265.6112251771979800 ) ) ;
#25708 = CARTESIAN_POINT ( 'NONE',  ( -21.30850104442570725, 1508.868632323871680, 191.9271483346492175 ) ) ;
#25710 = EDGE_CURVE ( 'NONE', #109266, #94676, #63135, .T. ) ;
#25709 = CARTESIAN_POINT ( 'NONE',  ( 11.27545180150000093, 1433.597762786930161, 151.5307970856979978 ) ) ;
#25711 = CARTESIAN_POINT ( 'NONE',  ( 19.00000000000000000, 1440.913060387330006, 209.1218459616979999 ) ) ;
#25712 = CARTESIAN_POINT ( 'NONE',  ( 12.61823209568870041, 1416.826860677879949, 196.1892328963569980 ) ) ;
#25713 = CARTESIAN_POINT ( 'NONE',  ( 18.36305868314869727, 1428.555240223059855, 201.4018503782459959 ) ) ;
#25714 = CARTESIAN_POINT ( 'NONE',  ( 12.37883759903940017, 1420.474967537750217, 199.7601132055380049 ) ) ;
#25715 = AXIS2_PLACEMENT_3D ( 'NONE', #60406, #77205, #23995 ) ;
#25716 = CARTESIAN_POINT ( 'NONE',  ( 5.938839624758309732, 1465.760319836029794, 217.5705628005549954 ) ) ;
#25717 = CARTESIAN_POINT ( 'NONE',  ( 23.10442899973940101, 1411.095127650270115, 207.3185325528490068 ) ) ;
#25718 = CARTESIAN_POINT ( 'NONE',  ( 12.26702939395647007, 1398.276750168901572, 204.6184358455272445 ) ) ;
#25719 = CARTESIAN_POINT ( 'NONE',  ( -21.40702923872559893, 1509.660610321120203, 231.3015350172729825 ) ) ;
#25720 = CARTESIAN_POINT ( 'NONE',  ( 23.18005801880000050, 1410.911243130629828, 212.9212581473880164 ) ) ;
#25721 = VECTOR ( 'NONE', #39896, 1000.000000000000227 ) ;
#25722 = ADVANCED_FACE ( 'NONE', ( #41741 ), #33181, .T. ) ;
#25723 = CARTESIAN_POINT ( 'NONE',  ( 19.25375188179999952, 1464.258769156330118, 224.0689215379980226 ) ) ;
#25724 = CARTESIAN_POINT ( 'NONE',  ( 25.44482548711661707, 1436.625151458925302, 137.3198232488083477 ) ) ;
#25725 = CARTESIAN_POINT ( 'NONE',  ( 10.34950188612880062, 1451.639534178259964, 207.2650128704659949 ) ) ;
#25726 = CARTESIAN_POINT ( 'NONE',  ( 19.81155763900000011, 1453.313060387329870, 213.6835017937279986 ) ) ;
#25727 = CARTESIAN_POINT ( 'NONE',  ( -12.04602614745110145, 1481.198043355260097, 227.9689297718389867 ) ) ;
#25728 = CARTESIAN_POINT ( 'NONE',  ( 3.460101851884999746, 1516.812923327049930, 213.1504765548870068 ) ) ;
#25729 = CARTESIAN_POINT ( 'NONE',  ( -20.71620237759999839, 1418.282126647740142, 210.1201477243000113 ) ) ;
#25730 = CARTESIAN_POINT ( 'NONE',  ( 0.2053818061695609765, 1459.950573050879939, 182.9551974283099867 ) ) ;
#25732 = EDGE_LOOP ( 'NONE', ( #73133, #17550, #68180, #81637, #5603, #6573, #100267, #7842 ) ) ;
#25731 = LINE ( 'NONE', #104668, #21106 ) ;
#25733 = CARTESIAN_POINT ( 'NONE',  ( -24.17420166734180498, 1452.068876450862490, 137.1289955490235855 ) ) ;
#25734 = CARTESIAN_POINT ( 'NONE',  ( -38.71377205869448801, 1443.913060387330233, 136.9322096537518973 ) ) ;
#25735 = CARTESIAN_POINT ( 'NONE',  ( -10.41132050640263174, 1519.551704408389924, 189.4661702785461728 ) ) ;
#25736 = CARTESIAN_POINT ( 'NONE',  ( -39.63067020672009733, 1438.364472241019939, 134.0999999979140114 ) ) ;
#25737 = CARTESIAN_POINT ( 'NONE',  ( -115.1534609392471395, 1305.714868215269917, 309.4347587285261625 ) ) ;
#25738 = VERTEX_POINT ( 'NONE', #7586 ) ;
#25739 = B_SPLINE_SURFACE_WITH_KNOTS ( 'NONE', 5, 5, ( 
 ( #70520, #18955, #104635, #28486, #36877, #2757 ),
 ( #19516, #27932, #96240, #53721, #105195, #45856 ),
 ( #80251, #52860, #28743, #19206, #94840, #53408 ),
 ( #27638, #18661, #18116, #96500, #19780, #86987 ),
 ( #78035, #105454, #104899, #3021, #45019, #45572 ),
 ( #62948, #62374, #70787, #3569, #61823, #10276 ) ),
 .UNSPECIFIED., .F., .F., .F.,
 ( 6, 6 ),
 ( 6, 6 ),
 ( 6.877204621659999795, 14.95798807776640160 ),
 ( -0.002550205044612160153, 2.002549943480759875 ),
 .UNSPECIFIED. ) ;
#25740 = CARTESIAN_POINT ( 'NONE',  ( -10.17543907640000000, 1472.210474395689971, 209.2297550078889969 ) ) ;
#25741 = CARTESIAN_POINT ( 'NONE',  ( -11.97102458384909873, 1391.459503355940114, 212.4918544850630155 ) ) ;
#25742 = CARTESIAN_POINT ( 'NONE',  ( -16.47341459099999739, 1414.971287085229960, 211.7498588889980056 ) ) ;
#25743 = CARTESIAN_POINT ( 'NONE',  ( -16.65100080374379843, 1526.335487865669393, 183.3462803417096723 ) ) ;
#25744 = CARTESIAN_POINT ( 'NONE',  ( -4.150844423549710172, 1433.756621307029945, 217.8254834218780047 ) ) ;
#25745 = CARTESIAN_POINT ( 'NONE',  ( -109.2894791384494653, 1382.540884933779353, 311.0173327546005453 ) ) ;
#25746 = CARTESIAN_POINT ( 'NONE',  ( 22.64731540989999914, 1507.637957906029897, 209.7207049147999953 ) ) ;
#25747 = CARTESIAN_POINT ( 'NONE',  ( -5.364455102291621813, 1422.311257715712372, 141.1472075467242462 ) ) ;
#25748 = DIRECTION ( 'NONE',  ( 0.000000000000000000, 1.000000000000000000, 0.000000000000000000 ) ) ;
#25749 = B_SPLINE_SURFACE_WITH_KNOTS ( 'NONE', 5, 5, ( 
 ( #104853, #102612, #61238, #18071, #25912, #52266 ),
 ( #9140, #10802, #94227, #9678, #1869, #69627 ),
 ( #76904, #43303, #18612, #36543, #8572, #44972 ),
 ( #43847, #77994, #753, #103750, #61776, #1299 ),
 ( #27052, #95352, #60110, #17502, #52812, #93664 ),
 ( #44411, #78551, #51146, #36002, #70195, #27591 ),
 ( #95900, #85272, #79120, #21908, #56104, #12976 ),
 ( #47159, #54482, #3522, #71295, #46073, #88072 ),
 ( #63979, #81286, #72373, #4601, #55571, #11359 ) ),
 .UNSPECIFIED., .F., .F., .F.,
 ( 6, 3, 6 ),
 ( 6, 6 ),
 ( -3.623787203323129550E-05, 8.942376592629999621, 17.88478942317200193 ),
 ( -3.623787203323129550E-05, 2.000000000000000000 ),
 .UNSPECIFIED. ) ;
#25750 = CARTESIAN_POINT ( 'NONE',  ( -77.54836707579930533, 1385.147474671279952, 279.6196463459559709 ) ) ;
#25751 = CIRCLE ( 'NONE', #70493, 2.000000000000003109 ) ;
#25752 = EDGE_CURVE ( 'NONE', #89980, #56739, #68961, .T. ) ;
#25753 = CARTESIAN_POINT ( 'NONE',  ( -20.71343476517490600, 1522.382868172863937, 238.3377464195766606 ) ) ;
#25754 = CARTESIAN_POINT ( 'NONE',  ( 10.05758522378950026, 1423.330231444269884, 209.0100830007820321 ) ) ;
#25755 = EDGE_LOOP ( 'NONE', ( #32228, #74018, #86672, #46996, #106199, #1699, #37512 ) ) ;
#25756 = CARTESIAN_POINT ( 'NONE',  ( -29.31191257029999875, 1451.029043731829915, 136.3073297265979988 ) ) ;
#25757 = CARTESIAN_POINT ( 'NONE',  ( 17.11714625305222981, 1443.086052842849995, 162.7561045841209193 ) ) ;
#25759 = EDGE_LOOP ( 'NONE', ( #64883, #27264, #85845, #47625, #32133 ) ) ;
#25758 = DIRECTION ( 'NONE',  ( -0.4999999999998399614, 0.7071067811867740582, -0.4999999999998399614 ) ) ;
#25760 = CARTESIAN_POINT ( 'NONE',  ( 1.959285271270000184, 1474.800623574289830, 220.3715841371990223 ) ) ;
#25761 = EDGE_CURVE ( 'NONE', #59101, #4103, #82199, .T. ) ;
#25762 = CARTESIAN_POINT ( 'NONE',  ( -18.17365796220000007, 1441.208305948289762, 213.5442559039389891 ) ) ;
#25763 = CARTESIAN_POINT ( 'NONE',  ( -7.592250591143125504, 1364.366890427691942, 209.6218459617148824 ) ) ;
#25764 = CARTESIAN_POINT ( 'NONE',  ( -7.208571784880000166, 1494.204594205489911, 199.0650244531990154 ) ) ;
#25765 = CARTESIAN_POINT ( 'NONE',  ( 38.49563125392135277, 1453.175225740012138, 269.5844195324700650 ) ) ;
#25766 = CARTESIAN_POINT ( 'NONE',  ( -22.52594230423108002, 1509.699683626128490, 190.3521439076764068 ) ) ;
#25767 = CARTESIAN_POINT ( 'NONE',  ( 19.27691768841802045, 1439.085048996816795, 212.6567080453250753 ) ) ;
#25768 = CARTESIAN_POINT ( 'NONE',  ( 9108.204429824800172, -2340.220200558880151, 1988.052214260419987 ) ) ;
#25769 = CARTESIAN_POINT ( 'NONE',  ( 7.253065918429999925, 1447.817965204990060, 203.4084464636989935 ) ) ;
#25770 = DIRECTION ( 'NONE',  ( 0.000000000000000000, 0.000000000000000000, -1.000000000000000000 ) ) ;
#25771 = CARTESIAN_POINT ( 'NONE',  ( -9.209502321770001387, 1366.683160837839978, 207.6218459616989946 ) ) ;
#25772 = CARTESIAN_POINT ( 'NONE',  ( -29.00779973304124582, 1526.382868172864164, 217.2942086403127178 ) ) ;
#25773 = CARTESIAN_POINT ( 'NONE',  ( 7.709681268295000223, 1516.559109716219837, 206.2491454149069909 ) ) ;
#25774 = CYLINDRICAL_SURFACE ( 'NONE', #35768, 2.000000000000003553 ) ;
#25775 = B_SPLINE_SURFACE_WITH_KNOTS ( 'NONE', 5, 5, ( 
 ( #26604, #103874, #17068, #18199, #44534, #36677 ),
 ( #94926, #10928, #104429, #61359, #1421, #27721 ),
 ( #53497, #52396, #86519, #9812, #45104, #51265 ),
 ( #77033, #85398, #95478, #34466, #43978, #18745 ),
 ( #30470, #106623, #38861, #54608, #13642, #72494 ),
 ( #89826, #55705, #12575, #5271, #89278, #64656 ),
 ( #46204, #98775, #96588, #28273, #37232, #62466 ),
 ( #47832, #98223, #22037, #4717, #3103, #55157 ),
 ( #37784, #29910, #64102, #38315, #80338, #71428 ),
 ( #20403, #71973, #21493, #13098, #81965, #54063 ),
 ( #80886, #88190, #46755, #81405, #19860, #3655 ),
 ( #56234, #88739, #105544, #11482, #4182, #73039 ),
 ( #90364, #47282, #28831, #107178, #104983, #70870 ),
 ( #45658, #12024, #79797, #63029, #97134, #106085 ),
 ( #29363, #63564, #97679, #20952, #92573, #65198 ),
 ( #75793, #33223, #15307, #31018, #109945, #6921 ),
 ( #57900, #83085, #59003, #92035, #67412, #101512 ),
 ( #41077, #50049, #14767, #49499, #84724, #74153 ),
 ( #75255, #24798, #16398, #57363, #83624, #39977 ),
 ( #109404, #99864, #91487, #6378, #73603, #48398 ),
 ( #100968, #107733, #5837, #108283, #58445, #108833 ),
 ( #24265, #15844, #50593, #22584, #56789, #32680 ),
 ( #48954, #7476, #14212, #40524, #74702, #66859 ),
 ( #90926, #99310, #93131, #84178, #82541, #31570 ) ),
 .UNSPECIFIED., .F., .F., .F.,
 ( 6, 3, 3, 3, 3, 3, 3, 6 ),
 ( 6, 6 ),
 ( 0.000000000000000000, 19.27951045849999900, 37.56883265599999788, 64.75259520960000259, 97.48063803579999842, 123.9428332119999965, 141.7919792689999952, 160.6499452009999800 ),
 ( 3.122614431000000135, 7.854052422239930387 ),
 .UNSPECIFIED. ) ;
#25776 = DIRECTION ( 'NONE',  ( 0.5412924984494058567, 0.1391731009594480151, 0.8292365640103740443 ) ) ;
#25777 = CARTESIAN_POINT ( 'NONE',  ( 13.79577721849999961, 1416.837309283630020, 196.3345427477979968 ) ) ;
#25779 = ORIENTED_EDGE ( 'NONE', *, *, #55141, .T. ) ;
#25778 = CARTESIAN_POINT ( 'NONE',  ( 1.702416242259999768, 1493.957958499289816, 220.1113518661990156 ) ) ;
#25780 = LINE ( 'NONE', #94655, #95641 ) ;
#25781 = VERTEX_POINT ( 'NONE', #52922 ) ;
#25782 = CARTESIAN_POINT ( 'NONE',  ( -16.19963475833718647, 1512.859148089886276, 220.4046715791462532 ) ) ;
#25783 = CARTESIAN_POINT ( 'NONE',  ( -24.55148953109999965, 1430.358502428329984, 207.1124260302279652 ) ) ;
#25785 = CARTESIAN_POINT ( 'NONE',  ( 16.70811614616980023, 1409.743563081069851, 192.5257515985450141 ) ) ;
#25784 = CARTESIAN_POINT ( 'NONE',  ( -11.40400955750629919, 1426.004897788209973, 127.8394256862669920 ) ) ;
#25786 = CARTESIAN_POINT ( 'NONE',  ( 2.881222757585000238, 1516.891731298979948, 211.5992195760969707 ) ) ;
#25787 = CARTESIAN_POINT ( 'NONE',  ( 17.77641320823512672, 1509.653574700879062, 184.9552422975178843 ) ) ;
#25788 = DIRECTION ( 'NONE',  ( 0.000000000000000000, 0.000000000000000000, -1.000000000000000000 ) ) ;
#25789 = CARTESIAN_POINT ( 'NONE',  ( -42.46016416089999979, 1427.243204226630041, 266.3334699379980179 ) ) ;
#25790 = CARTESIAN_POINT ( 'NONE',  ( -13.06508296313580075, 1379.379227062329846, 208.5508266283169689 ) ) ;
#25791 = CARTESIAN_POINT ( 'NONE',  ( 44.93136772329302175, 1446.458183624383310, 269.6838061997164573 ) ) ;
#25792 = CARTESIAN_POINT ( 'NONE',  ( 3.742606737671509975, 1508.551704408389924, 213.7724622950010200 ) ) ;
#25793 = CARTESIAN_POINT ( 'NONE',  ( -37.31136631233590606, 1438.104314947570174, 136.5707455465820033 ) ) ;
#25794 = ORIENTED_EDGE ( 'NONE', *, *, #79495, .F. ) ;
#25795 = CARTESIAN_POINT ( 'NONE',  ( 8.565474820639810360, 1396.738687322869964, 218.6445593244839927 ) ) ;
#25796 = CARTESIAN_POINT ( 'NONE',  ( -19.29973955919999895, 1464.638518991389901, 213.2496029295089954 ) ) ;
#25797 = CARTESIAN_POINT ( 'NONE',  ( -17.96824696200000204, 1459.790589356729924, 228.0722388631980095 ) ) ;
#25798 = ORIENTED_EDGE ( 'NONE', *, *, #63819, .F. ) ;
#25799 = ORIENTED_EDGE ( 'NONE', *, *, #78172, .F. ) ;
#25800 = VECTOR ( 'NONE', #109309, 1000.000000000000000 ) ;
#25801 = CARTESIAN_POINT ( 'NONE',  ( 5.277460848200000498, 1426.742654866309977, 191.8370381630989812 ) ) ;
#25802 = CARTESIAN_POINT ( 'NONE',  ( -9.236167301360001858, 1423.625854809029988, 144.1549878472980026 ) ) ;
#25803 = CARTESIAN_POINT ( 'NONE',  ( 18.69816095120771493, 1526.382868172863937, 234.8576566410002897 ) ) ;
#25804 = CARTESIAN_POINT ( 'NONE',  ( -14.16755010633700174, 1508.249070031330120, 209.5474642701840082 ) ) ;
#25805 = CARTESIAN_POINT ( 'NONE',  ( 4.282704111100000155, 1515.349907855090123, 210.2219876055189900 ) ) ;
#25806 = DIRECTION ( 'NONE',  ( 0.000000000000000000, 1.000000000000000000, 0.000000000000000000 ) ) ;
#25807 = CARTESIAN_POINT ( 'NONE',  ( -2.896421349160000158, 1461.194462919229863, 234.8054986878979946 ) ) ;
#25808 = CARTESIAN_POINT ( 'NONE',  ( 3.644878262961745108, 1516.661627594595529, 215.6772027093610120 ) ) ;
#25809 = CARTESIAN_POINT ( 'NONE',  ( 10.57600172136130112, 1452.469479793819801, 209.2385615662339831 ) ) ;
#25810 = CARTESIAN_POINT ( 'NONE',  ( 16.68463225827704122, 1442.773887286370382, 162.0935120918187806 ) ) ;
#25811 = CARTESIAN_POINT ( 'NONE',  ( -104.7048071253149999, 1384.888671349390052, 296.8869291217460500 ) ) ;
#25812 = ORIENTED_EDGE ( 'NONE', *, *, #92471, .F. ) ;
#25813 = CARTESIAN_POINT ( 'NONE',  ( 2.869693458934999608, 1517.070197312179971, 203.3343689375869872 ) ) ;
#25814 = CARTESIAN_POINT ( 'NONE',  ( -1.709766532154999963, 1516.959716008189844, 209.1345041580460133 ) ) ;
#25815 = VERTEX_POINT ( 'NONE', #34448 ) ;
#25816 = CARTESIAN_POINT ( 'NONE',  ( 11.74539289358659921, 1426.717885751599852, 144.7561986137889960 ) ) ;
#25817 = CARTESIAN_POINT ( 'NONE',  ( 4.487065301914353377, 1511.405768592958111, 217.4750366866610420 ) ) ;
#25818 = EDGE_LOOP ( 'NONE', ( #405, #69873, #82723, #49406 ) ) ;
#25819 = CARTESIAN_POINT ( 'NONE',  ( 20.59269117493390056, 1507.766073655780019, 227.7908423917359926 ) ) ;
#25820 = CARTESIAN_POINT ( 'NONE',  ( -11.86176259532119914, 1432.335962297939886, 150.1420601836709920 ) ) ;
#25821 = CARTESIAN_POINT ( 'NONE',  ( 2.906876508539999904, 1508.504005161229998, 236.5181634588980160 ) ) ;
#25822 = CARTESIAN_POINT ( 'NONE',  ( -3.847490228401430734, 1488.832123754849817, 219.3169755907300384 ) ) ;
#25823 = CARTESIAN_POINT ( 'NONE',  ( -4.983160662360000437, 1423.641753194130160, 185.4826375174980058 ) ) ;
#25824 = CARTESIAN_POINT ( 'NONE',  ( -6.569253884907100272, 1446.774627395847801, 154.4165862851036195 ) ) ;
#25825 = CARTESIAN_POINT ( 'NONE',  ( -9.700924147820000343, 1472.526415508389846, 203.7850276454490199 ) ) ;
#25826 = CARTESIAN_POINT ( 'NONE',  ( -9.603402670887449588, 1410.623332638303509, 188.2819919630825041 ) ) ;
#25827 = CARTESIAN_POINT ( 'NONE',  ( -26.01816549270000323, 1379.613343931319832, 211.4995553492590261 ) ) ;
#25828 = CARTESIAN_POINT ( 'NONE',  ( -16.22876982940000090, 1473.844758900830129, 223.1935655822979925 ) ) ;
#25830 = CARTESIAN_POINT ( 'NONE',  ( 3.485764247198380072, 1466.371155763999923, 198.6273673771169967 ) ) ;
#25829 = CARTESIAN_POINT ( 'NONE',  ( -21.66822351760000132, 1505.633081141090088, 209.3276579973889966 ) ) ;
#25831 = CARTESIAN_POINT ( 'NONE',  ( 15.21149316085690018, 1507.619498583100039, 226.3435933218330263 ) ) ;
#25832 = B_SPLINE_CURVE_WITH_KNOTS ( 'NONE', 3,
 ( #5903, #66385, #32203, #108360, #82039, #47904, #12646, #47355, #90441, #4254, #55781, #49024, #99386, #22109, #65273, #98296, #100504, #83160, #6453, #72565, #107805, #81483, #31642 ),
 .UNSPECIFIED., .F., .F.,
 ( 4, 2, 1, 1, 1, 2, 2, 2, 2, 1, 1, 2, 2, 4 ),
 ( 0.000000000000000000, 0.1249999999997535305, 0.1874999999996302402, 0.2187499999995681232, 0.2343749999995374256, 0.2421874999995221045, 0.2499999999995067834, 0.4999999999996687094, 0.6249999999997648548, 0.6874999999998291367, 0.7187499999998765432, 0.7343749999998833156, 0.7499999999998901989, 1.000000000000000000 ),
 .UNSPECIFIED. ) ;
#25833 = AXIS2_PLACEMENT_3D ( 'NONE', #25452, #1962, #36099 ) ;
#25834 = CARTESIAN_POINT ( 'NONE',  ( -7.357910506076572155, 1506.503176757026722, 188.2719473218194821 ) ) ;
#25835 = EDGE_LOOP ( 'NONE', ( #104986, #14217, #11666, #75259 ) ) ;
#25836 = DIRECTION ( 'NONE',  ( 0.8672669759446665072, 0.000000000000000000, 0.4978433412588676998 ) ) ;
#25837 = CARTESIAN_POINT ( 'NONE',  ( 1.514120138310384167, 1516.566819146330090, 216.8317291170628209 ) ) ;
#25838 = CARTESIAN_POINT ( 'NONE',  ( -2.921262571303605782, 1484.943831670156214, 183.1664153039595249 ) ) ;
#25839 = CARTESIAN_POINT ( 'NONE',  ( -20.79738390328697406, 1511.187213306747708, 237.0406858230491025 ) ) ;
#25841 = ORIENTED_EDGE ( 'NONE', *, *, #79276, .F. ) ;
#25840 = CARTESIAN_POINT ( 'NONE',  ( -0.5721718501029199322, 1515.139735159960082, 204.7943596184780120 ) ) ;
#25842 = CARTESIAN_POINT ( 'NONE',  ( -8.156721943249999995, 1384.915541804160057, 199.6468728678090088 ) ) ;
#25843 = DIRECTION ( 'NONE',  ( 0.9858563016923833633, 0.000000000000000000, 0.1675928173085483863 ) ) ;
#25844 = CARTESIAN_POINT ( 'NONE',  ( -11.77148215669999942, 1427.082524922729817, 146.5557703533980032 ) ) ;
#25845 = CARTESIAN_POINT ( 'NONE',  ( -10.82298596616855590, 1424.914553627307214, 144.7927276520015880 ) ) ;
#25846 = CARTESIAN_POINT ( 'NONE',  ( -10.88434851486570132, 1461.922897766000006, 210.7637379796009895 ) ) ;
#25847 = CARTESIAN_POINT ( 'NONE',  ( 14.17716488154820098, 1509.408135427139996, 234.9453616465329731 ) ) ;
#25848 = CARTESIAN_POINT ( 'NONE',  ( -7.467969047550820250, 1425.935834671629891, 203.5501275869820290 ) ) ;
#25849 = CARTESIAN_POINT ( 'NONE',  ( -15.83297151926499602, 1514.812393650459853, 224.4015772493669942 ) ) ;
#25850 = CARTESIAN_POINT ( 'NONE',  ( -2.455820327400000114, 1434.541746329560056, 150.3615916412979914 ) ) ;
#25851 = B_SPLINE_CURVE_WITH_KNOTS ( 'NONE', 5,
 ( #56474, #57037, #13330, #12800, #30703, #89509, #21725, #6058, #82203, #29596, #46980, #5509 ),
 .UNSPECIFIED., .F., .F.,
 ( 6, 3, 3, 6 ),
 ( -7.661770164330000021, -7.525802029310000307, -3.316542704129999741, -3.139241426659999945 ),
 .UNSPECIFIED. ) ;
#25853 = CARTESIAN_POINT ( 'NONE',  ( -10.62969216458879984, 1481.435998155740208, 207.6925002982229955 ) ) ;
#25852 = CARTESIAN_POINT ( 'NONE',  ( -19.22484529489999971, 1470.091603696130051, 227.4635202857980119 ) ) ;
#25854 = DIRECTION ( 'NONE',  ( -0.000000000000000000, -1.000000000000000000, -0.000000000000000000 ) ) ;
#25855 = VERTEX_POINT ( 'NONE', #103857 ) ;
#25856 = CARTESIAN_POINT ( 'NONE',  ( 2.864326087304999824, 1516.826109302209943, 206.6287721023469999 ) ) ;
#25857 = CARTESIAN_POINT ( 'NONE',  ( 23.58347146439999875, 1410.948704344629959, 266.7402917337980170 ) ) ;
#25858 = CARTESIAN_POINT ( 'NONE',  ( 1.497499201727195306, 1455.575695172564792, 218.4485741766675346 ) ) ;
#25859 = CARTESIAN_POINT ( 'NONE',  ( 21.76798767740000073, 1449.724426459390088, 197.1464471020979943 ) ) ;
#25860 = EDGE_CURVE ( 'NONE', #93518, #62097, #25470, .T. ) ;
#25861 = CARTESIAN_POINT ( 'NONE',  ( -0.2962894524850000488, 1508.149850360829987, 237.5387477236979805 ) ) ;
#25862 = CARTESIAN_POINT ( 'NONE',  ( 17.19739463999647100, 1525.960063244516959, 236.2603809477409982 ) ) ;
#25863 = CARTESIAN_POINT ( 'NONE',  ( -40.23240883470000284, 1442.695644260940071, 137.0096571460979646 ) ) ;
#25864 = FACE_OUTER_BOUND ( 'NONE', #33700, .T. ) ;
#25865 = CARTESIAN_POINT ( 'NONE',  ( -16.73160448879999862, 1417.112108414879913, 207.5092061429490116 ) ) ;
#25866 = CARTESIAN_POINT ( 'NONE',  ( -12.91070994500000069, 1445.031679802599911, 186.8505891716980045 ) ) ;
#25867 = EDGE_CURVE ( 'NONE', #58583, #106936, #92916, .T. ) ;
#25868 = CARTESIAN_POINT ( 'NONE',  ( -19.67658020740000069, 1453.313060387329870, 209.1218459620799877 ) ) ;
#25869 = CARTESIAN_POINT ( 'NONE',  ( -17.00277584490474680, 1419.505931447407647, 208.3295775563994710 ) ) ;
#25870 = CARTESIAN_POINT ( 'NONE',  ( -5.405424721240001062, 1496.292287258489750, 218.9823198700590012 ) ) ;
#25871 = ORIENTED_EDGE ( 'NONE', *, *, #91691, .F. ) ;
#25872 = B_SPLINE_CURVE_WITH_KNOTS ( 'NONE', 5,
 ( #76913, #18081, #221, #41648, #86401, #109956 ),
 .UNSPECIFIED., .F., .F.,
 ( 6, 6 ),
 ( 0.000000000000000000, 1.000000000000000000 ),
 .UNSPECIFIED. ) ;
#25873 = CARTESIAN_POINT ( 'NONE',  ( 1.467664789042199880, 1488.639595165949913, 181.9190109959569952 ) ) ;
#25874 = CARTESIAN_POINT ( 'NONE',  ( -13.02339026569499936, 1409.367847196819866, 216.4483738165630200 ) ) ;
#25875 = B_SPLINE_SURFACE_WITH_KNOTS ( 'NONE', 5, 1, ( 
 ( #85219, #15253 ),
 ( #9079, #50544 ),
 ( #58392, #43246 ),
 ( #8511, #24743 ),
 ( #23667, #93610 ),
 ( #49444, #83568 ) ),
 .UNSPECIFIED., .F., .F., .F.,
 ( 6, 6 ),
 ( 2, 2 ),
 ( 0.000000000000000000, 16.34325491069999714 ),
 ( 0.000000000000000000, 14.00000000000000000 ),
 .UNSPECIFIED. ) ;
#25876 = CIRCLE ( 'NONE', #74204, 1.000060826959960236 ) ;
#25877 = CARTESIAN_POINT ( 'NONE',  ( -11.64956323076249944, 1508.434911808069955, 208.7884202097649791 ) ) ;
#25878 = CARTESIAN_POINT ( 'NONE',  ( -15.62861149524349891, 1418.244676918490086, 203.0179538217920197 ) ) ;
#25879 = CARTESIAN_POINT ( 'NONE',  ( -21.85618413279999572, 1471.634021946630128, 266.7712522008980613 ) ) ;
#25880 = CARTESIAN_POINT ( 'NONE',  ( -5.598467674920000192, 1448.782436168089816, 211.2741064300589926 ) ) ;
#25881 = CARTESIAN_POINT ( 'NONE',  ( -12.43458797219282808, 1513.190411469892297, 192.3969053724739808 ) ) ;
#25882 = CARTESIAN_POINT ( 'NONE',  ( 17.85701005936880037, 1417.692377606080072, 223.8866627408119712 ) ) ;
#25883 = CARTESIAN_POINT ( 'NONE',  ( -80.81157604502008951, 1384.636890264109979, 304.3801429775080578 ) ) ;
#25884 = DIRECTION ( 'NONE',  ( -0.7074300732568278294, 0.02470400251969403355, -0.7063514732138287400 ) ) ;
#25885 = CIRCLE ( 'NONE', #7996, 1.000000000000000888 ) ;
#25886 = CARTESIAN_POINT ( 'NONE',  ( -11.91388749740000108, 1435.945967586000052, 151.0354243678980026 ) ) ;
#25887 = B_SPLINE_SURFACE_WITH_KNOTS ( 'NONE', 5, 1, ( 
 ( #98050, #72335 ),
 ( #106465, #62292 ),
 ( #90195, #80161 ),
 ( #105932, #107009 ),
 ( #71249, #29749 ),
 ( #21324, #105372 ),
 ( #12941, #29211 ),
 ( #20785, #47122 ),
 ( #99693, #14596 ) ),
 .UNSPECIFIED., .F., .F., .F.,
 ( 6, 3, 6 ),
 ( 2, 2 ),
 ( 2.977480884639999825, 6.317148707589999468, 12.84597182780000146 ),
 ( -13.57759716840000053, -1.277641461229999997 ),
 .UNSPECIFIED. ) ;
#25888 = CARTESIAN_POINT ( 'NONE',  ( -107.5501839869999969, 1379.272371748259957, 299.1643429852589975 ) ) ;
#25889 = DIRECTION ( 'NONE',  ( 0.000000000000000000, -1.000000000000000000, 6.123233995736769734E-17 ) ) ;
#25890 = CARTESIAN_POINT ( 'NONE',  ( 38.60856580501570079, 1443.613625263020140, 137.1750438873210101 ) ) ;
#25891 = CARTESIAN_POINT ( 'NONE',  ( -23.79341481419999837, 1411.104518318830060, 207.4167121037980053 ) ) ;
#25892 = CARTESIAN_POINT ( 'NONE',  ( 14.27054156580000033, 1415.934222461130048, 196.9549357831980103 ) ) ;
#25893 = CARTESIAN_POINT ( 'NONE',  ( 4.868883885119999810, 1484.326762180689911, 219.4762353022989885 ) ) ;
#25894 = CARTESIAN_POINT ( 'NONE',  ( -23.74108753817469974, 1436.296634041249945, 212.5883363871789982 ) ) ;
#25895 = B_SPLINE_SURFACE_WITH_KNOTS ( 'NONE', 5, 1, ( 
 ( #71101, #98460 ),
 ( #2786, #36906 ),
 ( #11711, #30145 ),
 ( #3341, #89513 ),
 ( #87320, #10615 ),
 ( #36354, #37465 ),
 ( #21174, #104664 ),
 ( #105225, #28512 ),
 ( #71668, #63253 ),
 ( #88959, #12251 ),
 ( #46440, #38018 ),
 ( #72198, #29601 ),
 ( #65442, #66001 ),
 ( #23941, #90610 ),
 ( #56479, #74944 ) ),
 .UNSPECIFIED., .F., .F., .F.,
 ( 6, 3, 3, 3, 6 ),
 ( 2, 2 ),
 ( 62.08793508101459935, 77.35181134419998727, 110.5715862349999981, 131.5832540680000022, 137.5414126590000023 ),
 ( -8.966358544465320387E-05, 4.664442523398899532 ),
 .UNSPECIFIED. ) ;
#25896 = CARTESIAN_POINT ( 'NONE',  ( 22.75273496409596774, 1523.382868172864164, 234.5707981297186109 ) ) ;
#25897 = CARTESIAN_POINT ( 'NONE',  ( 4.862561345523300105, 1435.671581979260054, 228.7561080407950271 ) ) ;
#25898 = CARTESIAN_POINT ( 'NONE',  ( 16.52275697107005570, 1525.042337199239910, 180.9739969239476522 ) ) ;
#25899 = CARTESIAN_POINT ( 'NONE',  ( -11.77904575181089974, 1483.168265960099916, 228.2502168366870023 ) ) ;
#25901 = CARTESIAN_POINT ( 'NONE',  ( -8.875403779870000065, 1384.475744450559887, 199.9572675252190095 ) ) ;
#25900 = CARTESIAN_POINT ( 'NONE',  ( -22.92334060740000368, 1411.083494322230081, 211.1057397514580032 ) ) ;
#25902 = CARTESIAN_POINT ( 'NONE',  ( 11.72965050516489960, 1426.700625785630109, 143.6412421599850120 ) ) ;
#25903 = FACE_OUTER_BOUND ( 'NONE', #94931, .T. ) ;
#25904 = CARTESIAN_POINT ( 'NONE',  ( -10.70370633090000112, 1490.481523645589959, 212.1270248953690043 ) ) ;
#25905 = CARTESIAN_POINT ( 'NONE',  ( 9.283513090479321050, 1450.226982269150085, 204.4123054901219803 ) ) ;
#25906 = DIRECTION ( 'NONE',  ( 0.000000000000000000, 0.000000000000000000, 1.000000000000000000 ) ) ;
#25907 = CARTESIAN_POINT ( 'NONE',  ( -2.294209667535000108, 1516.603620185149794, 203.3509623682169831 ) ) ;
#25908 = CARTESIAN_POINT ( 'NONE',  ( -7.465699360109450566, 1398.134876652174398, 219.7837385695886212 ) ) ;
#25909 = DIRECTION ( 'NONE',  ( 0.000000000000000000, 1.000000000000000000, 0.000000000000000000 ) ) ;
#25910 = FACE_BOUND ( 'NONE', #28542, .T. ) ;
#25911 = CARTESIAN_POINT ( 'NONE',  ( 1.847634001515719993, 1478.089546411300262, 198.8590795898780073 ) ) ;
#25912 = CARTESIAN_POINT ( 'NONE',  ( 5.517763559299710074, 1505.096907884720167, 220.1774585940589759 ) ) ;
#25913 = CARTESIAN_POINT ( 'NONE',  ( 40.70529000807259479, 1444.199214852859996, 137.0833980395239848 ) ) ;
#25915 = VERTEX_POINT ( 'NONE', #74132 ) ;
#25914 = CARTESIAN_POINT ( 'NONE',  ( -60.10696580412420076, 1379.726343179680043, 266.0067701417399917 ) ) ;
#25916 = VERTEX_POINT ( 'NONE', #100947 ) ;
#25917 = CARTESIAN_POINT ( 'NONE',  ( 11.31987186643520005, 1434.499830821800060, 151.5385002157870247 ) ) ;
#25918 = CARTESIAN_POINT ( 'NONE',  ( 21.55808852498703843, 1523.844789899191710, 183.9826104398626967 ) ) ;
#25919 = ORIENTED_EDGE ( 'NONE', *, *, #55366, .F. ) ;
#25920 = CARTESIAN_POINT ( 'NONE',  ( -106.6672824069999876, 1379.424819370810155, 308.2861885763590521 ) ) ;
#25921 = CIRCLE ( 'NONE', #88537, 1.999999999999999556 ) ;
#25922 = CARTESIAN_POINT ( 'NONE',  ( 21.12212911287011963, 1512.187213306747481, 182.4210318429774134 ) ) ;
#25923 = CARTESIAN_POINT ( 'NONE',  ( -7.567240553890000498, 1385.515681772639937, 219.0512273331090114 ) ) ;
#25925 = CARTESIAN_POINT ( 'NONE',  ( 13.84277359751999903, 1452.957910650600070, 224.2058953944790005 ) ) ;
#25924 = CARTESIAN_POINT ( 'NONE',  ( 16.07755494024289789, 1424.336998408409954, 191.1005968644109885 ) ) ;
#25926 = CARTESIAN_POINT ( 'NONE',  ( 15.93081432798890162, 1498.109692542990160, 231.2852987234049920 ) ) ;
#25927 = CARTESIAN_POINT ( 'NONE',  ( 4.709678610000000099, 1507.637404285230105, 181.8385339875979980 ) ) ;
#25928 = CARTESIAN_POINT ( 'NONE',  ( 3.266173989019999890, 1467.802313959489993, 218.5517745389790036 ) ) ;
#25929 = CARTESIAN_POINT ( 'NONE',  ( -32.86802468386279941, 1523.382868172864164, 217.2040256693919957 ) ) ;
#25930 = CARTESIAN_POINT ( 'NONE',  ( -2.864972154145000172, 1516.859514182039902, 212.0024388992169975 ) ) ;
#25931 = CARTESIAN_POINT ( 'NONE',  ( 3.512785867830420180E-12, 1395.913060387330006, 198.1220674046479928 ) ) ;
#25933 = CONICAL_SURFACE ( 'NONE', #63553, 7.999999999999996447, 0.02617993877989872875 ) ;
#25932 = CARTESIAN_POINT ( 'NONE',  ( 14.14453214075280130, 1415.673583083940002, 197.1727595455269864 ) ) ;
#25934 = CARTESIAN_POINT ( 'NONE',  ( 11.85636366039999956, 1431.657450769009984, 149.9409103546979907 ) ) ;
#25935 = CARTESIAN_POINT ( 'NONE',  ( 7.381112317704999981, 1512.341575225269935, 202.3461611114969969 ) ) ;
#25936 = ORIENTED_EDGE ( 'NONE', *, *, #18144, .T. ) ;
#25937 = CARTESIAN_POINT ( 'NONE',  ( 14.11983163027539945, 1435.196066153720039, 149.2983271376729988 ) ) ;
#25938 = ORIENTED_EDGE ( 'NONE', *, *, #2794, .T. ) ;
#25939 = ORIENTED_EDGE ( 'NONE', *, *, #95346, .F. ) ;
#25940 = CARTESIAN_POINT ( 'NONE',  ( -19.64047668580450079, 1507.861171522700261, 229.4570402217679828 ) ) ;
#25941 = CARTESIAN_POINT ( 'NONE',  ( 16.43125155181079933, 1512.939392325030667, 197.4646673575076363 ) ) ;
#25942 = CARTESIAN_POINT ( 'NONE',  ( -11.46285746319973953, 1503.757028837903590, 207.6153346572946532 ) ) ;
#25943 = DIRECTION ( 'NONE',  ( 1.000000000000000000, -3.196303315166338322E-31, 4.657260248767550292E-10 ) ) ;
#25944 = CARTESIAN_POINT ( 'NONE',  ( -8.152189559000989405, 1511.505225070767210, 212.9862058279672681 ) ) ;
#25945 = B_SPLINE_CURVE_WITH_KNOTS ( 'NONE', 3,
 ( #110175, #17736, #41327, #448, #67648, #60341, #34569, #42984, #76574, #8803, #100658, #23942, #66554, #34016, #58686, #77143, #59792, #101756, #68754 ),
 .UNSPECIFIED., .F., .F.,
 ( 4, 2, 2, 2, 1, 1, 1, 2, 2, 2, 4 ),
 ( 0.000000000000000000, 0.2499999999971138087, 0.3749999999957732699, 0.4374999999950133778, 0.4687499999947145057, 0.4843749999945661799, 0.4921874999944930718, 0.4960937499945325957, 0.4999999999945721196, 0.7499999999972859488, 1.000000000000000000 ),
 .UNSPECIFIED. ) ;
#25946 = CARTESIAN_POINT ( 'NONE',  ( -108.0661742336610018, 1378.913060387289988, 308.5496305239910271 ) ) ;
#25947 = CARTESIAN_POINT ( 'NONE',  ( -35.68096903199556635, 1379.642192106147149, 218.6344609364291500 ) ) ;
#25948 = CARTESIAN_POINT ( 'NONE',  ( -7.630907732839999902, 1377.866160257680122, 206.3143087701089939 ) ) ;
#25949 = VERTEX_POINT ( 'NONE', #108815 ) ;
#25950 = CARTESIAN_POINT ( 'NONE',  ( 3.251888829344999898, 1516.793978928989873, 206.6294022811970024 ) ) ;
#25951 = ORIENTED_EDGE ( 'NONE', *, *, #73390, .T. ) ;
#25952 = CARTESIAN_POINT ( 'NONE',  ( 22.43577763531170177, 1440.913060387330006, 229.3504540723680236 ) ) ;
#25953 = CARTESIAN_POINT ( 'NONE',  ( -18.87155817529999879, 1509.015965077730016, 230.2334335948979742 ) ) ;
#25954 = ORIENTED_EDGE ( 'NONE', *, *, #77734, .F. ) ;
#25955 = CARTESIAN_POINT ( 'NONE',  ( -11.36373753890000060, 1409.476796350030099, 189.5641612269979817 ) ) ;
#25956 = CARTESIAN_POINT ( 'NONE',  ( 7.641777858334999785, 1513.965983108860200, 215.0411262584869974 ) ) ;
#25958 = ORIENTED_EDGE ( 'NONE', *, *, #92623, .T. ) ;
#25957 = CARTESIAN_POINT ( 'NONE',  ( -11.00355868719999997, 1414.913528139930122, 195.9181521845980001 ) ) ;
#25959 = CARTESIAN_POINT ( 'NONE',  ( 22.86920506520000274, 1432.244263168689940, 216.4472202372080005 ) ) ;
#25960 = CARTESIAN_POINT ( 'NONE',  ( -15.28723455579760149, 1508.551704408389924, 210.3672327514449876 ) ) ;
#25961 = CARTESIAN_POINT ( 'NONE',  ( -5.062212390315069754, 1474.342205398819942, 198.8731691453010058 ) ) ;
#25962 = CARTESIAN_POINT ( 'NONE',  ( 5.385523159618170297, 1511.435001054559962, 217.7746220610370074 ) ) ;
#25963 = DIRECTION ( 'NONE',  ( 1.755985294532469921E-16, -1.000000000000000000, 1.338183447452831989E-16 ) ) ;
#25964 = CARTESIAN_POINT ( 'NONE',  ( -2.869693497065000098, 1517.070197312179971, 214.9093229647470196 ) ) ;
#25965 = CARTESIAN_POINT ( 'NONE',  ( 24.07913224159999999, 1410.980207832730002, 209.6302583906470147 ) ) ;
#25966 = CARTESIAN_POINT ( 'NONE',  ( -11.14671771210699980, 1434.019356486030119, 151.6529807626459956 ) ) ;
#25967 = CARTESIAN_POINT ( 'NONE',  ( 22.07680818022633318, 1523.847248782568613, 184.4451128950378518 ) ) ;
#25968 = CARTESIAN_POINT ( 'NONE',  ( 3.462948796544999652, 1516.956048353049937, 211.4063724288770061 ) ) ;
#25969 = B_SPLINE_CURVE_WITH_KNOTS ( 'NONE', 3,
 ( #70169, #87491, #28116, #96435 ),
 .UNSPECIFIED., .F., .F.,
 ( 4, 4 ),
 ( -23.36254398669999688, -0.7259150538130008101 ),
 .UNSPECIFIED. ) ;
#25970 = CARTESIAN_POINT ( 'NONE',  ( -11.86894174216629949, 1482.050028868399977, 208.4783409248709916 ) ) ;
#25971 = CARTESIAN_POINT ( 'NONE',  ( 30.30249668296529464, 1524.678872986498618, 221.8071382193505201 ) ) ;
#25973 = EDGE_LOOP ( 'NONE', ( #93036, #74971, #17969 ) ) ;
#25972 = CARTESIAN_POINT ( 'NONE',  ( -96.24084593199999915, 1384.955172021569979, 310.5859090792589541 ) ) ;
#25975 = B_SPLINE_CURVE_WITH_KNOTS ( 'NONE', 5,
 ( #26906, #87367, #61628, #85693, #614, #44270 ),
 .UNSPECIFIED., .F., .F.,
 ( 6, 6 ),
 ( -22.60166147410000193, -9.285377787159999841 ),
 .UNSPECIFIED. ) ;
#25974 = CARTESIAN_POINT ( 'NONE',  ( -57.60619611540929697, 1385.078379728229947, 276.7333735769680061 ) ) ;
#25976 = CARTESIAN_POINT ( 'NONE',  ( 35.51629366599999571, 1458.123799197230028, 261.8361074970979416 ) ) ;
#25977 = CARTESIAN_POINT ( 'NONE',  ( 1.533207931480909281, 1452.703037475436531, 183.4902445653410155 ) ) ;
#25978 = CARTESIAN_POINT ( 'NONE',  ( -7.552141952424999971, 1510.542924508009946, 212.9021323590669965 ) ) ;
#25979 = CARTESIAN_POINT ( 'NONE',  ( -6.854598081119999797, 1507.853711066930146, 235.7978674939980124 ) ) ;
#25980 = CARTESIAN_POINT ( 'NONE',  ( 12.45033887509999992, 1421.619541826690238, 207.5029467985389999 ) ) ;
#25982 = CARTESIAN_POINT ( 'NONE',  ( 19.09048981950000012, 1456.312469618329942, 226.2254625276979709 ) ) ;
#25981 = DIRECTION ( 'NONE',  ( 1.000000000000000000, 0.000000000000000000, 0.000000000000000000 ) ) ;
#25983 = CARTESIAN_POINT ( 'NONE',  ( -9.172189383897210391, 1449.366367657520186, 209.4775503665190115 ) ) ;
#25984 = CARTESIAN_POINT ( 'NONE',  ( -109.5250186310779981, 1383.241630048620209, 311.1713175981399786 ) ) ;
#25985 = ORIENTED_EDGE ( 'NONE', *, *, #93387, .T. ) ;
#25986 = CARTESIAN_POINT ( 'NONE',  ( 7.712490952985000980, 1516.666407245520077, 204.5049844236870058 ) ) ;
#25987 = CARTESIAN_POINT ( 'NONE',  ( 0.3382504354559999760, 1405.989871386730101, 266.9611136494980315 ) ) ;
#25988 = CARTESIAN_POINT ( 'NONE',  ( 29.30029655192942073, 1525.907212628473644, 196.8717316207784620 ) ) ;
#25989 = CIRCLE ( 'NONE', #13439, 30.10786454236638576 ) ;
#25990 = CARTESIAN_POINT ( 'NONE',  ( 12.89348889060000047, 1425.726071551529913, 223.5999069075979833 ) ) ;
#25991 = CARTESIAN_POINT ( 'NONE',  ( -1.556370157619999972, 1414.996444526030018, 226.5294865527980051 ) ) ;
#25992 = CARTESIAN_POINT ( 'NONE',  ( 3.461590032740000211, 1467.254004089789987, 218.5936129320489840 ) ) ;
#25993 = CARTESIAN_POINT ( 'NONE',  ( -1.221263722386547901, 1469.682530730686949, 219.1105054375227894 ) ) ;
#25994 = CARTESIAN_POINT ( 'NONE',  ( 28.38546418346980005, 1435.488905026550128, 135.6743912052290000 ) ) ;
#25995 = CARTESIAN_POINT ( 'NONE',  ( -26.02650053749999870, 1446.299505181590121, 138.3420241739979986 ) ) ;
#25996 = CARTESIAN_POINT ( 'NONE',  ( -45.63712966311000230, 1440.913059426480004, 268.9747523979869470 ) ) ;
#25997 = CARTESIAN_POINT ( 'NONE',  ( -1.749097280350000005, 1429.787493520590033, 200.2727799645290077 ) ) ;
#25998 = EDGE_CURVE ( 'NONE', #48821, #105177, #56477, .T. ) ;
#25999 = DIRECTION ( 'NONE',  ( -0.9510565162951566398, 0.000000000000000000, -0.3090169943749382919 ) ) ;
#26000 = DIRECTION ( 'NONE',  ( 0.7414773880254711402, 0.000000000000000000, 0.6709778558543678662 ) ) ;
#26001 = CIRCLE ( 'NONE', #29615, 1.000000000000000444 ) ;
#26002 = CARTESIAN_POINT ( 'NONE',  ( -9.103468112560660686, 1449.499701819690017, 210.3008494512589834 ) ) ;
#26003 = ORIENTED_EDGE ( 'NONE', *, *, #5288, .F. ) ;
#26004 = CARTESIAN_POINT ( 'NONE',  ( 19.54391504031716664, 1526.306647125542895, 185.2858915736553911 ) ) ;
#26005 = CARTESIAN_POINT ( 'NONE',  ( 2.500000001190000098, 1425.952486856224823, 183.8951078798580454 ) ) ;
#26006 = CARTESIAN_POINT ( 'NONE',  ( -21.84020450222019250, 1512.187213306747481, 234.9798068779743403 ) ) ;
#26007 = CARTESIAN_POINT ( 'NONE',  ( 16.93884299705920071, 1507.634939766059915, 188.0954313100240256 ) ) ;
#26008 = CARTESIAN_POINT ( 'NONE',  ( -0.5319847658459999629, 1417.295974482030033, 234.8116028735980194 ) ) ;
#26010 = CARTESIAN_POINT ( 'NONE',  ( -14.61611649526098589, 1469.120177286887611, 195.1467201088773606 ) ) ;
#26009 = CARTESIAN_POINT ( 'NONE',  ( 12.24365544940000028, 1500.600793972790143, 208.6479367508759992 ) ) ;
#26011 = CARTESIAN_POINT ( 'NONE',  ( 19.36248556598933845, 1455.763297351556048, 225.9778007399211788 ) ) ;
#26012 = B_SPLINE_SURFACE_WITH_KNOTS ( 'NONE', 5, 5, ( 
 ( #56625, #90760, #48231, #30301, #98055, #65584 ),
 ( #64493, #90198, #108108, #47672, #82372, #76039 ),
 ( #110184, #33455, #89113, #38701, #81800, #107565 ),
 ( #5671, #38158, #46587, #14600, #107013, #73978 ),
 ( #99696, #22988, #84435, #12402, #80722, #4030 ),
 ( #72339, #102323, #87197, #26164, #101765, #60350 ),
 ( #77693, #103989, #61468, #10489, #59801, #93921 ),
 ( #9930, #94473, #34579, #16641, #26730, #50837 ),
 ( #18863, #17746, #85516, #25054, #78238, #34026 ),
 ( #77153, #68218, #17188, #68763, #102867, #53060 ),
 ( #42995, #27286, #59257, #95047, #44660, #1005 ),
 ( #8262, #35683, #44100, #51384, #42426, #78801 ) ),
 .UNSPECIFIED., .F., .F., .F.,
 ( 6, 3, 3, 6 ),
 ( 6, 6 ),
 ( -3.831645261493030061E-05, 4.695069562340000502, 9.390139124690000116, 12.39571065745260015 ),
 ( 0.000000000000000000, 2.000038316452609877 ),
 .UNSPECIFIED. ) ;
#26013 = CARTESIAN_POINT ( 'NONE',  ( 8.239069889199999608, 1423.385677187009833, 212.2461209534189948 ) ) ;
#26014 = CARTESIAN_POINT ( 'NONE',  ( -11.28131443171900017, 1384.886896985610065, 218.8719869723099976 ) ) ;
#26015 = CARTESIAN_POINT ( 'NONE',  ( 42.06228640162340326, 1440.913015538450054, 269.6487197970989769 ) ) ;
#26016 = CARTESIAN_POINT ( 'NONE',  ( -12.97408886687033558, 1451.220703713921466, 150.9179168472272750 ) ) ;
#26017 = CARTESIAN_POINT ( 'NONE',  ( -6.588204561759999578, 1484.019114425890166, 200.1196401685189983 ) ) ;
#26018 = CARTESIAN_POINT ( 'NONE',  ( 25.95593065371449981, 1435.599270252459974, 136.1659943809549986 ) ) ;
#26019 = CARTESIAN_POINT ( 'NONE',  ( -8.759831409813630287, 1396.218960441809713, 202.3723544762349889 ) ) ;
#26020 = ORIENTED_EDGE ( 'NONE', *, *, #88002, .T. ) ;
#26021 = B_SPLINE_CURVE_WITH_KNOTS ( 'NONE', 5,
 ( #90015, #55342, #22238, #107373, #20057, #54251 ),
 .UNSPECIFIED., .F., .F.,
 ( 6, 6 ),
 ( 0.000000000000000000, 1.000000000000000000 ),
 .UNSPECIFIED. ) ;
#26022 = CARTESIAN_POINT ( 'NONE',  ( 30.31643683089982844, 1523.530935881284904, 195.7504610701754189 ) ) ;
#26023 = CARTESIAN_POINT ( 'NONE',  ( 11.94046459599999999, 1438.194204504490017, 147.6340003373980210 ) ) ;
#26024 = VERTEX_POINT ( 'NONE', #32110 ) ;
#26025 = ORIENTED_EDGE ( 'NONE', *, *, #80964, .T. ) ;
#26026 = CYLINDRICAL_SURFACE ( 'NONE', #5183, 0.9999999999999906741 ) ;
#26027 = CARTESIAN_POINT ( 'NONE',  ( 6.929954890342334473, 1516.587827493819759, 206.2351373589867762 ) ) ;
#26029 = CARTESIAN_POINT ( 'NONE',  ( -9.927759914837499977, 1438.851595397029996, 209.8644134391970226 ) ) ;
#26028 = CARTESIAN_POINT ( 'NONE',  ( 11.08126927090000002, 1426.907418872530116, 96.53620495169779758 ) ) ;
#26030 = CARTESIAN_POINT ( 'NONE',  ( 23.13309424899999911, 1409.720885835030003, 209.3985505581069901 ) ) ;
#26031 = CARTESIAN_POINT ( 'NONE',  ( -11.85917953740000108, 1433.048083576320096, 150.2760150462979993 ) ) ;
#26032 = ADVANCED_FACE ( 'NONE', ( #31549 ), #69030, .T. ) ;
#26033 = CARTESIAN_POINT ( 'NONE',  ( -2.512979519748912871, 1421.005010328889739, 185.2548484884229367 ) ) ;
#26034 = CARTESIAN_POINT ( 'NONE',  ( 6.908704138140000062, 1424.414520317140159, 213.3241070330990112 ) ) ;
#26035 = B_SPLINE_CURVE_WITH_KNOTS ( 'NONE', 3,
 ( #76261, #10155, #25831, #60032, #17421, #18533, #51619, #85755, #9051, #103667, #43224, #26965 ),
 .UNSPECIFIED., .F., .F.,
 ( 4, 2, 2, 2, 2, 4 ),
 ( -0.1123552072008140029, -0.09789080009285709705, -0.08345977780132710078, -0.05408602703201970119, -0.02844234071178690371, 0.000000000000000000 ),
 .UNSPECIFIED. ) ;
#26036 = CARTESIAN_POINT ( 'NONE',  ( -17.51440555739999994, 1442.103933559090137, 219.2287671671990097 ) ) ;
#26037 = CARTESIAN_POINT ( 'NONE',  ( 8.247663932760000094, 1509.138309195029933, 181.6038655551980128 ) ) ;
#26038 = CARTESIAN_POINT ( 'NONE',  ( 2.479936572040000176, 1449.203345246219897, 182.3137392801979786 ) ) ;
#26039 = CARTESIAN_POINT ( 'NONE',  ( 8.963248341601568470, 1364.599977456154647, 207.6218459616988241 ) ) ;
#26041 = VERTEX_POINT ( 'NONE', #2955 ) ;
#26040 = DIRECTION ( 'NONE',  ( 0.9510565162951518658, 0.000000000000000000, -0.3090169943749528914 ) ) ;
#26042 = ORIENTED_EDGE ( 'NONE', *, *, #48835, .F. ) ;
#26043 = FACE_OUTER_BOUND ( 'NONE', #17617, .T. ) ;
#26044 = AXIS2_PLACEMENT_3D ( 'NONE', #33838, #67471, #101576 ) ;
#26045 = CARTESIAN_POINT ( 'NONE',  ( 7.501250477999354516, 1510.704533481359476, 203.0986210076053169 ) ) ;
#26046 = CARTESIAN_POINT ( 'NONE',  ( -1.476727087160000007, 1474.160226259529963, 270.1373298219979802 ) ) ;
#26047 = CARTESIAN_POINT ( 'NONE',  ( 17.17241001986483795, 1512.187213306747481, 181.6185504016043240 ) ) ;
#26048 = CARTESIAN_POINT ( 'NONE',  ( -107.4576978852700648, 1306.483669372788427, 307.4681403979344623 ) ) ;
#26049 = CARTESIAN_POINT ( 'NONE',  ( -32.18358323225091766, 1524.059547553519224, 201.4963293957178792 ) ) ;
#26050 = CARTESIAN_POINT ( 'NONE',  ( 1.355095489612469839, 1476.075987768590039, 197.7236685275530021 ) ) ;
#26051 = CARTESIAN_POINT ( 'NONE',  ( -21.41971086555067316, 1512.187213306747481, 233.0798096144383749 ) ) ;
#26052 = B_SPLINE_SURFACE_WITH_KNOTS ( 'NONE', 5, 5, ( 
 ( #90053, #3889, #99002, #39097, #13892, #63255, #64895, #30148, #64339 ),
 ( #106321, #37467, #82211, #88962, #98462, #12806, #30709, #72731, #107413 ),
 ( #3343, #89515, #22279, #56481, #63789, #73839, #13336, #97363, #20635 ),
 ( #47528, #38020, #54838, #4427, #73275, #5516, #12253, #21731, #46986 ),
 ( #55934, #90612, #31263, #71670, #81110, #39671, #107966, #21175, #65445 ),
 ( #46442, #80574, #55383, #81649, #38553, #4954, #99555, #22839, #88423 ) ),
 .UNSPECIFIED., .F., .F., .F.,
 ( 6, 6 ),
 ( 6, 3, 6 ),
 ( 32.35314871179999585, 33.17903199610000087 ),
 ( 0.000000000000000000, 1.000000000000000000, 2.000000000000000000 ),
 .UNSPECIFIED. ) ;
#26053 = CARTESIAN_POINT ( 'NONE',  ( -22.68012700156480221, 1507.275789587069767, 208.4743628061380036 ) ) ;
#26054 = CARTESIAN_POINT ( 'NONE',  ( 8.795499755375784545, 1368.316259268678550, 207.6218459616987673 ) ) ;
#26055 = CARTESIAN_POINT ( 'NONE',  ( 3.320336327120199993, 1408.845769750169893, 195.0433881623220032 ) ) ;
#26056 = CARTESIAN_POINT ( 'NONE',  ( -18.52619959329609856, 1409.651470360259964, 269.5393490716199949 ) ) ;
#26057 = CARTESIAN_POINT ( 'NONE',  ( -17.71193100849139768, 1519.551704408389924, 221.5709757781449980 ) ) ;
#26058 = ORIENTED_EDGE ( 'NONE', *, *, #53028, .F. ) ;
#26059 = CARTESIAN_POINT ( 'NONE',  ( -11.86561511689999904, 1432.302094693870004, 149.9824189743979730 ) ) ;
#26060 = CARTESIAN_POINT ( 'NONE',  ( 13.48763800459999906, 1443.604195705930124, 188.0280588922980201 ) ) ;
#26061 = ORIENTED_EDGE ( 'NONE', *, *, #62287, .F. ) ;
#26062 = VERTEX_POINT ( 'NONE', #37626 ) ;
#26063 = CARTESIAN_POINT ( 'NONE',  ( -22.06852505282392229, 1506.535970898746427, 209.1479492043462187 ) ) ;
#26064 = CARTESIAN_POINT ( 'NONE',  ( 5.703720466386680066, 1424.346729877480129, 193.4758770404599773 ) ) ;
#26065 = CARTESIAN_POINT ( 'NONE',  ( 5.784008635194999748, 1516.911981270829983, 214.1231845985469988 ) ) ;
#26066 = CARTESIAN_POINT ( 'NONE',  ( -2.901842622390000237, 1485.480021844630073, 183.2625817364980207 ) ) ;
#26067 = VERTEX_POINT ( 'NONE', #96437 ) ;
#26068 = EDGE_CURVE ( 'NONE', #75258, #93813, #12958, .T. ) ;
#26069 = DIRECTION ( 'NONE',  ( -0.9455185755993178454, 0.000000000000000000, 0.3255681544571537578 ) ) ;
#26071 = EDGE_CURVE ( 'NONE', #25680, #10167, #79651, .T. ) ;
#26070 = CIRCLE ( 'NONE', #110102, 1.999999954393710588 ) ;
#26072 = EDGE_CURVE ( 'NONE', #63587, #97374, #96997, .T. ) ;
#26073 = EDGE_CURVE ( 'NONE', #70574, #96461, #2123, .T. ) ;
#26074 = DIRECTION ( 'NONE',  ( 0.000000000000000000, -0.8286769424886414326, -0.5597271880011518430 ) ) ;
#26075 = CARTESIAN_POINT ( 'NONE',  ( -1.712644754285000070, 1516.636036526019780, 204.1262224792070015 ) ) ;
#26076 = CARTESIAN_POINT ( 'NONE',  ( -27.78811175689999757, 1509.876756555029942, 201.6112073881680260 ) ) ;
#26077 = EDGE_CURVE ( 'NONE', #15423, #2577, #108344, .T. ) ;
#26078 = CARTESIAN_POINT ( 'NONE',  ( 5.508554876272072853, 1427.333971811663332, 134.0999999980980135 ) ) ;
#26080 = EDGE_CURVE ( 'NONE', #18078, #8168, #44014, .T. ) ;
#26079 = CARTESIAN_POINT ( 'NONE',  ( -73.12095152039999846, 1385.004348552520014, 272.3390795393589769 ) ) ;
#26082 = VECTOR ( 'NONE', #36455, 1000.000000000000114 ) ;
#26081 = CARTESIAN_POINT ( 'NONE',  ( -38.53560686260429691, 1384.578460514909921, 211.5649073465099832 ) ) ;
#26083 = CARTESIAN_POINT ( 'NONE',  ( -13.72624666517843472, 1517.051704408389924, 195.8110037935180969 ) ) ;
#26084 = CARTESIAN_POINT ( 'NONE',  ( -5.316196955749759923, 1519.551704408389924, 231.0177287530028423 ) ) ;
#26086 = ORIENTED_EDGE ( 'NONE', *, *, #31790, .F. ) ;
#26085 = CARTESIAN_POINT ( 'NONE',  ( -7.386732042270000242, 1447.816120179589916, 185.7874553686979766 ) ) ;
#26087 = CARTESIAN_POINT ( 'NONE',  ( 8.788316489185000080, 1511.741868877540128, 202.8695794779170001 ) ) ;
#26088 = CARTESIAN_POINT ( 'NONE',  ( 27.49404549280000154, 1488.693617962429926, 208.9387129124660021 ) ) ;
#26089 = EDGE_CURVE ( 'NONE', #24504, #18900, #94179, .T. ) ;
#26090 = CARTESIAN_POINT ( 'NONE',  ( 19.69912643434309985, 1477.269676134359997, 225.7986965500050189 ) ) ;
#26091 = CARTESIAN_POINT ( 'NONE',  ( -25.83444865290000081, 1435.692496567170110, 136.3622603797980162 ) ) ;
#26092 = CARTESIAN_POINT ( 'NONE',  ( -0.7353365779029981120, 1516.995911393979895, 212.0011643880069698 ) ) ;
#26093 = CARTESIAN_POINT ( 'NONE',  ( -68.70867971649998651, 1379.747832788930054, 279.9818316718590268 ) ) ;
#26094 = CARTESIAN_POINT ( 'NONE',  ( -15.12936268429999842, 1413.157696382230142, 226.7979570398979945 ) ) ;
#26095 = CARTESIAN_POINT ( 'NONE',  ( -11.71533056565333553, 1414.421228241719973, 208.3857400952160788 ) ) ;
#26096 = CARTESIAN_POINT ( 'NONE',  ( 7.713648834184999359, 1516.710624944440042, 208.3691743819339877 ) ) ;
#26097 = VERTEX_POINT ( 'NONE', #70720 ) ;
#26098 = FACE_BOUND ( 'NONE', #33963, .T. ) ;
#26100 = EDGE_CURVE ( 'NONE', #108726, #31217, #79753, .T. ) ;
#26099 = CARTESIAN_POINT ( 'NONE',  ( -3.619881192149999816, 1412.838016826329977, 232.4469606129980264 ) ) ;
#26101 = CARTESIAN_POINT ( 'NONE',  ( -17.46966162369999864, 1385.147636303250010, 219.9515191535590191 ) ) ;
#26102 = EDGE_LOOP ( 'NONE', ( #92320, #32591, #8411, #95647 ) ) ;
#26103 = CARTESIAN_POINT ( 'NONE',  ( -12.47378745274919964, 1385.303368465689800, 218.9863576209239966 ) ) ;
#26104 = CARTESIAN_POINT ( 'NONE',  ( -9.415828895194328751, 1493.189318859109790, 201.2122058663049700 ) ) ;
#26105 = CARTESIAN_POINT ( 'NONE',  ( 12.52472169154620119, 1435.436724083190029, 150.8432062471219979 ) ) ;
#26106 = CARTESIAN_POINT ( 'NONE',  ( -4.118451982573078318, 1441.437192870819899, 184.2612739964320099 ) ) ;
#26107 = EDGE_CURVE ( 'NONE', #109511, #40850, #74151, .T. ) ;
#26108 = CARTESIAN_POINT ( 'NONE',  ( -23.32961689541300032, 1509.451491745719977, 225.2641564516229948 ) ) ;
#26109 = DIRECTION ( 'NONE',  ( -0.6038592750913972518, 0.7071067811868648745, 0.3679048462383220919 ) ) ;
#26110 = EDGE_CURVE ( 'NONE', #36972, #12048, #61863, .T. ) ;
#26111 = CARTESIAN_POINT ( 'NONE',  ( -20.01067139950000140, 1507.877425041529932, 188.9709217985979706 ) ) ;
#26112 = CARTESIAN_POINT ( 'NONE',  ( 12.42529224677513078, 1522.051704408389924, 202.6823640254548309 ) ) ;
#26114 = CARTESIAN_POINT ( 'NONE',  ( 6.824596708572589598, 1424.815923006090998, 213.4892281219103154 ) ) ;
#26113 = CARTESIAN_POINT ( 'NONE',  ( 2.489617538345000103, 1516.665179208830068, 214.1178407578070164 ) ) ;
#26115 = CARTESIAN_POINT ( 'NONE',  ( 19.60066840860000070, 1508.321169339229982, 188.7280170016979923 ) ) ;
#26116 = CARTESIAN_POINT ( 'NONE',  ( -2.872836660654999985, 1517.158319634930194, 216.8472181024670249 ) ) ;
#26117 = VERTEX_POINT ( 'NONE', #44952 ) ;
#26118 = CARTESIAN_POINT ( 'NONE',  ( 7.722580314247720068, 1517.051704408590012, 209.5565402419049974 ) ) ;
#26119 = CARTESIAN_POINT ( 'NONE',  ( -17.12870856829999866, 1420.279571949720093, 203.5620527584690080 ) ) ;
#26120 = ORIENTED_EDGE ( 'NONE', *, *, #109746, .T. ) ;
#26121 = ADVANCED_FACE ( 'NONE', ( #79099 ), #75214, .T. ) ;
#26122 = CARTESIAN_POINT ( 'NONE',  ( -8.775825618903718706, 1379.913060387289988, 204.3275905756569841 ) ) ;
#26123 = PRODUCT_DEFINITION_FORMATION_WITH_SPECIFIED_SOURCE ( 'ANY', '', #82225, .NOT_KNOWN. ) ;
#26124 = FACE_OUTER_BOUND ( 'NONE', #58480, .T. ) ;
#26125 = CARTESIAN_POINT ( 'NONE',  ( 2.596261494520262225, 1525.907212628473644, 177.4701144822247727 ) ) ;
#26126 = CARTESIAN_POINT ( 'NONE',  ( 2.901843670269999897, 1442.289985319589960, 217.6299988927789855 ) ) ;
#26127 = FACE_OUTER_BOUND ( 'NONE', #25732, .T. ) ;
#26128 = CARTESIAN_POINT ( 'NONE',  ( -762.4595027414246715, -8387.357407334298841, -1619.876006850564636 ) ) ;
#26129 = CARTESIAN_POINT ( 'NONE',  ( 17.80652095830000192, 1415.128105756529976, 210.3714338108779884 ) ) ;
#26130 = CARTESIAN_POINT ( 'NONE',  ( 11.21247613359999917, 1490.926120241489798, 206.9376360906590264 ) ) ;
#26131 = FACE_OUTER_BOUND ( 'NONE', #66, .T. ) ;
#26132 = DIRECTION ( 'NONE',  ( 0.9125304618753908859, 0.000000000000000000, -0.4090087482554448095 ) ) ;
#26133 = CARTESIAN_POINT ( 'NONE',  ( 38.11840859848789620, 1440.913060382519916, 256.4711611452369766 ) ) ;
#26135 = CARTESIAN_POINT ( 'NONE',  ( -5.034319209093887082, 1391.795857067797897, 203.5666908100943715 ) ) ;
#26134 = CARTESIAN_POINT ( 'NONE',  ( -14.06060368556070017, 1417.615943288039944, 202.3868150088759990 ) ) ;
#26136 = CARTESIAN_POINT ( 'NONE',  ( 7.260305599174779800, 1509.032998980356297, 202.6015522927725669 ) ) ;
#26137 = ORIENTED_EDGE ( 'NONE', *, *, #53997, .F. ) ;
#26138 = CARTESIAN_POINT ( 'NONE',  ( 1.552591573816870074, 1415.651572961190141, 190.6893068747150153 ) ) ;
#26139 = CARTESIAN_POINT ( 'NONE',  ( -4.678144232538111069, 1508.611354625609920, 211.6097690136730023 ) ) ;
#26140 = CARTESIAN_POINT ( 'NONE',  ( -27.96976564920000285, 1509.201555287429983, 210.6640595776979978 ) ) ;
#26141 = CARTESIAN_POINT ( 'NONE',  ( 2.449123001110840470, 1410.376692143526043, 185.5607414632172834 ) ) ;
#26142 = CARTESIAN_POINT ( 'NONE',  ( -10.41319835519830050, 1479.501835575390032, 210.3840731168270111 ) ) ;
#26143 = FACE_OUTER_BOUND ( 'NONE', #92293, .T. ) ;
#26144 = CARTESIAN_POINT ( 'NONE',  ( -14.44411435775000108, 1509.548839476979992, 182.8006741103589832 ) ) ;
#26145 = EDGE_CURVE ( 'NONE', #93372, #109266, #88840, .T. ) ;
#26147 =( GEOMETRIC_REPRESENTATION_CONTEXT ( 3 ) GLOBAL_UNCERTAINTY_ASSIGNED_CONTEXT ( ( #26688 ) ) GLOBAL_UNIT_ASSIGNED_CONTEXT ( ( #110698, #26686, #1513 ) ) REPRESENTATION_CONTEXT ( 'NONE', 'WORKASPACE' ) );
#26146 = CARTESIAN_POINT ( 'NONE',  ( -4.634289585198445138, 1377.926009802909448, 204.1816958463118112 ) ) ;
#26148 = B_SPLINE_CURVE_WITH_KNOTS ( 'NONE', 5,
 ( #51924, #51356, #9362, #68738, #44075, #36219, #69848, #78213, #53036, #8789, #68195, #102842 ),
 .UNSPECIFIED., .F., .F.,
 ( 6, 3, 3, 6 ),
 ( 0.000000000000000000, 0.2753503963466049087, 0.7584501321178948041, 1.000000000000000000 ),
 .UNSPECIFIED. ) ;
#26149 = CARTESIAN_POINT ( 'NONE',  ( 11.69992624430000028, 1435.514532378290141, 225.6365414701989778 ) ) ;
#26150 = VECTOR ( 'NONE', #4967, 1000.000000000000114 ) ;
#26151 = CARTESIAN_POINT ( 'NONE',  ( -70.29742853679998404, 1383.784953440819891, 295.1360135794139978 ) ) ;
#26152 = CARTESIAN_POINT ( 'NONE',  ( 15.70760032500000136, 1452.364538897129933, 147.9013275455980079 ) ) ;
#26153 = ADVANCED_FACE ( 'NONE', ( #27855 ), #43995, .F. ) ;
#26155 =( BOUNDED_SURFACE ( )  B_SPLINE_SURFACE ( 1, 2, ( 
 ( #87888, #18981, #88960, #71102, #2243, #105226, #28513, #61583, #10616 ),
 ( #79480, #10050, #1674, #27961, #38019, #78934, #11179, #45340, #44223 ) ),
 .UNSPECIFIED., .F., .T., .T. ) 
 B_SPLINE_SURFACE_WITH_KNOTS ( ( 2, 2 ),
 ( 3, 2, 2, 2, 3 ),
 ( -10000.00000000000000, 10000.00000000000000 ),
 ( 0.000000000000000000, 1.570796326794899889, 3.141592653589790007, 4.712388980384689674, 6.283185307179590673 ),
 .UNSPECIFIED. ) 
 GEOMETRIC_REPRESENTATION_ITEM ( )  RATIONAL_B_SPLINE_SURFACE ( (
 ( 1.000000000000000000, 0.7071067811865480168, 1.000000000000000000, 0.7071067811865480168, 1.000000000000000000, 0.7071067811865480168, 1.000000000000000000, 0.7071067811865480168, 1.000000000000000000),
 ( 1.000000000000000000, 0.7071067811865480168, 1.000000000000000000, 0.7071067811865480168, 1.000000000000000000, 0.7071067811865480168, 1.000000000000000000, 0.7071067811865480168, 1.000000000000000000) ) ) 
 REPRESENTATION_ITEM ( '' )  SURFACE ( )  );
#26154 = CARTESIAN_POINT ( 'NONE',  ( 0.000000000000000000, 1401.254281879943164, 137.0999999980979851 ) ) ;
#26156 = CARTESIAN_POINT ( 'NONE',  ( -1.810518240848369986, 1516.538255842539911, 201.4127107417070022 ) ) ;
#26158 = ORIENTED_EDGE ( 'NONE', *, *, #17536, .T. ) ;
#26157 = CARTESIAN_POINT ( 'NONE',  ( 23.93532109230000060, 1509.062825906829858, 195.0658673578979858 ) ) ;
#26159 = CARTESIAN_POINT ( 'NONE',  ( -17.67443188212616434, 1460.218465826193324, 228.1753073352142849 ) ) ;
#26160 = CARTESIAN_POINT ( 'NONE',  ( -50.70917129120000055, 1383.085947422079926, 226.2616357312589912 ) ) ;
#26161 = CARTESIAN_POINT ( 'NONE',  ( 8.473460899918398681, 1436.816749859699939, 207.5081568175040161 ) ) ;
#26162 = ORIENTED_EDGE ( 'NONE', *, *, #35860, .T. ) ;
#26163 = VERTEX_POINT ( 'NONE', #35144 ) ;
#26164 = CARTESIAN_POINT ( 'NONE',  ( 16.93701544105510237, 1508.758026244639950, 231.4689131582919970 ) ) ;
#26165 = CARTESIAN_POINT ( 'NONE',  ( -31.32995031131208918, 1523.678648413191695, 196.3423562208917872 ) ) ;
#26166 = CARTESIAN_POINT ( 'NONE',  ( 39.71405398454739100, 1440.955322443209980, 136.8225870968819891 ) ) ;
#26168 = CARTESIAN_POINT ( 'NONE',  ( 4.351134154479999516, 1486.174099317390073, 218.9925762311689823 ) ) ;
#26167 = CARTESIAN_POINT ( 'NONE',  ( 5.451195050909999503E-14, 1410.389826760030019, 269.3346704430979912 ) ) ;
#26169 = DIRECTION ( 'NONE',  ( -0.5877852522927941026, 1.077399419887002351E-16, 0.8090169943747143044 ) ) ;
#26170 = CARTESIAN_POINT ( 'NONE',  ( -109.3407845659999964, 1384.040961356549815, 297.1897130710590318 ) ) ;
#26171 = EDGE_CURVE ( 'NONE', #107938, #234, #99523, .T. ) ;
#26172 = CARTESIAN_POINT ( 'NONE',  ( -12.84239665067440050, 1435.935719077439899, 150.8114796122480072 ) ) ;
#26173 = CARTESIAN_POINT ( 'NONE',  ( -19.87824503550000088, 1484.486535651230042, 191.0390967410979783 ) ) ;
#26174 = CARTESIAN_POINT ( 'NONE',  ( 1.337177534479999874, 1409.127636081429955, 185.8413015776979762 ) ) ;
#26175 = CARTESIAN_POINT ( 'NONE',  ( 1.980108968457849894, 1486.664140084620158, 197.3565552069889861 ) ) ;
#26176 = CARTESIAN_POINT ( 'NONE',  ( -11.53918879130000086, 1434.258396904259826, 151.3471600665980077 ) ) ;
#26177 = CARTESIAN_POINT ( 'NONE',  ( 8.601478387608290532, 1434.291646609100098, 205.4210292933150015 ) ) ;
#26178 = CARTESIAN_POINT ( 'NONE',  ( -16.38663586692679885, 1420.666626819609974, 203.2878343952710054 ) ) ;
#26179 = CARTESIAN_POINT ( 'NONE',  ( -2.080482507937010173, 1450.172760316540007, 183.1621233083120046 ) ) ;
#26180 = CARTESIAN_POINT ( 'NONE',  ( 2.228957627849999845, 1464.745732024629888, 236.9236403881979811 ) ) ;
#26181 = ORIENTED_EDGE ( 'NONE', *, *, #102233, .F. ) ;
#26182 = CARTESIAN_POINT ( 'NONE',  ( -2.775540907220860110, 1468.867511704140043, 187.4507030301369923 ) ) ;
#26183 = CARTESIAN_POINT ( 'NONE',  ( -44.79032719779999638, 1444.249662561040168, 269.6864475883979821 ) ) ;
#26184 = CARTESIAN_POINT ( 'NONE',  ( -23.72500815532294638, 1436.282246268031486, 212.5115884784333105 ) ) ;
#26185 = CARTESIAN_POINT ( 'NONE',  ( -9.526128307108560733, 1440.436522615020067, 205.9995050262249947 ) ) ;
#26186 = CARTESIAN_POINT ( 'NONE',  ( -10.69712516999999963, 1469.751244810890057, 192.0684298487989849 ) ) ;
#26187 = B_SPLINE_CURVE_WITH_KNOTS ( 'NONE', 3,
 ( #11287, #45454, #79596, #2900, #37018, #20209, #101300, #15638, #83420, #67750, #92926, #66110, #49292, #49844, #16198, #57706, #15101, #110278, #6716, #7274, #91278, #91822, #109734, #31365, #100234, #101860, #14558, #41986, #57153, #48748, #6165, #33554, #108070, #108630, #24048, #25154, #32484, #24594, #5628, #82329, #82872, #58243, #67200, #41438, #40872, #90720, #22948, #39780, #40319, #73939, #75048, #14004, #74501, #48191, #66656, #109200, #84528, #50400, #31917, #65548, #100758, #92365, #7816, #83974, #99657, #75604, #23513, #33014, #76135, #58787, #69973, #34677, #86185 ),
 .UNSPECIFIED., .F., .F.,
 ( 4, 3, 3, 3, 3, 3, 3, 3, 3, 3, 3, 3, 3, 3, 3, 3, 3, 3, 3, 3, 3, 3, 3, 3, 4 ),
 ( -3.000000000000000000, -2.908102647996280155, -2.782376461063030160, -2.655195141559369976, -2.527218228074600059, -2.398166538595950303, -2.268699843587460130, -2.139077724919949741, -2.009568716481330064, -1.880785536864220120, -1.752803873385159861, -1.625825473067359805, -1.500001823732700190, -1.408018940171470001, -1.282042450005529854, -1.154645469624880239, -1.026484574474419986, -0.8973212114648321247, -0.7677990144031130448, -0.6381809425520890144, -0.5087351739316061661, -0.3801018622984368989, -0.2523159959961591703, -0.1255687713132269678, -1.339495774743681977E-06 ),
 .UNSPECIFIED. ) ;
#26188 = ADVANCED_FACE ( 'NONE', ( #12149 ), #35025, .F. ) ;
#26189 = CARTESIAN_POINT ( 'NONE',  ( -1.045136941292439999E-08, 1473.203432950090018, 261.6844113528200069 ) ) ;
#26190 = CARTESIAN_POINT ( 'NONE',  ( 2.816490516637460306, 1409.065320745530244, 230.5891822038450130 ) ) ;
#26191 = CARTESIAN_POINT ( 'NONE',  ( -1.184716195880000100, 1415.245980409529921, 227.1375410387979912 ) ) ;
#26192 = CARTESIAN_POINT ( 'NONE',  ( -10.22449367669999987, 1419.740728945330147, 231.9262419709980065 ) ) ;
#26193 = CARTESIAN_POINT ( 'NONE',  ( -2.703378773469999885, 1475.094742016189912, 198.0005565889990180 ) ) ;
#26194 = CARTESIAN_POINT ( 'NONE',  ( -104.4762617860000091, 1389.781270533860152, 306.5625267145589987 ) ) ;
#26195 = CARTESIAN_POINT ( 'NONE',  ( -0.8188256143092619288, 1485.179768421087147, 182.0112568513308133 ) ) ;
#26196 = CARTESIAN_POINT ( 'NONE',  ( -0.8254386033013292323, 1358.527646167416151, 208.3718459617010978 ) ) ;
#26197 = CARTESIAN_POINT ( 'NONE',  ( -45.81331811595649839, 1439.434550458239983, 268.7575993174490350 ) ) ;
#26198 = CARTESIAN_POINT ( 'NONE',  ( -2.500000000000000000, 1431.404049859629822, 183.8987783686980038 ) ) ;
#26199 = EDGE_CURVE ( 'NONE', #48650, #59045, #49188, .T. ) ;
#26200 = CARTESIAN_POINT ( 'NONE',  ( 26.21857634852423047, 1435.413047617778602, 135.3174475323201591 ) ) ;
#26201 = ORIENTED_EDGE ( 'NONE', *, *, #94114, .F. ) ;
#26202 = CARTESIAN_POINT ( 'NONE',  ( 3.462835627365000057, 1517.038650117239968, 210.2415636864969883 ) ) ;
#26203 = FACE_OUTER_BOUND ( 'NONE', #76452, .T. ) ;
#26204 = CARTESIAN_POINT ( 'NONE',  ( -5.064170362302888861, 1470.551699771569702, 217.9081933660337143 ) ) ;
#26205 = CARTESIAN_POINT ( 'NONE',  ( 7.523283297491509813, 1425.862182174410009, 212.2493654379539976 ) ) ;
#26206 = CIRCLE ( 'NONE', #72753, 1.000002393159227010 ) ;
#26207 = CARTESIAN_POINT ( 'NONE',  ( -26.86092681858010067, 1451.722180651600183, 135.7938040751629671 ) ) ;
#26208 = EDGE_LOOP ( 'NONE', ( #24291, #37019, #61934, #8169, #98887 ) ) ;
#26209 = CARTESIAN_POINT ( 'NONE',  ( -11.75869035857540013, 1517.151704408390060, 190.9442076533970010 ) ) ;
#26211 = CARTESIAN_POINT ( 'NONE',  ( 15.28316325029999945, 1506.811133727029983, 193.2980993196979966 ) ) ;
#26210 = CARTESIAN_POINT ( 'NONE',  ( -3.317974621678423830, 1524.412455883367784, 176.3320022186326241 ) ) ;
#26212 = EDGE_CURVE ( 'NONE', #27637, #44414, #45237, .T. ) ;
#26213 = CARTESIAN_POINT ( 'NONE',  ( 2.197066704608598098, 1487.041132010079082, 219.7150323356243575 ) ) ;
#26214 = CARTESIAN_POINT ( 'NONE',  ( -23.72150209009999955, 1436.115933882590070, 211.9493966405580068 ) ) ;
#26215 = ADVANCED_FACE ( 'NONE', ( #9810 ), #60071, .F. ) ;
#26216 = FACE_OUTER_BOUND ( 'NONE', #39165, .T. ) ;
#26217 = CYLINDRICAL_SURFACE ( 'NONE', #7825, 2.000000000000000000 ) ;
#26218 = ORIENTED_EDGE ( 'NONE', *, *, #42400, .T. ) ;
#26219 = CARTESIAN_POINT ( 'NONE',  ( -4.199545054528389443, 1410.181605891940080, 269.8668074039729845 ) ) ;
#26220 = CARTESIAN_POINT ( 'NONE',  ( -2.493697079054999932, 1516.977201124959947, 208.0034927161370035 ) ) ;
#26221 = CARTESIAN_POINT ( 'NONE',  ( 6.457394820134600089, 1416.588625856350063, 231.2278128514520006 ) ) ;
#26222 = CARTESIAN_POINT ( 'NONE',  ( -0.2658540493943280514, 1507.120020986029886, 237.3289608297170048 ) ) ;
#26224 = EDGE_LOOP ( 'NONE', ( #21085, #101645, #87232, #29166, #61387 ) ) ;
#26223 = CARTESIAN_POINT ( 'NONE',  ( -3.585211238355716645, 1368.112806773307057, 207.6218459616988241 ) ) ;
#26225 = ORIENTED_EDGE ( 'NONE', *, *, #39138, .T. ) ;
#26226 = CARTESIAN_POINT ( 'NONE',  ( -23.60449339185390016, 1410.417139340120002, 210.1580197820780143 ) ) ;
#26227 = EDGE_CURVE ( 'NONE', #26062, #36172, #29360, .T. ) ;
#26228 = CARTESIAN_POINT ( 'NONE',  ( -4.159820404830000484, 1424.695346998130162, 185.9273424667980237 ) ) ;
#26229 = CARTESIAN_POINT ( 'NONE',  ( -109.9849400530580112, 1384.915723531200001, 311.4561069221339835 ) ) ;
#26230 = CARTESIAN_POINT ( 'NONE',  ( -45.66959065914245031, 1440.472161357215555, 266.1886509646802779 ) ) ;
#26231 = EDGE_CURVE ( 'NONE', #81018, #4524, #90423, .T. ) ;
#26232 = CARTESIAN_POINT ( 'NONE',  ( -18.87215647974419852, 1416.576002133260090, 207.5745059148389942 ) ) ;
#26233 = ADVANCED_FACE ( 'NONE', ( #19857 ), #94941, .T. ) ;
#26234 = CARTESIAN_POINT ( 'NONE',  ( -19.62275393000000179, 1430.792229069829773, 223.6261147419979807 ) ) ;
#26235 = CARTESIAN_POINT ( 'NONE',  ( 35.73139755195909117, 1463.185613522950007, 267.0027651688810124 ) ) ;
#26236 = CARTESIAN_POINT ( 'NONE',  ( -11.66472555445337633, 1463.778378584986285, 231.3814271317881150 ) ) ;
#26237 = CARTESIAN_POINT ( 'NONE',  ( 20.71343476517513338, 1522.382868172863937, 179.9059455038194528 ) ) ;
#26238 = CARTESIAN_POINT ( 'NONE',  ( 3.446329775655000205, 1516.812046502680005, 206.2422037788969931 ) ) ;
#26239 = ORIENTED_EDGE ( 'NONE', *, *, #55441, .F. ) ;
#26240 = CARTESIAN_POINT ( 'NONE',  ( 18.75857324853270924, 1458.153377316558135, 227.2545901758803950 ) ) ;
#26241 = CARTESIAN_POINT ( 'NONE',  ( 1.528009309627449852, 1453.500417136500118, 183.4545884030709999 ) ) ;
#26242 = DIRECTION ( 'NONE',  ( 5.980589973904019347E-17, -1.000000000000000000, 1.736889445713099699E-16 ) ) ;
#26243 = ORIENTED_EDGE ( 'NONE', *, *, #51535, .T. ) ;
#26245 = B_SPLINE_CURVE_WITH_KNOTS ( 'NONE', 3,
 ( #22179, #5406, #107862, #64798, #98907, #65340, #97805, #23294, #48532, #56376, #91615, #90506, #98361, #108420, #13784, #14342, #82671, #5962, #82108, #100006, #31151, #56927, #21083, #55287, #99448, #21634, #22725, #89961, #40107, #33347, #101643, #50189, #15987, #7062, #24931, #42314, #58031, #84315, #102213, #59142, #15439, #49631, #33904, #16527, #75389, #66444, #83767, #93264, #6507, #17070, #74834, #76469, #59683, #24396, #68099, #58581, #93796, #49083, #110622, #41217, #92168, #101097, #50718, #23839, #7606, #40662, #25493, #109526, #41760, #51267, #83218, #32802, #8148, #108977, #32264 ),
 .UNSPECIFIED., .F., .F.,
 ( 4, 2, 2, 2, 2, 2, 1, 2, 2, 1, 1, 1, 2, 2, 2, 2, 2, 2, 1, 1, 2, 2, 2, 2, 2, 1, 1, 1, 2, 2, 2, 2, 2, 2, 1, 1, 1, 1, 2, 2, 2, 2, 2, 4 ),
 ( 0.000000000000000000, 0.03124999999985165339, 0.06249999999970330677, 0.09374999999955496710, 0.1249999999994066135, 0.1406249999993321453, 0.1425781249993236521, 0.1428222656243233468, 0.1430664062493230415, 0.1435546874993231803, 0.1445312499993236244, 0.1484374999993233746, 0.1562499999993230138, 0.1874999999993217370, 0.2499999999993183786, 0.2812499999993166577, 0.2851562499993169353, 0.2871093749993167688, 0.2890624999993166022, 0.2968749999993162136, 0.3124999999993156030, 0.3749999999993113842, 0.4374999999993071653, 0.4687499999993049449, 0.4843749999993032795, 0.4921874999993019473, 0.4960937499993012811, 0.4980468749993015032, 0.4990234374993021693, 0.4999999999993027799, 0.6249999999993367528, 0.6874999999993542943, 0.7187499999993625099, 0.7343749999993666178, 0.7421874999993686162, 0.7460937499993696154, 0.7480468749993695043, 0.7490234374993699484, 0.7495117187493701705, 0.7499999999993703925, 0.8124999999995278221, 0.8749999999996852518, 0.9374999999998425704, 1.000000000000000000 ),
 .UNSPECIFIED. ) ;
#26244 = CARTESIAN_POINT ( 'NONE',  ( 3.945788320329008503, 1515.565606824783117, 207.8723252021519272 ) ) ;
#26246 = CARTESIAN_POINT ( 'NONE',  ( 25.67981543420000179, 1451.858828621529938, 135.9465745059980009 ) ) ;
#26247 = CARTESIAN_POINT ( 'NONE',  ( -4.771130221740180311, 1508.551704408389924, 212.6291175505820092 ) ) ;
#26248 = CARTESIAN_POINT ( 'NONE',  ( -6.042424523860000285, 1389.870610953139931, 214.5741421020690041 ) ) ;
#26249 = PLANE ( 'NONE',  #77115 ) ;
#26250 = CARTESIAN_POINT ( 'NONE',  ( 17.44743351239999996, 1409.522338191229892, 195.3742125755979941 ) ) ;
#26251 = CARTESIAN_POINT ( 'NONE',  ( 13.51610093809999924, 1444.324653571829913, 169.3501091259980171 ) ) ;
#26252 = CARTESIAN_POINT ( 'NONE',  ( 3.363947596952667318, 1439.689793485319342, 184.4158855439752074 ) ) ;
#26254 = CARTESIAN_POINT ( 'NONE',  ( -21.57689972017744395, 1429.260891947445543, 219.1104016736593678 ) ) ;
#26253 = CARTESIAN_POINT ( 'NONE',  ( 1.043151750310000070, 1416.586530163930092, 233.4334045153980242 ) ) ;
#26255 = DIRECTION ( 'NONE',  ( 0.9942586961433745874, 0.000000000000000000, -0.1070030146457423004 ) ) ;
#26256 = AXIS2_PLACEMENT_3D ( 'NONE', #73800, #63218, #97325 ) ;
#26257 = CARTESIAN_POINT ( 'NONE',  ( 19.77969251879999746, 1507.818093401829856, 229.2755605921979907 ) ) ;
#26258 = CARTESIAN_POINT ( 'NONE',  ( -8.982687423579998054, 1383.819621401789846, 218.5044028809089980 ) ) ;
#26259 = ADVANCED_FACE ( 'NONE', ( #67409 ), #57897, .T. ) ;
#26260 = CARTESIAN_POINT ( 'NONE',  ( 14.36154233419531501, 1421.756987585290744, 230.5507565205384992 ) ) ;
#26261 = ORIENTED_EDGE ( 'NONE', *, *, #109015, .T. ) ;
#26262 = CARTESIAN_POINT ( 'NONE',  ( 12.80019129569889991, 1416.529254608160045, 221.9949054940630049 ) ) ;
#26263 = CARTESIAN_POINT ( 'NONE',  ( -17.43675326300159867, 1417.688629928019964, 206.2161178420579972 ) ) ;
#26264 = CARTESIAN_POINT ( 'NONE',  ( -0.5150210539746830074, 1410.202340106000293, 233.1625166594439804 ) ) ;
#26265 = CARTESIAN_POINT ( 'NONE',  ( -11.39903424189999903, 1388.037600957480208, 201.7885523045490004 ) ) ;
#26266 = CARTESIAN_POINT ( 'NONE',  ( -0.1950033126530047733, 1421.009551141655493, 193.7183299770628651 ) ) ;
#26267 = CARTESIAN_POINT ( 'NONE',  ( -4.327305182179610021, 1515.146653429449998, 208.6708865915660169 ) ) ;
#26268 = CARTESIAN_POINT ( 'NONE',  ( -15.71554774059999815, 1452.384630541829893, 224.8635561783979711 ) ) ;
#26269 = CARTESIAN_POINT ( 'NONE',  ( -21.77056747205107712, 1509.419234473328515, 191.5442852694430087 ) ) ;
#26270 = CARTESIAN_POINT ( 'NONE',  ( 11.89682012279999945, 1433.280912625190012, 150.0673495551980068 ) ) ;
#26271 = CARTESIAN_POINT ( 'NONE',  ( 15.71554773450000297, 1452.384630544830088, 224.8635562088979896 ) ) ;
#26272 = AXIS2_PLACEMENT_3D ( 'NONE', #99388, #5905, #93202 ) ;
#26273 = CARTESIAN_POINT ( 'NONE',  ( 12.51099735422840098, 1416.825783990419950, 196.0986168021389915 ) ) ;
#26274 = CARTESIAN_POINT ( 'NONE',  ( -9.807154110200000829, 1424.402417317040090, 192.4107027041989966 ) ) ;
#26275 = CARTESIAN_POINT ( 'NONE',  ( -1.842962231260000028, 1515.064792882589927, 213.4512947377390049 ) ) ;
#26276 = CARTESIAN_POINT ( 'NONE',  ( 14.89703407660000067, 1485.172368269729986, 224.4040237037980035 ) ) ;
#26277 = CARTESIAN_POINT ( 'NONE',  ( -4.664011873159999766, 1486.047054426829845, 182.2406068358980065 ) ) ;
#26278 = APPLICATION_CONTEXT ( 'automotive_design' ) ;
#26279 = DIRECTION ( 'NONE',  ( 0.7074300732638268974, 0.02470400251906259420, -0.7063514732068408852 ) ) ;
#26280 = CARTESIAN_POINT ( 'NONE',  ( -30.16083877470000019, 1510.094636368229885, 211.8907222485079842 ) ) ;
#26281 = CARTESIAN_POINT ( 'NONE',  ( -8.111163737316729794, 1425.152143030509933, 209.4308767762499599 ) ) ;
#26282 = VECTOR ( 'NONE', #49750, 1000.000000000000000 ) ;
#26283 = CARTESIAN_POINT ( 'NONE',  ( 2.964073292005991345, 1446.907476413705126, 170.5322007588701752 ) ) ;
#26284 = CARTESIAN_POINT ( 'NONE',  ( 25.74953088568717163, 1436.651976592735537, 137.0890486594359459 ) ) ;
#26285 = CARTESIAN_POINT ( 'NONE',  ( -1.105873109679999855, 1515.456834174690130, 204.9203193849689910 ) ) ;
#26286 = CARTESIAN_POINT ( 'NONE',  ( 22.78047381600000065, 1519.913060387329779, 214.2867222517980110 ) ) ;
#26287 = CARTESIAN_POINT ( 'NONE',  ( 13.52268454819029841, 1497.923627212899873, 227.8730059201319875 ) ) ;
#26288 = CARTESIAN_POINT ( 'NONE',  ( 7.722536764694999611, 1517.050041317280147, 213.7387458049869906 ) ) ;
#26289 = CARTESIAN_POINT ( 'NONE',  ( -17.81440792103600046, 1419.712128143199834, 206.0771405611880027 ) ) ;
#26290 = CARTESIAN_POINT ( 'NONE',  ( 0.1636539809332889783, 1484.078125311330041, 181.9191924309680246 ) ) ;
#26292 = ORIENTED_EDGE ( 'NONE', *, *, #89173, .F. ) ;
#26291 = CARTESIAN_POINT ( 'NONE',  ( 18.22756002379999529, 1431.409129072690121, 207.4347713430790066 ) ) ;
#26293 = DIRECTION ( 'NONE',  ( -0.6736849260863840838, 0.000000000000000000, 0.7390186874254150995 ) ) ;
#26294 = CARTESIAN_POINT ( 'NONE',  ( -9.129808743239919977, 1383.863787745319996, 218.5279288296370055 ) ) ;
#26295 = DIRECTION ( 'NONE',  ( 0.4794255386042002298, -8.806904269216945661E-17, -0.8775825618903744241 ) ) ;
#26296 = CARTESIAN_POINT ( 'NONE',  ( -31.80535162409287864, 1525.137906803776332, 216.1511969346493345 ) ) ;
#26297 = CARTESIAN_POINT ( 'NONE',  ( 11.69994445601069977, 1435.514615917619949, 225.6365337787890155 ) ) ;
#26298 = ORIENTED_EDGE ( 'NONE', *, *, #45205, .T. ) ;
#26299 = LINE ( 'NONE', #35265, #89610 ) ;
#26300 = CARTESIAN_POINT ( 'NONE',  ( -14.49023771376019987, 1379.969971553530058, 208.6314281993359998 ) ) ;
#26301 = CARTESIAN_POINT ( 'NONE',  ( 6.725176165684159102, 1446.961637082904645, 203.0350805069372484 ) ) ;
#26302 = LINE ( 'NONE', #94613, #60669 ) ;
#26303 = CARTESIAN_POINT ( 'NONE',  ( -8.459774974535099190, 1436.681737689380043, 211.0369107578229944 ) ) ;
#26304 = CARTESIAN_POINT ( 'NONE',  ( -109.0401330529258956, 1382.147805055439449, 310.8429168940339764 ) ) ;
#26305 = CARTESIAN_POINT ( 'NONE',  ( -12.31584554800360465, 1377.880485592854939, 209.0191605607812733 ) ) ;
#26306 = DIRECTION ( 'NONE',  ( 0.000000000000000000, 0.000000000000000000, 1.000000000000000000 ) ) ;
#26307 = CARTESIAN_POINT ( 'NONE',  ( -11.67564806959999935, 1391.913060387289988, 208.7639730238099958 ) ) ;
#26308 = CARTESIAN_POINT ( 'NONE',  ( -72.68591527607071612, 1385.125501078250181, 271.2577098130889794 ) ) ;
#26309 = CARTESIAN_POINT ( 'NONE',  ( -17.32903452410000256, 1411.910626558729973, 192.2240021034980089 ) ) ;
#26310 = CARTESIAN_POINT ( 'NONE',  ( 10.30462054015580087, 1426.851742110210125, 209.1703782512580005 ) ) ;
#26311 = ORIENTED_EDGE ( 'NONE', *, *, #60018, .T. ) ;
#26312 = CARTESIAN_POINT ( 'NONE',  ( -15.80615402491370247, 1410.712807750240017, 226.7221385999669963 ) ) ;
#26314 = ORIENTED_EDGE ( 'NONE', *, *, #44853, .F. ) ;
#26313 = CARTESIAN_POINT ( 'NONE',  ( 5.519891178750000016, 1440.499824924530003, 154.7645185998979969 ) ) ;
#26315 = CARTESIAN_POINT ( 'NONE',  ( 6.786745158321280336, 1466.611179241469927, 216.3706489178590004 ) ) ;
#26316 = ORIENTED_EDGE ( 'NONE', *, *, #69366, .T. ) ;
#26317 = CARTESIAN_POINT ( 'NONE',  ( 26.26214385720000166, 1509.606682185630007, 219.0507925541380132 ) ) ;
#26318 = CARTESIAN_POINT ( 'NONE',  ( -9.328535443866920573, 1363.278783432113869, 210.6218459616987957 ) ) ;
#26319 = CARTESIAN_POINT ( 'NONE',  ( -10.48582348350000082, 1492.891079834690117, 204.9070088834189960 ) ) ;
#26320 = EDGE_CURVE ( 'NONE', #77955, #75598, #101130, .T. ) ;
#26321 = CARTESIAN_POINT ( 'NONE',  ( -2.038847259689231084, 1501.977400791986611, 173.3106345060153046 ) ) ;
#26322 = CARTESIAN_POINT ( 'NONE',  ( -11.60004869885203505, 1428.147403133767057, 134.2065354802118975 ) ) ;
#26323 = CARTESIAN_POINT ( 'NONE',  ( 17.94073347927875872, 1434.894695372993056, 215.4556157790318309 ) ) ;
#26324 = DIRECTION ( 'NONE',  ( 0.000000000000000000, 1.000000000000000000, -1.836970198721029688E-16 ) ) ;
#26325 = CARTESIAN_POINT ( 'NONE',  ( 1.600048698852036821, 1411.254281879943164, 137.0999999980979851 ) ) ;
#26326 = CARTESIAN_POINT ( 'NONE',  ( -10.25368860849440011, 1391.913060387289988, 204.2726074216130030 ) ) ;
#26327 = CARTESIAN_POINT ( 'NONE',  ( -6.371134682390000137, 1368.423166410909971, 207.6218459616989946 ) ) ;
#26328 = CARTESIAN_POINT ( 'NONE',  ( -29.41145195048104455, 1525.795403383247276, 221.5574857735277874 ) ) ;
#26329 = CARTESIAN_POINT ( 'NONE',  ( 2.477986732234999767, 1516.922519270759949, 205.8529865360470126 ) ) ;
#26330 = AXIS2_PLACEMENT_3D ( 'NONE', #30241, #64976, #81197 ) ;
#26331 = CARTESIAN_POINT ( 'NONE',  ( 3.701620314320000382, 1446.913866055039989, 156.0867562885979964 ) ) ;
#26332 = CARTESIAN_POINT ( 'NONE',  ( -2.500000000000000000, 1433.175796427819932, 157.5194111165980075 ) ) ;
#26333 = CARTESIAN_POINT ( 'NONE',  ( 44.92382427180000093, 1440.913060384100163, 269.6913831871979710 ) ) ;
#26335 = ORIENTED_EDGE ( 'NONE', *, *, #70675, .F. ) ;
#26334 = CARTESIAN_POINT ( 'NONE',  ( -3.607508154840000092, 1496.493922223389973, 219.8931764588990063 ) ) ;
#26336 = PLANE ( 'NONE',  #34891 ) ;
#26337 = ORIENTED_EDGE ( 'NONE', *, *, #103789, .T. ) ;
#26338 = CARTESIAN_POINT ( 'NONE',  ( -16.52740844507182416, 1514.201209519881331, 223.4276059376695400 ) ) ;
#26339 = CARTESIAN_POINT ( 'NONE',  ( -24.41209542680000055, 1449.795792328920015, 203.6715618845580025 ) ) ;
#26340 = B_SPLINE_CURVE_WITH_KNOTS ( 'NONE', 3,
 ( #94257, #69099, #110520, #93693, #16429, #16973, #67996, #9171, #35469, #34914, #51734, #94825, #8051, #102642, #27083, #50621, #101542, #17532, #24831, #59036 ),
 .UNSPECIFIED., .F., .F.,
 ( 4, 2, 2, 2, 1, 1, 1, 1, 2, 2, 2, 4 ),
 ( 0.000000000000000000, 0.2499999999984017229, 0.3749999999975950904, 0.4374999999971947440, 0.4687499999969976794, 0.4843749999969083619, 0.4921874999968666176, 0.4960937499968487430, 0.4980468749968492426, 0.4999999999968497422, 0.7499999999984249266, 1.000000000000000000 ),
 .UNSPECIFIED. ) ;
#26342 = CARTESIAN_POINT ( 'NONE',  ( 16.75289443972269865, 1410.133484963379942, 192.0576568603480041 ) ) ;
#26341 = CARTESIAN_POINT ( 'NONE',  ( -11.61237467649999999, 1426.780387251330012, 135.2650375955979882 ) ) ;
#26343 = CARTESIAN_POINT ( 'NONE',  ( -6.933587693644999383, 1516.542957540330008, 210.8312046333570038 ) ) ;
#26344 = CARTESIAN_POINT ( 'NONE',  ( 18.18605408113305799, 1509.667548394901132, 185.2623056092570266 ) ) ;
#26345 = CARTESIAN_POINT ( 'NONE',  ( -22.91749086919999812, 1507.625766668030110, 207.6071136176580012 ) ) ;
#26346 = CARTESIAN_POINT ( 'NONE',  ( -40.57810857620000178, 1433.211872144790050, 261.6156768307980087 ) ) ;
#26347 = CARTESIAN_POINT ( 'NONE',  ( -13.93938412159879903, 1379.689544443230034, 208.2922637222520166 ) ) ;
#26349 = ADVANCED_FACE ( 'NONE', ( #33220 ), #74699, .T. ) ;
#26348 = CARTESIAN_POINT ( 'NONE',  ( 29.34423976395289912, 1509.844966207019979, 209.6154881191580159 ) ) ;
#26350 = CONTEXT_DEPENDENT_SHAPE_REPRESENTATION ( #54934, #89347 ) ;
#26351 = CARTESIAN_POINT ( 'NONE',  ( -4.994803988990000221, 1391.714632731289839, 214.5952593868790075 ) ) ;
#26352 = CARTESIAN_POINT ( 'NONE',  ( -35.08468067933920054, 1437.159863514480094, 136.5376250597369960 ) ) ;
#26353 = ORIENTED_EDGE ( 'NONE', *, *, #99676, .T. ) ;
#26354 = CARTESIAN_POINT ( 'NONE',  ( 10.35663606681439930, 1396.797897193559947, 200.7170876621850084 ) ) ;
#26355 = CARTESIAN_POINT ( 'NONE',  ( 9.633682766397971164, 1462.526647204680103, 207.6052849751269775 ) ) ;
#26356 = EDGE_CURVE ( 'NONE', #69273, #2114, #14444, .T. ) ;
#26357 = CARTESIAN_POINT ( 'NONE',  ( 37.65047687761219919, 1442.773887286080026, 137.1096749932030150 ) ) ;
#26358 = ORIENTED_EDGE ( 'NONE', *, *, #88850, .T. ) ;
#26359 = ORIENTED_EDGE ( 'NONE', *, *, #40504, .T. ) ;
#26360 = CIRCLE ( 'NONE', #35324, 2.000061678640922214 ) ;
#26361 = DIRECTION ( 'NONE',  ( 0.6709778558543747495, 0.000000000000000000, 0.7414773880254650340 ) ) ;
#26362 = CARTESIAN_POINT ( 'NONE',  ( -11.84030404028099781, 1430.236004227029980, 151.0624551439379957 ) ) ;
#26363 = EDGE_CURVE ( 'NONE', #22756, #109851, #57119, .T. ) ;
#26364 = VERTEX_POINT ( 'NONE', #34879 ) ;
#26365 = LINE ( 'NONE', #25803, #102813 ) ;
#26366 = CARTESIAN_POINT ( 'NONE',  ( -13.59512379659999937, 1507.703333832490216, 209.3532891243080201 ) ) ;
#26367 = CARTESIAN_POINT ( 'NONE',  ( -11.87502386937130083, 1433.007271227619867, 149.9804723889419904 ) ) ;
#26368 = EDGE_CURVE ( 'NONE', #53580, #23969, #36659, .T. ) ;
#26369 = CARTESIAN_POINT ( 'NONE',  ( 28.17098211812724173, 1509.816545695249943, 206.0731778711173092 ) ) ;
#26370 = CARTESIAN_POINT ( 'NONE',  ( 7.321627508978070686, 1508.611138448550037, 203.6086236178030333 ) ) ;
#26371 = CARTESIAN_POINT ( 'NONE',  ( 10.56996490077299811, 1452.372263598349946, 208.9876866165449769 ) ) ;
#26372 = DIRECTION ( 'NONE',  ( -0.3363363969979660806, -0.9417419115949053898, 0.000000000000000000 ) ) ;
#26373 = CARTESIAN_POINT ( 'NONE',  ( -89.02434603483330022, 1384.834799535030015, 291.9443828696540209 ) ) ;
#26374 = VERTEX_POINT ( 'NONE', #69623 ) ;
#26375 = CARTESIAN_POINT ( 'NONE',  ( -2.873958889724999910, 1516.588006113850042, 202.1873174023370154 ) ) ;
#26376 = CARTESIAN_POINT ( 'NONE',  ( 2.879318417774999972, 1516.995911393979895, 209.8571825100049750 ) ) ;
#26377 = ORIENTED_EDGE ( 'NONE', *, *, #73348, .T. ) ;
#26378 = CARTESIAN_POINT ( 'NONE',  ( 11.81236103907129831, 1428.866417594400218, 148.7658394821069692 ) ) ;
#26379 = CARTESIAN_POINT ( 'NONE',  ( 3.965270473948547814, 1511.478973222888044, 217.3060377250480713 ) ) ;
#26380 = EDGE_LOOP ( 'NONE', ( #14121, #91669, #55313, #8849 ) ) ;
#26381 = CARTESIAN_POINT ( 'NONE',  ( -1.465793917108519917, 1484.360957496709943, 182.4810413606819850 ) ) ;
#26382 = CARTESIAN_POINT ( 'NONE',  ( -6.427049037362169592, 1508.551704408389924, 219.3403462825500014 ) ) ;
#26383 = CARTESIAN_POINT ( 'NONE',  ( -2.887288154357296133, 1368.159587626394341, 207.9537811227674808 ) ) ;
#26384 = CARTESIAN_POINT ( 'NONE',  ( -1.636404844837480166, 1469.777808224259843, 219.0527859593750009 ) ) ;
#26385 = CARTESIAN_POINT ( 'NONE',  ( -5.949769683449999569, 1423.165531658830105, 186.4741557280979976 ) ) ;
#26386 = CARTESIAN_POINT ( 'NONE',  ( 10.86918694049999878, 1409.184211811729938, 270.3751304090980057 ) ) ;
#26387 = CARTESIAN_POINT ( 'NONE',  ( 3.116134665881934662, 1509.034509761476329, 204.6344887231309997 ) ) ;
#26388 = CARTESIAN_POINT ( 'NONE',  ( -12.48995958582669985, 1501.883328869510024, 211.6213070116990025 ) ) ;
#26389 = CARTESIAN_POINT ( 'NONE',  ( -16.95839816991464843, 1517.034034369547498, 195.0103398635659744 ) ) ;
#26390 = CARTESIAN_POINT ( 'NONE',  ( -21.11637064600000002, 1379.664572420290142, 209.7302724572810178 ) ) ;
#26391 = CARTESIAN_POINT ( 'NONE',  ( -15.42411914529999883, 1451.321947525430005, 222.6614283628979933 ) ) ;
#26393 = CARTESIAN_POINT ( 'NONE',  ( 15.70632159480000034, 1471.312091221729816, 194.7047488413979863 ) ) ;
#26392 = CARTESIAN_POINT ( 'NONE',  ( -4.804225480384130442, 1496.882362067949998, 198.9430272844270178 ) ) ;
#26394 = CARTESIAN_POINT ( 'NONE',  ( -4.668567705819710589, 1423.680010517363371, 184.4694098598055803 ) ) ;
#26395 = B_SPLINE_CURVE_WITH_KNOTS ( 'NONE', 3,
 ( #47221, #96521, #3041, #107114, #72976, #37713, #38253, #47768, #39361, #62396, #28763, #11959, #46145, #80275, #3589, #83553, #75730, #99244, #99799, #40456, #50531, #56723 ),
 .UNSPECIFIED., .F., .F.,
 ( 4, 3, 3, 3, 3, 3, 3, 4 ),
 ( -15.61492507820850051, -14.86289102913099924, -13.52885667192749963, -12.35991797187899977, -11.57914177227580055, -10.59814511392120018, -9.795446212852318979, -9.104900351529998659 ),
 .UNSPECIFIED. ) ;
#26396 = CIRCLE ( 'NONE', #46106, 7.146147325060000277 ) ;
#26397 = CARTESIAN_POINT ( 'NONE',  ( 17.97366410996650288, 1422.795681845899935, 225.1544947853240046 ) ) ;
#26398 = ADVANCED_FACE ( 'NONE', ( #749 ), #101703, .F. ) ;
#26399 = CARTESIAN_POINT ( 'NONE',  ( -5.789249456297649310, 1423.399501566140088, 91.66914618043580276 ) ) ;
#26400 = ORIENTED_EDGE ( 'NONE', *, *, #86549, .T. ) ;
#26401 = CARTESIAN_POINT ( 'NONE',  ( 18.22058378356810238, 1424.504050405589851, 223.7587054751699895 ) ) ;
#26402 = CARTESIAN_POINT ( 'NONE',  ( -20.64339891394635629, 1523.429859730330236, 179.9837476533126335 ) ) ;
#26403 = CARTESIAN_POINT ( 'NONE',  ( -2.993081948865825570, 1485.686210600610138, 182.6348840854386140 ) ) ;
#26404 = EDGE_CURVE ( 'NONE', #36172, #42124, #101869, .T. ) ;
#26405 = CARTESIAN_POINT ( 'NONE',  ( -14.71755666980000044, 1415.865102022439942, 213.5049452957989899 ) ) ;
#26407 = ORIENTED_EDGE ( 'NONE', *, *, #95293, .F. ) ;
#26406 = CARTESIAN_POINT ( 'NONE',  ( -0.3081309750529439562, 1515.153045852119931, 204.7947081710710222 ) ) ;
#26408 = CARTESIAN_POINT ( 'NONE',  ( -15.46337563405010052, 1415.677402202039957, 209.5778891453549875 ) ) ;
#26409 = CARTESIAN_POINT ( 'NONE',  ( -15.31719378736699966, 1507.616838180409786, 191.9970397177449968 ) ) ;
#26410 = CARTESIAN_POINT ( 'NONE',  ( -11.25570387199999978, 1428.983030176930015, 150.6823813367980165 ) ) ;
#26411 = FACE_OUTER_BOUND ( 'NONE', #61363, .T. ) ;
#26412 = CARTESIAN_POINT ( 'NONE',  ( -5.698435440679999964, 1440.539195541149866, 185.7251249343980248 ) ) ;
#26413 = CARTESIAN_POINT ( 'NONE',  ( -12.26059042640000030, 1378.259319071030177, 207.8536744588589897 ) ) ;
#26414 = DIRECTION ( 'NONE',  ( 8.881784197000000007E-16, -1.000000000000000000, 1.836970198721029688E-16 ) ) ;
#26415 = CARTESIAN_POINT ( 'NONE',  ( -16.25489180516500198, 1512.123798513659949, 221.6559977385670095 ) ) ;
#26416 = CARTESIAN_POINT ( 'NONE',  ( 0.3641805750159999855, 1424.317995881729985, 227.5054904076980051 ) ) ;
#26417 = CARTESIAN_POINT ( 'NONE',  ( -9.809506047440001097, 1478.918602606890090, 213.0364292658189811 ) ) ;
#26419 = CARTESIAN_POINT ( 'NONE',  ( -16.38967734719999925, 1460.095605315129887, 228.4964222805979830 ) ) ;
#26418 = CIRCLE ( 'NONE', #22799, 1.000000000000000888 ) ;
#26420 = CARTESIAN_POINT ( 'NONE',  ( 6.933616821004999764, 1516.548716157039962, 206.8295387017270173 ) ) ;
#26421 = CARTESIAN_POINT ( 'NONE',  ( 21.88497915990000209, 1410.158872715429879, 268.8545754686979876 ) ) ;
#26422 = CARTESIAN_POINT ( 'NONE',  ( 25.00977939330000055, 1436.598012869960030, 137.9330249918980087 ) ) ;
#26423 = CARTESIAN_POINT ( 'NONE',  ( 23.35803260569999651, 1449.721564088129981, 201.4915734787180099 ) ) ;
#26424 = CARTESIAN_POINT ( 'NONE',  ( 15.81201445386249915, 1506.433683730510211, 224.3933755863170063 ) ) ;
#26425 = CARTESIAN_POINT ( 'NONE',  ( -0.4986853141550000035, 1508.982344982729956, 238.8510891614980096 ) ) ;
#26426 = CARTESIAN_POINT ( 'NONE',  ( -15.03352721073179943, 1417.917664510099939, 203.1866864770329926 ) ) ;
#26427 = CARTESIAN_POINT ( 'NONE',  ( -41.61955346608320383, 1442.631757267950206, 136.0084039258269968 ) ) ;
#26428 = CARTESIAN_POINT ( 'NONE',  ( -18.97170710130291127, 1506.426094405750746, 198.0110083291505703 ) ) ;
#26429 = CARTESIAN_POINT ( 'NONE',  ( -18.81809407629999953, 1416.219761279530076, 207.5984327672580037 ) ) ;
#26430 = CARTESIAN_POINT ( 'NONE',  ( -14.15644638650000076, 1445.184054452470036, 188.6148688927980004 ) ) ;
#26431 = CARTESIAN_POINT ( 'NONE',  ( 18.89924248923649941, 1416.831923566683599, 210.6687426849658493 ) ) ;
#26432 = CARTESIAN_POINT ( 'NONE',  ( 17.77898125735369916, 1428.911568982719928, 205.3667159481209978 ) ) ;
#26433 = CARTESIAN_POINT ( 'NONE',  ( -3.584844276230000126, 1496.864215754190127, 220.1846649233989979 ) ) ;
#26434 = ORIENTED_EDGE ( 'NONE', *, *, #88708, .T. ) ;
#26435 = CARTESIAN_POINT ( 'NONE',  ( -2.933667460025000118, 1512.215430505229961, 201.2384290929069834 ) ) ;
#26436 = CARTESIAN_POINT ( 'NONE',  ( -12.32543969330590095, 1409.343474225730006, 200.6744456079329950 ) ) ;
#26437 = AXIS2_PLACEMENT_3D ( 'NONE', #44370, #46030, #80158 ) ;
#26438 = CARTESIAN_POINT ( 'NONE',  ( 10.49820941578430045, 1481.974680494319955, 210.5709914680880104 ) ) ;
#26439 = CARTESIAN_POINT ( 'NONE',  ( -12.23938407635016823, 1377.915032069682411, 210.5017074410068858 ) ) ;
#26440 = CARTESIAN_POINT ( 'NONE',  ( -18.39364418590000128, 1473.256894900929865, 268.3411905449979713 ) ) ;
#26441 = CARTESIAN_POINT ( 'NONE',  ( -18.54648005354870222, 1507.559782640589901, 227.6869933707240250 ) ) ;
#26442 = CARTESIAN_POINT ( 'NONE',  ( 0.3368680511838070268, 1419.194708778680024, 184.5876889618309917 ) ) ;
#26443 = CARTESIAN_POINT ( 'NONE',  ( -24.04911540300000183, 1508.500175526130079, 222.3302192762980098 ) ) ;
#26444 = CARTESIAN_POINT ( 'NONE',  ( -82.57690316193580315, 1384.633320654690124, 305.4287651558460084 ) ) ;
#26445 = B_SPLINE_SURFACE_WITH_KNOTS ( 'NONE', 5, 1, ( 
 ( #52356, #43388 ),
 ( #35523, #104385 ),
 ( #27134, #18703 ),
 ( #841, #34421 ),
 ( #94882, #43933 ),
 ( #8651, #86473 ) ),
 .UNSPECIFIED., .F., .F., .F.,
 ( 6, 6 ),
 ( 2, 2 ),
 ( 0.000000000000000000, 16.10035485789999754 ),
 ( 0.000000000000000000, 14.00000000000000000 ),
 .UNSPECIFIED. ) ;
#26446 = CARTESIAN_POINT ( 'NONE',  ( -20.72718479384839796, 1384.952021344829973, 201.8520775233429845 ) ) ;
#26447 = CARTESIAN_POINT ( 'NONE',  ( 17.96271488095740310, 1423.981419269019852, 225.6927239374410306 ) ) ;
#26448 = AXIS2_PLACEMENT_3D ( 'NONE', #21352, #62321, #55559 ) ;
#26449 = CARTESIAN_POINT ( 'NONE',  ( -9.663014860980000620, 1442.759804623820173, 153.0865865510980086 ) ) ;
#26450 = CARTESIAN_POINT ( 'NONE',  ( -26.12012303998839968, 1482.704885440409953, 211.0358973181160138 ) ) ;
#26451 = CARTESIAN_POINT ( 'NONE',  ( -15.73033044518626333, 1415.742871371153342, 209.5189858198543220 ) ) ;
#26452 = CARTESIAN_POINT ( 'NONE',  ( -8.370897861499999593, 1384.935302011549993, 199.7749308614990014 ) ) ;
#26453 = CARTESIAN_POINT ( 'NONE',  ( -22.52398816560000228, 1409.699615386230107, 206.4986819826179953 ) ) ;
#26454 = CARTESIAN_POINT ( 'NONE',  ( 14.39499504100000138, 1414.971339025629959, 199.6144774512380025 ) ) ;
#26455 = CARTESIAN_POINT ( 'NONE',  ( 3.759063234690000144, 1484.612424520689956, 220.3580642450990013 ) ) ;
#26456 = CARTESIAN_POINT ( 'NONE',  ( 5.046810547520000689, 1422.880139949140130, 194.5523469769989902 ) ) ;
#26457 = CARTESIAN_POINT ( 'NONE',  ( 0.8288084222790000899, 1440.444625599219989, 150.6821045058979962 ) ) ;
#26458 = CARTESIAN_POINT ( 'NONE',  ( 5.325107150730000072, 1437.628063137190111, 228.7363426427990305 ) ) ;
#26459 = CARTESIAN_POINT ( 'NONE',  ( 17.83486663330484845, 1523.678648413191922, 180.3677388339000061 ) ) ;
#26460 = CARTESIAN_POINT ( 'NONE',  ( 20.33643750506929848, 1475.138452887649919, 218.0161091833910234 ) ) ;
#26462 = CARTESIAN_POINT ( 'NONE',  ( -8.297363970850001991, 1383.661068711170174, 199.8123430960490055 ) ) ;
#26461 = CARTESIAN_POINT ( 'NONE',  ( -16.69478953993380088, 1417.256065975089996, 208.2559420391330036 ) ) ;
#26463 = CARTESIAN_POINT ( 'NONE',  ( 11.70972657649789994, 1426.713614540399931, 142.2152413248659855 ) ) ;
#26464 = DIRECTION ( 'NONE',  ( -0.2778957479319200119, -0.4510399357639849338, 0.8481373294622629455 ) ) ;
#26465 = CARTESIAN_POINT ( 'NONE',  ( -11.44853639979999826, 1489.809568400389935, 211.8872501198590044 ) ) ;
#26466 = CARTESIAN_POINT ( 'NONE',  ( 3.553091682609760049, 1446.489235633270255, 199.6236789066639972 ) ) ;
#26467 = CARTESIAN_POINT ( 'NONE',  ( -0.1681561557501680126, 1420.473116156940023, 182.7663335526739843 ) ) ;
#26468 = CARTESIAN_POINT ( 'NONE',  ( -1.711311266675000109, 1516.591755933730155, 203.3510257909670145 ) ) ;
#26470 = CARTESIAN_POINT ( 'NONE',  ( 4.571596902580940203, 1429.775350729068123, 216.5860468117702169 ) ) ;
#26469 = VECTOR ( 'NONE', #88316, 999.9999999999998863 ) ;
#26471 = CARTESIAN_POINT ( 'NONE',  ( 15.83297148113499730, 1514.812393650459853, 193.8421146529669841 ) ) ;
#26472 = CARTESIAN_POINT ( 'NONE',  ( 17.30273524950730035, 1431.037683288380094, 215.1927343395939829 ) ) ;
#26473 = CARTESIAN_POINT ( 'NONE',  ( -18.80245169759999868, 1449.640794194290038, 193.0678026872980126 ) ) ;
#26474 = PLANE ( 'NONE',  #104916 ) ;
#26475 = CARTESIAN_POINT ( 'NONE',  ( 37.73053733700000123, 1449.071358796530149, 136.3468597391979813 ) ) ;
#26477 = ORIENTED_EDGE ( 'NONE', *, *, #47494, .T. ) ;
#26476 = CARTESIAN_POINT ( 'NONE',  ( -59.63899719916989994, 1379.734822786960194, 264.7657198495529656 ) ) ;
#26478 = ORIENTED_EDGE ( 'NONE', *, *, #91780, .T. ) ;
#26479 = CARTESIAN_POINT ( 'NONE',  ( 11.91460776122049836, 1433.652109726360095, 150.4736492753009998 ) ) ;
#26480 = CARTESIAN_POINT ( 'NONE',  ( 20.49599333844850335, 1525.960063244516959, 184.3798832129034793 ) ) ;
#26481 = ORIENTED_EDGE ( 'NONE', *, *, #16455, .F. ) ;
#26482 = CARTESIAN_POINT ( 'NONE',  ( -106.9651580870000060, 1379.002928632980002, 308.0502217555589937 ) ) ;
#26483 = CARTESIAN_POINT ( 'NONE',  ( -10.35394977520730109, 1447.847288705600022, 209.4908303012460067 ) ) ;
#26484 = DIRECTION ( 'NONE',  ( 0.3090169943749447867, 0.000000000000000000, -0.9510565162951545304 ) ) ;
#26485 =( BOUNDED_SURFACE ( )  B_SPLINE_SURFACE ( 3, 2, ( 
 ( #4848, #57491, #80473 ),
 ( #38453, #46891, #12707 ),
 ( #106218, #14892, #81547 ),
 ( #74289, #3791, #29500 ),
 ( #55839, #39566, #65886 ),
 ( #37922, #107316, #4322 ),
 ( #72625, #63694, #73739 ),
 ( #47424, #30611, #89417 ),
 ( #38995, #106757, #30047 ),
 ( #64239, #13235, #73172 ) ),
 .UNSPECIFIED., .F., .F., .F. ) 
 B_SPLINE_SURFACE_WITH_KNOTS ( ( 4, 2, 2, 2, 4 ),
 ( 3, 3 ),
 ( 0.000000000000000000, 0.3926990816987241395, 0.7853981633974482790, 1.178097245096172418, 1.570796326794896558 ),
 ( 0.000000000000000000, 1.000000000000000000 ),
 .UNSPECIFIED. ) 
 GEOMETRIC_REPRESENTATION_ITEM ( )  RATIONAL_B_SPLINE_SURFACE ( (
 ( 1.000000000000000000, 0.7763623250684333899, 1.000000000000000000),
 ( 1.000000000000000000, 0.7763684247036575226, 1.000000000000000000),
 ( 1.000000000000000000, 0.7746454561795425020, 1.000000000000000000),
 ( 1.000000000000000000, 0.7679730451975060879, 1.000000000000000000),
 ( 1.000000000000000000, 0.7630177051941748889, 1.000000000000000000),
 ( 1.000000000000000000, 0.7504512394533247033, 1.000000000000000000),
 ( 1.000000000000000000, 0.7428408967923679773, 1.000000000000000000),
 ( 1.000000000000000000, 0.7259222650913751407, 1.000000000000000000),
 ( 1.000000000000000000, 0.7166207884817078488, 1.000000000000000000),
 ( 1.000000000000000000, 0.7071067811865879849, 1.000000000000000000) ) ) 
 REPRESENTATION_ITEM ( '' )  SURFACE ( )  );
#26487 = CARTESIAN_POINT ( 'NONE',  ( 13.88167667317130061, 1452.893272873260003, 224.0381707035730017 ) ) ;
#26486 = CARTESIAN_POINT ( 'NONE',  ( -1.430539319850000046, 1444.328264637789971, 199.1703804529689990 ) ) ;
#26488 = CARTESIAN_POINT ( 'NONE',  ( 16.21991559299999963, 1507.811519393530261, 231.6071110291980233 ) ) ;
#26489 = CARTESIAN_POINT ( 'NONE',  ( -0.1200844908460000082, 1507.645210318029967, 180.8332078508980203 ) ) ;
#26490 = CARTESIAN_POINT ( 'NONE',  ( 2.309279387819999751, 1467.303868143789941, 219.2083978630990089 ) ) ;
#26491 = FACE_OUTER_BOUND ( 'NONE', #84960, .T. ) ;
#26492 = EDGE_CURVE ( 'NONE', #11469, #78070, #82446, .T. ) ;
#26493 = FILL_AREA_STYLE_COLOUR ( '', #9015 ) ;
#26494 = CARTESIAN_POINT ( 'NONE',  ( 2.299014030735000436, 1516.811292230880099, 211.9858893885470081 ) ) ;
#26495 = CARTESIAN_POINT ( 'NONE',  ( 14.09832007171499946, 1415.595619977640126, 197.2198605877450177 ) ) ;
#26496 = CARTESIAN_POINT ( 'NONE',  ( -11.39395055920610034, 1422.323217934379954, 208.3944487261120173 ) ) ;
#26497 = CARTESIAN_POINT ( 'NONE',  ( 6.259132986314999592, 1514.370494773840164, 201.3780798503470066 ) ) ;
#26498 = VERTEX_POINT ( 'NONE', #16745 ) ;
#26499 = CARTESIAN_POINT ( 'NONE',  ( 13.77200850713100166, 1434.987125276089955, 148.8039589176320021 ) ) ;
#26500 = CARTESIAN_POINT ( 'NONE',  ( -0.5665393661006929982, 1432.061368030950007, 200.7215048253549980 ) ) ;
#26501 = ORIENTED_EDGE ( 'NONE', *, *, #33786, .F. ) ;
#26502 = VERTEX_POINT ( 'NONE', #109208 ) ;
#26503 = CARTESIAN_POINT ( 'NONE',  ( -7.951263648584999899, 1511.644799026709961, 215.1357399413169844 ) ) ;
#26504 = CARTESIAN_POINT ( 'NONE',  ( 16.19963472355905054, 1512.859148090011331, 197.8390203186946223 ) ) ;
#26505 = VECTOR ( 'NONE', #77432, 1000.000000000000114 ) ;
#26506 = CARTESIAN_POINT ( 'NONE',  ( -5.629143959155359589, 1407.138657505239962, 221.3608015446720003 ) ) ;
#26507 = CARTESIAN_POINT ( 'NONE',  ( -2.485205687335000135, 1517.181921232829836, 216.8478361320569832 ) ) ;
#26508 = CARTESIAN_POINT ( 'NONE',  ( 1.034685474009820139, 1465.654288377450257, 198.1561616953400176 ) ) ;
#26509 = CARTESIAN_POINT ( 'NONE',  ( 11.95411458668919913, 1421.865014672959887, 208.9185006178269930 ) ) ;
#26510 = CARTESIAN_POINT ( 'NONE',  ( -59.04611253552638317, 1379.721492120048424, 259.2250396778080699 ) ) ;
#26511 = CARTESIAN_POINT ( 'NONE',  ( 2.345806028950000233, 1465.851187384389959, 198.7475428451990069 ) ) ;
#26512 = EDGE_CURVE ( 'NONE', #63858, #11469, #43825, .T. ) ;
#26513 = CARTESIAN_POINT ( 'NONE',  ( -0.06540635796760001230, 1508.967893392429914, 238.8759467174980102 ) ) ;
#26514 = ORIENTED_EDGE ( 'NONE', *, *, #60175, .F. ) ;
#26515 = CARTESIAN_POINT ( 'NONE',  ( 4.995994787574999485, 1516.665179208830068, 206.6322283937570035 ) ) ;
#26516 = EDGE_LOOP ( 'NONE', ( #10809, #68060, #4365, #71040 ) ) ;
#26517 = CARTESIAN_POINT ( 'NONE',  ( 21.16084444640559781, 1440.913060387330006, 223.1877144379700155 ) ) ;
#26518 = CARTESIAN_POINT ( 'NONE',  ( -19.56461557969999987, 1509.492094407029981, 230.7210067600980210 ) ) ;
#26519 = EDGE_LOOP ( 'NONE', ( #94952, #77603, #101815, #78457 ) ) ;
#26520 = CARTESIAN_POINT ( 'NONE',  ( -5.513243736250649896, 1508.551565959790196, 201.9548213322269987 ) ) ;
#26521 = EDGE_CURVE ( 'NONE', #660, #59669, #109276, .T. ) ;
#26522 = CARTESIAN_POINT ( 'NONE',  ( -13.22111819830000101, 1410.747856120229926, 189.8101292799980229 ) ) ;
#26523 = CARTESIAN_POINT ( 'NONE',  ( 0.1595995995380000143, 1486.508831850330125, 181.8147405652979671 ) ) ;
#26525 = VERTEX_POINT ( 'NONE', #6723 ) ;
#26524 = CARTESIAN_POINT ( 'NONE',  ( 1.694839287372699843, 1423.343597660659952, 192.5785702911879866 ) ) ;
#26526 = CARTESIAN_POINT ( 'NONE',  ( 20.44315793190000008, 1427.648655133030161, 220.7419575218979730 ) ) ;
#26527 = CARTESIAN_POINT ( 'NONE',  ( -18.39846574424100112, 1508.551704408389924, 210.4158962701780240 ) ) ;
#26529 = CARTESIAN_POINT ( 'NONE',  ( -3.892685920502783059, 1515.551704408390833, 207.5713311529123644 ) ) ;
#26528 = AXIS2_PLACEMENT_3D ( 'NONE', #3038, #43907, #53998 ) ;
#26530 = CARTESIAN_POINT ( 'NONE',  ( 6.588066741534899684, 1432.346495030159986, 154.2384753665409960 ) ) ;
#26532 = CARTESIAN_POINT ( 'NONE',  ( 5.405732451549999595, 1434.707887834109897, 154.6595955769979867 ) ) ;
#26531 = CARTESIAN_POINT ( 'NONE',  ( -10.44087869485973030, 1517.051704408389924, 205.3524051900861593 ) ) ;
#26533 = CIRCLE ( 'NONE', #22906, 1.999999999999999556 ) ;
#26534 = CARTESIAN_POINT ( 'NONE',  ( 4.620008207075000151, 1516.777260590120022, 214.8964555921769772 ) ) ;
#26535 = AXIS2_PLACEMENT_3D ( 'NONE', #28097, #18569, #52764 ) ;
#26536 = CARTESIAN_POINT ( 'NONE',  ( -2.672560874067200221, 1429.102242977169908, 200.1400491528160046 ) ) ;
#26537 = DIRECTION ( 'NONE',  ( -0.7414773880254735827, -0.000000000000000000, -0.6709778558543652016 ) ) ;
#26538 = AXIS2_PLACEMENT_3D ( 'NONE', #25683, #50377, #110808 ) ;
#26539 = CARTESIAN_POINT ( 'NONE',  ( 30.17514886432845955, 1525.712830164893376, 221.2664250985396848 ) ) ;
#26540 = CARTESIAN_POINT ( 'NONE',  ( 2.494020282435000180, 1516.876240617270014, 211.4047611534970201 ) ) ;
#26541 = CARTESIAN_POINT ( 'NONE',  ( -11.83738977962950045, 1482.193131579070041, 207.9752198576520072 ) ) ;
#26542 = EDGE_CURVE ( 'NONE', #101005, #24504, #101297, .T. ) ;
#26543 = CARTESIAN_POINT ( 'NONE',  ( -16.95041357008780381, 1486.123329410929728, 187.6573714191846705 ) ) ;
#26544 = AXIS2_PLACEMENT_3D ( 'NONE', #8990, #43161, #34746 ) ;
#26546 = ORIENTED_EDGE ( 'NONE', *, *, #65359, .F. ) ;
#26545 = CARTESIAN_POINT ( 'NONE',  ( -84.12715333319998479, 1385.173288781940073, 288.0594686105589517 ) ) ;
#26547 = CARTESIAN_POINT ( 'NONE',  ( 13.01667709480000035, 1472.524070381529782, 262.4459321295979635 ) ) ;
#26548 = CARTESIAN_POINT ( 'NONE',  ( -33.91369265678890343, 1437.010538859309918, 136.5611844326260211 ) ) ;
#26549 = DIRECTION ( 'NONE',  ( -0.9510565162951561957, 0.000000000000000000, -0.3090169943749392911 ) ) ;
#26550 = CARTESIAN_POINT ( 'NONE',  ( -3.671418758874580135, 1507.725831406179850, 236.7601474078430215 ) ) ;
#26551 = LINE ( 'NONE', #1940, #55520 ) ;
#26553 = CARTESIAN_POINT ( 'NONE',  ( 17.60715780957560028, 1409.859378988159960, 222.6687402345539795 ) ) ;
#26552 = CARTESIAN_POINT ( 'NONE',  ( 11.87502394290000041, 1433.007271885549926, 149.9804723912980080 ) ) ;
#26554 = CARTESIAN_POINT ( 'NONE',  ( 12.68801083313210043, 1500.413651417279880, 208.6561539661539939 ) ) ;
#26555 = DIRECTION ( 'NONE',  ( -4.222254822704919979E-17, -1.000000000000000000, 7.728785610902649958E-17 ) ) ;
#26556 = VECTOR ( 'NONE', #84744, 1000.000000000000000 ) ;
#26557 = ORIENTED_EDGE ( 'NONE', *, *, #5896, .F. ) ;
#26558 = CARTESIAN_POINT ( 'NONE',  ( -0.7560907659159991079, 1516.770163853809890, 204.1215159365669933 ) ) ;
#26559 = CARTESIAN_POINT ( 'NONE',  ( 0.2161990375369999828, 1405.749718733130067, 267.5371521303979989 ) ) ;
#26560 = CARTESIAN_POINT ( 'NONE',  ( 27.76495483950000320, 1507.998797214829892, 207.7528748142179609 ) ) ;
#26561 = CARTESIAN_POINT ( 'NONE',  ( 24.67650857399999964, 1442.459111621740021, 212.6549697286179992 ) ) ;
#26562 = DIRECTION ( 'NONE',  ( 0.4794255386042031719, 0.000000000000000000, 0.8775825618903726477 ) ) ;
#26563 = CARTESIAN_POINT ( 'NONE',  ( -19.72258750869999844, 1466.915458833189859, 211.2872857108489768 ) ) ;
#26564 = CARTESIAN_POINT ( 'NONE',  ( 0.2178157486290130118, 1452.982786607829894, 183.2541296479709843 ) ) ;
#26565 = CARTESIAN_POINT ( 'NONE',  ( -27.30961438860000001, 1446.324487285050054, 137.1908813208980291 ) ) ;
#26566 = CARTESIAN_POINT ( 'NONE',  ( -12.59722456003193614, 1416.835288280216218, 194.8442844972019259 ) ) ;
#26567 = CARTESIAN_POINT ( 'NONE',  ( -109.8178621839999920, 1385.875214223179910, 297.0872587395590472 ) ) ;
#26568 = CARTESIAN_POINT ( 'NONE',  ( 11.31762420324339935, 1479.941427780220010, 210.0023256529900095 ) ) ;
#26569 = PLANE ( 'NONE',  #94824 ) ;
#26570 = CARTESIAN_POINT ( 'NONE',  ( -38.89645918617060971, 1452.470420418182130, 269.5913652274755918 ) ) ;
#26571 = ORIENTED_EDGE ( 'NONE', *, *, #50187, .T. ) ;
#26572 = CARTESIAN_POINT ( 'NONE',  ( 3.932775080253070321, 1448.980696629100066, 184.2693358254829832 ) ) ;
#26573 = FACE_OUTER_BOUND ( 'NONE', #84729, .T. ) ;
#26574 = CARTESIAN_POINT ( 'NONE',  ( 3.451256915079999654, 1486.991676997989771, 198.1002658732990085 ) ) ;
#26575 = DIRECTION ( 'NONE',  ( 0.000000000000000000, 1.000000000000000000, -1.836970198721029688E-16 ) ) ;
#26576 = CARTESIAN_POINT ( 'NONE',  ( -0.4034485627230000038, 1415.424111452130091, 233.4119044095980087 ) ) ;
#26578 = CARTESIAN_POINT ( 'NONE',  ( 31.81407709659792715, 1522.644714754857659, 196.2902540610638198 ) ) ;
#26577 = CARTESIAN_POINT ( 'NONE',  ( 12.70252038000000105, 1500.491347428390100, 208.9664825564809689 ) ) ;
#26579 = CARTESIAN_POINT ( 'NONE',  ( 23.84533589473599946, 1452.080362908450070, 136.9869410992479857 ) ) ;
#26580 = CARTESIAN_POINT ( 'NONE',  ( 8.405796631650000350, 1426.718801237130037, 211.2874662749189838 ) ) ;
#26581 = CARTESIAN_POINT ( 'NONE',  ( -15.36962477406189898, 1384.875951172459963, 219.5140789649539954 ) ) ;
#26582 = B_SPLINE_CURVE_WITH_KNOTS ( 'NONE', 3,
 ( #107123, #37722, #81912, #72985, #98167, #14157, #31510 ),
 .UNSPECIFIED., .F., .F.,
 ( 4, 3, 4 ),
 ( -157.7108139869999945, -101.4631973234740059, -30.86246212755040119 ),
 .UNSPECIFIED. ) ;
#26583 = DIRECTION ( 'NONE',  ( -5.980589973904019347E-17, 1.000000000000000000, -1.736889445713099699E-16 ) ) ;
#26584 = CARTESIAN_POINT ( 'NONE',  ( -18.64588652299999794, 1416.828040475229955, 208.5593769277110141 ) ) ;
#26585 = CARTESIAN_POINT ( 'NONE',  ( -17.84204394271100114, 1415.932840154009909, 209.4661953843999811 ) ) ;
#26586 = CARTESIAN_POINT ( 'NONE',  ( 24.94575029499999985, 1435.868986808510044, 137.3376222402980034 ) ) ;
#26587 = CARTESIAN_POINT ( 'NONE',  ( -13.28785892136501090, 1443.221467901020333, 169.3801346219540847 ) ) ;
#26588 = ORIENTED_EDGE ( 'NONE', *, *, #52749, .T. ) ;
#26589 = CARTESIAN_POINT ( 'NONE',  ( -16.34066499524799809, 1409.492051723080067, 225.1454641123489750 ) ) ;
#26590 = CARTESIAN_POINT ( 'NONE',  ( 4.946284671489999951, 1438.194204504490017, 150.2421849576980151 ) ) ;
#26591 = ORIENTED_EDGE ( 'NONE', *, *, #55688, .F. ) ;
#26592 = EDGE_LOOP ( 'NONE', ( #66242, #43434, #89191, #101674 ) ) ;
#26593 = CARTESIAN_POINT ( 'NONE',  ( 2.654812158838510072, 1435.276104861070053, 227.3789647914429963 ) ) ;
#26594 = DIRECTION ( 'NONE',  ( 0.03489949670250328678, -0.9993908270190956511, 0.000000000000000000 ) ) ;
#26596 = CARTESIAN_POINT ( 'NONE',  ( -1.042127096165949895, 1457.293139024839775, 219.7093524084000080 ) ) ;
#26595 = CARTESIAN_POINT ( 'NONE',  ( 10.67434751849999941, 1425.711863979930058, 92.68737539269790204 ) ) ;
#26597 = CARTESIAN_POINT ( 'NONE',  ( -2.494390017649999791, 1456.456026124890059, 202.8045864964890086 ) ) ;
#26598 = CARTESIAN_POINT ( 'NONE',  ( 4.158758314750929941, 1424.719666987580013, 185.0501326411299772 ) ) ;
#26599 = CARTESIAN_POINT ( 'NONE',  ( -2.805877869264751912, 1419.865265789671412, 186.1385795869015283 ) ) ;
#26600 = AXIS2_PLACEMENT_3D ( 'NONE', #110757, #104010, #95617 ) ;
#26601 = CARTESIAN_POINT ( 'NONE',  ( 7.465511834920000922, 1425.245174624619949, 212.3173831568290097 ) ) ;
#26602 = CARTESIAN_POINT ( 'NONE',  ( -17.66147422859999949, 1440.150478811289986, 218.7822781203190061 ) ) ;
#26603 = FACE_BOUND ( 'NONE', #31733, .T. ) ;
#26604 = CARTESIAN_POINT ( 'NONE',  ( -113.4000000000000057, 1376.122490972250034, 306.5935542023590301 ) ) ;
#26605 = CIRCLE ( 'NONE', #28379, 1.000000000000000000 ) ;
#26606 = CARTESIAN_POINT ( 'NONE',  ( 9.971295257839999593, 1364.502667329740007, 207.6218459616989946 ) ) ;
#26608 = ORIENTED_EDGE ( 'NONE', *, *, #74694, .T. ) ;
#26607 = CARTESIAN_POINT ( 'NONE',  ( 5.215576331900000362, 1455.428525482890109, 217.8852023316690065 ) ) ;
#26609 = VERTEX_POINT ( 'NONE', #34135 ) ;
#26610 = CARTESIAN_POINT ( 'NONE',  ( 1.376928043298433657, 1522.051704408389924, 191.7575736759021936 ) ) ;
#26611 = VECTOR ( 'NONE', #8910, 999.9999999999998863 ) ;
#26612 = CARTESIAN_POINT ( 'NONE',  ( -1.658081806242819971E-15, 1375.886883438980021, 209.1218459572589836 ) ) ;
#26613 = CARTESIAN_POINT ( 'NONE',  ( -0.9478952718030000391, 1471.581311749730048, 269.6149987492980244 ) ) ;
#26614 = CARTESIAN_POINT ( 'NONE',  ( 8.356958208356386919, 1500.521215832928192, 201.3523197060887355 ) ) ;
#26615 = CARTESIAN_POINT ( 'NONE',  ( -0.5359254698907657266, 1410.309918930317508, 185.0934049815310800 ) ) ;
#26616 = B_SPLINE_CURVE_WITH_KNOTS ( 'NONE', 3,
 ( #57791, #100846, #24138, #41525, #31453, #101386, #75683, #23042, #24681, #16282, #107621, #44286, #51579, #103052, #635, #61647, #67840, #17940, #25238, #101951, #34212, #78430, #60547, #34764, #35316, #27460, #51025, #9007, #94109, #86823, #95775, #76223, #25792, #1742, #93552, #68397, #42073, #110367, #19042, #17380, #85711, #53244, #85160, #33645, #9554, #7902, #59991, #26923, #8446 ),
 .UNSPECIFIED., .F., .F.,
 ( 4, 3, 3, 3, 3, 3, 3, 3, 3, 3, 3, 3, 3, 3, 3, 3, 4 ),
 ( -12.57638456940000005, -12.28317881101169995, -11.95680856207710008, -11.62570944449999999, -11.51472436910760067, -11.17721019327809984, -10.83638269496280060, -10.49376598039089892, -10.14927727062430129, -9.804494080932538935, -9.458815399652909406, -9.117616601314919578, -8.780289088742080139, -8.445887015311230428, -8.114782774053489689, -7.787209585589999428, -7.548674336869999557 ),
 .UNSPECIFIED. ) ;
#26617 = B_SPLINE_CURVE_WITH_KNOTS ( 'NONE', 4,
 ( #104919, #69126, #95961, #27110, #10290 ),
 .UNSPECIFIED., .F., .F.,
 ( 5, 5 ),
 ( 1.967616199060000071, 3.613988937050000239 ),
 .UNSPECIFIED. ) ;
#26618 = CARTESIAN_POINT ( 'NONE',  ( -31.31962774233543101, 1525.556090473913400, 201.5436825240319365 ) ) ;
#26619 = CARTESIAN_POINT ( 'NONE',  ( 2.297639806071400059, 1476.253136155009997, 197.8580381094499785 ) ) ;
#26620 = CARTESIAN_POINT ( 'NONE',  ( 22.57636543919999994, 1411.060965668830022, 206.4507511260079866 ) ) ;
#26621 = FILL_AREA_STYLE_COLOUR ( '', #35973 ) ;
#26622 = CARTESIAN_POINT ( 'NONE',  ( -2.500000000000000000, 1448.204674875420096, 169.9458606413490145 ) ) ;
#26623 = CARTESIAN_POINT ( 'NONE',  ( 7.445922712490000706, 1367.935115748530052, 207.6218459616989946 ) ) ;
#26624 = CARTESIAN_POINT ( 'NONE',  ( 13.39680589851269943, 1407.451641433219947, 204.6080239228549829 ) ) ;
#26625 = CARTESIAN_POINT ( 'NONE',  ( -11.94938536144059960, 1407.933938028119883, 269.6043413872750421 ) ) ;
#26626 = DIRECTION ( 'NONE',  ( -1.836970198721024757E-16, -1.000000000000000000, -1.001483571081361959E-32 ) ) ;
#26627 = VERTEX_POINT ( 'NONE', #74509 ) ;
#26628 = CARTESIAN_POINT ( 'NONE',  ( 4.124127541549999165, 1440.791920158089852, 218.1322488136489994 ) ) ;
#26629 = CARTESIAN_POINT ( 'NONE',  ( 13.39080007399999950, 1444.566365729019935, 188.1636725064979885 ) ) ;
#26630 = ORIENTED_EDGE ( 'NONE', *, *, #81750, .F. ) ;
#26631 = EDGE_LOOP ( 'NONE', ( #77997, #64018, #102082 ) ) ;
#26632 = CARTESIAN_POINT ( 'NONE',  ( 0.000000000000000000, 1522.051704408389924, 232.8211094035767985 ) ) ;
#26633 = CARTESIAN_POINT ( 'NONE',  ( -0.7618909056700008398, 1360.403425203260213, 207.6218459616989946 ) ) ;
#26634 = AXIS2_PLACEMENT_3D ( 'NONE', #21400, #13552, #104462 ) ;
#26635 = CARTESIAN_POINT ( 'NONE',  ( -5.773668852974999766, 1516.734985836460055, 213.1604834329569940 ) ) ;
#26636 = CARTESIAN_POINT ( 'NONE',  ( -18.73391074110000076, 1470.474872498130026, 190.1492551849979975 ) ) ;
#26637 = ORIENTED_EDGE ( 'NONE', *, *, #9071, .T. ) ;
#26638 = CARTESIAN_POINT ( 'NONE',  ( -105.7600638790000005, 1375.390212577269949, 302.0293825393590055 ) ) ;
#26639 = CARTESIAN_POINT ( 'NONE',  ( -107.0376884417929944, 1378.913060387299993, 301.1156876987260489 ) ) ;
#26640 = CARTESIAN_POINT ( 'NONE',  ( 6.937965660314999283, 1516.732530461250008, 204.1161457306970135 ) ) ;
#26641 = CARTESIAN_POINT ( 'NONE',  ( -29.25495334789999902, 1509.872415968630094, 208.6412278715359889 ) ) ;
#26642 = DIRECTION ( 'NONE',  ( -0.000000000000000000, -1.000000000000000000, -0.000000000000000000 ) ) ;
#26643 = CARTESIAN_POINT ( 'NONE',  ( -79.49732243889999950, 1384.913765794120081, 282.9461888724590040 ) ) ;
#26644 = CARTESIAN_POINT ( 'NONE',  ( -65.40151035413138914, 1384.707520014439979, 255.9531160123350162 ) ) ;
#26645 = CARTESIAN_POINT ( 'NONE',  ( -3.897582650600000420, 1407.987767143230258, 196.4241821881980172 ) ) ;
#26646 = CARTESIAN_POINT ( 'NONE',  ( -12.66827423740000036, 1410.284634327829963, 227.9748965595980223 ) ) ;
#26648 = ORIENTED_EDGE ( 'NONE', *, *, #96767, .T. ) ;
#26647 = CARTESIAN_POINT ( 'NONE',  ( -12.29575548589999912, 1445.147284857479917, 186.2458214697980168 ) ) ;
#26649 = DIRECTION ( 'NONE',  ( -1.755985294532469921E-16, 1.000000000000000000, -1.338183447452831989E-16 ) ) ;
#26650 = CARTESIAN_POINT ( 'NONE',  ( 25.81147510750000151, 1488.682669033129741, 215.7372411931079910 ) ) ;
#26651 = CARTESIAN_POINT ( 'NONE',  ( -0.4403324739431219714, 1517.051704035390003, 216.6089087266339845 ) ) ;
#26652 = CARTESIAN_POINT ( 'NONE',  ( -24.82487920160000172, 1435.549279665109907, 136.8315248583980122 ) ) ;
#26653 = CARTESIAN_POINT ( 'NONE',  ( 2.492443650904999863, 1516.793978928989873, 212.3737347995770222 ) ) ;
#26654 = CIRCLE ( 'NONE', #37389, 23.05825808840000946 ) ;
#26655 = CARTESIAN_POINT ( 'NONE',  ( -68.74622153960000048, 1379.747865581630094, 280.1024420339589938 ) ) ;
#26656 = DIRECTION ( 'NONE',  ( 0.000000000000000000, 1.000000000000000000, 0.000000000000000000 ) ) ;
#26657 = CARTESIAN_POINT ( 'NONE',  ( 13.01048185389249845, 1478.887107457059983, 225.7213801538089797 ) ) ;
#26658 = CARTESIAN_POINT ( 'NONE',  ( -2.493697079054999932, 1516.977201124959947, 208.0034927161370035 ) ) ;
#26659 = ORIENTED_EDGE ( 'NONE', *, *, #34974, .T. ) ;
#26660 = DIRECTION ( 'NONE',  ( 0.7470743985697100298, 0.03252369126397396115, -0.6639443143127832236 ) ) ;
#26661 = CARTESIAN_POINT ( 'NONE',  ( -1.927358540839999801, 1410.305851446330053, 232.8221572591980078 ) ) ;
#26662 = CARTESIAN_POINT ( 'NONE',  ( -22.68195036590000058, 1384.853989887049920, 222.0405270882590116 ) ) ;
#26663 = ORIENTED_EDGE ( 'NONE', *, *, #94626, .T. ) ;
#26664 = CARTESIAN_POINT ( 'NONE',  ( -13.67877973650669965, 1385.299323577030009, 219.1660709978279726 ) ) ;
#26665 = AXIS2_PLACEMENT_3D ( 'NONE', #88024, #70690, #22270 ) ;
#26666 = CARTESIAN_POINT ( 'NONE',  ( -9.209823531518070538, 1493.295436042139954, 200.9664195331480130 ) ) ;
#26667 = CARTESIAN_POINT ( 'NONE',  ( 12.21725359463179927, 1434.113778757119917, 149.7882389495470079 ) ) ;
#26668 = B_SPLINE_SURFACE_WITH_KNOTS ( 'NONE', 5, 1, ( 
 ( #15731, #42627 ),
 ( #101394, #59999 ),
 ( #82974, #50493 ),
 ( #58884, #34220 ),
 ( #33113, #33654 ),
 ( #76779, #97 ),
 ( #108727, #6267 ),
 ( #100326, #93017 ),
 ( #16289, #25801 ) ),
 .UNSPECIFIED., .F., .F., .F.,
 ( 6, 3, 6 ),
 ( 2, 2 ),
 ( 0.000000000000000000, 3.291079314230000108, 6.557401248809999750 ),
 ( 0.000000000000000000, 14.00000000000000000 ),
 .UNSPECIFIED. ) ;
#26669 = CARTESIAN_POINT ( 'NONE',  ( 14.40204153438889989, 1488.406232492609888, 231.6322952228059933 ) ) ;
#26670 = CARTESIAN_POINT ( 'NONE',  ( -22.14848624618590023, 1507.850251992550056, 225.9298071555170111 ) ) ;
#26671 = CARTESIAN_POINT ( 'NONE',  ( -1.682318697039999922, 1409.475163255830012, 186.2035163265980202 ) ) ;
#26672 = CARTESIAN_POINT ( 'NONE',  ( 2.175409717514719593E-31, 1397.551704408390151, 209.1218459616989946 ) ) ;
#26673 = LINE ( 'NONE', #60301, #102339 ) ;
#26674 = EDGE_CURVE ( 'NONE', #94444, #15354, #6571, .T. ) ;
#26676 = CARTESIAN_POINT ( 'NONE',  ( -4.649633098669999853, 1420.176632532630038, 186.4708447736979906 ) ) ;
#26675 = CARTESIAN_POINT ( 'NONE',  ( -2.869693497065000098, 1517.070197312179971, 214.9093229647470196 ) ) ;
#26677 = CARTESIAN_POINT ( 'NONE',  ( 20.05348425099999687, 1509.507670995530134, 187.8272102738980038 ) ) ;
#26678 = FACE_OUTER_BOUND ( 'NONE', #88514, .T. ) ;
#26679 = ORIENTED_EDGE ( 'NONE', *, *, #26212, .T. ) ;
#26680 = CARTESIAN_POINT ( 'NONE',  ( 2.872836622524999939, 1517.158319634930194, 201.3964737998670103 ) ) ;
#26681 = CARTESIAN_POINT ( 'NONE',  ( -6.240097849340000558, 1499.713794654230014, 181.2208793725980058 ) ) ;
#26682 = ORIENTED_EDGE ( 'NONE', *, *, #15394, .F. ) ;
#26683 = AXIS2_PLACEMENT_3D ( 'NONE', #60576, #661, #78458 ) ;
#26684 = CARTESIAN_POINT ( 'NONE',  ( 4.123035148590000531, 1421.670590998829766, 184.9173806918979892 ) ) ;
#26685 = AXIS2_PLACEMENT_3D ( 'NONE', #18588, #28115, #95327 ) ;
#26686 =( NAMED_UNIT ( * ) PLANE_ANGLE_UNIT ( ) SI_UNIT ( $, .RADIAN. ) );
#26687 = CARTESIAN_POINT ( 'NONE',  ( 8.720950440807788695, 1511.461696079649982, 203.5356427006819899 ) ) ;
#26688 = UNCERTAINTY_MEASURE_WITH_UNIT (LENGTH_MEASURE( 1.000000000000000082E-05 ), #110698, 'distance_accuracy_value', 'NONE');
#26689 = CARTESIAN_POINT ( 'NONE',  ( 3.114546081289999435, 1442.643943093889902, 217.4397813744189989 ) ) ;
#26690 = CARTESIAN_POINT ( 'NONE',  ( -32.59719044532482002, 1523.982201850120191, 201.1951351303495414 ) ) ;
#26691 = CARTESIAN_POINT ( 'NONE',  ( -16.66101146819999812, 1410.867390116229899, 191.7375337716979971 ) ) ;
#26692 = CARTESIAN_POINT ( 'NONE',  ( 18.62061618460000290, 1416.021639796329964, 209.9108522146810003 ) ) ;
#26693 = CARTESIAN_POINT ( 'NONE',  ( -3.159798962964550206, 1454.349606548080146, 199.1257215370219740 ) ) ;
#26694 = CARTESIAN_POINT ( 'NONE',  ( 9.611936100793599280, 1460.529534319539835, 206.0552085173229955 ) ) ;
#26695 = CARTESIAN_POINT ( 'NONE',  ( -7.467133905529999893, 1443.913060387330006, 149.7989312978980081 ) ) ;
#26696 = CARTESIAN_POINT ( 'NONE',  ( -1.757532416683340148, 1451.933574871519795, 184.1885909450070073 ) ) ;
#26698 = CARTESIAN_POINT ( 'NONE',  ( 4.328976357965480304, 1515.082833801169954, 207.7712354839940190 ) ) ;
#26697 = CARTESIAN_POINT ( 'NONE',  ( -15.17668789299639975, 1418.088918213290071, 203.1695124900660119 ) ) ;
#26699 = DIRECTION ( 'NONE',  ( 0.000000000000000000, 0.000000000000000000, -1.000000000000000000 ) ) ;
#26700 = ORIENTED_EDGE ( 'NONE', *, *, #75300, .F. ) ;
#26701 = CARTESIAN_POINT ( 'NONE',  ( -8.282452265539999914, 1508.539485426189913, 219.0858899887390123 ) ) ;
#26702 = CARTESIAN_POINT ( 'NONE',  ( -4.832611339330879829, 1508.551704408389924, 211.6097681392950278 ) ) ;
#26703 = CARTESIAN_POINT ( 'NONE',  ( -11.87899307332345522, 1433.117273378820073, 149.9761472051002329 ) ) ;
#26704 = CARTESIAN_POINT ( 'NONE',  ( 11.89856584206491874, 1410.698127348937987, 189.7512122486814974 ) ) ;
#26705 = AXIS2_PLACEMENT_3D ( 'NONE', #36604, #1356, #35496 ) ;
#26706 = DIRECTION ( 'NONE',  ( 0.000000000000000000, 0.000000000000000000, -1.000000000000000000 ) ) ;
#26707 = B_SPLINE_SURFACE_WITH_KNOTS ( 'NONE', 5, 5, ( 
 ( #97269, #63167, #28979, #105131, #88878, #88329 ),
 ( #12163, #36820, #3801, #62620, #37931, #72113 ),
 ( #71010, #27309, #26753, #28422, #87222, #78830 ),
 ( #60941, #61490, #78262, #79932, #18337, #95619 ),
 ( #18886, #96738, #53084, #10512, #2141, #20008 ),
 ( #54203, #46900, #99458, #47978, #65898, #31712 ) ),
 .UNSPECIFIED., .F., .F., .F.,
 ( 6, 6 ),
 ( 6, 6 ),
 ( 19.64510849129999670, 96.65569525989999988 ),
 ( -2.775557561569999727E-17, 1.000000000000000000 ),
 .UNSPECIFIED. ) ;
#26708 = CARTESIAN_POINT ( 'NONE',  ( 9.638115859579080791, 1516.551188146539971, 214.4931927712729873 ) ) ;
#26709 = B_SPLINE_CURVE_WITH_KNOTS ( 'NONE', 5,
 ( #26828, #54265, #95140, #52599, #86735, #27934, #10025, #62117, #63229 ),
 .UNSPECIFIED., .F., .F.,
 ( 6, 3, 6 ),
 ( 0.000000000000000000, 0.3434076321145757560, 1.000000000000000000 ),
 .UNSPECIFIED. ) ;
#26710 = CARTESIAN_POINT ( 'NONE',  ( -11.35534575645690047, 1470.545164360740046, 210.1099061434680095 ) ) ;
#26711 = CARTESIAN_POINT ( 'NONE',  ( -4.069166842042879928, 1487.126672562190151, 220.0157357502849891 ) ) ;
#26712 = CARTESIAN_POINT ( 'NONE',  ( -13.97983671313290088, 1420.196096071459806, 195.9955716203340046 ) ) ;
#26713 = CARTESIAN_POINT ( 'NONE',  ( -67.60195043141951032, 1383.787634321580072, 291.9320215662019677 ) ) ;
#26714 = EDGE_CURVE ( 'NONE', #103179, #59173, #6439, .T. ) ;
#26715 = EDGE_CURVE ( 'NONE', #40553, #62944, #33023, .T. ) ;
#26716 = CARTESIAN_POINT ( 'NONE',  ( 21.14467612950000230, 1450.943517307629918, 144.6008493241980091 ) ) ;
#26717 = CARTESIAN_POINT ( 'NONE',  ( -106.4016663176860078, 1391.913060387289988, 304.1497498221540354 ) ) ;
#26718 = CARTESIAN_POINT ( 'NONE',  ( -1.336491736407680042, 1516.593294715569982, 201.4112694980950096 ) ) ;
#26719 = ADVANCED_FACE ( 'NONE', ( #101308 ), #18027, .F. ) ;
#26721 = ORIENTED_EDGE ( 'NONE', *, *, #107775, .T. ) ;
#26720 = CARTESIAN_POINT ( 'NONE',  ( 23.36488590689999967, 1508.462599307330038, 194.4514040896980021 ) ) ;
#26722 = CARTESIAN_POINT ( 'NONE',  ( -1.442946131772449903, 1414.913527292460003, 226.2142476967059963 ) ) ;
#26723 = VECTOR ( 'NONE', #19019, 1000.000000000000000 ) ;
#26724 = CARTESIAN_POINT ( 'NONE',  ( -83.23303318460000355, 1380.073362198620089, 301.6916257618590294 ) ) ;
#26725 = EDGE_CURVE ( 'NONE', #63057, #37652, #107867, .T. ) ;
#26726 = CARTESIAN_POINT ( 'NONE',  ( -14.65245215464970130, 1420.119839417710182, 213.8659310620899987 ) ) ;
#26727 = ORIENTED_EDGE ( 'NONE', *, *, #66731, .F. ) ;
#26728 = ORIENTED_EDGE ( 'NONE', *, *, #21887, .F. ) ;
#26729 = EDGE_CURVE ( 'NONE', #78872, #28184, #15367, .T. ) ;
#26730 = CARTESIAN_POINT ( 'NONE',  ( 18.10666025242040078, 1508.254734886140113, 230.4759121335879968 ) ) ;
#26731 = CARTESIAN_POINT ( 'NONE',  ( -6.223685729618609663, 1459.529526055099950, 211.3909926741320078 ) ) ;
#26732 = CYLINDRICAL_SURFACE ( 'NONE', #37261, 1.000000000000000888 ) ;
#26734 = CARTESIAN_POINT ( 'NONE',  ( 4.626199203489999690, 1486.054098565890172, 218.8608866932789851 ) ) ;
#26733 = CARTESIAN_POINT ( 'NONE',  ( 22.18308977499999912, 1506.802866779730039, 209.2929401371579843 ) ) ;
#26735 = CARTESIAN_POINT ( 'NONE',  ( 9.362162057066138132, 1436.138703257420048, 210.0625319500269939 ) ) ;
#26736 = CARTESIAN_POINT ( 'NONE',  ( -108.7852627620000021, 1383.811234508949838, 297.2705451043590301 ) ) ;
#26737 = CARTESIAN_POINT ( 'NONE',  ( -11.46423977836468744, 1434.765458290011566, 151.4552492457040387 ) ) ;
#26738 = FACE_OUTER_BOUND ( 'NONE', #88812, .T. ) ;
#26739 = CARTESIAN_POINT ( 'NONE',  ( 2.651685169959999921, 1409.005659273929950, 187.1129167388979795 ) ) ;
#26740 = CARTESIAN_POINT ( 'NONE',  ( -1.708234279288180169, 1485.711368808090128, 197.3465205308800137 ) ) ;
#26741 = CARTESIAN_POINT ( 'NONE',  ( -10.15459880809999937, 1436.277525070270030, 152.4140741291979850 ) ) ;
#26742 = CARTESIAN_POINT ( 'NONE',  ( 12.03552245250000041, 1436.199553546779953, 151.3007240698979956 ) ) ;
#26743 = DIRECTION ( 'NONE',  ( 0.000000000000000000, 0.000000000000000000, -1.000000000000000000 ) ) ;
#26744 = CARTESIAN_POINT ( 'NONE',  ( -14.75483871110000145, 1452.397810064229816, 149.0856641680979919 ) ) ;
#26745 = CARTESIAN_POINT ( 'NONE',  ( -15.69795926999090163, 1517.151704408390060, 195.4758181584410011 ) ) ;
#26746 = VERTEX_POINT ( 'NONE', #85405 ) ;
#26747 = CARTESIAN_POINT ( 'NONE',  ( -3.137381254594690194, 1508.729448404669938, 213.6787528672270184 ) ) ;
#26748 = CARTESIAN_POINT ( 'NONE',  ( 11.18657871290000116, 1480.479923154690141, 229.7819052381989877 ) ) ;
#26750 = ADVANCED_FACE ( 'NONE', ( #103304 ), #81466, .T. ) ;
#26749 = CARTESIAN_POINT ( 'NONE',  ( -40.84706851859999688, 1449.487018346279910, 269.8579372096979796 ) ) ;
#26751 = CARTESIAN_POINT ( 'NONE',  ( -1.906499846882070084E-08, 1517.051704408389924, 209.1218459511669892 ) ) ;
#26752 = CARTESIAN_POINT ( 'NONE',  ( 17.72823807780000038, 1410.893857103729943, 223.4207927510979914 ) ) ;
#26753 = CARTESIAN_POINT ( 'NONE',  ( -14.98670476610000080, 1485.045873338330011, 224.0415272780979876 ) ) ;
#26754 = AXIS2_PLACEMENT_3D ( 'NONE', #91162, #75490, #48634 ) ;
#26755 = CARTESIAN_POINT ( 'NONE',  ( -110.0631843759950499, 1384.903000323588458, 296.9512581633061359 ) ) ;
#26756 = CARTESIAN_POINT ( 'NONE',  ( 2.926868927680989607, 1410.230421244640183, 231.6146595459809987 ) ) ;
#26757 = CARTESIAN_POINT ( 'NONE',  ( -2.057188004130400039, 1421.133947679400080, 193.7687826666459898 ) ) ;
#26758 = CARTESIAN_POINT ( 'NONE',  ( -8.361365488320000594, 1417.261522080730174, 230.7875359346980133 ) ) ;
#26759 = ADVANCED_FACE ( 'NONE', ( #34474 ), #43988, .F. ) ;
#26760 = CARTESIAN_POINT ( 'NONE',  ( 0.03708545786814630707, 1486.336401889381705, 181.8124888147413003 ) ) ;
#26761 = CARTESIAN_POINT ( 'NONE',  ( 4.262353028419999745, 1360.811275533920025, 207.6218459616989946 ) ) ;
#26762 = CARTESIAN_POINT ( 'NONE',  ( -45.97629855748849792, 1437.677199724009824, 266.9778860158930343 ) ) ;
#26763 = CARTESIAN_POINT ( 'NONE',  ( -19.02974267272307074, 1517.151704408390060, 207.1627782414018100 ) ) ;
#26764 = CIRCLE ( 'NONE', #53657, 1.000000000000003775 ) ;
#26765 = VERTEX_POINT ( 'NONE', #68649 ) ;
#26766 = CARTESIAN_POINT ( 'NONE',  ( -8.042714958110000367, 1424.476437214510042, 210.0061173360819851 ) ) ;
#26767 = EDGE_CURVE ( 'NONE', #77078, #46740, #103881, .T. ) ;
#26768 = EDGE_LOOP ( 'NONE', ( #9273, #70770, #48939, #13320 ) ) ;
#26769 = CARTESIAN_POINT ( 'NONE',  ( 5.788691325514999875, 1517.157901477309906, 210.2449475486469908 ) ) ;
#26770 = DIRECTION ( 'NONE',  ( -0.9455185755993178454, 0.000000000000000000, 0.3255681544571539243 ) ) ;
#26771 = CARTESIAN_POINT ( 'NONE',  ( -1.636741614903409969, 1469.777368438049962, 219.0527109355280118 ) ) ;
#26772 = CARTESIAN_POINT ( 'NONE',  ( 7.538868782738779473, 1425.612187812159846, 212.1827042067879745 ) ) ;
#26773 = CIRCLE ( 'NONE', #85758, 0.9999999999999987788 ) ;
#26774 = CARTESIAN_POINT ( 'NONE',  ( -27.03107691188749939, 1451.712358130050006, 135.7978697014619911 ) ) ;
#26775 = VERTEX_POINT ( 'NONE', #102219 ) ;
#26776 = CARTESIAN_POINT ( 'NONE',  ( -13.34233688319999978, 1434.814457747640063, 195.5472743009979979 ) ) ;
#26778 = CARTESIAN_POINT ( 'NONE',  ( -14.98757063811820167, 1513.799047786500068, 223.8171003904659813 ) ) ;
#26777 = CARTESIAN_POINT ( 'NONE',  ( -2.410659749415533071, 1525.163457223744217, 176.1169438982480244 ) ) ;
#26779 = CARTESIAN_POINT ( 'NONE',  ( 3.584503077415259753, 1486.500511906220027, 219.3043361390229791 ) ) ;
#26780 = CARTESIAN_POINT ( 'NONE',  ( -18.80034332280520104, 1508.551704409080230, 209.8506955288309825 ) ) ;
#26781 = CARTESIAN_POINT ( 'NONE',  ( 2.761692215590000110, 1460.406946357790048, 228.5031849494990013 ) ) ;
#26782 = CARTESIAN_POINT ( 'NONE',  ( -8.552145378091630334, 1438.550163890339945, 207.4884571577819941 ) ) ;
#26783 = ORIENTED_EDGE ( 'NONE', *, *, #103754, .F. ) ;
#26784 = CARTESIAN_POINT ( 'NONE',  ( -6.798292825562660013, 1408.601192976899711, 270.3857984775779641 ) ) ;
#26785 = CARTESIAN_POINT ( 'NONE',  ( -3.267039729984999585, 1517.012231669750008, 208.3862772893259887 ) ) ;
#26786 = CARTESIAN_POINT ( 'NONE',  ( 12.35539357289999884, 1419.606906044829884, 229.3575800037980059 ) ) ;
#26787 = CARTESIAN_POINT ( 'NONE',  ( -6.036759191025518057, 1509.035273823006037, 216.5824821671302800 ) ) ;
#26789 = EDGE_LOOP ( 'NONE', ( #22728, #60599, #58584, #69532 ) ) ;
#26788 = CARTESIAN_POINT ( 'NONE',  ( -8.436812995028324380, 1365.738857087742417, 210.6218459617142003 ) ) ;
#26790 = ORIENTED_EDGE ( 'NONE', *, *, #49368, .F. ) ;
#26791 = CARTESIAN_POINT ( 'NONE',  ( -22.70631399555909979, 1409.706076165010018, 209.4577935351849760 ) ) ;
#26792 = CARTESIAN_POINT ( 'NONE',  ( -10.48474110849999974, 1480.275079708390194, 208.2232256045050178 ) ) ;
#26793 = CARTESIAN_POINT ( 'NONE',  ( 3.675435886750538117, 1425.136160367158254, 185.0298737722915519 ) ) ;
#26794 = CIRCLE ( 'NONE', #100087, 1.999999999920172522 ) ;
#26795 = DIRECTION ( 'NONE',  ( 0.000000000000000000, 0.000000000000000000, 1.000000000000000000 ) ) ;
#26796 = CARTESIAN_POINT ( 'NONE',  ( -18.89905695062199698, 1416.828039266840278, 207.5749027128360069 ) ) ;
#26797 = CARTESIAN_POINT ( 'NONE',  ( -20.02836947109999954, 1430.790674585230136, 222.8465340271980040 ) ) ;
#26798 = PRODUCT_RELATED_PRODUCT_CATEGORY ( 'part', '', ( #14279 ) ) ;
#26799 = CARTESIAN_POINT ( 'NONE',  ( 22.59632237563830159, 1471.921777372659790, 267.3281857808220252 ) ) ;
#26800 = CARTESIAN_POINT ( 'NONE',  ( -11.58386370990380065, 1391.913060387200176, 208.1431450511909986 ) ) ;
#26801 = CARTESIAN_POINT ( 'NONE',  ( -16.26336930940977510, 1421.047042384238921, 227.0220306831831181 ) ) ;
#26802 = CARTESIAN_POINT ( 'NONE',  ( 3.253141137235000091, 1516.858171774179937, 205.8542424163969997 ) ) ;
#26803 = ORIENTED_EDGE ( 'NONE', *, *, #27666, .T. ) ;
#26804 = CARTESIAN_POINT ( 'NONE',  ( 17.99954443082109989, 1410.904693892220166, 222.9872220945560173 ) ) ;
#26805 = CARTESIAN_POINT ( 'NONE',  ( -3.879787126964284294, 1516.685805519419546, 202.7020868552936292 ) ) ;
#26806 = CARTESIAN_POINT ( 'NONE',  ( 22.73795006019999931, 1409.715685400830125, 208.6721383975130095 ) ) ;
#26807 = ORIENTED_EDGE ( 'NONE', *, *, #78822, .F. ) ;
#26809 = AXIS2_PLACEMENT_3D ( 'NONE', #34881, #50048, #103170 ) ;
#26808 = CARTESIAN_POINT ( 'NONE',  ( 4.679791067032149421, 1508.610720099250102, 205.9457795546310024 ) ) ;
#26810 = CARTESIAN_POINT ( 'NONE',  ( 25.71786717807909994, 1451.999026050069915, 135.3980030440489770 ) ) ;
#26811 = CARTESIAN_POINT ( 'NONE',  ( 2.487935123032369411, 1508.909942010395071, 204.6312267424608820 ) ) ;
#26812 = CARTESIAN_POINT ( 'NONE',  ( -15.80299171769999944, 1389.615364110129804, 203.8617420411390242 ) ) ;
#26813 = CARTESIAN_POINT ( 'NONE',  ( -18.64442766462446244, 1507.939506224431170, 229.7217055948968891 ) ) ;
#26815 = B_SPLINE_SURFACE_WITH_KNOTS ( 'NONE', 5, 5, ( 
 ( #70911, #69236, #87117, #19341, #103917, #17673, #11523, #19902, #60846 ),
 ( #27216, #69799, #44578, #18788, #96632, #96068, #94393, #52985, #86012 ),
 ( #54103, #94971, #2592, #44024, #10408, #53541, #88232, #102789, #26085 ),
 ( #60275, #9856, #78723, #51876, #105026, #931, #2038, #36171, #3144 ),
 ( #70355, #78160, #35055, #1472, #27763, #87688, #68682, #10969, #77619 ),
 ( #45142, #103345, #26647, #36718, #18239, #28319, #62510, #52434, #86560 ) ),
 .UNSPECIFIED., .F., .F., .F.,
 ( 6, 6 ),
 ( 6, 3, 6 ),
 ( 6.655359042069999731, 17.59398672700000077 ),
 ( 0.000000000000000000, 1.000000000000000000, 2.000000000000000000 ),
 .UNSPECIFIED. ) ;
#26814 = CARTESIAN_POINT ( 'NONE',  ( 17.43919469369999931, 1409.522050485830050, 194.4592152026980045 ) ) ;
#26816 = CARTESIAN_POINT ( 'NONE',  ( 13.31869796660000027, 1444.740067931809790, 169.3753098992980028 ) ) ;
#26817 = CARTESIAN_POINT ( 'NONE',  ( 2.654237714975077100, 1439.650388619271325, 183.5414635488324961 ) ) ;
#26819 = CARTESIAN_POINT ( 'NONE',  ( -22.62148864339994958, 1431.812645719854345, 216.1894225434491830 ) ) ;
#26818 = CARTESIAN_POINT ( 'NONE',  ( 30.41976661596575937, 1524.374142163904025, 196.3903116790124841 ) ) ;
#26820 = CARTESIAN_POINT ( 'NONE',  ( -15.36549427709999982, 1420.352425059129928, 229.0210324418980008 ) ) ;
#26821 = EDGE_CURVE ( 'NONE', #8701, #36205, #33201, .T. ) ;
#26822 = DIRECTION ( 'NONE',  ( 0.01559025466217519272, 0.9998783227618376346, 0.0005325697541269488111 ) ) ;
#26823 = CARTESIAN_POINT ( 'NONE',  ( -10.31524791190000023, 1382.179600870839977, 217.6122790885089842 ) ) ;
#26824 = EDGE_CURVE ( 'NONE', #49383, #93417, #30530, .T. ) ;
#26825 = CARTESIAN_POINT ( 'NONE',  ( 1.133516965105000107, 1516.713079096360161, 213.7319258036569920 ) ) ;
#26826 = CARTESIAN_POINT ( 'NONE',  ( -10.47043688597563005, 1517.151704408390060, 221.2386401010601844 ) ) ;
#26827 = ORIENTED_EDGE ( 'NONE', *, *, #74806, .T. ) ;
#26828 = CARTESIAN_POINT ( 'NONE',  ( -4.794426340529999386, 1463.608615258990085, 228.2108236244990280 ) ) ;
#26829 = CARTESIAN_POINT ( 'NONE',  ( -22.74803453391424668, 1523.678648413191695, 234.5603111028700027 ) ) ;
#26830 = CARTESIAN_POINT ( 'NONE',  ( -0.5126689071185190905, 1409.979044830439989, 233.1189724269549970 ) ) ;
#26831 = CARTESIAN_POINT ( 'NONE',  ( -20.16530468839962609, 1508.094484761909825, 209.6061611864197687 ) ) ;
#26832 =( BOUNDED_CURVE ( )  B_SPLINE_CURVE ( 3, ( #101446, #108219, #41581, #6316 ),
 .UNSPECIFIED., .F., .F. ) 
 B_SPLINE_CURVE_WITH_KNOTS ( ( 4, 4 ),
 ( 2.354951092798057921, 3.925058725375623947 ),
 .UNSPECIFIED. ) 
 CURVE ( )  GEOMETRIC_REPRESENTATION_ITEM ( )  RATIONAL_B_SPLINE_CURVE ( ( 1.000000000000000000, 0.8049001529565240620, 0.8049001529565240620, 1.000000000000000000 ) ) 
 REPRESENTATION_ITEM ( '' )  );
#26833 = CARTESIAN_POINT ( 'NONE',  ( 1.089943175529721975, 1421.340729913779114, 193.7538244426485790 ) ) ;
#26834 = CARTESIAN_POINT ( 'NONE',  ( -10.76760958711749971, 1462.889620211719830, 206.6132149273230141 ) ) ;
#26835 = CARTESIAN_POINT ( 'NONE',  ( -23.42675388609999843, 1440.913060387330006, 234.3916895593979746 ) ) ;
#26836 = VECTOR ( 'NONE', #5553, 1000.000000000000114 ) ;
#26837 = EDGE_CURVE ( 'NONE', #11116, #18619, #22355, .T. ) ;
#26838 = CARTESIAN_POINT ( 'NONE',  ( 22.48842373632798797, 1471.669969102955292, 266.7673555805813521 ) ) ;
#26839 = CARTESIAN_POINT ( 'NONE',  ( 11.60789637760000126, 1433.302712684209837, 151.0870278953979948 ) ) ;
#26840 = CARTESIAN_POINT ( 'NONE',  ( 19.62446893450000118, 1443.054186837139923, 214.3676144203579952 ) ) ;
#26841 = B_SPLINE_SURFACE_WITH_KNOTS ( 'NONE', 5, 5, ( 
 ( #34040, #100682, #23965, #82790, #23430, #32396 ),
 ( #15013, #84980, #16654, #42439, #41895, #83339 ),
 ( #91739, #58708, #50322, #84448, #92290, #6635 ),
 ( #74967, #15560, #25624, #100144, #59270, #49761 ),
 ( #93388, #76598, #83890, #24518, #7734, #68231 ),
 ( #59815, #6084, #76052, #66577, #14472, #48664 ),
 ( #40236, #41353, #75520, #74419, #109654, #108545 ),
 ( #31836, #86649, #78815, #104002, #26177, #86103 ),
 ( #51397, #60930, #9944, #102879, #78251, #1020 ) ),
 .UNSPECIFIED., .F., .F., .F.,
 ( 6, 3, 6 ),
 ( 6, 6 ),
 ( 12.43653261939170029, 21.89999795660000004, 30.61791799421799709 ),
 ( -4.891601802749729813E-05, 2.000000000000000000 ),
 .UNSPECIFIED. ) ;
#26842 = CARTESIAN_POINT ( 'NONE',  ( 25.51103972045700274, 1440.913060399400138, 219.1553983413110132 ) ) ;
#26843 = CARTESIAN_POINT ( 'NONE',  ( 2.597701311440000271, 1426.721572854839906, 188.7323019695990070 ) ) ;
#26844 = VECTOR ( 'NONE', #17552, 1000.000000000000114 ) ;
#26845 = CARTESIAN_POINT ( 'NONE',  ( 22.94032544519500050, 1507.620489270479993, 210.4476540011760051 ) ) ;
#26846 = DIRECTION ( 'NONE',  ( -0.02359658529091402182, 0.000000000000000000, 0.9997215618173935781 ) ) ;
#26847 = CARTESIAN_POINT ( 'NONE',  ( 22.61598442209999860, 1409.702807929629898, 208.8472236539830078 ) ) ;
#26848 = CARTESIAN_POINT ( 'NONE',  ( 6.232532001850000114, 1398.098440471829917, 220.5304192662980256 ) ) ;
#26849 = CARTESIAN_POINT ( 'NONE',  ( -14.93146304581260075, 1509.434478566749931, 236.0736287727190188 ) ) ;
#26850 = CARTESIAN_POINT ( 'NONE',  ( 23.81087019270000127, 1469.236087438830054, 218.4544119103479716 ) ) ;
#26851 = CARTESIAN_POINT ( 'NONE',  ( 22.53878404599999641, 1411.058442739730026, 206.1986151668880041 ) ) ;
#26852 = CARTESIAN_POINT ( 'NONE',  ( 26.14612021479581827, 1436.691281381861927, 136.8989692470566411 ) ) ;
#26853 = CARTESIAN_POINT ( 'NONE',  ( 3.266092768566498439, 1508.418517148852288, 219.8660019118054834 ) ) ;
#26854 = ADVANCED_FACE ( 'NONE', ( #3109 ), #60998, .F. ) ;
#26855 = CARTESIAN_POINT ( 'NONE',  ( -0.3862241457470880213, 1500.063268800599872, 233.1571801898780052 ) ) ;
#26856 = CARTESIAN_POINT ( 'NONE',  ( 1.135185044044999980, 1516.778853242349896, 212.5689744308569971 ) ) ;
#26857 = CARTESIAN_POINT ( 'NONE',  ( -21.76329145269999898, 1417.858357255770215, 210.0119042203199911 ) ) ;
#26858 = CARTESIAN_POINT ( 'NONE',  ( 0.1607068516070830067, 1485.841473127519976, 181.8434205804739747 ) ) ;
#26859 = EDGE_CURVE ( 'NONE', #57781, #59685, #47524, .T. ) ;
#26861 = ORIENTED_EDGE ( 'NONE', *, *, #7637, .T. ) ;
#26860 = CARTESIAN_POINT ( 'NONE',  ( 3.810264595240000052, 1441.769887200890025, 217.2430996589589824 ) ) ;
#26862 = DIRECTION ( 'NONE',  ( 0.000000000000000000, -1.000000000000000000, 0.000000000000000000 ) ) ;
#26863 = CARTESIAN_POINT ( 'NONE',  ( -3.078458343110000328, 1380.177950180139987, 203.2132938454989812 ) ) ;
#26864 = CARTESIAN_POINT ( 'NONE',  ( -4.467521880299999637, 1476.320660351190099, 199.7823413832389861 ) ) ;
#26866 = EDGE_LOOP ( 'NONE', ( #100130, #4792, #6198, #90490 ) ) ;
#26865 = CARTESIAN_POINT ( 'NONE',  ( -34.74890047483789601, 1451.658442319130017, 134.0999999982409747 ) ) ;
#26867 = CARTESIAN_POINT ( 'NONE',  ( -4.774552475180789735, 1508.551704408389924, 219.7184675692020051 ) ) ;
#26868 = ORIENTED_EDGE ( 'NONE', *, *, #91727, .T. ) ;
#26869 = DIRECTION ( 'NONE',  ( 0.000000000000000000, -1.000000000000000000, -2.960594732333529473E-13 ) ) ;
#26870 = CARTESIAN_POINT ( 'NONE',  ( -13.66489604771229871, 1390.428739317620057, 209.8137282845850109 ) ) ;
#26871 = CARTESIAN_POINT ( 'NONE',  ( 4.391835068428125766, 1445.322768932143845, 201.2232284873072103 ) ) ;
#26872 = DIRECTION ( 'NONE',  ( -1.000000000000000000, 0.000000000000000000, 0.000000000000000000 ) ) ;
#26874 = EDGE_CURVE ( 'NONE', #67163, #44154, #20474, .T. ) ;
#26873 = CARTESIAN_POINT ( 'NONE',  ( -2.829895884882737356, 1367.754820046488248, 209.5158523731048206 ) ) ;
#26875 = CARTESIAN_POINT ( 'NONE',  ( 0.6272946189549990503, 1431.084551388790032, 217.8556865675190011 ) ) ;
#26876 = VECTOR ( 'NONE', #66821, 1000.000000000000227 ) ;
#26877 = CARTESIAN_POINT ( 'NONE',  ( -14.82737418450000000, 1417.731569263860138, 213.2974731918289706 ) ) ;
#26878 = DIRECTION ( 'NONE',  ( 0.0002664641286723620469, 9.557308255310623861E-06, -0.9999999644527624021 ) ) ;
#26879 = CARTESIAN_POINT ( 'NONE',  ( 8.456465142934458612, 1517.151704408390060, 223.1002094411418284 ) ) ;
#26880 = CARTESIAN_POINT ( 'NONE',  ( -80.37803371308351075, 1385.159040155630009, 283.6058164050980395 ) ) ;
#26881 = CARTESIAN_POINT ( 'NONE',  ( -17.70260268349999677, 1414.015781091530016, 193.3445239933980133 ) ) ;
#26882 = CARTESIAN_POINT ( 'NONE',  ( -57.93277555979999960, 1379.748264674359916, 257.2455319417590545 ) ) ;
#26883 = ORIENTED_EDGE ( 'NONE', *, *, #87069, .T. ) ;
#26884 = EDGE_CURVE ( 'NONE', #58330, #104688, #97383, .T. ) ;
#26885 = CARTESIAN_POINT ( 'NONE',  ( -15.68556824057530008, 1410.853906741479932, 226.7268389267310056 ) ) ;
#26887 = ORIENTED_EDGE ( 'NONE', *, *, #81571, .F. ) ;
#26886 = CARTESIAN_POINT ( 'NONE',  ( -1.556370157619999972, 1414.996444526030018, 226.5294865527980051 ) ) ;
#26888 = CARTESIAN_POINT ( 'NONE',  ( 7.808553570872349248, 1465.967952420329993, 215.2103419416679913 ) ) ;
#26889 = ORIENTED_EDGE ( 'NONE', *, *, #78331, .T. ) ;
#26890 = CARTESIAN_POINT ( 'NONE',  ( 6.044783878490000539, 1450.853430557689990, 209.5026623076140027 ) ) ;
#26891 = CARTESIAN_POINT ( 'NONE',  ( -8.626596292616463657, 1364.357876662198805, 210.6218459617142003 ) ) ;
#26892 = CARTESIAN_POINT ( 'NONE',  ( -7.596603738389999805, 1494.381468487990105, 200.3558461181089854 ) ) ;
#26893 = AXIS2_PLACEMENT_3D ( 'NONE', #42377, #25006, #49700 ) ;
#26894 = CARTESIAN_POINT ( 'NONE',  ( 8.410267065803780360E-17, 1471.436294031830130, 269.3346704751489824 ) ) ;
#26895 = CARTESIAN_POINT ( 'NONE',  ( -33.14208818188965466, 1524.841055067850448, 220.4153344904860887 ) ) ;
#26896 = CARTESIAN_POINT ( 'NONE',  ( 18.15018407203804429, 1435.336561788914423, 215.0477887658213660 ) ) ;
#26897 = CARTESIAN_POINT ( 'NONE',  ( 3.043251598679999947, 1417.779699930629931, 234.3208245700980115 ) ) ;
#26898 = CARTESIAN_POINT ( 'NONE',  ( -7.042712267680692584, 1516.564738270622684, 211.7005065504913262 ) ) ;
#26899 = CARTESIAN_POINT ( 'NONE',  ( -19.87223104929999806, 1484.291808912129909, 191.2808552885979907 ) ) ;
#26900 = CARTESIAN_POINT ( 'NONE',  ( -9.841049031033593408, 1368.780040876450585, 209.6218459617033432 ) ) ;
#26901 = EDGE_CURVE ( 'NONE', #4103, #93518, #89237, .T. ) ;
#26902 = CARTESIAN_POINT ( 'NONE',  ( 0.5910745650690010233, 1455.956094962490170, 198.5601078200990059 ) ) ;
#26903 = CARTESIAN_POINT ( 'NONE',  ( 6.546039395294999785, 1516.565291103010168, 206.8289057630870218 ) ) ;
#26904 = DIRECTION ( 'NONE',  ( 0.000000000000000000, 0.000000000000000000, -1.000000000000000000 ) ) ;
#26905 = EDGE_CURVE ( 'NONE', #106936, #109851, #47790, .T. ) ;
#26906 = CARTESIAN_POINT ( 'NONE',  ( -15.97230738210199696, 1420.722887419069821, 227.0315163971459924 ) ) ;
#26907 = CARTESIAN_POINT ( 'NONE',  ( -1.119159361899999983, 1498.157713505790070, 197.8376082938989953 ) ) ;
#26909 = ORIENTED_EDGE ( 'NONE', *, *, #67976, .F. ) ;
#26908 = CARTESIAN_POINT ( 'NONE',  ( 0.4190295626039989840, 1494.278158734189901, 220.2761818919989878 ) ) ;
#26910 = CARTESIAN_POINT ( 'NONE',  ( -33.93529464457562028, 1436.159566638202477, 136.2997917599399500 ) ) ;
#26911 = ORIENTED_EDGE ( 'NONE', *, *, #47038, .T. ) ;
#26912 = CARTESIAN_POINT ( 'NONE',  ( 20.92767404034517753, 1511.187213306747708, 235.3888156262294444 ) ) ;
#26913 = CARTESIAN_POINT ( 'NONE',  ( -23.81975463399999882, 1410.917033286930064, 207.5563923665380059 ) ) ;
#26915 = CARTESIAN_POINT ( 'NONE',  ( 17.20744637360730067, 1410.879831455439898, 192.2037466765110025 ) ) ;
#26914 = CARTESIAN_POINT ( 'NONE',  ( -11.23695071452640093, 1426.040567954700236, 115.9703727133710061 ) ) ;
#26916 = CARTESIAN_POINT ( 'NONE',  ( -0.7355686809059980291, 1517.012231669750008, 212.3888856620870058 ) ) ;
#26917 = CARTESIAN_POINT ( 'NONE',  ( 30.16461248337728307, 1510.076493878218344, 208.1432171045278778 ) ) ;
#26918 = VECTOR ( 'NONE', #899, 1000.000000000000114 ) ;
#26919 = CARTESIAN_POINT ( 'NONE',  ( -19.76254418480000297, 1434.994542537920097, 208.0022035227879940 ) ) ;
#26920 = CARTESIAN_POINT ( 'NONE',  ( -30.28727319960000131, 1436.978278693949960, 240.1330978320980023 ) ) ;
#26921 = CARTESIAN_POINT ( 'NONE',  ( -14.22747554434230111, 1379.717775689809969, 208.2706285310750047 ) ) ;
#26922 = CARTESIAN_POINT ( 'NONE',  ( 28.25996324251219960, 1508.267047287839887, 209.3916282000910201 ) ) ;
#26923 = CARTESIAN_POINT ( 'NONE',  ( 2.550017816056660003, 1508.551704408389924, 214.1089244005430317 ) ) ;
#26924 = CARTESIAN_POINT ( 'NONE',  ( -37.89607820300650332, 1438.541137717810216, 136.6017170863420063 ) ) ;
#26925 = EDGE_LOOP ( 'NONE', ( #19205, #68043, #48703, #97952, #87708 ) ) ;
#26926 = CARTESIAN_POINT ( 'NONE',  ( 5.492325009455980123, 1396.104856602990139, 219.0480593849839863 ) ) ;
#26927 = CARTESIAN_POINT ( 'NONE',  ( 9.540313770239269076, 1461.184271939180007, 206.7184343888850151 ) ) ;
#26928 = CARTESIAN_POINT ( 'NONE',  ( -18.27671705869999741, 1459.242480605829996, 227.8606357436979977 ) ) ;
#26929 = ORIENTED_EDGE ( 'NONE', *, *, #37738, .T. ) ;
#26930 = ORIENTED_EDGE ( 'NONE', *, *, #39548, .F. ) ;
#26931 = CARTESIAN_POINT ( 'NONE',  ( 8.722999621409400106, 1451.780902529460036, 212.2858504672719846 ) ) ;
#26932 = CARTESIAN_POINT ( 'NONE',  ( 9.419895454800000678, 1425.271803998110045, 195.8713000332990077 ) ) ;
#26933 = ORIENTED_EDGE ( 'NONE', *, *, #106125, .T. ) ;
#26934 = CARTESIAN_POINT ( 'NONE',  ( -0.2617375006140000293, 1419.310405523930058, 227.5755756972980066 ) ) ;
#26935 = CARTESIAN_POINT ( 'NONE',  ( -12.17364444887732233, 1417.444261838927787, 199.6837928435173524 ) ) ;
#26936 = VECTOR ( 'NONE', #7757, 1000.000000000000000 ) ;
#26937 = DIRECTION ( 'NONE',  ( 0.000000000000000000, 0.000000000000000000, -1.000000000000000000 ) ) ;
#26938 = B_SPLINE_CURVE_WITH_KNOTS ( 'NONE', 3,
 ( #32154, #51170, #59578, #93691, #16971, #110518, #33250, #58474, #93157, #109429, #84752, #8049, #100458, #67440, #59033, #32706, #68541, #8597, #239, #24828, #100996, #102640, #67994, #102106, #24292, #85298, #50619, #76368, #15875, #42769, #50077, #42217, #94255, #7503, #76930, #41665, #33800, #75822, #34367, #60136, #17529, #51732, #43334, #15334, #85867, #9169, #66342, #77482, #23741, #62359, #96483, #79146, #1896, #27081, #61807, #52294, #53393, #87542, #69097, #78580, #27621, #79697 ),
 .UNSPECIFIED., .F., .F.,
 ( 4, 2, 2, 2, 2, 2, 2, 2, 2, 2, 1, 2, 2, 2, 2, 1, 1, 1, 2, 2, 2, 2, 2, 1, 2, 2, 2, 1, 2, 2, 2, 2, 2, 4 ),
 ( 0.000000000000000000, 0.06249999999413463625, 0.09374999999120205152, 0.1093749999897352942, 0.1249999999882685370, 0.1874999999824022989, 0.2187499999793056094, 0.2343749999779313475, 0.2499999999765570302, 0.3124999999710579845, 0.3437499999684511809, 0.3593749999672830597, 0.3749999999661149386, 0.4374999999608228385, 0.4687499999580535537, 0.4843749999566689390, 0.4921874999560780783, 0.4960937499558828456, 0.4980468749556873354, 0.4999999999554918251, 0.5624999999632132042, 0.5937499999669603179, 0.6093749999689117569, 0.6171874999698874209, 0.6210937499703144127, 0.6249999999707414045, 0.6874999999758888425, 0.7187499999784625615, 0.7343749999797464234, 0.7499999999810301743, 0.8124999999857194233, 0.8437499999880609947, 0.8749999999904025660, 1.000000000000000000 ),
 .UNSPECIFIED. ) ;
#26939 = CARTESIAN_POINT ( 'NONE',  ( 18.02257621027597523, 1524.382868172863937, 235.3484976865586589 ) ) ;
#26940 = CARTESIAN_POINT ( 'NONE',  ( 6.769661272017690301, 1509.032013615249980, 201.8557649540310024 ) ) ;
#26941 = CARTESIAN_POINT ( 'NONE',  ( 10.34945510115269940, 1451.639433892800071, 207.2647969978239928 ) ) ;
#26942 = CARTESIAN_POINT ( 'NONE',  ( -11.76465091080000036, 1391.913063699309987, 210.9192594439790014 ) ) ;
#26943 = CARTESIAN_POINT ( 'NONE',  ( -101.8661395909159921, 1384.880064502870027, 296.5719465711759426 ) ) ;
#26944 = EDGE_LOOP ( 'NONE', ( #45070, #105974, #87137, #43964 ) ) ;
#26945 = CARTESIAN_POINT ( 'NONE',  ( -7.331812124104999384, 1516.906641539930206, 202.5676945058570197 ) ) ;
#26946 = CARTESIAN_POINT ( 'NONE',  ( 4.623892060624999800, 1517.066898074209803, 209.8584071487349831 ) ) ;
#26947 = EDGE_LOOP ( 'NONE', ( #107028, #15612, #97452, #63458 ) ) ;
#26948 = CARTESIAN_POINT ( 'NONE',  ( 11.86566114180100051, 1432.305310558320116, 149.9823219675499786 ) ) ;
#26949 = CARTESIAN_POINT ( 'NONE',  ( 12.59191600518032139, 1445.042944653935137, 186.1852526257982561 ) ) ;
#26950 = VERTEX_POINT ( 'NONE', #77460 ) ;
#26951 = FACE_OUTER_BOUND ( 'NONE', #26519, .T. ) ;
#26952 = CARTESIAN_POINT ( 'NONE',  ( -17.11714625305222981, 1443.086052842849995, 162.7561045841209193 ) ) ;
#26953 = CARTESIAN_POINT ( 'NONE',  ( 2.953750800410000377, 1508.842156638330152, 237.0357385784979840 ) ) ;
#26954 = CIRCLE ( 'NONE', #80829, 2.000000000000001776 ) ;
#26955 = CARTESIAN_POINT ( 'NONE',  ( -31.81407709660760830, 1522.382868172863937, 221.9534378623334590 ) ) ;
#26956 = CARTESIAN_POINT ( 'NONE',  ( -4.875918348960000870, 1422.177864437230028, 185.3310708335980053 ) ) ;
#26957 = CARTESIAN_POINT ( 'NONE',  ( 2.230919469291039903, 1410.429474903630080, 269.3352092892910150 ) ) ;
#26958 = CARTESIAN_POINT ( 'NONE',  ( 9.224548086651552126, 1450.561207767010046, 209.2764872802650018 ) ) ;
#26959 = CARTESIAN_POINT ( 'NONE',  ( 0.4151546846821905223, 1524.726013923371283, 173.3106345060153330 ) ) ;
#26960 = CARTESIAN_POINT ( 'NONE',  ( 9.739193628800000724, 1492.624356258490025, 214.7590332456690021 ) ) ;
#26961 = DIRECTION ( 'NONE',  ( 6.123233995736769734E-17, 1.000000000000000000, 1.124819836996399911E-32 ) ) ;
#26962 = CARTESIAN_POINT ( 'NONE',  ( 8.930916390941154859, 1424.998531210375177, 195.6484565887391227 ) ) ;
#26964 = CARTESIAN_POINT ( 'NONE',  ( 10.01604805806510079, 1469.197346657220123, 203.9457370999409989 ) ) ;
#26963 = CARTESIAN_POINT ( 'NONE',  ( -21.25454558919999926, 1505.414223313590128, 209.4451586182409812 ) ) ;
#26965 = CARTESIAN_POINT ( 'NONE',  ( 15.57748978360000081, 1507.212883781729943, 225.5460497861979832 ) ) ;
#26966 = EDGE_CURVE ( 'NONE', #42556, #105229, #87865, .T. ) ;
#26967 = AXIS2_PLACEMENT_3D ( 'NONE', #47501, #64316, #72707 ) ;
#26968 = CARTESIAN_POINT ( 'NONE',  ( 17.63459991112690162, 1411.813115813379909, 224.8352634770240002 ) ) ;
#26969 = CARTESIAN_POINT ( 'NONE',  ( -4.893927726379848409, 1506.405825327593448, 187.7130172094022100 ) ) ;
#26970 = ORIENTED_EDGE ( 'NONE', *, *, #89715, .T. ) ;
#26971 = CARTESIAN_POINT ( 'NONE',  ( 28.27139721233038827, 1526.382868172863937, 198.6830693683571667 ) ) ;
#26972 = DIRECTION ( 'NONE',  ( 0.000000000000000000, 0.000000000000000000, 1.000000000000000000 ) ) ;
#26973 = B_SPLINE_CURVE_WITH_KNOTS ( 'NONE', 3,
 ( #47806, #66830, #23688, #99840, #56763, #13618 ),
 .UNSPECIFIED., .F., .F.,
 ( 4, 2, 4 ),
 ( 2.841188977517477842E-17, 0.001087661325621714888, 0.002175322651243401587 ),
 .UNSPECIFIED. ) ;
#26974 = LINE ( 'NONE', #67341, #77004 ) ;
#26975 = CARTESIAN_POINT ( 'NONE',  ( -14.58313706979999935, 1416.023439710309958, 214.1199149666390156 ) ) ;
#26977 = ORIENTED_EDGE ( 'NONE', *, *, #26145, .F. ) ;
#26976 = CARTESIAN_POINT ( 'NONE',  ( 0.7087989430401649971, 1515.130721759790049, 204.7941235941219986 ) ) ;
#26978 = CARTESIAN_POINT ( 'NONE',  ( -15.88400460199908615, 1415.958461537839639, 209.7364282889150218 ) ) ;
#26979 = AXIS2_PLACEMENT_3D ( 'NONE', #107535, #54957, #3455 ) ;
#26980 = CARTESIAN_POINT ( 'NONE',  ( 20.21728935790000037, 1475.862786327189951, 209.1218459616989946 ) ) ;
#26981 = EDGE_CURVE ( 'NONE', #21533, #49433, #74574, .T. ) ;
#26982 = CARTESIAN_POINT ( 'NONE',  ( -16.05592744339999811, 1416.237390274000063, 209.1226952231629923 ) ) ;
#26983 = CARTESIAN_POINT ( 'NONE',  ( -14.54063862746090052, 1419.501189642470081, 221.4764621185310034 ) ) ;
#26984 = CARTESIAN_POINT ( 'NONE',  ( -10.76610293753739889, 1461.751116445120033, 211.3389343603909936 ) ) ;
#26985 = ADVANCED_FACE ( 'NONE', ( #17511 ), #1084, .F. ) ;
#26986 = CARTESIAN_POINT ( 'NONE',  ( 5.864566082395450408, 1517.051704408389924, 226.1537825710409777 ) ) ;
#26987 = CARTESIAN_POINT ( 'NONE',  ( -15.37702286096500082, 1512.655881406860090, 222.6262963000669970 ) ) ;
#26988 = CARTESIAN_POINT ( 'NONE',  ( 14.42199049240000086, 1412.743552572030012, 227.9099018574979993 ) ) ;
#26989 = CARTESIAN_POINT ( 'NONE',  ( -8.203088214330000127, 1478.337535159890194, 216.4441348706290285 ) ) ;
#26990 = CARTESIAN_POINT ( 'NONE',  ( -15.85075050099999849, 1459.333342989330049, 230.7228811812979927 ) ) ;
#26991 = CARTESIAN_POINT ( 'NONE',  ( 5.770883563884999568, 1516.603620185149794, 206.8276363026970159 ) ) ;
#26992 = CARTESIAN_POINT ( 'NONE',  ( 35.85544596869999623, 1418.707560334130221, 266.7164716470979897 ) ) ;
#26993 = CARTESIAN_POINT ( 'NONE',  ( 23.43375805480000196, 1435.459271872349973, 139.6354490908979926 ) ) ;
#26994 = CARTESIAN_POINT ( 'NONE',  ( 21.00038310420000087, 1508.013874135629976, 190.5210545032980178 ) ) ;
#26995 = CARTESIAN_POINT ( 'NONE',  ( -21.92914898369999932, 1430.600989885229865, 219.4305798082980061 ) ) ;
#26996 = CARTESIAN_POINT ( 'NONE',  ( -12.51041414926550033, 1378.851565959029813, 207.9029934983620365 ) ) ;
#26997 = CARTESIAN_POINT ( 'NONE',  ( 17.55387852034876772, 1524.816846803860926, 237.4833057087513168 ) ) ;
#26998 = CARTESIAN_POINT ( 'NONE',  ( -1.438892233660000075, 1452.191231073930112, 183.8587012488980008 ) ) ;
#26999 = DIRECTION ( 'NONE',  ( -2.745975287049403995E-15, -1.000000000000000000, 0.000000000000000000 ) ) ;
#27000 = CARTESIAN_POINT ( 'NONE',  ( -15.57711053439999915, 1415.747624789430120, 209.0870974357659975 ) ) ;
#27001 = CARTESIAN_POINT ( 'NONE',  ( -12.94626818629999931, 1441.161188681390058, 188.2109162517980110 ) ) ;
#27002 = EDGE_CURVE ( 'NONE', #47989, #52269, #38458, .T. ) ;
#27003 = CARTESIAN_POINT ( 'NONE',  ( -27.81074406628219720, 1508.344687507839808, 210.5011464727880082 ) ) ;
#27004 = CARTESIAN_POINT ( 'NONE',  ( -29.16177349730000046, 1435.516078635969961, 135.2137962254980152 ) ) ;
#27005 = DIRECTION ( 'NONE',  ( -6.162707975952100561E-15, -1.000000000000000000, -1.094450614310000083E-14 ) ) ;
#27006 = VERTEX_POINT ( 'NONE', #96464 ) ;
#27007 = ADVANCED_FACE ( 'NONE', ( #29254 ), #2437, .F. ) ;
#27008 = CARTESIAN_POINT ( 'NONE',  ( -2.475398974845000044, 1511.813148765560072, 201.5364415457169969 ) ) ;
#27009 = CARTESIAN_POINT ( 'NONE',  ( -13.60185556200659995, 1409.388047650059889, 202.9415292635579817 ) ) ;
#27011 = ADVANCED_FACE ( 'NONE', ( #95360 ), #97563, .F. ) ;
#27010 = CARTESIAN_POINT ( 'NONE',  ( -2.478345701239999865, 1438.626251700270132, 157.7274745556979951 ) ) ;
#27012 = CARTESIAN_POINT ( 'NONE',  ( -5.191234770863918158, 1422.191368612545830, 138.4296091694463655 ) ) ;
#27013 = CARTESIAN_POINT ( 'NONE',  ( -23.45916826750000084, 1470.553228125530040, 269.3037833821979916 ) ) ;
#27014 = CARTESIAN_POINT ( 'NONE',  ( -5.780263042159999642, 1449.134363676490011, 210.7231825170590014 ) ) ;
#27015 = FACE_OUTER_BOUND ( 'NONE', #11773, .T. ) ;
#27016 = CARTESIAN_POINT ( 'NONE',  ( 18.27178068149059698, 1424.508154551730058, 223.6268415059790016 ) ) ;
#27017 = CARTESIAN_POINT ( 'NONE',  ( -77.06261576968471161, 1384.644925923339997, 301.7490929136619684 ) ) ;
#27018 = CARTESIAN_POINT ( 'NONE',  ( -22.48406008717340043, 1384.955127046689995, 202.3785104426330008 ) ) ;
#27019 = AXIS2_PLACEMENT_3D ( 'NONE', #50202, #84327, #39007 ) ;
#27020 = CARTESIAN_POINT ( 'NONE',  ( 17.03077326642920042, 1422.100639735759842, 226.8181581180180046 ) ) ;
#27021 = CARTESIAN_POINT ( 'NONE',  ( 21.33101636929999856, 1509.431424277029919, 227.6967412429980300 ) ) ;
#27022 = CARTESIAN_POINT ( 'NONE',  ( 15.22885431829999980, 1495.920296619829969, 224.7378832126979944 ) ) ;
#27023 = EDGE_CURVE ( 'NONE', #18694, #67656, #40157, .T. ) ;
#27024 = CARTESIAN_POINT ( 'NONE',  ( -20.50000000000000000, 1443.913060387330006, 169.0968414572980123 ) ) ;
#27025 = CARTESIAN_POINT ( 'NONE',  ( 4.274333237420000486, 1515.341807516890185, 207.6471969281190013 ) ) ;
#27026 = CARTESIAN_POINT ( 'NONE',  ( -7.965791537440000347, 1384.924596536209947, 199.4891613279189926 ) ) ;
#27027 = CARTESIAN_POINT ( 'NONE',  ( -22.84695657510000188, 1409.710893691230012, 207.6723829003780111 ) ) ;
#27028 = AXIS2_PLACEMENT_3D ( 'NONE', #9194, #35488, #110538 ) ;
#27029 = CARTESIAN_POINT ( 'NONE',  ( 17.29183750270000175, 1416.216252248729916, 203.8075771790779811 ) ) ;
#27030 = CARTESIAN_POINT ( 'NONE',  ( 4.637205103430000364, 1484.703917610690041, 219.2115800062989877 ) ) ;
#27031 = CARTESIAN_POINT ( 'NONE',  ( 11.27956504841369956, 1479.374699450910157, 208.0836311270099941 ) ) ;
#27032 = CARTESIAN_POINT ( 'NONE',  ( -106.4289199541310040, 1391.913060387289988, 304.6850071326550164 ) ) ;
#27033 = CARTESIAN_POINT ( 'NONE',  ( -2.956277750134179705, 1450.104957259319917, 188.5563321079999923 ) ) ;
#27034 = CARTESIAN_POINT ( 'NONE',  ( -5.984345136421869604, 1508.551704613440052, 216.1343701918329998 ) ) ;
#27035 = CARTESIAN_POINT ( 'NONE',  ( 10.99044570490370099, 1479.494708708640019, 229.8297407083400117 ) ) ;
#27038 = CARTESIAN_POINT ( 'NONE',  ( -9.742013687190000937, 1382.306311483530180, 200.9513237270989805 ) ) ;
#27037 = AXIS2_PLACEMENT_3D ( 'NONE', #49712, #16066, #75473 ) ;
#27036 = CYLINDRICAL_SURFACE ( 'NONE', #94381, 1.000000000000000888 ) ;
#27039 = CARTESIAN_POINT ( 'NONE',  ( -5.222641464789999688, 1391.931189815790049, 203.5968850314390011 ) ) ;
#27040 = CARTESIAN_POINT ( 'NONE',  ( 9.808398454338320249, 1435.362476046070242, 208.7559545901820002 ) ) ;
#27041 = CARTESIAN_POINT ( 'NONE',  ( -14.96851909909330125, 1420.519469560630114, 212.0434853293359936 ) ) ;
#27042 = EDGE_CURVE ( 'NONE', #48449, #106610, #102718, .T. ) ;
#27043 = CARTESIAN_POINT ( 'NONE',  ( -23.32329893220000017, 1415.973289857730151, 210.9192745123079931 ) ) ;
#27044 = CARTESIAN_POINT ( 'NONE',  ( 4.325405441708593202, 1515.219201591195542, 206.7917118349596421 ) ) ;
#27045 = CONICAL_SURFACE ( 'NONE', #48556, 23.69926344187880929, 1.195358426993359036 ) ;
#27046 = CARTESIAN_POINT ( 'NONE',  ( -2.877113108595000135, 1516.697242742309982, 204.1252037719370094 ) ) ;
#27047 = CARTESIAN_POINT ( 'NONE',  ( -4.234262180109699791, 1398.039394699497734, 221.4129439625630482 ) ) ;
#27048 = CARTESIAN_POINT ( 'NONE',  ( 16.11449818973499859, 1514.335759350750095, 194.1182033692670075 ) ) ;
#27049 = DIRECTION ( 'NONE',  ( 1.000000000000000000, 0.000000000000000000, 0.000000000000000000 ) ) ;
#27050 = CARTESIAN_POINT ( 'NONE',  ( 1.893906785159999995, 1508.749492714529879, 237.3763040025980047 ) ) ;
#27051 = EDGE_CURVE ( 'NONE', #83952, #89419, #54596, .T. ) ;
#27052 = CARTESIAN_POINT ( 'NONE',  ( 9.536702226868399634, 1504.881375799320040, 215.9278409599580186 ) ) ;
#27053 = CARTESIAN_POINT ( 'NONE',  ( 39.57440995424759933, 1448.587977546229922, 136.2060456146669765 ) ) ;
#27055 = VERTEX_POINT ( 'NONE', #86951 ) ;
#27054 = CARTESIAN_POINT ( 'NONE',  ( -66.36191841066799668, 1379.742046394640056, 277.0709747383730246 ) ) ;
#27056 = ORIENTED_EDGE ( 'NONE', *, *, #91961, .T. ) ;
#27057 = CARTESIAN_POINT ( 'NONE',  ( 11.41050180535800074, 1433.984814470099991, 151.4218912366809775 ) ) ;
#27058 = CARTESIAN_POINT ( 'NONE',  ( 21.60819468828557177, 1524.659802833171625, 183.5975935901099376 ) ) ;
#27059 = ORIENTED_EDGE ( 'NONE', *, *, #56436, .T. ) ;
#27060 = CARTESIAN_POINT ( 'NONE',  ( -1.485124824312086922, 1457.022419630208788, 199.7284311504454877 ) ) ;
#27061 = CARTESIAN_POINT ( 'NONE',  ( -10.32117538795129974, 1448.479331933469894, 208.0292346068879965 ) ) ;
#27062 = CARTESIAN_POINT ( 'NONE',  ( -2.372478608332516892, 1512.187213306747481, 243.3440112565233449 ) ) ;
#27065 = EDGE_CURVE ( 'NONE', #26775, #92807, #105298, .T. ) ;
#27064 = CARTESIAN_POINT ( 'NONE',  ( 4.579624579470000789, 1427.832655172230034, 112.4493539157979995 ) ) ;
#27063 = CARTESIAN_POINT ( 'NONE',  ( 16.04547803650780224, 1423.236165506360067, 191.1345828222399916 ) ) ;
#27066 = CARTESIAN_POINT ( 'NONE',  ( 17.88837883210679891, 1459.164429878010196, 217.9459145873090051 ) ) ;
#27067 = CIRCLE ( 'NONE', #86114, 1.000000000000001554 ) ;
#27068 = CARTESIAN_POINT ( 'NONE',  ( 2.284878824769999817, 1507.640563443429983, 181.2510407452979848 ) ) ;
#27069 = CARTESIAN_POINT ( 'NONE',  ( -5.191737366139999921, 1415.425433635630043, 192.3072415768979795 ) ) ;
#27070 = CARTESIAN_POINT ( 'NONE',  ( 15.96541745440000248, 1410.402655727529918, 226.9120801968979890 ) ) ;
#27071 = CARTESIAN_POINT ( 'NONE',  ( -7.708770045145000083, 1516.524310051880093, 211.4128934593470035 ) ) ;
#27072 = DIRECTION ( 'NONE',  ( -1.000000000000000000, -5.823966869780190178E-19, 4.137698748469999823E-18 ) ) ;
#27074 = AXIS2_PLACEMENT_3D ( 'NONE', #41455, #109752, #67220 ) ;
#27073 = CARTESIAN_POINT ( 'NONE',  ( -11.94865520339239851, 1422.082048078050093, 208.3249290792549857 ) ) ;
#27075 = CARTESIAN_POINT ( 'NONE',  ( 6.242053746214999421, 1513.743447518349967, 201.5518632705069706 ) ) ;
#27076 = EDGE_LOOP ( 'NONE', ( #96944, #89989, #79838, #84216 ) ) ;
#27077 = CARTESIAN_POINT ( 'NONE',  ( 13.80090640870000129, 1435.296980361239775, 149.7022445371979984 ) ) ;
#27078 = CARTESIAN_POINT ( 'NONE',  ( -5.013435694540000043, 1375.426148861440197, 203.5256706139790310 ) ) ;
#27079 = ORIENTED_EDGE ( 'NONE', *, *, #24852, .T. ) ;
#27080 = ORIENTED_EDGE ( 'NONE', *, *, #76982, .F. ) ;
#27081 = CARTESIAN_POINT ( 'NONE',  ( 12.76025368180385478, 1444.996096971014367, 169.4538372660288985 ) ) ;
#27082 = CARTESIAN_POINT ( 'NONE',  ( -1.606022318079999955, 1464.996810821029840, 236.7393652189979889 ) ) ;
#27083 = CARTESIAN_POINT ( 'NONE',  ( -8.356582281726788963, 1474.676444402793095, 203.1368637855367183 ) ) ;
#27084 = CARTESIAN_POINT ( 'NONE',  ( -7.329930051325000306, 1516.881930554049859, 216.8399805996670011 ) ) ;
#27085 = CARTESIAN_POINT ( 'NONE',  ( -1.910306335979069958, 1465.019396637220098, 198.2840305075910123 ) ) ;
#27086 = VECTOR ( 'NONE', #38514, 1000.000000000000000 ) ;
#27087 = CARTESIAN_POINT ( 'NONE',  ( 11.46028677100449933, 1422.055054995990076, 209.9672720893090059 ) ) ;
#27088 = CARTESIAN_POINT ( 'NONE',  ( -50.32639114276440040, 1379.689784808286959, 240.1992801506042099 ) ) ;
#27089 = CARTESIAN_POINT ( 'NONE',  ( 4.240521952282210627, 1446.386233147809889, 162.7524229475580171 ) ) ;
#27090 = CARTESIAN_POINT ( 'NONE',  ( 0.5968024102800000286, 1507.130435900830207, 237.3073193260979963 ) ) ;
#27091 = VERTEX_POINT ( 'NONE', #21370 ) ;
#27092 = CARTESIAN_POINT ( 'NONE',  ( 4.996642160164999957, 1516.697242742309982, 206.2447328616370044 ) ) ;
#27093 = EDGE_LOOP ( 'NONE', ( #90040, #38214, #5878, #3891 ) ) ;
#27094 = CARTESIAN_POINT ( 'NONE',  ( -104.2285098495619877, 1379.857407253709880, 305.0244821878710013 ) ) ;
#27095 = CARTESIAN_POINT ( 'NONE',  ( -19.86721352349999847, 1507.838653463430092, 229.2281063170979678 ) ) ;
#27096 = EDGE_LOOP ( 'NONE', ( #38338, #109305, #17682, #47306 ) ) ;
#27097 = CARTESIAN_POINT ( 'NONE',  ( -7.320053526199809646, 1508.610509074409947, 203.0404548948610000 ) ) ;
#27098 = CARTESIAN_POINT ( 'NONE',  ( -14.54785189459999906, 1409.587746979729900, 191.1299195843979817 ) ) ;
#27099 = CARTESIAN_POINT ( 'NONE',  ( -24.30324774889999873, 1442.429924160389874, 211.8155477906580018 ) ) ;
#27100 = CARTESIAN_POINT ( 'NONE',  ( -10.79382126600000014, 1414.913060387329779, 196.1395803457980094 ) ) ;
#27101 = CARTESIAN_POINT ( 'NONE',  ( 0.5938345015652835013, 1455.008249108801238, 218.5312979207114950 ) ) ;
#27102 = CARTESIAN_POINT ( 'NONE',  ( 18.72979941119999836, 1454.437773883689943, 204.5413093961989830 ) ) ;
#27103 = CARTESIAN_POINT ( 'NONE',  ( -5.387811863060000483, 1496.648312753189884, 199.2595355468089906 ) ) ;
#27104 = CARTESIAN_POINT ( 'NONE',  ( -3.252554812490000113, 1508.258009291689859, 220.7618944614989971 ) ) ;
#27105 = CARTESIAN_POINT ( 'NONE',  ( 2.175771579259999644, 1492.304798991390044, 188.2630637080989970 ) ) ;
#27107 = CARTESIAN_POINT ( 'NONE',  ( -3.257220640824999958, 1517.040132827679827, 214.9086836491569841 ) ) ;
#27106 = STYLED_ITEM ( 'NONE', ( #16961 ), #89391 ) ;
#27108 = CARTESIAN_POINT ( 'NONE',  ( 23.28443042909999861, 1409.830905058029884, 209.4348658987040039 ) ) ;
#27109 = CARTESIAN_POINT ( 'NONE',  ( 5.652025608424629866, 1510.855104182140167, 216.7229383695649858 ) ) ;
#27110 = CARTESIAN_POINT ( 'NONE',  ( -17.22592475670000312, 1443.501467202829872, 162.9227486557980171 ) ) ;
#27111 = CARTESIAN_POINT ( 'NONE',  ( 1.715704490974999885, 1516.757508073510053, 212.3732403323669757 ) ) ;
#27112 = CARTESIAN_POINT ( 'NONE',  ( 14.12346818419999828, 1409.573558249629968, 191.9327832110980125 ) ) ;
#27113 = CIRCLE ( 'NONE', #84324, 2.000000000000001332 ) ;
#27114 = CARTESIAN_POINT ( 'NONE',  ( -15.46014185669380758, 1486.078827481694816, 186.6217453166497933 ) ) ;
#27116 = VERTEX_POINT ( 'NONE', #81294 ) ;
#27115 = CARTESIAN_POINT ( 'NONE',  ( -77.92118381710000108, 1389.362486221770041, 299.0650494567590272 ) ) ;
#27117 = CARTESIAN_POINT ( 'NONE',  ( 24.09667836379999883, 1455.346817057629778, 238.1639200605980022 ) ) ;
#27118 = CARTESIAN_POINT ( 'NONE',  ( 3.932775080253070321, 1448.980696629100066, 184.2693358254829832 ) ) ;
#27119 = CARTESIAN_POINT ( 'NONE',  ( -27.91227906400350278, 1509.887778650499968, 218.1998177527819962 ) ) ;
#27120 = CARTESIAN_POINT ( 'NONE',  ( -1.586365103999400006, 1508.858152673860104, 238.2399376808540126 ) ) ;
#27121 = CARTESIAN_POINT ( 'NONE',  ( -18.72407526530000155, 1458.246115540929850, 227.3156487912980026 ) ) ;
#27122 = CONICAL_SURFACE ( 'NONE', #39661, 0.9999999999999956701, 0.7853981633970000820 ) ;
#27124 = CARTESIAN_POINT ( 'NONE',  ( -8.861333410770001251, 1384.870662623919998, 218.6848950059789729 ) ) ;
#27123 = CARTESIAN_POINT ( 'NONE',  ( 10.98084429529999895, 1433.016923057050008, 151.7694244727979935 ) ) ;
#27125 = CARTESIAN_POINT ( 'NONE',  ( -8.681712390459869866, 1448.751914763990044, 212.0069377265070045 ) ) ;
#27126 = CARTESIAN_POINT ( 'NONE',  ( -107.1170720883229990, 1381.212740012770155, 309.4630679377449951 ) ) ;
#27127 = ORIENTED_EDGE ( 'NONE', *, *, #100930, .T. ) ;
#27128 = CARTESIAN_POINT ( 'NONE',  ( -4.038637500854999729, 1516.734985836460055, 203.3481771172569950 ) ) ;
#27129 = CARTESIAN_POINT ( 'NONE',  ( 0.1062812984699999935, 1406.777728848529932, 269.6500679733979950 ) ) ;
#27130 = CARTESIAN_POINT ( 'NONE',  ( -18.66420869458074350, 1526.382868172863937, 185.4599087859683095 ) ) ;
#27131 = CARTESIAN_POINT ( 'NONE',  ( 3.048828143997139861, 1509.019527812190063, 237.9289388395170306 ) ) ;
#27132 = DIRECTION ( 'NONE',  ( 5.980589973904019347E-17, -1.000000000000000000, 1.736889445713099699E-16 ) ) ;
#27133 = DIRECTION ( 'NONE',  ( 1.755985294532469921E-16, -1.000000000000000000, 1.338183447452831989E-16 ) ) ;
#27134 = CARTESIAN_POINT ( 'NONE',  ( 5.602114820939999795, 1448.090347409289961, 206.1652803823789952 ) ) ;
#27135 = CIRCLE ( 'NONE', #43207, 1.000000000000011102 ) ;
#27136 = CARTESIAN_POINT ( 'NONE',  ( -37.32042369672969784, 1440.913060388040094, 255.1694497076479990 ) ) ;
#27137 = CARTESIAN_POINT ( 'NONE',  ( 36.31051540993509974, 1449.892126659239921, 136.2553180242439907 ) ) ;
#27138 = FACE_OUTER_BOUND ( 'NONE', #80085, .T. ) ;
#27139 = CARTESIAN_POINT ( 'NONE',  ( -0.7394123279979990526, 1431.039654945390112, 200.6341525829290049 ) ) ;
#27140 = EDGE_CURVE ( 'NONE', #68445, #96281, #89702, .T. ) ;
#27141 = CARTESIAN_POINT ( 'NONE',  ( -32.02808312589930040, 1501.977400791986611, 198.2787714533499752 ) ) ;
#27142 = CARTESIAN_POINT ( 'NONE',  ( -0.1522252554610010189, 1508.600545075490118, 220.9033078710990026 ) ) ;
#27143 = CARTESIAN_POINT ( 'NONE',  ( -7.847012372209785980, 1448.000573986833842, 213.8304041876558301 ) ) ;
#27144 = VERTEX_POINT ( 'NONE', #82953 ) ;
#27145 = CARTESIAN_POINT ( 'NONE',  ( 0.000000000000000000, 1378.913060387289988, 209.1218459616989946 ) ) ;
#27146 = CARTESIAN_POINT ( 'NONE',  ( 2.526502914729999993, 1486.393260774789951, 198.2275259192990120 ) ) ;
#27147 = CARTESIAN_POINT ( 'NONE',  ( 5.518436134040229923, 1466.731182993539960, 200.2557783364140107 ) ) ;
#27148 = CARTESIAN_POINT ( 'NONE',  ( 11.16572705624736628, 1425.241472595376536, 138.5380445582760842 ) ) ;
#27149 = CARTESIAN_POINT ( 'NONE',  ( 11.66538825820000014, 1501.769421336390224, 211.4581643459090117 ) ) ;
#27150 = CARTESIAN_POINT ( 'NONE',  ( -27.78452742370000195, 1508.000976255530077, 210.4681928078880162 ) ) ;
#27151 = CARTESIAN_POINT ( 'NONE',  ( 8.000563468399999323, 1425.311447451950016, 211.1882539080190213 ) ) ;
#27152 = VECTOR ( 'NONE', #86327, 999.9999999999998863 ) ;
#27154 = EDGE_CURVE ( 'NONE', #35203, #34173, #19816, .T. ) ;
#27153 = CARTESIAN_POINT ( 'NONE',  ( -17.56720881609999907, 1415.048591087029763, 207.8848073021879941 ) ) ;
#27155 = CARTESIAN_POINT ( 'NONE',  ( 11.87064635662919976, 1432.676990320220057, 149.9815557213069894 ) ) ;
#27156 = CARTESIAN_POINT ( 'NONE',  ( 26.21858036434699812, 1435.413047757679806, 135.3174467644430194 ) ) ;
#27157 =( BOUNDED_CURVE ( )  B_SPLINE_CURVE ( 3, ( #60098, #42730, #61225, #110478 ),
 .UNSPECIFIED., .F., .F. ) 
 B_SPLINE_CURVE_WITH_KNOTS ( ( 4, 4 ),
 ( 4.286339096376821090, 4.712350959133279282 ),
 .UNSPECIFIED. ) 
 CURVE ( )  GEOMETRIC_REPRESENTATION_ITEM ( )  RATIONAL_B_SPLINE_CURVE ( ( 1.000000000000000000, 0.9849332539716901813, 0.9849332539716901813, 1.000000000000000000 ) ) 
 REPRESENTATION_ITEM ( '' )  );
#27158 = CARTESIAN_POINT ( 'NONE',  ( -6.881200948753640745, 1396.153357219529880, 200.4803135408690196 ) ) ;
#27159 = ORIENTED_EDGE ( 'NONE', *, *, #888, .F. ) ;
#27160 = AXIS2_PLACEMENT_3D ( 'NONE', #68239, #59824, #77175 ) ;
#27161 = CARTESIAN_POINT ( 'NONE',  ( -17.31304841774549885, 1410.598387540080012, 225.8442784478359897 ) ) ;
#27162 = CARTESIAN_POINT ( 'NONE',  ( 4.897375497219999652, 1432.353341358199941, 150.0655110971979980 ) ) ;
#27163 = ORIENTED_EDGE ( 'NONE', *, *, #83005, .T. ) ;
#27164 = CARTESIAN_POINT ( 'NONE',  ( -11.25901873070000114, 1500.172003391289991, 210.8567363387790010 ) ) ;
#27165 = DIRECTION ( 'NONE',  ( -0.8672669759446667292, 0.000000000000000000, -0.4978433412588673113 ) ) ;
#27167 = CARTESIAN_POINT ( 'NONE',  ( 0.3787159155534669530, 1456.889667869769937, 219.7399949435159954 ) ) ;
#27166 = CARTESIAN_POINT ( 'NONE',  ( 10.32455812189999911, 1425.433999229330084, 91.15122192769788967 ) ) ;
#27168 = DIRECTION ( 'NONE',  ( -1.836970198721029688E-16, -1.000000000000000000, 0.000000000000000000 ) ) ;
#27169 = CARTESIAN_POINT ( 'NONE',  ( 4.144484579423279413, 1424.490014308070158, 184.8547326364549974 ) ) ;
#27170 = CARTESIAN_POINT ( 'NONE',  ( 23.10442899973940101, 1411.095127650270115, 207.3185325528490068 ) ) ;
#27171 = CARTESIAN_POINT ( 'NONE',  ( 7.428831053269999707, 1425.174870893220032, 212.3938909338090184 ) ) ;
#27172 = CARTESIAN_POINT ( 'NONE',  ( 20.33508558929999666, 1432.834457682990205, 214.7556889579689994 ) ) ;
#27173 = CARTESIAN_POINT ( 'NONE',  ( 7.629628877820000099, 1508.993558936030013, 181.6876041027980193 ) ) ;
#27174 = CARTESIAN_POINT ( 'NONE',  ( 2.514853015309999940, 1449.255880420389985, 182.8296093962979967 ) ) ;
#27175 = EDGE_CURVE ( 'NONE', #94600, #5500, #99927, .T. ) ;
#27176 = CARTESIAN_POINT ( 'NONE',  ( 7.990250629489356271, 1364.963476878560641, 209.6218459617148824 ) ) ;
#27178 = ORIENTED_EDGE ( 'NONE', *, *, #34408, .F. ) ;
#27177 = CARTESIAN_POINT ( 'NONE',  ( -4.490619237334504632, 1508.909942010301620, 205.6342535026303437 ) ) ;
#27179 = ORIENTED_EDGE ( 'NONE', *, *, #6907, .F. ) ;
#27180 = CARTESIAN_POINT ( 'NONE',  ( -41.49088794730000274, 1443.869659108800079, 136.5795274476980126 ) ) ;
#27181 = CARTESIAN_POINT ( 'NONE',  ( 7.513187920566976707, 1510.663752934522563, 203.1583860890702908 ) ) ;
#27182 = CARTESIAN_POINT ( 'NONE',  ( -0.9815465312350000193, 1473.584474657329793, 270.3924816079979792 ) ) ;
#27183 = CARTESIAN_POINT ( 'NONE',  ( -110.0628754741750015, 1384.910641149650019, 296.9513051048269858 ) ) ;
#27185 = ADVANCED_FACE ( 'NONE', ( #106509 ), #74572, .T. ) ;
#27184 = CARTESIAN_POINT ( 'NONE',  ( -1.321799804340000106, 1485.974695964230023, 182.1001927673979992 ) ) ;
#27186 = CARTESIAN_POINT ( 'NONE',  ( 22.22649075570000221, 1507.849990204029837, 192.4185849886980009 ) ) ;
#27187 = CARTESIAN_POINT ( 'NONE',  ( 0.7060385530502589768, 1475.942608798000037, 197.6738236987649771 ) ) ;
#27188 = CARTESIAN_POINT ( 'NONE',  ( -33.92643721410139790, 1451.728327248950109, 135.1498936377919904 ) ) ;
#27189 = CARTESIAN_POINT ( 'NONE',  ( -2.500000000000000000, 1448.224516615570110, 166.8026561098010063 ) ) ;
#27190 = CARTESIAN_POINT ( 'NONE',  ( 10.29084807479042318, 1367.270713213549698, 210.6218459617030021 ) ) ;
#27191 = CARTESIAN_POINT ( 'NONE',  ( 12.15499524530000031, 1407.709276878430046, 215.7704773373179989 ) ) ;
#27192 = CARTESIAN_POINT ( 'NONE',  ( -1.525793978527139938, 1406.001425806299721, 266.9604480841060195 ) ) ;
#27193 = CARTESIAN_POINT ( 'NONE',  ( -13.91014378093700010, 1434.990842025300026, 148.7054735720130054 ) ) ;
#27194 = ORIENTED_EDGE ( 'NONE', *, *, #103727, .F. ) ;
#27195 = PLANE ( 'NONE',  #66120 ) ;
#27196 = CARTESIAN_POINT ( 'NONE',  ( 13.41353349150000085, 1442.422659372690077, 188.9779284783980131 ) ) ;
#27197 = ORIENTED_EDGE ( 'NONE', *, *, #83079, .F. ) ;
#27198 = ORIENTED_EDGE ( 'NONE', *, *, #91975, .F. ) ;
#27199 = VECTOR ( 'NONE', #106077, 1000.000000000000000 ) ;
#27200 = CARTESIAN_POINT ( 'NONE',  ( -4.162247305190000191, 1453.824586353890027, 199.5089249234089834 ) ) ;
#27201 = CARTESIAN_POINT ( 'NONE',  ( -9.934709065799999905, 1365.494406819939968, 207.6218459616989946 ) ) ;
#27202 = CARTESIAN_POINT ( 'NONE',  ( -4.610938249504999753, 1516.815231249920089, 213.1623732742069990 ) ) ;
#27203 = CARTESIAN_POINT ( 'NONE',  ( 2.930838039564999775, 1510.983859056260144, 216.6855341620170350 ) ) ;
#27204 = ORIENTED_EDGE ( 'NONE', *, *, #39405, .T. ) ;
#27205 = CARTESIAN_POINT ( 'NONE',  ( -73.95609427729999652, 1377.212643071030016, 283.6384370524589826 ) ) ;
#27206 = CARTESIAN_POINT ( 'NONE',  ( -106.6936934317039913, 1378.913060387289988, 301.5874337866879955 ) ) ;
#27207 = CARTESIAN_POINT ( 'NONE',  ( -2.295485539174999978, 1516.651306816259876, 204.1261199623870368 ) ) ;
#27208 = CIRCLE ( 'NONE', #64727, 10.00000000000000888 ) ;
#27209 = B_SPLINE_CURVE_WITH_KNOTS ( 'NONE', 3,
 ( #74755, #58505, #92089, #56848, #65259, #101024, #73660, #48459, #108892, #31626, #43225, #107792, #90980, #109456, #108343, #47888, #34806, #32185, #56294 ),
 .UNSPECIFIED., .F., .F.,
 ( 4, 3, 3, 3, 3, 3, 4 ),
 ( -7.874164591667580204, -7.680830555785009395, -6.505323578896399894, -5.552647998340869862, -4.828139871705260155, -4.001703595992710305, -3.231130238939999622 ),
 .UNSPECIFIED. ) ;
#27210 = CARTESIAN_POINT ( 'NONE',  ( -29.24389883310000116, 1509.942753386430013, 204.9097857627180019 ) ) ;
#27211 = CARTESIAN_POINT ( 'NONE',  ( 31.12456774391177206, 1525.960063244516959, 217.0912716842394730 ) ) ;
#27212 = CARTESIAN_POINT ( 'NONE',  ( -94.50571792069999333, 1385.206310935810052, 294.8715553429590273 ) ) ;
#27213 = CARTESIAN_POINT ( 'NONE',  ( -66.81431226368310661, 1384.716740919450103, 259.0825501825760284 ) ) ;
#27214 = DIRECTION ( 'NONE',  ( 0.9455185755993178454, 0.000000000000000000, -0.3255681544571539243 ) ) ;
#27215 = CARTESIAN_POINT ( 'NONE',  ( -27.41498742912919795, 1488.731319228159919, 208.8198958867089914 ) ) ;
#27217 = VERTEX_POINT ( 'NONE', #5712 ) ;
#27216 = CARTESIAN_POINT ( 'NONE',  ( -5.934959410920000344, 1445.987167410879920, 183.4479431745980094 ) ) ;
#27218 = DIRECTION ( 'NONE',  ( -0.000000000000000000, -1.000000000000000000, -0.000000000000000000 ) ) ;
#27219 = PLANE ( 'NONE',  #49681 ) ;
#27220 = CARTESIAN_POINT ( 'NONE',  ( 2.326513286163319538, 1476.258183507229887, 197.8633931498989966 ) ) ;
#27221 = CARTESIAN_POINT ( 'NONE',  ( -24.68314314579999902, 1435.638739216969952, 137.2594662373980157 ) ) ;
#27222 = CARTESIAN_POINT ( 'NONE',  ( 6.949574947644999945, 1517.102359858469754, 212.3809477691169718 ) ) ;
#27223 = CIRCLE ( 'NONE', #66579, 1.999999999999999556 ) ;
#27224 = CARTESIAN_POINT ( 'NONE',  ( -68.27348358399999029, 1379.748432006229905, 279.1146441202590722 ) ) ;
#27225 = CARTESIAN_POINT ( 'NONE',  ( 8.631813300402768618, 1438.018477990890005, 210.0180809498099848 ) ) ;
#27226 = FACE_OUTER_BOUND ( 'NONE', #104304, .T. ) ;
#27227 = CARTESIAN_POINT ( 'NONE',  ( 21.64484447964171920, 1411.027633016495201, 201.9719268724466872 ) ) ;
#27228 = CARTESIAN_POINT ( 'NONE',  ( -0.7533003905399979772, 1516.992029636990083, 208.3816250717139837 ) ) ;
#27229 = ORIENTED_EDGE ( 'NONE', *, *, #3822, .T. ) ;
#27230 = DIRECTION ( 'NONE',  ( 0.000000000000000000, 1.000000000000000000, 0.000000000000000000 ) ) ;
#27231 = CARTESIAN_POINT ( 'NONE',  ( -10.20816227200000093, 1412.829161712830000, 229.6472676344980073 ) ) ;
#27232 = CARTESIAN_POINT ( 'NONE',  ( -54.13602515839999541, 1384.720040384200047, 270.3656545589590223 ) ) ;
#27233 = ORIENTED_EDGE ( 'NONE', *, *, #68470, .T. ) ;
#27234 = CARTESIAN_POINT ( 'NONE',  ( -11.60595113161150138, 1385.306217073230073, 218.8812244881439995 ) ) ;
#27235 = CARTESIAN_POINT ( 'NONE',  ( -3.703976537560000004, 1430.299880473189887, 201.6469541626590001 ) ) ;
#27236 = CARTESIAN_POINT ( 'NONE',  ( 11.98752746249999923, 1434.301235679619822, 150.7926998538980001 ) ) ;
#27237 = CARTESIAN_POINT ( 'NONE',  ( 18.93888774064880209, 1478.713824472059969, 228.3712757747710214 ) ) ;
#27238 = CARTESIAN_POINT ( 'NONE',  ( -21.35051360876400040, 1508.382796155649885, 227.2446047990909790 ) ) ;
#27239 = CARTESIAN_POINT ( 'NONE',  ( -2.425152001779999900, 1410.373299902729968, 186.4984030417980136 ) ) ;
#27240 = CARTESIAN_POINT ( 'NONE',  ( 0.3258471608539999509, 1410.291732689529908, 233.1866582016979805 ) ) ;
#27241 = CARTESIAN_POINT ( 'NONE',  ( 0.1518848447092220055, 1420.467538266630072, 182.7318014650070097 ) ) ;
#27243 = CARTESIAN_POINT ( 'NONE',  ( -3.423194496299999834, 1420.340339280129911, 186.2413968210979931 ) ) ;
#27242 = CARTESIAN_POINT ( 'NONE',  ( 6.944231748164999551, 1516.882690742909972, 215.6753703478370028 ) ) ;
#27244 = CARTESIAN_POINT ( 'NONE',  ( -5.485381178603089936, 1391.646552095500056, 214.9250346642329816 ) ) ;
#27245 = CARTESIAN_POINT ( 'NONE',  ( -7.329930051325000306, 1516.881930554049859, 216.8399805996670011 ) ) ;
#27246 = ORIENTED_EDGE ( 'NONE', *, *, #5587, .F. ) ;
#27247 = CARTESIAN_POINT ( 'NONE',  ( 7.329930013194999816, 1516.881930554049859, 201.4037113026670056 ) ) ;
#27248 = DIRECTION ( 'NONE',  ( -1.224646799147353947E-16, 1.836970198721029688E-16, 1.000000000000000000 ) ) ;
#27249 = ORIENTED_EDGE ( 'NONE', *, *, #61018, .F. ) ;
#27250 = CARTESIAN_POINT ( 'NONE',  ( 0.9892016712189999339, 1417.304970919730067, 235.7878985900979956 ) ) ;
#27251 = CARTESIAN_POINT ( 'NONE',  ( -17.06552703839999907, 1504.165251161390188, 208.8534522804940252 ) ) ;
#27252 = CARTESIAN_POINT ( 'NONE',  ( 7.444284895405609781, 1510.876154134890157, 202.8741411524250111 ) ) ;
#27253 = CARTESIAN_POINT ( 'NONE',  ( 3.060046444349999728, 1442.201648410489952, 217.5704250855989983 ) ) ;
#27254 = CARTESIAN_POINT ( 'NONE',  ( -30.31052258194604576, 1523.604703353109699, 195.7506062427372058 ) ) ;
#27255 = CARTESIAN_POINT ( 'NONE',  ( 1966.210325831229966, 11216.44053380570040, 439.9203465415980077 ) ) ;
#27256 = DIRECTION ( 'NONE',  ( -0.9993902469236103370, -0.03489947644258441228, 0.001077449766195770313 ) ) ;
#27257 = CARTESIAN_POINT ( 'NONE',  ( -18.75767574410000194, 1425.635095768630208, 226.0811886220980114 ) ) ;
#27258 = CARTESIAN_POINT ( 'NONE',  ( -17.30326228670000077, 1435.529124648550123, 147.5648915083980057 ) ) ;
#27259 = CARTESIAN_POINT ( 'NONE',  ( -11.89544747750000120, 1434.541746328260160, 147.6465872843980094 ) ) ;
#27260 = CARTESIAN_POINT ( 'NONE',  ( 7.012921545624998920, 1508.551704408389924, 214.6352815241970120 ) ) ;
#27262 = CARTESIAN_POINT ( 'NONE',  ( -19.05726004021619957, 1440.248441431409674, 209.7973887611863688 ) ) ;
#27261 = DIRECTION ( 'NONE',  ( 5.980589973904019347E-17, -1.000000000000000000, 1.736889445713099699E-16 ) ) ;
#27263 = CARTESIAN_POINT ( 'NONE',  ( 0.8350686643532179154, 1526.382868172863937, 240.9330574173806951 ) ) ;
#27264 = ORIENTED_EDGE ( 'NONE', *, *, #72631, .F. ) ;
#27265 = CARTESIAN_POINT ( 'NONE',  ( 1.554710334620659884, 1415.393085341110009, 190.9507836336619846 ) ) ;
#27266 = CARTESIAN_POINT ( 'NONE',  ( 22.77022259470000165, 1411.047177419029822, 206.9289107030080004 ) ) ;
#27267 = CARTESIAN_POINT ( 'NONE',  ( -11.93818408299999945, 1433.480074519959999, 149.8972116839979947 ) ) ;
#27268 = CARTESIAN_POINT ( 'NONE',  ( 3.015935646565480077, 1410.395869510137345, 185.7231583079203290 ) ) ;
#27269 = CARTESIAN_POINT ( 'NONE',  ( -3.975393244031079742, 1426.016855281922062, 186.0738092297652884 ) ) ;
#27270 = CARTESIAN_POINT ( 'NONE',  ( -14.17716072747469980, 1509.408135630319975, 183.2983236682360086 ) ) ;
#27271 = CARTESIAN_POINT ( 'NONE',  ( -4.458756895905489515, 1488.529440655459894, 219.1126515454099888 ) ) ;
#27272 = CARTESIAN_POINT ( 'NONE',  ( -19.34949465300000071, 1446.106505183189938, 200.0047805777890062 ) ) ;
#27274 = EDGE_CURVE ( 'NONE', #8025, #21719, #16964, .T. ) ;
#27273 = CARTESIAN_POINT ( 'NONE',  ( -91.29898430540859522, 1383.769499161590147, 308.9254833966310230 ) ) ;
#27275 = CARTESIAN_POINT ( 'NONE',  ( -109.1111907142439890, 1384.583402408000211, 311.2497943572710142 ) ) ;
#27276 = FACE_OUTER_BOUND ( 'NONE', #13396, .T. ) ;
#27277 = CARTESIAN_POINT ( 'NONE',  ( -23.55007224577885339, 1410.927093357725198, 210.4721751823504690 ) ) ;
#27279 = ORIENTED_EDGE ( 'NONE', *, *, #76917, .T. ) ;
#27278 = CARTESIAN_POINT ( 'NONE',  ( 1.711055448681089940E-31, 1424.874073124720098, 209.1218459616989946 ) ) ;
#27280 = CARTESIAN_POINT ( 'NONE',  ( -17.96439385675617828, 1459.774127481555070, 228.0505170696288246 ) ) ;
#27281 = CARTESIAN_POINT ( 'NONE',  ( -83.50618377039999984, 1381.859495333320183, 288.7003657451589902 ) ) ;
#27282 = FACE_BOUND ( 'NONE', #82137, .T. ) ;
#27283 = EDGE_CURVE ( 'NONE', #94338, #1934, #24169, .T. ) ;
#27284 = ORIENTED_EDGE ( 'NONE', *, *, #14136, .F. ) ;
#27285 = ORIENTED_EDGE ( 'NONE', *, *, #74064, .T. ) ;
#27286 = CARTESIAN_POINT ( 'NONE',  ( 20.01964129088910127, 1509.548583382980041, 230.4035799795959747 ) ) ;
#27287 = B_SPLINE_CURVE_WITH_KNOTS ( 'NONE', 3,
 ( #98920, #105134, #72115, #98373, #105699, #21645, #55853, #13246, #47436, #73183 ),
 .UNSPECIFIED., .F., .F.,
 ( 4, 3, 3, 4 ),
 ( -3.121899831669039838, -2.863851907766889582, -1.429084544020210013, 4.440892098500626162E-16 ),
 .UNSPECIFIED. ) ;
#27288 = CARTESIAN_POINT ( 'NONE',  ( -19.15307798683139850, 1464.559873833900156, 213.8318764457040118 ) ) ;
#27289 = CARTESIAN_POINT ( 'NONE',  ( 6.824596748387858014, 1424.393356309073852, 213.4892280596932892 ) ) ;
#27291 = CARTESIAN_POINT ( 'NONE',  ( -30.10637269909999958, 1468.180606183130067, 266.8104569320979635 ) ) ;
#27290 = DIRECTION ( 'NONE',  ( 0.6665120492724535550, 0.000000000000000000, -0.7454942576402816545 ) ) ;
#27292 = CARTESIAN_POINT ( 'NONE',  ( 9.357192914159959685, 1435.432353859119985, 208.4552369967489938 ) ) ;
#27293 = CARTESIAN_POINT ( 'NONE',  ( -107.8906272039999976, 1382.782317645739795, 297.7506189441589868 ) ) ;
#27294 = CARTESIAN_POINT ( 'NONE',  ( 28.51851353229999830, 1509.908948824629988, 203.7504615519080176 ) ) ;
#27295 = CARTESIAN_POINT ( 'NONE',  ( -19.94044037020000104, 1485.838040724430130, 190.5384349266980166 ) ) ;
#27296 = CARTESIAN_POINT ( 'NONE',  ( 2.896135874330000082, 1409.181763743129977, 186.2668185386979758 ) ) ;
#27297 = CARTESIAN_POINT ( 'NONE',  ( 5.855088903640000453, 1423.239027948129888, 186.0981068077980183 ) ) ;
#27298 = CARTESIAN_POINT ( 'NONE',  ( -5.630091727850000005, 1441.487383650409811, 154.7801822665980183 ) ) ;
#27299 = CARTESIAN_POINT ( 'NONE',  ( 12.15187854179999860, 1435.108173852649770, 151.0159323405979990 ) ) ;
#27300 = CARTESIAN_POINT ( 'NONE',  ( -16.32813191276419928, 1420.694869237870080, 203.2969751068219750 ) ) ;
#27301 = CARTESIAN_POINT ( 'NONE',  ( -11.12609304200080018, 1491.160356735590085, 209.7795734073339986 ) ) ;
#27302 = CARTESIAN_POINT ( 'NONE',  ( -15.94347048536829803, 1409.469818645040050, 192.9752432267480060 ) ) ;
#27303 = ORIENTED_EDGE ( 'NONE', *, *, #65857, .F. ) ;
#27304 = CARTESIAN_POINT ( 'NONE',  ( -12.45097904980000081, 1507.808706184189987, 209.1434958805429858 ) ) ;
#27305 = CARTESIAN_POINT ( 'NONE',  ( -2.893915299462510138, 1469.660611638019873, 187.4298741930020071 ) ) ;
#27306 = CARTESIAN_POINT ( 'NONE',  ( -43.12011480509999473, 1450.389500078439823, 269.9366955693979548 ) ) ;
#27307 = CARTESIAN_POINT ( 'NONE',  ( -27.27137786365319982, 1446.453610550540134, 137.2094999256019889 ) ) ;
#27308 = CARTESIAN_POINT ( 'NONE',  ( 17.60618138139999900, 1410.892634160230045, 223.9222036297979912 ) ) ;
#27309 = CARTESIAN_POINT ( 'NONE',  ( -15.13234893939999992, 1485.042171593129979, 224.0148604844980014 ) ) ;
#27310 = CARTESIAN_POINT ( 'NONE',  ( 5.164876290100000489, 1519.913060387329779, 186.3413721456980170 ) ) ;
#27311 = CARTESIAN_POINT ( 'NONE',  ( -13.58235846979999906, 1416.828040475229955, 221.9087530951979659 ) ) ;
#27312 = CARTESIAN_POINT ( 'NONE',  ( -6.554764199473687825, 1516.786099426707551, 201.4062207776168236 ) ) ;
#27313 = CARTESIAN_POINT ( 'NONE',  ( -3.076054745830000048, 1415.755548294329856, 232.7548256247980021 ) ) ;
#27314 = CARTESIAN_POINT ( 'NONE',  ( -10.06805134449999883, 1461.229810737490197, 212.3649339894689945 ) ) ;
#27315 = CARTESIAN_POINT ( 'NONE',  ( -0.7618909056619500575, 1360.403425203269990, 210.6218459616991936 ) ) ;
#27316 = CARTESIAN_POINT ( 'NONE',  ( -45.75888640774939375, 1437.122255822999932, 268.5047239448639971 ) ) ;
#27317 = DIRECTION ( 'NONE',  ( 1.000000000000000000, 0.000000000000000000, 0.000000000000000000 ) ) ;
#27318 = ORIENTED_EDGE ( 'NONE', *, *, #103453, .F. ) ;
#27319 = CARTESIAN_POINT ( 'NONE',  ( -8.116268411100000080, 1423.917527323469812, 210.3428539577589902 ) ) ;
#27320 = ORIENTED_EDGE ( 'NONE', *, *, #11684, .F. ) ;
#27321 = CARTESIAN_POINT ( 'NONE',  ( 1.717139084115000047, 1516.949031626070109, 210.2396860569670025 ) ) ;
#27322 = CARTESIAN_POINT ( 'NONE',  ( 19.44117294853580091, 1456.941945407359981, 224.4539793896520052 ) ) ;
#27323 = CARTESIAN_POINT ( 'NONE',  ( -11.00204100220000036, 1410.396409030930045, 188.8227745368980379 ) ) ;
#27324 = DIRECTION ( 'NONE',  ( 1.755985294532464991E-16, -1.000000000000000000, 1.338183447452830017E-16 ) ) ;
#27325 = ORIENTED_EDGE ( 'NONE', *, *, #83079, .T. ) ;
#27326 = CARTESIAN_POINT ( 'NONE',  ( -15.03597275369999942, 1488.809466528929988, 194.0187079571979893 ) ) ;
#27328 = CARTESIAN_POINT ( 'NONE',  ( 14.40805950830000093, 1470.815019615529991, 194.5894316583980128 ) ) ;
#27327 = CARTESIAN_POINT ( 'NONE',  ( -2.472529913803048984, 1523.678648413191922, 175.3762130535718597 ) ) ;
#27329 = CARTESIAN_POINT ( 'NONE',  ( 1.429289317213857879, 1487.311642763506370, 219.8598652476721611 ) ) ;
#27330 = LINE ( 'NONE', #61516, #78343 ) ;
#27331 = DIRECTION ( 'NONE',  ( -0.7600087925167848812, -0.4999999999970536346, 0.4151946956550925383 ) ) ;
#27332 = CARTESIAN_POINT ( 'NONE',  ( -8.565099867639800024, 1437.917637130210096, 207.7375823160310233 ) ) ;
#27333 = ORIENTED_EDGE ( 'NONE', *, *, #63222, .F. ) ;
#27334 = CARTESIAN_POINT ( 'NONE',  ( -3.114907484115349678, 1408.000211163370068, 270.2910159990690317 ) ) ;
#27335 = CARTESIAN_POINT ( 'NONE',  ( -0.01012492377659850000, 1516.989863902050047, 207.9939175986969815 ) ) ;
#27336 = CARTESIAN_POINT ( 'NONE',  ( 4.187645461488620491, 1418.024921168729861, 233.4325071608510029 ) ) ;
#27337 = CARTESIAN_POINT ( 'NONE',  ( -0.3886416839960190606, 1508.683136490621791, 238.1396719883204298 ) ) ;
#27339 = ORIENTED_EDGE ( 'NONE', *, *, #77699, .T. ) ;
#27338 = CARTESIAN_POINT ( 'NONE',  ( -8.624710350820000926, 1367.191948709370081, 207.6218459616989946 ) ) ;
#27340 = ORIENTED_EDGE ( 'NONE', *, *, #5020, .T. ) ;
#27341 = CARTESIAN_POINT ( 'NONE',  ( -32.02808312589930040, 1512.187213306747481, 196.2787714533499752 ) ) ;
#27342 = CARTESIAN_POINT ( 'NONE',  ( -3.956504371649999463, 1424.255369803030135, 185.4171806679979966 ) ) ;
#27343 = CARTESIAN_POINT ( 'NONE',  ( 3.690176726703637389, 1424.194312783380838, 183.9655579347969478 ) ) ;
#27344 = CARTESIAN_POINT ( 'NONE',  ( 18.58525782085794731, 1474.564397078151160, 201.0252237832114020 ) ) ;
#27345 = B_SPLINE_CURVE_WITH_KNOTS ( 'NONE', 5,
 ( #99842, #41048, #92007, #93100, #101483, #47808 ),
 .UNSPECIFIED., .F., .F.,
 ( 6, 6 ),
 ( -2.000000000000000000, -8.403479023755267008E-09 ),
 .UNSPECIFIED. ) ;
#27346 = CARTESIAN_POINT ( 'NONE',  ( -17.99954540876850118, 1410.904693920620048, 195.2564682659330231 ) ) ;
#27347 = CARTESIAN_POINT ( 'NONE',  ( -18.31548309940000152, 1420.838217743430050, 225.0570179786980134 ) ) ;
#27348 = CARTESIAN_POINT ( 'NONE',  ( 32.87669591961419968, 1465.269253061860127, 266.5396782138440130 ) ) ;
#27349 = EDGE_CURVE ( 'NONE', #98891, #42640, #621, .T. ) ;
#27350 = CARTESIAN_POINT ( 'NONE',  ( -7.438002979262030578, 1465.685359695273746, 233.5328670419079344 ) ) ;
#27351 = CARTESIAN_POINT ( 'NONE',  ( 7.201451958809999887, 1447.808573296560098, 185.4041577039979813 ) ) ;
#27352 = CARTESIAN_POINT ( 'NONE',  ( 5.771797426184999580, 1516.647618671360078, 206.2459958378869942 ) ) ;
#27353 = ORIENTED_EDGE ( 'NONE', *, *, #105647, .T. ) ;
#27354 = CARTESIAN_POINT ( 'NONE',  ( 21.73282879226712083, 1411.032371074868252, 216.6638630078411438 ) ) ;
#27355 = CARTESIAN_POINT ( 'NONE',  ( -3.644878300669852855, 1516.661627594551419, 202.5664891927213489 ) ) ;
#27356 = CARTESIAN_POINT ( 'NONE',  ( 23.65254864839999982, 1410.841227188329867, 207.9071628193579784 ) ) ;
#27357 = ORIENTED_EDGE ( 'NONE', *, *, #79156, .T. ) ;
#27358 = CARTESIAN_POINT ( 'NONE',  ( 3.829619994797929916, 1515.551704292389786, 207.2788821832570250 ) ) ;
#27359 = EDGE_CURVE ( 'NONE', #38027, #17126, #29139, .T. ) ;
#27360 = CARTESIAN_POINT ( 'NONE',  ( 24.93611935033429816, 1452.026605045649831, 135.8540817300889785 ) ) ;
#27361 = ADVANCED_FACE ( 'NONE', ( #100837 ), #67283, .T. ) ;
#27362 = CARTESIAN_POINT ( 'NONE',  ( 11.87563352516160009, 1433.006677200080048, 147.6591433499779953 ) ) ;
#27363 = CARTESIAN_POINT ( 'NONE',  ( -1.036208156320000032E-15, 1384.913060387289988, 199.6218459572590120 ) ) ;
#27364 = CARTESIAN_POINT ( 'NONE',  ( 7.513730101630000213, 1422.952558782609913, 195.6781497891990114 ) ) ;
#27365 = CARTESIAN_POINT ( 'NONE',  ( 17.38484768960000082, 1410.884447801129909, 192.4603983160980079 ) ) ;
#27366 = CARTESIAN_POINT ( 'NONE',  ( -3.560962994120000058, 1496.007316878489974, 198.0872883060989977 ) ) ;
#27367 = CARTESIAN_POINT ( 'NONE',  ( 3.280909904081581008, 1439.687164527259256, 184.3576248092443848 ) ) ;
#27369 = CARTESIAN_POINT ( 'NONE',  ( -19.08455381886165014, 1425.050945183270869, 224.0897855658817832 ) ) ;
#27368 = CARTESIAN_POINT ( 'NONE',  ( -0.01332681072910000056, 1417.281753988030005, 234.8503422950979882 ) ) ;
#27370 = CARTESIAN_POINT ( 'NONE',  ( 0.7437212546499240018, 1452.305686085940124, 183.2916024963490145 ) ) ;
#27371 = DIRECTION ( 'NONE',  ( -5.980589973904019347E-17, 1.000000000000000000, -1.736889445713099699E-16 ) ) ;
#27372 = CARTESIAN_POINT ( 'NONE',  ( -8.687735435529999606, 1383.717527281549792, 218.5005275664289854 ) ) ;
#27373 = CARTESIAN_POINT ( 'NONE',  ( 1.713317409674999903, 1516.660388280709867, 213.7298676393670291 ) ) ;
#27374 = DIRECTION ( 'NONE',  ( 0.5117323852941357831, -0.8591449038673127925, 0.000000000000000000 ) ) ;
#27375 = VERTEX_POINT ( 'NONE', #76761 ) ;
#27376 = CARTESIAN_POINT ( 'NONE',  ( -17.14979733940000273, 1417.522661905800078, 207.4349891442189744 ) ) ;
#27377 = B_SPLINE_SURFACE_WITH_KNOTS ( 'NONE', 5, 5, ( 
 ( #42394, #92799, #85482, #101736, #83300, #93891 ),
 ( #25024, #50805, #42963, #110704, #33996, #102293 ),
 ( #40744, #17157, #429, #34548, #74920, #32352 ),
 ( #49716, #66531, #100635, #95015, #26692, #54143 ),
 ( #94436, #61994, #96678, #77662, #104515, #19950 ),
 ( #36763, #103959, #11013, #78206, #87735, #28361 ),
 ( #53589, #60318, #69841, #26129, #35099, #96112 ),
 ( #87164, #44627, #45184, #18833, #1518, #17715 ),
 ( #62558, #95563, #35651, #44067, #36212, #88272 ) ),
 .UNSPECIFIED., .F., .F., .F.,
 ( 6, 3, 6 ),
 ( 6, 6 ),
 ( 0.7655572723410000169, 2.316155491860000026, 3.835724788519999873 ),
 ( 0.000000000000000000, 1.000000000000000000 ),
 .UNSPECIFIED. ) ;
#27378 = CARTESIAN_POINT ( 'NONE',  ( 21.19880661589024839, 1524.382868172863937, 233.5487980989310302 ) ) ;
#27379 = CARTESIAN_POINT ( 'NONE',  ( -0.5153922977329320476, 1410.146051047059700, 233.1556763689120260 ) ) ;
#27380 = CARTESIAN_POINT ( 'NONE',  ( -20.23414992579679605, 1508.068540423656941, 209.5914070171807850 ) ) ;
#27381 = CARTESIAN_POINT ( 'NONE',  ( -34.50882828746139808, 1450.391922407039829, 136.2327768001300115 ) ) ;
#27382 = CARTESIAN_POINT ( 'NONE',  ( -0.1909393205278206718, 1506.691119452750399, 231.3199018796742337 ) ) ;
#27383 = B_SPLINE_CURVE_WITH_KNOTS ( 'NONE', 3,
 ( #41714, #84263, #84803, #62273, #59633, #7560, #25440, #42269, #8102, #10182 ),
 .UNSPECIFIED., .F., .F.,
 ( 4, 2, 2, 2, 4 ),
 ( 0.000000000000000000, 0.02214642915447170152, 0.06470200879455109688, 0.1010821742375619947, 0.1380341206303599966 ),
 .UNSPECIFIED. ) ;
#27384 = CARTESIAN_POINT ( 'NONE',  ( -6.215408291060000145, 1454.402584563930077, 214.3676144191779827 ) ) ;
#27385 = CARTESIAN_POINT ( 'NONE',  ( 35.50739915879996289, 1462.949854392428279, 266.4727958076973664 ) ) ;
#27386 = CARTESIAN_POINT ( 'NONE',  ( 11.87502391619999997, 1433.007272034859852, 149.9804603544980068 ) ) ;
#27387 = CARTESIAN_POINT ( 'NONE',  ( 18.41412373400000035, 1444.997163189090088, 209.1218459616979999 ) ) ;
#27388 = CARTESIAN_POINT ( 'NONE',  ( -9.556981692808550477, 1460.090769935110075, 210.4171492488110005 ) ) ;
#27389 = CARTESIAN_POINT ( 'NONE',  ( 3.217394093085149898, 1424.184525167369884, 188.9579921258149966 ) ) ;
#27390 = DIRECTION ( 'NONE',  ( -1.000000000000000000, 0.000000000000000000, 0.000000000000000000 ) ) ;
#27391 = CARTESIAN_POINT ( 'NONE',  ( 9.957354707566970831, 1462.547202367510181, 211.2474092644970085 ) ) ;
#27392 = CARTESIAN_POINT ( 'NONE',  ( 22.71938917269999791, 1409.706427035829847, 209.1785880919549925 ) ) ;
#27393 = CARTESIAN_POINT ( 'NONE',  ( -30.02739323485179668, 1510.039195650590045, 211.8782729601720121 ) ) ;
#27394 = CARTESIAN_POINT ( 'NONE',  ( 25.48925201540000174, 1449.802587353020044, 210.7369667112079981 ) ) ;
#27395 = CARTESIAN_POINT ( 'NONE',  ( 29.99620953741496976, 1526.382868172863937, 219.7462484079458704 ) ) ;
#27396 = CARTESIAN_POINT ( 'NONE',  ( -40.27308906366239682, 1443.612067134240078, 137.1163379626329970 ) ) ;
#27397 = CARTESIAN_POINT ( 'NONE',  ( -25.73187104542529724, 1383.847228980049977, 224.0191246321959682 ) ) ;
#27398 = CARTESIAN_POINT ( 'NONE',  ( -13.67845548232380004, 1504.250296044910101, 227.6838177328889969 ) ) ;
#27399 = CARTESIAN_POINT ( 'NONE',  ( 3.459156578084999989, 1516.769879638719885, 213.7318425517769924 ) ) ;
#27400 = CARTESIAN_POINT ( 'NONE',  ( -11.71402071852000049, 1489.483213258419937, 212.5376296399540195 ) ) ;
#27401 = CARTESIAN_POINT ( 'NONE',  ( 0.1676281277942339998, 1481.725157098900127, 182.0202826403800032 ) ) ;
#27403 = EDGE_LOOP ( 'NONE', ( #56434, #110182 ) ) ;
#27402 = FACE_OUTER_BOUND ( 'NONE', #38074, .T. ) ;
#27404 = CARTESIAN_POINT ( 'NONE',  ( 12.48894518679548860, 1384.913060387289988, 208.5962528435125591 ) ) ;
#27405 = CARTESIAN_POINT ( 'NONE',  ( -8.830847595988496224, 1387.926285407787191, 200.3861648232594348 ) ) ;
#27406 = CARTESIAN_POINT ( 'NONE',  ( -4.016810458580000187, 1476.004922423390099, 199.5922506328190025 ) ) ;
#27407 = EDGE_CURVE ( 'NONE', #87891, #84881, #108194, .T. ) ;
#27409 = ORIENTED_EDGE ( 'NONE', *, *, #99050, .F. ) ;
#27408 = CARTESIAN_POINT ( 'NONE',  ( -37.29624469558390132, 1450.849357696489960, 134.0999999986649698 ) ) ;
#27410 = CARTESIAN_POINT ( 'NONE',  ( -7.003352422824639767, 1508.551704404799921, 219.1865514027120128 ) ) ;
#27411 = ORIENTED_EDGE ( 'NONE', *, *, #63941, .F. ) ;
#27412 = CARTESIAN_POINT ( 'NONE',  ( -14.31906343784990021, 1380.323795378649947, 209.9058136714729983 ) ) ;
#27413 = CARTESIAN_POINT ( 'NONE',  ( -16.63199885160000235, 1416.518938592030054, 216.8695166334780140 ) ) ;
#27414 = DIRECTION ( 'NONE',  ( 0.000000000000000000, 1.000000000000000000, 0.000000000000000000 ) ) ;
#27415 = CARTESIAN_POINT ( 'NONE',  ( -1.430539319850000046, 1444.328264637789971, 199.1703804529689990 ) ) ;
#27416 = CARTESIAN_POINT ( 'NONE',  ( 0.2166670160139989865, 1431.553687047090079, 218.2358754814289910 ) ) ;
#27417 = CARTESIAN_POINT ( 'NONE',  ( -12.23669307423070052, 1377.661331666050273, 207.7794331870949804 ) ) ;
#27418 = CARTESIAN_POINT ( 'NONE',  ( 14.58630151190530100, 1409.422425260170030, 205.9107706399979918 ) ) ;
#27419 = CARTESIAN_POINT ( 'NONE',  ( -10.82437014639999973, 1391.913060387289988, 205.5047960701089949 ) ) ;
#27420 = CARTESIAN_POINT ( 'NONE',  ( -87.72787637423360252, 1385.185452115049884, 291.0380262421580255 ) ) ;
#27421 = CARTESIAN_POINT ( 'NONE',  ( -17.00586071620000084, 1421.470251449630041, 191.4405153155979917 ) ) ;
#27422 = CARTESIAN_POINT ( 'NONE',  ( -65.82430152899999598, 1379.749194687180079, 274.2810710116589803 ) ) ;
#27423 = ORIENTED_EDGE ( 'NONE', *, *, #82010, .F. ) ;
#27424 = CARTESIAN_POINT ( 'NONE',  ( 11.13284031615599901, 1491.007009142829929, 208.5102145449120030 ) ) ;
#27426 = EDGE_LOOP ( 'NONE', ( #38880, #47588, #51708, #81729 ) ) ;
#27425 = DIRECTION ( 'NONE',  ( -0.9455185755993178454, 0.000000000000000000, 0.3255681544571537578 ) ) ;
#27427 = CARTESIAN_POINT ( 'NONE',  ( 8.937899474855068860, 1465.013579540770252, 213.2848641858089991 ) ) ;
#27428 = EDGE_LOOP ( 'NONE', ( #101138, #3345, #64341, #88249 ) ) ;
#27429 = CARTESIAN_POINT ( 'NONE',  ( 22.39346815460000428, 1508.437849850330167, 224.3979271850979842 ) ) ;
#27430 = CARTESIAN_POINT ( 'NONE',  ( 6.113148423521039376, 1363.477843159564372, 209.6218459617148824 ) ) ;
#27431 = CARTESIAN_POINT ( 'NONE',  ( -0.7474653422925290336, 1496.370314053810034, 196.7891267297500235 ) ) ;
#27432 = B_SPLINE_CURVE_WITH_KNOTS ( 'NONE', 3,
 ( #31764, #109588, #32858, #58639, #16048, #67598, #91674, #101706, #24998, #57551, #50778, #8203 ),
 .UNSPECIFIED., .F., .F.,
 ( 4, 2, 2, 2, 2, 4 ),
 ( 0.000000000000000000, 0.0007194225121803534111, 0.001079133768270215590, 0.001438845024360077551, 0.002158267536539286695, 0.002877690048718496273 ),
 .UNSPECIFIED. ) ;
#27433 = CARTESIAN_POINT ( 'NONE',  ( 29.83189240543555698, 1462.372292350401267, 269.4690225947026647 ) ) ;
#27434 = CARTESIAN_POINT ( 'NONE',  ( -32.09235212274860771, 1525.402221411349046, 221.9833860708173461 ) ) ;
#27435 = CARTESIAN_POINT ( 'NONE',  ( -0.001991323853590000036, 1395.912990848829850, 220.4358217571979992 ) ) ;
#27436 = CARTESIAN_POINT ( 'NONE',  ( 32.79520046278974377, 1523.954924407802309, 201.0814700520839438 ) ) ;
#27437 = CARTESIAN_POINT ( 'NONE',  ( 22.28696231330000188, 1506.798305107829947, 209.3970118511340104 ) ) ;
#27438 = CARTESIAN_POINT ( 'NONE',  ( -1.452061816759999902, 1467.474562141730075, 183.2045861867980250 ) ) ;
#27439 = CARTESIAN_POINT ( 'NONE',  ( -7.450033292398919649, 1367.931913175455975, 210.6218459616991936 ) ) ;
#27440 = CARTESIAN_POINT ( 'NONE',  ( -8.652776130911478347, 1511.435001053830092, 214.5073691320910143 ) ) ;
#27441 = CARTESIAN_POINT ( 'NONE',  ( 10.81507089421240053, 1424.921187596799882, 144.1620444706739761 ) ) ;
#27442 = EDGE_CURVE ( 'NONE', #40850, #19317, #88548, .T. ) ;
#27443 = CARTESIAN_POINT ( 'NONE',  ( -0.7579844201469989606, 1516.883361325900069, 206.8353730456769881 ) ) ;
#27444 = CARTESIAN_POINT ( 'NONE',  ( -32.02808312589908013, 1512.187213306747481, 219.9649204700466782 ) ) ;
#27445 = FACE_OUTER_BOUND ( 'NONE', #23945, .T. ) ;
#27446 = CARTESIAN_POINT ( 'NONE',  ( 6.721801505100000185, 1474.175172799430129, 270.1377427386980230 ) ) ;
#27448 = ORIENTED_EDGE ( 'NONE', *, *, #67347, .T. ) ;
#27447 = CARTESIAN_POINT ( 'NONE',  ( 1.060739532880000002, 1494.110723351890101, 220.2175052815989886 ) ) ;
#27449 = CARTESIAN_POINT ( 'NONE',  ( 40.49318544340329851, 1444.190211223800134, 137.0748560406749732 ) ) ;
#27450 = ORIENTED_EDGE ( 'NONE', *, *, #86810, .F. ) ;
#27451 = CARTESIAN_POINT ( 'NONE',  ( 9.989727630039999957E-09, 1407.100401496229779, 264.8986986722979964 ) ) ;
#27452 = CARTESIAN_POINT ( 'NONE',  ( -27.42581371189999828, 1488.692458008330050, 208.8841174044290199 ) ) ;
#27454 = CARTESIAN_POINT ( 'NONE',  ( 16.52699712982959923, 1409.590692121840220, 192.7142616149739922 ) ) ;
#27453 = CARTESIAN_POINT ( 'NONE',  ( -1.545285848170000031, 1504.644139859730103, 180.9077348290979899 ) ) ;
#27455 = CARTESIAN_POINT ( 'NONE',  ( 6.561995960394999550, 1517.083030555940013, 212.3803205491769859 ) ) ;
#27456 = CARTESIAN_POINT ( 'NONE',  ( -13.73040296198626997, 1519.551704408389924, 190.6090220189334445 ) ) ;
#27457 = CARTESIAN_POINT ( 'NONE',  ( -29.66529950410000183, 1430.834809504130135, 244.2516413604979846 ) ) ;
#27458 = CARTESIAN_POINT ( 'NONE',  ( -12.35054461905689926, 1378.471275783050260, 209.3240372099530191 ) ) ;
#27459 = CARTESIAN_POINT ( 'NONE',  ( 28.86205551402650116, 1509.507027960610003, 209.5284224540439766 ) ) ;
#27460 = CARTESIAN_POINT ( 'NONE',  ( 4.240165130249540226, 1508.551704408389924, 213.3930704938919973 ) ) ;
#27461 = CARTESIAN_POINT ( 'NONE',  ( 30.82338973599999932, 1451.683219239730079, 135.6778805674979935 ) ) ;
#27462 = VERTEX_POINT ( 'NONE', #26912 ) ;
#27463 = CARTESIAN_POINT ( 'NONE',  ( 8.020322465218489683, 1396.252981828660040, 218.0167330499769776 ) ) ;
#27464 = CARTESIAN_POINT ( 'NONE',  ( 10.41168706946910127, 1460.024584131529764, 205.9060538633809756 ) ) ;
#27465 = CARTESIAN_POINT ( 'NONE',  ( -17.14944014479999979, 1460.897692083130096, 228.2718297098980145 ) ) ;
#27466 = ORIENTED_EDGE ( 'NONE', *, *, #9792, .T. ) ;
#27467 = ORIENTED_EDGE ( 'NONE', *, *, #50775, .F. ) ;
#27468 = CARTESIAN_POINT ( 'NONE',  ( 9.367229934758190879, 1453.004463604660259, 211.8810869144209903 ) ) ;
#27469 = CARTESIAN_POINT ( 'NONE',  ( 7.975553363950000474, 1424.201270073840078, 195.7335007005989951 ) ) ;
#27470 = VERTEX_POINT ( 'NONE', #80064 ) ;
#27471 = CARTESIAN_POINT ( 'NONE',  ( 0.09171298916310000049, 1419.319896810129876, 184.5979190233979921 ) ) ;
#27472 = CARTESIAN_POINT ( 'NONE',  ( -2.518203147932353225, 1420.414483601807888, 193.9149677586775908 ) ) ;
#27473 = LINE ( 'NONE', #61663, #67255 ) ;
#27474 = CARTESIAN_POINT ( 'NONE',  ( -1.739071167590000133, 1461.196621557430035, 235.0776999716979958 ) ) ;
#27475 = CARTESIAN_POINT ( 'NONE',  ( 5.513199790315740145, 1509.038617475689989, 201.6090956973179971 ) ) ;
#27476 = EDGE_CURVE ( 'NONE', #71414, #64503, #17995, .T. ) ;
#27477 = SURFACE_STYLE_FILL_AREA ( #95244 ) ;
#27478 = EDGE_CURVE ( 'NONE', #94274, #22497, #86027, .T. ) ;
#27479 = DIRECTION ( 'NONE',  ( -0.9099290007293374671, 0.3041652670682291060, 0.2819799708153441498 ) ) ;
#27480 = CARTESIAN_POINT ( 'NONE',  ( 15.20160463690000086, 1496.666401959530049, 225.6166776728979642 ) ) ;
#27481 = EDGE_LOOP ( 'NONE', ( #48088, #86146, #8448, #25432 ) ) ;
#27482 =( BOUNDED_CURVE ( )  B_SPLINE_CURVE ( 3, ( #22848, #48653, #15001, #32383 ),
 .UNSPECIFIED., .F., .T. ) 
 B_SPLINE_CURVE_WITH_KNOTS ( ( 4, 4 ),
 ( 4.177898496904434822, 5.246901655145340015 ),
 .UNSPECIFIED. ) 
 CURVE ( )  GEOMETRIC_REPRESENTATION_ITEM ( )  RATIONAL_B_SPLINE_CURVE ( ( 1.000000000000000000, 0.9070150918854136268, 0.9070150918854136268, 1.000000000000000000 ) ) 
 REPRESENTATION_ITEM ( '' )  );
#27483 = CARTESIAN_POINT ( 'NONE',  ( -5.006329619514999330, 1516.755758396839838, 202.5714564999769891 ) ) ;
#27484 = CARTESIAN_POINT ( 'NONE',  ( -0.7374509209069979310, 1516.978425811520083, 210.2554991112269818 ) ) ;
#27485 = VERTEX_POINT ( 'NONE', #105835 ) ;
#27487 = ADVANCED_FACE ( 'NONE', ( #1731 ), #25933, .T. ) ;
#27486 = CARTESIAN_POINT ( 'NONE',  ( 11.86328075526730075, 1432.138978093059904, 149.9787975337250145 ) ) ;
#27488 = CARTESIAN_POINT ( 'NONE',  ( 12.66538237952104673, 1445.025812281660365, 186.3114105575668304 ) ) ;
#27489 = EDGE_LOOP ( 'NONE', ( #57202, #7238, #4622, #82710 ) ) ;
#27490 = CARTESIAN_POINT ( 'NONE',  ( -15.81201443571409904, 1506.433683733589987, 193.8503163142329981 ) ) ;
#27491 = ADVANCED_FACE ( 'NONE', ( #45390 ), #16179, .T. ) ;
#27492 = CARTESIAN_POINT ( 'NONE',  ( -17.22623662315568893, 1443.913060387331598, 162.9225832754749490 ) ) ;
#27493 = CARTESIAN_POINT ( 'NONE',  ( 6.918620528049999940, 1507.562034369630055, 235.3523762123979850 ) ) ;
#27494 = ADVANCED_FACE ( 'NONE', ( #44147 ), #1595, .F. ) ;
#27495 = CARTESIAN_POINT ( 'NONE',  ( -3.950491156583319619, 1468.310306949679898, 219.6290600318629913 ) ) ;
#27496 = CARTESIAN_POINT ( 'NONE',  ( -5.866240475749999739, 1421.246203026429839, 186.6777796954980033 ) ) ;
#27497 = CARTESIAN_POINT ( 'NONE',  ( 2.303607911415140208, 1408.601389339190064, 270.4285322758109942 ) ) ;
#27498 = CARTESIAN_POINT ( 'NONE',  ( -9.380124768717641004, 1428.163396101657781, 137.0999999980979851 ) ) ;
#27499 = LINE ( 'NONE', #44322, #90654 ) ;
#27500 = CARTESIAN_POINT ( 'NONE',  ( -2.262341589641910122, 1421.834387796660167, 193.3950565057020015 ) ) ;
#27501 = CARTESIAN_POINT ( 'NONE',  ( -14.16433532520000149, 1379.580334929220044, 207.9040437273089879 ) ) ;
#27502 = CARTESIAN_POINT ( 'NONE',  ( 9.028476196572741586, 1425.072251678628390, 195.6284098769293678 ) ) ;
#27503 = EDGE_CURVE ( 'NONE', #98841, #4207, #19599, .T. ) ;
#27505 = CARTESIAN_POINT ( 'NONE',  ( 14.00912961620000097, 1416.839648768830102, 196.3913569366980028 ) ) ;
#27504 = CARTESIAN_POINT ( 'NONE',  ( -17.55491153119999836, 1504.812299793789862, 208.9605407232600101 ) ) ;
#27506 = CARTESIAN_POINT ( 'NONE',  ( -4.833007409577117386, 1423.506200470894100, 184.6062591623307583 ) ) ;
#27507 = CARTESIAN_POINT ( 'NONE',  ( 18.02093535799999913, 1424.326836137830014, 225.1991050518980160 ) ) ;
#27508 = CARTESIAN_POINT ( 'NONE',  ( -1.268034562940015375, 1506.397833124954104, 187.1879512861502235 ) ) ;
#27509 = VERTEX_POINT ( 'NONE', #34624 ) ;
#27510 = CARTESIAN_POINT ( 'NONE',  ( 4.540901342749999792, 1419.211677879630088, 248.0989693021979861 ) ) ;
#27511 = AXIS2_PLACEMENT_3D ( 'NONE', #89930, #48506, #28940 ) ;
#27512 = CARTESIAN_POINT ( 'NONE',  ( -5.649719788644999241, 1514.243099272629934, 216.7708803706970002 ) ) ;
#27513 = B_SPLINE_SURFACE_WITH_KNOTS ( 'NONE', 5, 5, ( 
 ( #52493, #76017, #68750, #24492, #103407, #78225 ),
 ( #16086, #1536, #34565, #9371, #102853, #991 ),
 ( #35117, #101195, #50293, #69300, #26711, #62582 ),
 ( #36229, #27271, #96131, #95580, #46318, #45760 ),
 ( #79897, #62010, #54164, #12125, #37894, #44645 ),
 ( #79343, #36782, #20504, #71536, #105657, #72076 ),
 ( #19409, #70414, #3210, #70974, #78787, #28380 ),
 ( #53611, #37339, #96699, #63130, #97232, #80447 ),
 ( #18849, #53045, #11035, #106190, #87753, #2655 ),
 ( #87184, #28942, #105090, #88289, #54713, #19970 ),
 ( #69857, #3760, #11584, #45202, #88839, #104534 ),
 ( #103976, #61455, #27830, #10474, #2101, #27400 ) ),
 .UNSPECIFIED., .F., .F., .F.,
 ( 6, 3, 3, 6 ),
 ( 6, 6 ),
 ( 13.45148704079599966, 21.22852775220000154, 29.00530734079999817, 33.91527837888789776 ),
 ( -0.0002611228039829010042, 2.000000000000000000 ),
 .UNSPECIFIED. ) ;
#27514 = CARTESIAN_POINT ( 'NONE',  ( -18.72690275719048714, 1526.278758871496620, 182.1127646906402333 ) ) ;
#27515 = CARTESIAN_POINT ( 'NONE',  ( 4.025751050180000234, 1506.805340958390161, 220.0912426404989901 ) ) ;
#27516 = CYLINDRICAL_SURFACE ( 'NONE', #40209, 2.000000000000006661 ) ;
#27517 = EDGE_CURVE ( 'NONE', #100321, #53518, #60963, .T. ) ;
#27519 = ORIENTED_EDGE ( 'NONE', *, *, #108317, .T. ) ;
#27518 = CARTESIAN_POINT ( 'NONE',  ( -0.2432117950169480070, 1515.155210303460080, 204.7947648491820019 ) ) ;
#27520 = CARTESIAN_POINT ( 'NONE',  ( -17.43675326300159867, 1417.688629928019964, 206.2161178420579972 ) ) ;
#27521 = CARTESIAN_POINT ( 'NONE',  ( -15.57943187099139948, 1507.275789587220061, 192.6267346305599801 ) ) ;
#27522 = CARTESIAN_POINT ( 'NONE',  ( -1.746205394668796762, 1450.465189299475924, 154.2919931100517772 ) ) ;
#27523 = DIRECTION ( 'NONE',  ( -0.06162841671618445039, -0.9961946980917499861, 0.06162841671618458916 ) ) ;
#27524 = DIRECTION ( 'NONE',  ( 0.000000000000000000, 0.000000000000000000, -1.000000000000000000 ) ) ;
#27525 = CARTESIAN_POINT ( 'NONE',  ( -8.970685674490001205, 1442.046922168800165, 185.8306878991980113 ) ) ;
#27526 = ADVANCED_FACE ( 'NONE', ( #44705 ), #95089, .F. ) ;
#27527 = DIRECTION ( 'NONE',  ( -0.000000000000000000, -1.000000000000000000, -0.000000000000000000 ) ) ;
#27528 = AXIS2_PLACEMENT_3D ( 'NONE', #98525, #63313, #36970 ) ;
#27529 = DIRECTION ( 'NONE',  ( 0.001619481661242269796, -0.06184550950381718926, -0.9980844203940678616 ) ) ;
#27530 = CARTESIAN_POINT ( 'NONE',  ( -10.60236678890000128, 1431.113060387329824, 224.6557647168980338 ) ) ;
#27531 = ADVANCED_FACE ( 'NONE', ( #72521 ), #77952, .F. ) ;
#27532 = CARTESIAN_POINT ( 'NONE',  ( 15.72821513129999893, 1415.087486802329977, 227.2801319970979819 ) ) ;
#27533 = CARTESIAN_POINT ( 'NONE',  ( -10.94901061624040040, 1481.831333076229839, 207.7501958990100093 ) ) ;
#27534 = CARTESIAN_POINT ( 'NONE',  ( -15.91456197569999986, 1459.203849340630086, 230.3656326198979798 ) ) ;
#27535 = CARTESIAN_POINT ( 'NONE',  ( 2.477373605864999995, 1516.891731298979948, 206.2406231745169976 ) ) ;
#27536 = CARTESIAN_POINT ( 'NONE',  ( 46.02999043379999478, 1438.908956426789928, 268.4959127839979942 ) ) ;
#27537 = CARTESIAN_POINT ( 'NONE',  ( -31.47409394596284571, 1526.278758871496848, 218.5859237437391869 ) ) ;
#27538 = LINE ( 'NONE', #102019, #66127 ) ;
#27539 = EDGE_CURVE ( 'NONE', #83109, #33676, #71831, .T. ) ;
#27540 = CARTESIAN_POINT ( 'NONE',  ( 20.26569827480000185, 1469.158149366930047, 192.4428757755979973 ) ) ;
#27541 = CARTESIAN_POINT ( 'NONE',  ( -22.09796275270000265, 1430.768449482030064, 219.6318221129980088 ) ) ;
#27542 = CARTESIAN_POINT ( 'NONE',  ( -13.12582437823970061, 1379.460555358370129, 208.2157137769850124 ) ) ;
#27543 = B_SPLINE_CURVE_WITH_KNOTS ( 'NONE', 5,
 ( #56002, #47056, #5030, #107483, #11784, #39175, #4496, #20711, #38629 ),
 .UNSPECIFIED., .F., .F.,
 ( 6, 3, 6 ),
 ( -12.84112607031869935, -7.747513759300000302, -3.918736331710000798 ),
 .UNSPECIFIED. ) ;
#27544 = CARTESIAN_POINT ( 'NONE',  ( -16.49693783299999694, 1410.833576558129835, 226.6232151731979911 ) ) ;
#27545 = CARTESIAN_POINT ( 'NONE',  ( 17.61555691395466638, 1524.600389084707103, 237.5961665349170744 ) ) ;
#27546 = CARTESIAN_POINT ( 'NONE',  ( 20.61224126549999980, 1508.367040378830097, 227.7934948748979878 ) ) ;
#27547 = CARTESIAN_POINT ( 'NONE',  ( -11.73709356400000026, 1426.695943141129874, 144.1748013759980154 ) ) ;
#27548 = CARTESIAN_POINT ( 'NONE',  ( -17.27338612379999816, 1414.913060387329779, 208.0459408281480194 ) ) ;
#27549 = CARTESIAN_POINT ( 'NONE',  ( -12.67591333549999888, 1442.786765023099861, 186.5187981297980002 ) ) ;
#27550 = CARTESIAN_POINT ( 'NONE',  ( -7.719966901963539740, 1383.460063487440038, 218.9046041349110112 ) ) ;
#27551 = CARTESIAN_POINT ( 'NONE',  ( -29.16176511740000166, 1436.844852152720023, 136.7082758069980173 ) ) ;
#27552 = ORIENTED_EDGE ( 'NONE', *, *, #79593, .F. ) ;
#27553 = DIRECTION ( 'NONE',  ( -0.3363363969979658030, -0.9417419115949056119, 0.000000000000000000 ) ) ;
#27554 = CARTESIAN_POINT ( 'NONE',  ( -14.89215741792830094, 1409.433105983750011, 210.1887096901859877 ) ) ;
#27555 = CARTESIAN_POINT ( 'NONE',  ( -12.85018798063330081, 1508.236131449000140, 209.4043565344470039 ) ) ;
#27556 = CYLINDRICAL_SURFACE ( 'NONE', #67019, 0.9999999999999967804 ) ;
#27557 = CARTESIAN_POINT ( 'NONE',  ( -46.15245045410000557, 1446.051659328119968, 268.2044218355979979 ) ) ;
#27558 = CARTESIAN_POINT ( 'NONE',  ( -29.86281881105125180, 1525.137906803777014, 196.1139937296260598 ) ) ;
#27559 = CARTESIAN_POINT ( 'NONE',  ( 0.4382968505613619725, 1418.849865278630205, 184.6907702969609772 ) ) ;
#27560 = CARTESIAN_POINT ( 'NONE',  ( -26.20833356250000179, 1507.984236983630126, 216.2555649815679999 ) ) ;
#27561 = CARTESIAN_POINT ( 'NONE',  ( -74.96511919152730741, 1384.649769891829919, 300.0113357655470168 ) ) ;
#27562 = CARTESIAN_POINT ( 'NONE',  ( -9.690554794615099610, 1384.932168088679873, 199.9862972160919981 ) ) ;
#27563 = CARTESIAN_POINT ( 'NONE',  ( 17.47926118081009861, 1422.862077572759972, 226.4946375912610108 ) ) ;
#27564 = CARTESIAN_POINT ( 'NONE',  ( 12.85971948620000127, 1415.932840167130053, 221.4945874069979936 ) ) ;
#27565 = CARTESIAN_POINT ( 'NONE',  ( -6.464994551020000202, 1433.443311356699951, 154.6859263780980029 ) ) ;
#27566 = B_SPLINE_CURVE_WITH_KNOTS ( 'NONE', 5,
 ( #51059, #6289, #15753, #67322, #66777, #14684 ),
 .UNSPECIFIED., .F., .F.,
 ( 6, 6 ),
 ( 115.1755349879999955, 119.9142073339999968 ),
 .UNSPECIFIED. ) ;
#27567 = FACE_OUTER_BOUND ( 'NONE', #52815, .T. ) ;
#27568 = CARTESIAN_POINT ( 'NONE',  ( 12.94448954231351223, 1512.413060387330006, 232.8165751327380519 ) ) ;
#27569 = CARTESIAN_POINT ( 'NONE',  ( -8.604130659810000026, 1384.938024752220144, 199.8686491574789841 ) ) ;
#27570 = CARTESIAN_POINT ( 'NONE',  ( -22.64306613040000116, 1409.703773680230142, 208.6811978374589955 ) ) ;
#27571 = EDGE_CURVE ( 'NONE', #88339, #92672, #70418, .T. ) ;
#27572 = CARTESIAN_POINT ( 'NONE',  ( -21.60894078505574711, 1519.551704408389924, 199.6722430287886709 ) ) ;
#27573 = CARTESIAN_POINT ( 'NONE',  ( -12.60885230210000074, 1416.021639796329964, 195.3971703157980073 ) ) ;
#27574 = CARTESIAN_POINT ( 'NONE',  ( 3.926929841440000235, 1423.889174606040115, 192.9370842642990169 ) ) ;
#27575 = CARTESIAN_POINT ( 'NONE',  ( -4.390441442984810649, 1449.947851038559975, 190.5482995516449876 ) ) ;
#27576 = CARTESIAN_POINT ( 'NONE',  ( 20.82993010370000064, 1457.408288935790097, 206.8069621084789844 ) ) ;
#27577 = CARTESIAN_POINT ( 'NONE',  ( -15.52168021169999967, 1422.715911009230012, 228.7996066201980057 ) ) ;
#27579 = CARTESIAN_POINT ( 'NONE',  ( -9.766491094179999166, 1381.677989206189977, 201.2633182758889916 ) ) ;
#27578 = CARTESIAN_POINT ( 'NONE',  ( -7.544890056106759779, 1384.926148859619843, 219.0875905756669795 ) ) ;
#27580 = CARTESIAN_POINT ( 'NONE',  ( 1.361885589129999907, 1414.404335136930058, 232.8121858128980080 ) ) ;
#27581 = CARTESIAN_POINT ( 'NONE',  ( -8.515581525576477517, 1517.151704408390060, 226.9159523030141372 ) ) ;
#27582 = CARTESIAN_POINT ( 'NONE',  ( -12.19439603320000032, 1490.074496100290162, 210.2238046367189952 ) ) ;
#27583 = CARTESIAN_POINT ( 'NONE',  ( -22.77022140789999938, 1411.047177455729752, 211.3147823620780059 ) ) ;
#27584 = AXIS2_PLACEMENT_3D ( 'NONE', #18937, #86161, #62661 ) ;
#27585 = CARTESIAN_POINT ( 'NONE',  ( 4.329448776040000446, 1515.064792882589927, 206.7917118356089929 ) ) ;
#27586 = EDGE_CURVE ( 'NONE', #5707, #69529, #26340, .T. ) ;
#27587 = CARTESIAN_POINT ( 'NONE',  ( 6.549762446985000430, 1516.729202374750002, 204.5030968636170030 ) ) ;
#27588 = DIRECTION ( 'NONE',  ( -0.000000000000000000, -1.000000000000000000, -0.000000000000000000 ) ) ;
#27589 = CARTESIAN_POINT ( 'NONE',  ( -18.38404635505749951, 1485.653075037670078, 189.0955620534189734 ) ) ;
#27590 = CARTESIAN_POINT ( 'NONE',  ( 1.559371654100000004, 1508.275840731030030, 237.0359025730980136 ) ) ;
#27591 = CARTESIAN_POINT ( 'NONE',  ( 11.36583536198319955, 1502.344531051060130, 215.0256689626610012 ) ) ;
#27592 = CARTESIAN_POINT ( 'NONE',  ( 40.93861322897850386, 1447.346027417549976, 135.6170675654770150 ) ) ;
#27593 = AXIS2_PLACEMENT_3D ( 'NONE', #29494, #97801, #22577 ) ;
#27595 = ORIENTED_EDGE ( 'NONE', *, *, #71913, .T. ) ;
#27594 = CARTESIAN_POINT ( 'NONE',  ( -65.77537376722109741, 1379.741348619400014, 276.1715386585039482 ) ) ;
#27596 = EDGE_LOOP ( 'NONE', ( #69968, #36185, #11384, #106528 ) ) ;
#27597 = CARTESIAN_POINT ( 'NONE',  ( 11.32737736758029889, 1433.997803480599941, 151.5041286862229981 ) ) ;
#27598 = FACE_OUTER_BOUND ( 'NONE', #101937, .T. ) ;
#27599 = ORIENTED_EDGE ( 'NONE', *, *, #103398, .F. ) ;
#27600 = CARTESIAN_POINT ( 'NONE',  ( 0.1035575932523252335, 1457.708278094112984, 199.5842560823692793 ) ) ;
#27601 = CARTESIAN_POINT ( 'NONE',  ( -109.3080931909999975, 1384.942533863100152, 311.2645480262589786 ) ) ;
#27603 = CARTESIAN_POINT ( 'NONE',  ( -0.1593348516950000016, 1508.131906080129966, 180.6917150519979884 ) ) ;
#27602 = LINE ( 'NONE', #52277, #51481 ) ;
#27604 = CARTESIAN_POINT ( 'NONE',  ( -4.500000000000000000, 1425.929641636930000, 172.2701767054979882 ) ) ;
#27605 = B_SPLINE_CURVE_WITH_KNOTS ( 'NONE', 3,
 ( #68558, #60152, #70242, #94273, #104349, #85316, #45577, #56149, #97064, #98139, #38238, #5190, #89201, #64026, #106017, #20330, #63488, #12494, #72421, #73520, #55625, #89748, #30939, #39345, #29293, #55074, #72961, #105459, #97608, #65116, #53986, #13020, #99227, #28749, #47206, #20878, #62953, #46676, #80808, #46127, #13567, #79719, #106552, #54534, #90286, #21414 ),
 .UNSPECIFIED., .F., .F.,
 ( 4, 3, 3, 3, 3, 3, 3, 3, 3, 3, 3, 3, 3, 3, 3, 4 ),
 ( -32.67973531808329568, -31.64931769156649821, -30.28925356829410021, -28.92077687594739999, -27.54739078441340183, -26.16616490320429733, -24.78057410064459987, -23.39129159825840176, -22.83865932529860032, -21.47138836030729792, -20.09934210731429971, -18.72767567390599908, -17.36349881665530148, -16.00861653030469967, -14.66567884330130056, -13.33660260599999958 ),
 .UNSPECIFIED. ) ;
#27606 = EDGE_CURVE ( 'NONE', #54763, #40367, #78307, .T. ) ;
#27607 = CARTESIAN_POINT ( 'NONE',  ( -23.99770110361529873, 1452.069770166940089, 137.0532919795800240 ) ) ;
#27608 = CARTESIAN_POINT ( 'NONE',  ( -105.8549603932629850, 1378.913060387669702, 304.7826772458390110 ) ) ;
#27609 = CARTESIAN_POINT ( 'NONE',  ( -24.04659120089169733, 1444.796772349889807, 212.0316830080810178 ) ) ;
#27610 = SHAPE_REPRESENTATION_RELATIONSHIP ( 'NONE' , 'NONE' ,  #45156, #67999 ) ;
#27611 = CARTESIAN_POINT ( 'NONE',  ( -2.865588722415000067, 1516.890356958860139, 212.3900816908670208 ) ) ;
#27612 = CARTESIAN_POINT ( 'NONE',  ( 14.25441464932749902, 1415.890045859410066, 197.0605362263979998 ) ) ;
#27613 = CARTESIAN_POINT ( 'NONE',  ( -5.849558551512059168, 1424.853816168500089, 209.2574496775069974 ) ) ;
#27614 = CARTESIAN_POINT ( 'NONE',  ( 4.987363906429999716, 1436.241616669089808, 206.8881657794889861 ) ) ;
#27615 = ORIENTED_EDGE ( 'NONE', *, *, #11999, .F. ) ;
#27616 = CARTESIAN_POINT ( 'NONE',  ( 14.31101212421439861, 1435.533114237510063, 149.6577325083550249 ) ) ;
#27617 = EDGE_CURVE ( 'NONE', #89576, #29868, #9711, .T. ) ;
#27618 = ORIENTED_EDGE ( 'NONE', *, *, #82371, .F. ) ;
#27619 = ORIENTED_EDGE ( 'NONE', *, *, #35804, .F. ) ;
#27620 = EDGE_LOOP ( 'NONE', ( #16771, #28720, #73115, #58450 ) ) ;
#27621 = CARTESIAN_POINT ( 'NONE',  ( 12.54683115582590780, 1445.050387922648497, 169.4738476292419023 ) ) ;
#27622 = CARTESIAN_POINT ( 'NONE',  ( -0.9888054234880000459, 1464.981437416829976, 237.6389206865979986 ) ) ;
#27623 = CARTESIAN_POINT ( 'NONE',  ( 16.24128197971020526, 1451.109843354380473, 148.8744789175986512 ) ) ;
#27624 = CARTESIAN_POINT ( 'NONE',  ( -7.545074240589999981, 1384.922368660639904, 219.0875752896790232 ) ) ;
#27625 = CARTESIAN_POINT ( 'NONE',  ( 2.026230520227449983, 1465.919631588679977, 198.2820304006920082 ) ) ;
#27626 = CARTESIAN_POINT ( 'NONE',  ( -18.98973562068158927, 1443.333582277293317, 211.5879291524545351 ) ) ;
#27627 = CARTESIAN_POINT ( 'NONE',  ( -35.55178430715702831, 1379.641840282145040, 218.5080530506718048 ) ) ;
#27628 = CARTESIAN_POINT ( 'NONE',  ( 3.350944662710000355, 1464.628126271390101, 199.8699733667390035 ) ) ;
#27629 = EDGE_CURVE ( 'NONE', #62097, #86845, #86421, .T. ) ;
#27630 = CARTESIAN_POINT ( 'NONE',  ( 8.644029068445851394, 1437.385894306310092, 208.7514692825569966 ) ) ;
#27631 = ORIENTED_EDGE ( 'NONE', *, *, #31043, .T. ) ;
#27632 = CARTESIAN_POINT ( 'NONE',  ( -4.044321718124999521, 1517.001127920769704, 206.8363583507369867 ) ) ;
#27633 = VERTEX_POINT ( 'NONE', #78021 ) ;
#27634 = CARTESIAN_POINT ( 'NONE',  ( 33.19045541928569776, 1440.913060387330006, 258.0029463747879959 ) ) ;
#27635 = CARTESIAN_POINT ( 'NONE',  ( 11.73501141340019949, 1479.231774555940092, 208.2345455324859813 ) ) ;
#27636 = ADVANCED_FACE ( 'NONE', ( #84754 ), #101062, .T. ) ;
#27637 = VERTEX_POINT ( 'NONE', #85300 ) ;
#27638 = CARTESIAN_POINT ( 'NONE',  ( 27.28304656200170086, 1449.116014730419920, 136.7093938965389839 ) ) ;
#27639 = CARTESIAN_POINT ( 'NONE',  ( -14.04862573770000012, 1409.570344837929952, 190.8576452217980091 ) ) ;
#27640 = CARTESIAN_POINT ( 'NONE',  ( -37.33274161817728753, 1379.649438190497904, 225.5526503184333365 ) ) ;
#27641 = CARTESIAN_POINT ( 'NONE',  ( -24.40934708730000224, 1441.356666723849912, 212.0571328731979861 ) ) ;
#27642 = CARTESIAN_POINT ( 'NONE',  ( -11.30241272439999989, 1414.983771848829747, 195.8621715482979937 ) ) ;
#27643 = CARTESIAN_POINT ( 'NONE',  ( 0.9695034778824223043, 1454.901985832918399, 218.4941352939971466 ) ) ;
#27644 = CARTESIAN_POINT ( 'NONE',  ( -12.17346841087018561, 1434.039807595294860, 147.4869002435401342 ) ) ;
#27645 = FACE_OUTER_BOUND ( 'NONE', #109617, .T. ) ;
#27646 = CARTESIAN_POINT ( 'NONE',  ( 22.15911651489999912, 1435.271885453649929, 140.1193622846980134 ) ) ;
#27647 = EDGE_CURVE ( 'NONE', #83462, #27055, #29447, .T. ) ;
#27649 = CARTESIAN_POINT ( 'NONE',  ( 4.186152965159999795, 1492.613584369290038, 188.5705375364989891 ) ) ;
#27648 = CARTESIAN_POINT ( 'NONE',  ( 7.934445985219999109, 1465.591001358030098, 233.1255853796979807 ) ) ;
#27650 = B_SPLINE_SURFACE_WITH_KNOTS ( 'NONE', 4, 5, ( 
 ( #55142, #98207, #106068, #88725, #30454, #29348, #47266, #13081, #21476 ),
 ( #55687, #38298, #81389, #4702, #97663, #73023, #12557, #64638, #98758 ),
 ( #89261, #87624, #64086, #10912, #45087, #19843, #71957, #3638, #12008 ),
 ( #46737, #80869, #46188, #88174, #11466, #37213, #80319, #79227, #2536 ),
 ( #70854, #104964, #20936, #28254, #37766, #62446, #96570, #63548, #45641 ),
 ( #79781, #3086, #71409, #105525, #28814, #63012, #31001, #48380, #81950 ),
 ( #109385, #39410, #108816, #47815, #48937, #41056, #66298, #99293, #82523 ),
 ( #84157, #74684, #75235, #5820, #83603, #65181, #7458, #32111, #32662 ),
 ( #6901, #83067, #22567, #66839, #100949, #24244, #92553, #92017, #15287 ) ),
 .UNSPECIFIED., .F., .F., .F.,
 ( 5, 4, 5 ),
 ( 6, 3, 6 ),
 ( 52.85187863200000180, 54.35145002560000194, 54.36644573953599746 ),
 ( 0.000000000000000000, 1.000000000000000000, 2.000000000000000000 ),
 .UNSPECIFIED. ) ;
#27651 = CARTESIAN_POINT ( 'NONE',  ( 0.7553264358530019651, 1516.745833913490060, 214.8974710475970085 ) ) ;
#27652 = EDGE_CURVE ( 'NONE', #79695, #42097, #61711, .T. ) ;
#27653 = CARTESIAN_POINT ( 'NONE',  ( -14.43289921072090110, 1509.539432542180066, 182.8218189571549885 ) ) ;
#27654 = CARTESIAN_POINT ( 'NONE',  ( 5.424122834273520155, 1511.219705715099963, 216.9885700916489952 ) ) ;
#27655 = CARTESIAN_POINT ( 'NONE',  ( 30.47387511496750179, 1525.394057003703438, 221.5016029580054635 ) ) ;
#27656 = CARTESIAN_POINT ( 'NONE',  ( -4.028307778284999863, 1516.797038924770050, 212.3881954442970255 ) ) ;
#27657 = CARTESIAN_POINT ( 'NONE',  ( -11.68864801762120109, 1482.492120394230142, 206.8697282117639986 ) ) ;
#27658 = CARTESIAN_POINT ( 'NONE',  ( 30.16747994869233196, 1524.964230758883104, 221.7255045378688862 ) ) ;
#27660 = ORIENTED_EDGE ( 'NONE', *, *, #37977, .F. ) ;
#27659 = CARTESIAN_POINT ( 'NONE',  ( -88.55663222859999451, 1388.280866479749875, 293.2112741491590668 ) ) ;
#27661 = CARTESIAN_POINT ( 'NONE',  ( -17.36692104388747637, 1525.425686270210235, 237.0071275365210681 ) ) ;
#27662 = CARTESIAN_POINT ( 'NONE',  ( 26.47164861350000109, 1444.397189212120111, 225.7812066110980140 ) ) ;
#27663 = CARTESIAN_POINT ( 'NONE',  ( 29.00779973304128134, 1526.382868172864164, 217.2942086403122630 ) ) ;
#27664 = CARTESIAN_POINT ( 'NONE',  ( 20.39147186912994769, 1526.073429442291854, 233.1306614363087419 ) ) ;
#27665 = CARTESIAN_POINT ( 'NONE',  ( -6.986089899625779864, 1508.628476212760006, 236.2437696408319994 ) ) ;
#27666 = EDGE_CURVE ( 'NONE', #88646, #53816, #106440, .T. ) ;
#27667 = CARTESIAN_POINT ( 'NONE',  ( -20.50175529719999901, 1455.144460757629986, 224.2427973570979702 ) ) ;
#27668 = CIRCLE ( 'NONE', #99173, 15.09021984820000029 ) ;
#27670 = CARTESIAN_POINT ( 'NONE',  ( 19.02805368359999960, 1456.948220378029873, 225.7924841714979891 ) ) ;
#27669 = DIRECTION ( 'NONE',  ( 0.009162716345344929306, -0.1630249886365709999, -0.9865793925018000454 ) ) ;
#27671 = CARTESIAN_POINT ( 'NONE',  ( 0.04654594267750000042, 1452.815214894130122, 189.3840791623979953 ) ) ;
#27672 = CARTESIAN_POINT ( 'NONE',  ( -105.3432687185630101, 1381.144191882089899, 308.8504376499449791 ) ) ;
#27673 = ORIENTED_EDGE ( 'NONE', *, *, #29514, .T. ) ;
#27674 = CARTESIAN_POINT ( 'NONE',  ( 6.550389432124999800, 1516.755758396839838, 204.1155163507169732 ) ) ;
#27675 = CARTESIAN_POINT ( 'NONE',  ( 5.565001792720000664E-10, 1406.264975254330011, 269.2947192204980524 ) ) ;
#27677 = EDGE_CURVE ( 'NONE', #12462, #86830, #58293, .T. ) ;
#27676 = AXIS2_PLACEMENT_3D ( 'NONE', #11408, #36594, #37697 ) ;
#27678 = CARTESIAN_POINT ( 'NONE',  ( 28.59841868990000080, 1509.911739173930073, 206.6816370787080075 ) ) ;
#27679 = AXIS2_PLACEMENT_3D ( 'NONE', #103400, #78220, #86071 ) ;
#27680 = CARTESIAN_POINT ( 'NONE',  ( 19.45506404997480132, 1470.566269694860011, 270.3921699878309823 ) ) ;
#27681 = CARTESIAN_POINT ( 'NONE',  ( 2.478483860230000335, 1437.758671269130218, 157.6934240700980183 ) ) ;
#27682 = CARTESIAN_POINT ( 'NONE',  ( 3.235048502819999783, 1466.472015869789857, 219.6884156563990018 ) ) ;
#27683 = CARTESIAN_POINT ( 'NONE',  ( 1.156001302284453303, 1469.029874416468601, 219.0895512148256046 ) ) ;
#27684 = CARTESIAN_POINT ( 'NONE',  ( -41.50287196043939986, 1440.913060410020080, 261.3196605011079896 ) ) ;
#27685 = CARTESIAN_POINT ( 'NONE',  ( 34.28525901495920181, 1450.415853699829995, 136.2365631467760068 ) ) ;
#27686 = CARTESIAN_POINT ( 'NONE',  ( 2.235474299570370693, 1449.899086179656706, 154.3826606052703028 ) ) ;
#27687 = CARTESIAN_POINT ( 'NONE',  ( 1.515282459810000093, 1431.991175246789908, 200.7184021833390091 ) ) ;
#27688 = CARTESIAN_POINT ( 'NONE',  ( 0.8724913224786620125, 1450.882592301979912, 154.2430449183819690 ) ) ;
#27689 = CARTESIAN_POINT ( 'NONE',  ( 2.446683647589999566, 1506.492871364290068, 220.9379107316989916 ) ) ;
#27690 = CARTESIAN_POINT ( 'NONE',  ( -4.226426730290000044, 1515.477082009390188, 209.4928634131090348 ) ) ;
#27691 = ORIENTED_EDGE ( 'NONE', *, *, #100925, .T. ) ;
#27692 = CARTESIAN_POINT ( 'NONE',  ( 2.500000726750000180, 1448.905931065010009, 182.6097889574979831 ) ) ;
#27693 = CARTESIAN_POINT ( 'NONE',  ( 2.975001697819999791, 1486.548690899389840, 198.3380112669989899 ) ) ;
#27694 = CARTESIAN_POINT ( 'NONE',  ( 10.04185642635390074, 1469.459450719869892, 207.3542015582230249 ) ) ;
#27695 = CARTESIAN_POINT ( 'NONE',  ( -0.1080245130140000120, 1476.050155969029902, 268.4837719563980158 ) ) ;
#27696 = CARTESIAN_POINT ( 'NONE',  ( -8.881784197000000993E-16, 1414.413060387330006, 209.1218459616989946 ) ) ;
#27697 = CARTESIAN_POINT ( 'NONE',  ( -33.43367350703748997, 1524.397344074318653, 197.7663411554295578 ) ) ;
#27698 = CARTESIAN_POINT ( 'NONE',  ( 8.348235655690000812, 1423.006858839259849, 212.9515974749489828 ) ) ;
#27699 = CARTESIAN_POINT ( 'NONE',  ( -8.862056518773441027, 1384.892951007370129, 218.6851137863439760 ) ) ;
#27700 = CARTESIAN_POINT ( 'NONE',  ( 17.66967186770163778, 1519.551704408389924, 223.1030593992828699 ) ) ;
#27701 = CARTESIAN_POINT ( 'NONE',  ( -9.087499124679998985, 1482.679315955489756, 203.1872625214689947 ) ) ;
#27702 = CARTESIAN_POINT ( 'NONE',  ( 26.81196021308459621, 1435.986317847600048, 136.4844220934189991 ) ) ;
#27703 = VECTOR ( 'NONE', #77320, 1000.000000000000000 ) ;
#27704 = CARTESIAN_POINT ( 'NONE',  ( -13.51610093809999924, 1443.913060387330006, 169.3501091259980171 ) ) ;
#27705 = CARTESIAN_POINT ( 'NONE',  ( -17.38130034684149905, 1410.742361519390215, 225.7780215077559944 ) ) ;
#27706 = CARTESIAN_POINT ( 'NONE',  ( 11.91321771470000002, 1435.943783413959864, 147.6429393588979906 ) ) ;
#27707 = ORIENTED_EDGE ( 'NONE', *, *, #107775, .F. ) ;
#27708 = CARTESIAN_POINT ( 'NONE',  ( 41.65675406397859604, 1443.992462633329978, 135.6790809494980010 ) ) ;
#27709 = CARTESIAN_POINT ( 'NONE',  ( -13.58739845499320076, 1508.434607234060195, 209.8723785710020309 ) ) ;
#27710 = CIRCLE ( 'NONE', #42019, 0.5000000000000000000 ) ;
#27711 = CARTESIAN_POINT ( 'NONE',  ( 2.045814292219999775, 1449.354251884889891, 190.1385047842989877 ) ) ;
#27713 = CARTESIAN_POINT ( 'NONE',  ( -2.259335814679200194, 1457.676294062130182, 219.5407953899610050 ) ) ;
#27712 = DIRECTION ( 'NONE',  ( 0.000000000000000000, -0.7071067811865475727, -0.7071067811865475727 ) ) ;
#27714 = CARTESIAN_POINT ( 'NONE',  ( -1.906499758064230099E-08, 1508.551704408389924, 216.1347675157070114 ) ) ;
#27715 = DIRECTION ( 'NONE',  ( -5.980589973904019347E-17, 1.000000000000000000, -1.736889445713099699E-16 ) ) ;
#27716 = CARTESIAN_POINT ( 'NONE',  ( 2.485205649205000089, 1517.181921232829836, 201.3958557702769951 ) ) ;
#27717 = CARTESIAN_POINT ( 'NONE',  ( 7.746190077790000572, 1425.513952521069996, 211.7745271020289977 ) ) ;
#27718 = CARTESIAN_POINT ( 'NONE',  ( 18.94656048379999902, 1455.761273475090093, 200.3458234316790083 ) ) ;
#27719 = LINE ( 'NONE', #8694, #110566 ) ;
#27720 = CARTESIAN_POINT ( 'NONE',  ( -11.87502393677010026, 1433.007271224430042, 149.9804568710339936 ) ) ;
#27721 = CARTESIAN_POINT ( 'NONE',  ( -109.5441724399999970, 1379.437034644700134, 304.2217752583950414 ) ) ;
#27722 = B_SPLINE_SURFACE_WITH_KNOTS ( 'NONE', 5, 5, ( 
 ( #101675, #93293, #16018, #24965, #16555, #8729, #920, #34498, #85430 ),
 ( #7634, #93828, #7093, #58611, #42909, #77065, #84346, #50745, #375 ),
 ( #41249, #94383, #86001, #43463, #77610, #26638, #50220, #84882, #60834 ),
 ( #94960, #83798, #75421, #109559, #32830, #105019, #27750, #80374, #28310 ),
 ( #78713, #63059, #3136, #88773, #52976, #12056, #97164, #18778, #29394 ),
 ( #1454, #46242, #87107, #62502, #87673, #105579, #36707, #71464, #106118 ),
 ( #53533, #28867, #20434, #61944, #45690, #70901, #19890, #96622, #44564 ),
 ( #2027, #10396, #79275, #37268, #3689, #86551, #96061, #36161, #2585 ),
 ( #54096, #44013, #54641, #95506, #27205, #35596, #37817, #104458, #70346 ),
 ( #72004, #19331, #63595, #88223, #97713, #10962, #52424, #9846, #45133 ),
 ( #69787, #11515, #79829, #78150, #103906, #61388, #30505, #13678, #106658 ),
 ( #81441, #32163, #64694, #21530, #31605, #48989, #55190, #47317, #99901 ),
 ( #29948, #90961, #4752, #73639, #66350, #89864, #4219, #5308, #5870 ),
 ( #38894, #55744, #6418, #73077, #13133, #65783, #91524, #80920, #23198 ),
 ( #64141, #98261, #31055, #46791, #47867, #40563, #22622, #99346, #56825 ),
 ( #48437, #40012, #89315, #82579, #90399, #107217, #39467, #98813, #22075 ),
 ( #57397, #14803, #83121, #74735, #38348, #82002, #65236, #56270, #20985 ),
 ( #12611, #108872, #74192, #107769, #14248, #108321, #72528, #42225, #75831 ),
 ( #60143, #33809, #67448, #76376, #32714, #790, #50087, #34919, #109981 ),
 ( #248, #17539, #23750, #15886, #68548, #100467, #109437, #59585, #84215 ),
 ( #57938, #58483, #83663, #84760, #85307, #102648, #93700, #92070, #7511 ),
 ( #24301, #34375, #94263, #49538, #25948, #6959, #75291, #66896, #8056 ),
 ( #41673, #102114, #92611, #15342, #110525, #16434, #24839, #51741, #85875 ),
 ( #33257, #50626, #9177, #101547, #25393, #59042, #68003, #41113, #16978 ) ),
 .UNSPECIFIED., .F., .F., .F.,
 ( 6, 3, 3, 3, 3, 3, 3, 6 ),
 ( 6, 3, 6 ),
 ( 0.000000000000000000, 19.27951045849999900, 37.56883265599999788, 64.75259520960000259, 97.48063803579999842, 123.9428332119999965, 141.7919792689999952, 160.6499452009999800 ),
 ( 7.853981633970000154, 11.78097245100000023, 15.70796326790000030 ),
 .UNSPECIFIED. ) ;
#27723 = CARTESIAN_POINT ( 'NONE',  ( 7.901460997567876454, 1365.119847262537405, 209.6218459617148824 ) ) ;
#27725 = ORIENTED_EDGE ( 'NONE', *, *, #15607, .T. ) ;
#27724 = CARTESIAN_POINT ( 'NONE',  ( -4.545982247914895247, 1508.783371651612924, 205.6342535022036202 ) ) ;
#27726 = ORIENTED_EDGE ( 'NONE', *, *, #18261, .F. ) ;
#27727 = CARTESIAN_POINT ( 'NONE',  ( -41.66146602930000142, 1443.809371001679892, 136.1342613200980054 ) ) ;
#27728 = CARTESIAN_POINT ( 'NONE',  ( 0.4231130519409999624, 1466.688341884629835, 235.6370719615979965 ) ) ;
#27729 = CARTESIAN_POINT ( 'NONE',  ( -0.9761296588700000276, 1473.260042257729992, 270.4290152423980089 ) ) ;
#27730 = CARTESIAN_POINT ( 'NONE',  ( -7.703229056714999246, 1511.126521646420088, 214.5635183388470182 ) ) ;
#27731 = CARTESIAN_POINT ( 'NONE',  ( 15.69795926444620271, 1522.051704408389924, 222.7678737639049871 ) ) ;
#27732 = CARTESIAN_POINT ( 'NONE',  ( 0.4151546846821903003, 1522.382868172863937, 173.3106345060153046 ) ) ;
#27733 = CARTESIAN_POINT ( 'NONE',  ( -36.07230721274900276, 1450.585147499210052, 136.1439704596049864 ) ) ;
#27734 = CARTESIAN_POINT ( 'NONE',  ( 33.92724067235770491, 1436.576420800989808, 136.5094946137080001 ) ) ;
#27735 = CARTESIAN_POINT ( 'NONE',  ( 9.919156197434499944, 1396.259444956319840, 214.0198213256190058 ) ) ;
#27736 = CARTESIAN_POINT ( 'NONE',  ( -0.02192818798958470067, 1407.539782041390026, 196.0601747775820058 ) ) ;
#27737 = CARTESIAN_POINT ( 'NONE',  ( -14.26333330936780008, 1452.396687514240057, 223.0069981058830137 ) ) ;
#27738 = CARTESIAN_POINT ( 'NONE',  ( -14.31417139289039930, 1435.588016961450194, 149.7074577630269800 ) ) ;
#27739 = ORIENTED_EDGE ( 'NONE', *, *, #29546, .T. ) ;
#27740 = CARTESIAN_POINT ( 'NONE',  ( 11.83466398051542612, 1521.951704408389787, 190.1848878783540897 ) ) ;
#27741 = CARTESIAN_POINT ( 'NONE',  ( 12.88115801269999849, 1441.996360158710104, 188.6196260033980252 ) ) ;
#27742 = EDGE_LOOP ( 'NONE', ( #7322, #10442, #67106, #71748 ) ) ;
#27743 = ORIENTED_EDGE ( 'NONE', *, *, #83400, .F. ) ;
#27744 = DIRECTION ( 'NONE',  ( 0.000000000000000000, -1.000000000000000000, 0.000000000000000000 ) ) ;
#27745 = CARTESIAN_POINT ( 'NONE',  ( 9.622136349630000751, 1363.684386430210225, 207.6218459616989946 ) ) ;
#27746 = CARTESIAN_POINT ( 'NONE',  ( -2.287084308194999860, 1517.068517094990057, 214.1351209316169957 ) ) ;
#27747 = CARTESIAN_POINT ( 'NONE',  ( 3.611462603544999705, 1511.572472350439739, 217.1939399984370027 ) ) ;
#27748 = ORIENTED_EDGE ( 'NONE', *, *, #75838, .F. ) ;
#27749 = CARTESIAN_POINT ( 'NONE',  ( 7.901745564190000515, 1424.856359000810016, 211.6778634635190031 ) ) ;
#27750 = CARTESIAN_POINT ( 'NONE',  ( -101.9210842570000040, 1374.792827289790011, 302.4435101425590346 ) ) ;
#27751 = AXIS2_PLACEMENT_3D ( 'NONE', #39813, #80160, #47121 ) ;
#27752 = CARTESIAN_POINT ( 'NONE',  ( -105.8811732696050001, 1378.913060387349788, 303.3307478265489863 ) ) ;
#27753 = CARTESIAN_POINT ( 'NONE',  ( 6.551643386774999023, 1516.807958722750072, 203.3403553877570005 ) ) ;
#27754 = EDGE_CURVE ( 'NONE', #54634, #64279, #67053, .T. ) ;
#27755 = CARTESIAN_POINT ( 'NONE',  ( -26.42714720800000094, 1440.913060387330006, 243.9198229517980110 ) ) ;
#27756 = ADVANCED_FACE ( 'NONE', ( #87544 ), #105998, .F. ) ;
#27757 = B_SPLINE_SURFACE_WITH_KNOTS ( 'NONE', 5, 5, ( 
 ( #102326, #26733, #51951, #34582, #79360, #86638 ),
 ( #59804, #42998, #53063, #69877, #96148, #45222 ),
 ( #93924, #86093, #104551, #87200, #10492, #70433 ),
 ( #103992, #34030, #78241, #9387, #460, #87770 ),
 ( #35136, #69317, #62028, #102870, #85519, #44663 ),
 ( #77156, #68221, #11051, #17191, #43550, #1554 ) ),
 .UNSPECIFIED., .F., .F., .F.,
 ( 6, 6 ),
 ( 6, 6 ),
 ( 30.32814665560000122, 157.7108139880000124 ),
 ( -6.245004513519998715E-17, 1.000000000000000000 ),
 .UNSPECIFIED. ) ;
#27758 = CARTESIAN_POINT ( 'NONE',  ( -1.324026618839999836, 1487.751343670030110, 231.2068259027980162 ) ) ;
#27759 = CARTESIAN_POINT ( 'NONE',  ( -41.99751584039131558, 1438.963961567131264, 269.6474901557800763 ) ) ;
#27760 = CARTESIAN_POINT ( 'NONE',  ( -9.809994025999090539, 1391.913060387289988, 214.8154631801960193 ) ) ;
#27761 = CARTESIAN_POINT ( 'NONE',  ( -4.481884685280000724, 1410.004874574130099, 232.0320561794979994 ) ) ;
#27762 = B_SPLINE_CURVE_WITH_KNOTS ( 'NONE', 3,
 ( #11213, #104700, #2280, #103028, #27995, #1162, #27437 ),
 .UNSPECIFIED., .F., .F.,
 ( 4, 3, 4 ),
 ( -157.6565403119999758, -100.4036150152009981, -30.32814665559999412 ),
 .UNSPECIFIED. ) ;
#27764 = VERTEX_POINT ( 'NONE', #28174 ) ;
#27763 = CARTESIAN_POINT ( 'NONE',  ( -10.50159781620000210, 1445.883858324350058, 186.3320361473979858 ) ) ;
#27765 = CARTESIAN_POINT ( 'NONE',  ( -24.58745215098610259, 1440.913060451950059, 213.2928209972399998 ) ) ;
#27766 = CARTESIAN_POINT ( 'NONE',  ( 20.86442530855919841, 1507.787512642029924, 226.2753960300409801 ) ) ;
#27767 = CARTESIAN_POINT ( 'NONE',  ( 4.687651746879999415, 1478.378160227390254, 228.9010599218989910 ) ) ;
#27768 = CARTESIAN_POINT ( 'NONE',  ( -24.55864424809999846, 1435.538845322140105, 137.1712378357980242 ) ) ;
#27769 = CARTESIAN_POINT ( 'NONE',  ( 4.624099291334999862, 1516.962555622980062, 212.3771868965270073 ) ) ;
#27770 = CARTESIAN_POINT ( 'NONE',  ( -66.93998226469999224, 1379.744520212610041, 276.4118626343590108 ) ) ;
#27771 = EDGE_CURVE ( 'NONE', #104164, #5427, #32878, .T. ) ;
#27772 = CARTESIAN_POINT ( 'NONE',  ( -7.911281457743720935, 1425.821179498857646, 225.8045002088393289 ) ) ;
#27773 = CARTESIAN_POINT ( 'NONE',  ( 4.987078422726499483, 1508.551704408389924, 205.6342535031670025 ) ) ;
#27775 = CARTESIAN_POINT ( 'NONE',  ( 19.30007074693602576, 1410.948536389271567, 195.8605864048363117 ) ) ;
#27774 = AXIS2_PLACEMENT_3D ( 'NONE', #59233, #40750, #23389 ) ;
#27776 = CARTESIAN_POINT ( 'NONE',  ( -5.781585816274999345, 1516.939646076049939, 209.1342929058909874 ) ) ;
#27777 = ORIENTED_EDGE ( 'NONE', *, *, #26981, .T. ) ;
#27778 = CARTESIAN_POINT ( 'NONE',  ( 2.500000000000000000, 1433.496992208500160, 157.5291644476980082 ) ) ;
#27779 = CARTESIAN_POINT ( 'NONE',  ( -7.717505791104999346, 1516.857914730730045, 201.4043401791270185 ) ) ;
#27780 = CARTESIAN_POINT ( 'NONE',  ( -19.18216750550000071, 1385.279599344249846, 220.5028985859590023 ) ) ;
#27781 = VERTEX_POINT ( 'NONE', #10833 ) ;
#27782 = CARTESIAN_POINT ( 'NONE',  ( -113.4000000000000057, 1390.913060387289988, 304.2218459572590064 ) ) ;
#27783 = CARTESIAN_POINT ( 'NONE',  ( -2.738226213839999978, 1429.529162839389755, 200.8905597157389877 ) ) ;
#27784 = CARTESIAN_POINT ( 'NONE',  ( 12.46581826982980168, 1434.413684206549988, 149.6162948891119981 ) ) ;
#27785 = CARTESIAN_POINT ( 'NONE',  ( 13.86236365335560095, 1469.002559954369872, 230.9511697035910061 ) ) ;
#27786 = CIRCLE ( 'NONE', #90353, 451.3444983786160947 ) ;
#27787 = CARTESIAN_POINT ( 'NONE',  ( -25.78157324093470137, 1509.813372837629913, 223.1298088449100021 ) ) ;
#27788 = CARTESIAN_POINT ( 'NONE',  ( -2.073863249510000006, 1408.985481286630147, 187.4413895757980129 ) ) ;
#27789 = CARTESIAN_POINT ( 'NONE',  ( -0.1681250064260000066, 1408.918931400830161, 232.2238576234980201 ) ) ;
#27790 = CARTESIAN_POINT ( 'NONE',  ( 0.09356662494084540260, 1420.452715721949971, 182.6929833556150129 ) ) ;
#27791 = B_SPLINE_CURVE_WITH_KNOTS ( 'NONE', 5,
 ( #84784, #74221, #110552, #108350, #75319, #101029, #65811, #15373, #14273 ),
 .UNSPECIFIED., .F., .F.,
 ( 6, 3, 6 ),
 ( 2.234462700939999991, 2.575722133019999749, 3.155688525630194974 ),
 .UNSPECIFIED. ) ;
#27793 = CARTESIAN_POINT ( 'NONE',  ( -2.727274045799999769, 1420.080670998130017, 186.1515345996979818 ) ) ;
#27792 = CARTESIAN_POINT ( 'NONE',  ( -6.940473372275000052, 1516.833525648419936, 215.6778681647369922 ) ) ;
#27794 = CARTESIAN_POINT ( 'NONE',  ( -5.432410439650000811, 1391.426148861440197, 214.9021618825790085 ) ) ;
#27795 = CARTESIAN_POINT ( 'NONE',  ( 10.92462469921369994, 1470.600674883090051, 208.4273988239069979 ) ) ;
#27796 = EDGE_LOOP ( 'NONE', ( #44696, #83769, #39083, #38997 ) ) ;
#27797 = FACE_OUTER_BOUND ( 'NONE', #87106, .T. ) ;
#27798 = EDGE_CURVE ( 'NONE', #4789, #86013, #91789, .T. ) ;
#27799 = CARTESIAN_POINT ( 'NONE',  ( 8.000452546092619244, 1425.311357000540056, 211.1883339932590218 ) ) ;
#27800 = CARTESIAN_POINT ( 'NONE',  ( -6.150877690909999806, 1490.513422154930140, 181.6085158044980119 ) ) ;
#27801 = ORIENTED_EDGE ( 'NONE', *, *, #93207, .T. ) ;
#27802 = CARTESIAN_POINT ( 'NONE',  ( 15.90990511613090241, 1514.921193439799936, 193.9190475034619965 ) ) ;
#27803 =( BOUNDED_SURFACE ( )  B_SPLINE_SURFACE ( 3, 2, ( 
 ( #90628, #3906, #29623 ),
 ( #22297, #47002, #62731 ),
 ( #97381, #4970, #106875 ),
 ( #39115, #71688, #45901 ) ),
 .UNSPECIFIED., .F., .F., .F. ) 
 B_SPLINE_SURFACE_WITH_KNOTS ( ( 4, 4 ),
 ( 3, 3 ),
 ( 0.000000000000000000, 0.0002960034161023844057 ),
 ( 0.000000000000000000, 1.000000000000000000 ),
 .UNSPECIFIED. ) 
 GEOMETRIC_REPRESENTATION_ITEM ( )  RATIONAL_B_SPLINE_SURFACE ( (
 ( 1.000000000000000000, 0.8070209408750013136, 1.000000000000000000),
 ( 1.000000000000000000, 0.8071723757218328688, 1.000000000000000000),
 ( 1.000000000000000000, 0.8072480346917663141, 1.000000000000000000),
 ( 1.000000000000000000, 0.8072480644198083422, 1.000000000000000000) ) ) 
 REPRESENTATION_ITEM ( '' )  SURFACE ( )  );
#27804 = CARTESIAN_POINT ( 'NONE',  ( 9.609510489164891922, 1436.202073637698732, 152.7520764886153870 ) ) ;
#27805 = EDGE_CURVE ( 'NONE', #96903, #109412, #40249, .T. ) ;
#27807 = B_SPLINE_CURVE_WITH_KNOTS ( 'NONE', 5,
 ( #58504, #15907, #94854, #76393, #59061, #68023, #93184, #25411, #51197, #86450, #85327, #8623 ),
 .UNSPECIFIED., .F., .F.,
 ( 6, 3, 3, 6 ),
 ( 0.000000000000000000, 0.3076635699321720319, 0.7692211899778510498, 1.000000000000000000 ),
 .UNSPECIFIED. ) ;
#27806 = CARTESIAN_POINT ( 'NONE',  ( 8.379224430868440265, 1511.478393686179970, 203.5654043840270049 ) ) ;
#27808 = UNCERTAINTY_MEASURE_WITH_UNIT (LENGTH_MEASURE( 1.000000000000000082E-05 ), #24282, 'distance_accuracy_value', 'NONE');
#27809 = CARTESIAN_POINT ( 'NONE',  ( 2.792478474500000196, 1441.472946933690082, 218.6424847214589988 ) ) ;
#27810 = CARTESIAN_POINT ( 'NONE',  ( -33.28034951413935261, 1522.382868172863937, 200.8029765415142549 ) ) ;
#27811 = SPHERICAL_SURFACE ( 'NONE', #81776, 2.000000000550000046 ) ;
#27812 = B_SPLINE_CURVE_WITH_KNOTS ( 'NONE', 3,
 ( #13455, #72313, #39793, #73952, #22398, #71790 ),
 .UNSPECIFIED., .F., .F.,
 ( 4, 2, 4 ),
 ( 0.000000000000000000, 0.5000000000000000000, 1.000000000000000000 ),
 .UNSPECIFIED. ) ;
#27813 = CARTESIAN_POINT ( 'NONE',  ( -4.271711423730000234, 1446.704873953880224, 157.7711695664980027 ) ) ;
#27814 = CARTESIAN_POINT ( 'NONE',  ( -18.35972178970000357, 1424.606442804230028, 225.2895523400979982 ) ) ;
#27815 = CARTESIAN_POINT ( 'NONE',  ( -17.08284985680000290, 1435.239220910890026, 147.2844623966980180 ) ) ;
#27816 = CARTESIAN_POINT ( 'NONE',  ( -4.897375497219999652, 1432.353341358199941, 150.0655110971979980 ) ) ;
#27817 = CARTESIAN_POINT ( 'NONE',  ( 17.24394154959999881, 1413.517467163129822, 192.0312209363980003 ) ) ;
#27819 = CARTESIAN_POINT ( 'NONE',  ( -5.074768907954896768, 1391.842035882342770, 203.6019732846310717 ) ) ;
#27818 = CARTESIAN_POINT ( 'NONE',  ( 0.2483634325632210205, 1408.921733429509914, 231.7190040910680011 ) ) ;
#27820 = CARTESIAN_POINT ( 'NONE',  ( 10.87371602109691970, 1426.219295122016547, 148.5295350641272591 ) ) ;
#27821 = ORIENTED_EDGE ( 'NONE', *, *, #84247, .T. ) ;
#27822 = CARTESIAN_POINT ( 'NONE',  ( 12.51099983133400073, 1416.825784014559986, 196.0986189223339977 ) ) ;
#27823 = CARTESIAN_POINT ( 'NONE',  ( 9856.831406526702267, 2833.746317950241519, 1378.242120268380177 ) ) ;
#27824 = CARTESIAN_POINT ( 'NONE',  ( -24.07870975389999657, 1437.132368761460157, 211.2127430859480057 ) ) ;
#27825 = CARTESIAN_POINT ( 'NONE',  ( -4.347083409420000599, 1484.166081217490046, 199.1975610816789981 ) ) ;
#27826 = CARTESIAN_POINT ( 'NONE',  ( -31.44837959398599736, 1511.187213306747708, 197.3353852117985525 ) ) ;
#27827 = CARTESIAN_POINT ( 'NONE',  ( -3.872181927699717363, 1426.015247764028345, 186.0427167524304082 ) ) ;
#27828 = CARTESIAN_POINT ( 'NONE',  ( 28.82451532742497946, 1526.348417187215318, 220.0525736641851609 ) ) ;
#27829 = CARTESIAN_POINT ( 'NONE',  ( -18.85772126319670150, 1509.650461852630087, 185.3681582559849801 ) ) ;
#27830 = CARTESIAN_POINT ( 'NONE',  ( -10.62221739863140080, 1490.415717394859939, 212.3810854760239977 ) ) ;
#27831 = CARTESIAN_POINT ( 'NONE',  ( -19.73707534100000061, 1467.795347597790169, 204.3773262252089751 ) ) ;
#27832 = CARTESIAN_POINT ( 'NONE',  ( -78.52563159432189366, 1383.778061994039945, 302.6299618360769728 ) ) ;
#27833 = CIRCLE ( 'NONE', #51017, 2.000000000000003553 ) ;
#27834 = CARTESIAN_POINT ( 'NONE',  ( -109.3672071742060012, 1383.631249172380194, 311.1356417145969999 ) ) ;
#27835 = CARTESIAN_POINT ( 'NONE',  ( -16.93884325354670040, 1507.634939694479954, 230.1482608329069990 ) ) ;
#27836 = CARTESIAN_POINT ( 'NONE',  ( -1.747411913067469902, 1516.543067334039961, 201.4125847483680047 ) ) ;
#27838 = ORIENTED_EDGE ( 'NONE', *, *, #39743, .F. ) ;
#27837 = CARTESIAN_POINT ( 'NONE',  ( 24.48015091930000153, 1509.748507779630017, 193.8668277333979972 ) ) ;
#27839 = CARTESIAN_POINT ( 'NONE',  ( -17.62175316511144985, 1460.293634674704435, 228.1921996207679797 ) ) ;
#27840 = CARTESIAN_POINT ( 'NONE',  ( -70.21063747969999724, 1380.040839330149993, 289.8377882247589810 ) ) ;
#27841 = CARTESIAN_POINT ( 'NONE',  ( 11.81780673814840021, 1522.051704408389924, 195.5270144474869767 ) ) ;
#27842 = ORIENTED_EDGE ( 'NONE', *, *, #103228, .F. ) ;
#27843 = VERTEX_POINT ( 'NONE', #89727 ) ;
#27844 = CARTESIAN_POINT ( 'NONE',  ( 18.18162401578809906, 1416.230844595159851, 209.3331246004520096 ) ) ;
#27845 = CARTESIAN_POINT ( 'NONE',  ( 18.12088407619999941, 1425.009777113730024, 225.3844322571980001 ) ) ;
#27846 = DIRECTION ( 'NONE',  ( -0.5369043659964716220, -0.4884709562386453929, -0.6878443331781037839 ) ) ;
#27848 = CARTESIAN_POINT ( 'NONE',  ( -33.93598460830000363, 1457.486625415129993, 259.3467912259980039 ) ) ;
#27847 = CARTESIAN_POINT ( 'NONE',  ( -106.8999999999999915, 1305.913060387289988, 304.2218459572590064 ) ) ;
#27849 = CARTESIAN_POINT ( 'NONE',  ( -3.686527624546230175, 1495.487496192859908, 197.3578822790109939 ) ) ;
#27850 = CARTESIAN_POINT ( 'NONE',  ( -11.92957103340000202, 1433.515502532339951, 150.1951483352979722 ) ) ;
#27851 = CARTESIAN_POINT ( 'NONE',  ( 24.27333642870000219, 1509.087578010229890, 195.8034309281979972 ) ) ;
#27852 = CARTESIAN_POINT ( 'NONE',  ( -19.45985541978930300, 1483.862530646330015, 228.1370256266669969 ) ) ;
#27853 = CARTESIAN_POINT ( 'NONE',  ( 5.230272464420000489, 1409.599014443830129, 186.6733164947980015 ) ) ;
#27854 = CARTESIAN_POINT ( 'NONE',  ( 5.004094174289999586, 1423.187700235230068, 184.8599579744980019 ) ) ;
#27855 = FACE_OUTER_BOUND ( 'NONE', #109768, .T. ) ;
#27856 = CARTESIAN_POINT ( 'NONE',  ( 11.36665852199999982, 1437.938651650400061, 152.0461524011979861 ) ) ;
#27857 = CARTESIAN_POINT ( 'NONE',  ( -13.35343597923650094, 1422.178733618030037, 203.8110371803210228 ) ) ;
#27858 = CARTESIAN_POINT ( 'NONE',  ( -14.98881544730000037, 1452.245887789929839, 149.4533671292980159 ) ) ;
#27859 = DIRECTION ( 'NONE',  ( -0.2054769195713187224, 0.000000000000000000, 0.9786619618251655162 ) ) ;
#27860 = VERTEX_POINT ( 'NONE', #5733 ) ;
#27861 = CARTESIAN_POINT ( 'NONE',  ( -4.058188250217909854, 1508.551704408389924, 213.8008314270979895 ) ) ;
#27862 = AXIS2_PLACEMENT_3D ( 'NONE', #26612, #84320, #41767 ) ;
#27863 = CARTESIAN_POINT ( 'NONE',  ( -4.214505117019999858, 1482.742666855489915, 231.1823280205989875 ) ) ;
#27864 = CARTESIAN_POINT ( 'NONE',  ( -42.16354462729999852, 1445.439307631620068, 270.0644491700979870 ) ) ;
#27865 = CARTESIAN_POINT ( 'NONE',  ( 8.315094184529998600, 1421.392059295079889, 196.2232414242990046 ) ) ;
#27866 = CARTESIAN_POINT ( 'NONE',  ( 6.655787406570000009, 1441.606255579999925, 154.8401361813980088 ) ) ;
#27867 = DIRECTION ( 'NONE',  ( 0.000000000000000000, -1.000000000000000000, 0.000000000000000000 ) ) ;
#27868 = CARTESIAN_POINT ( 'NONE',  ( 8.805428988939999257, 1497.713060387329961, 188.8615427550980144 ) ) ;
#27869 = CARTESIAN_POINT ( 'NONE',  ( -3.801734883709992019, 1509.034509900240437, 213.6092049266663651 ) ) ;
#27870 = CARTESIAN_POINT ( 'NONE',  ( -1.352297191969999979, 1415.128105759529944, 226.9541798989980066 ) ) ;
#27871 = CARTESIAN_POINT ( 'NONE',  ( -7.807415031859999743, 1418.825582515029964, 232.7594164784979966 ) ) ;
#27872 = CIRCLE ( 'NONE', #59848, 1.999999999999999556 ) ;
#27873 = CARTESIAN_POINT ( 'NONE',  ( -8.059380280939999253, 1459.910125804190102, 215.8672651265090110 ) ) ;
#27874 = CARTESIAN_POINT ( 'NONE',  ( 9.454737631248359975, 1363.431170718790099, 210.6218459616991936 ) ) ;
#27875 = CARTESIAN_POINT ( 'NONE',  ( -45.39090023088340331, 1434.413450932079968, 266.9978870292519559 ) ) ;
#27876 = CARTESIAN_POINT ( 'NONE',  ( -2.500000000000000000, 1431.429175495760319, 184.4562418606980145 ) ) ;
#27877 = ORIENTED_EDGE ( 'NONE', *, *, #52826, .T. ) ;
#27878 = CARTESIAN_POINT ( 'NONE',  ( -8.835341282630000848, 1423.496088729460098, 209.1285750384680284 ) ) ;
#27879 = VERTEX_POINT ( 'NONE', #14663 ) ;
#27880 = CARTESIAN_POINT ( 'NONE',  ( -3.253301419385000504, 1516.790374942449944, 210.2573062871869922 ) ) ;
#27881 = DIRECTION ( 'NONE',  ( -1.755985294532469921E-16, 1.000000000000000000, -1.338183447452831989E-16 ) ) ;
#27882 = CARTESIAN_POINT ( 'NONE',  ( -15.55634920516500053, 1516.551704408390151, 193.5654967650670244 ) ) ;
#27883 = CARTESIAN_POINT ( 'NONE',  ( -16.49339310219999888, 1410.410615637530100, 191.6555828938980142 ) ) ;
#27884 = CARTESIAN_POINT ( 'NONE',  ( -2.497291879483329868, 1496.910934660279963, 221.2460707102099775 ) ) ;
#27885 = ORIENTED_EDGE ( 'NONE', *, *, #91628, .T. ) ;
#27886 = CARTESIAN_POINT ( 'NONE',  ( -15.56483135600000089, 1506.802866779329861, 193.3150509027980206 ) ) ;
#27888 = CARTESIAN_POINT ( 'NONE',  ( -28.97303002314149367, 1526.186458717542109, 197.4313369063832511 ) ) ;
#27887 = CARTESIAN_POINT ( 'NONE',  ( 0.3740406207303079711, 1452.976564550639978, 183.2744760995269928 ) ) ;
#27889 = CARTESIAN_POINT ( 'NONE',  ( -0.3911955968562167429, 1487.889068533830141, 219.9704178722953429 ) ) ;
#27890 = CARTESIAN_POINT ( 'NONE',  ( -16.92975820021440114, 1508.551704415790027, 212.8312192336030080 ) ) ;
#27891 = CARTESIAN_POINT ( 'NONE',  ( 7.003548532139999949, 1472.375330369690118, 216.7528799998890179 ) ) ;
#27892 = CARTESIAN_POINT ( 'NONE',  ( -9.119406448533400322, 1439.059517726039985, 208.3668274699830079 ) ) ;
#27893 = ORIENTED_EDGE ( 'NONE', *, *, #45670, .F. ) ;
#27894 = CARTESIAN_POINT ( 'NONE',  ( -23.03491636582509727, 1413.194898312140140, 270.3705240770690352 ) ) ;
#27895 = CARTESIAN_POINT ( 'NONE',  ( 7.323390407215000231, 1516.613712827999962, 207.9924597298270044 ) ) ;
#27896 = LINE ( 'NONE', #63192, #90092 ) ;
#27897 = CARTESIAN_POINT ( 'NONE',  ( 9.468608843732580382, 1434.567639565649870, 206.6665354939389943 ) ) ;
#27899 = VERTEX_POINT ( 'NONE', #66209 ) ;
#27898 = CARTESIAN_POINT ( 'NONE',  ( -6.030651517141524920, 1367.479084863156004, 207.6218459616988241 ) ) ;
#27900 = ORIENTED_EDGE ( 'NONE', *, *, #23589, .F. ) ;
#27901 = CARTESIAN_POINT ( 'NONE',  ( 44.79110309957884084, 1447.468097970602912, 268.9984334317801995 ) ) ;
#27902 = CARTESIAN_POINT ( 'NONE',  ( 0.6065152646886989851, 1467.309601164520018, 220.1865271459919882 ) ) ;
#27903 = CARTESIAN_POINT ( 'NONE',  ( 3.648172162208111580, 1424.944969327661283, 184.9068109353121940 ) ) ;
#27904 = CARTESIAN_POINT ( 'NONE',  ( -0.01186867620443360014, 1408.939236553560022, 186.1929645843580090 ) ) ;
#27905 = B_SPLINE_CURVE_WITH_KNOTS ( 'NONE', 3,
 ( #82120, #41231, #5422, #24407, #107875, #5974, #49644, #31163, #74304, #6522, #92181, #83780, #32814 ),
 .UNSPECIFIED., .F., .F.,
 ( 4, 3, 3, 3, 4 ),
 ( 0.000000000000000000, 0.9022774465060450222, 1.803253076899530072, 2.701853961413190230, 3.242714680140000194 ),
 .UNSPECIFIED. ) ;
#27906 = CARTESIAN_POINT ( 'NONE',  ( -18.44487993178400131, 1415.666200586320201, 207.5693722478499978 ) ) ;
#27907 = CARTESIAN_POINT ( 'NONE',  ( -20.60769613969999980, 1425.808610859230157, 221.1268796063979778 ) ) ;
#27908 = AXIS2_PLACEMENT_3D ( 'NONE', #10971, #78162, #1474 ) ;
#27909 = ADVANCED_FACE ( 'NONE', ( #83514 ), #110084, .T. ) ;
#27910 = CARTESIAN_POINT ( 'NONE',  ( 15.61100558644629999, 1473.362487039310054, 269.5822769614250092 ) ) ;
#27911 = CARTESIAN_POINT ( 'NONE',  ( -5.330260781521928060, 1466.317908316536659, 234.3275359498189800 ) ) ;
#27912 = CARTESIAN_POINT ( 'NONE',  ( 10.27848897229999992, 1446.428916322279974, 186.7328515026979971 ) ) ;
#27913 = CARTESIAN_POINT ( 'NONE',  ( -7.725990199955000470, 1517.181921232829836, 206.6366402828969910 ) ) ;
#27914 = EDGE_LOOP ( 'NONE', ( #79007, #39510, #83442, #38739, #93961 ) ) ;
#27915 = LINE ( 'NONE', #61538, #72284 ) ;
#27916 = CARTESIAN_POINT ( 'NONE',  ( 1.482817440028709965, 1476.038795360169843, 182.4686008787339802 ) ) ;
#27917 = ORIENTED_EDGE ( 'NONE', *, *, #106740, .T. ) ;
#27918 = CARTESIAN_POINT ( 'NONE',  ( 4.858360384088095785, 1508.551704408384467, 212.6094383991669758 ) ) ;
#27920 = EDGE_CURVE ( 'NONE', #106524, #71158, #41028, .T. ) ;
#27919 = CARTESIAN_POINT ( 'NONE',  ( 25.43929575127770093, 1451.150448064199963, 137.0720221098989953 ) ) ;
#27921 = CARTESIAN_POINT ( 'NONE',  ( -13.43605234887320243, 1430.070734077150064, 196.2030595958090089 ) ) ;
#27922 = CARTESIAN_POINT ( 'NONE',  ( -22.66805973949999853, 1388.284003322340141, 203.4481520923190203 ) ) ;
#27923 = DIRECTION ( 'NONE',  ( 0.5224574779879248565, 0.7067418228238977473, -0.4770263929449307105 ) ) ;
#27924 = CARTESIAN_POINT ( 'NONE',  ( 17.39803002860000092, 1409.685664280330002, 193.5282844070979991 ) ) ;
#27925 = CARTESIAN_POINT ( 'NONE',  ( 18.64337105059429689, 1443.913060387331825, 162.1710875046050830 ) ) ;
#27926 = CARTESIAN_POINT ( 'NONE',  ( 3.625788738682097279, 1439.697084659004531, 184.5692930381153758 ) ) ;
#27928 = CARTESIAN_POINT ( 'NONE',  ( -19.88588797745208581, 1426.224259812586979, 222.6860395134592920 ) ) ;
#27927 = LINE ( 'NONE', #4249, #5632 ) ;
#27929 = CARTESIAN_POINT ( 'NONE',  ( 0.6545676963618470845, 1450.893079684980194, 181.6462381494110048 ) ) ;
#27930 = CARTESIAN_POINT ( 'NONE',  ( -9.791709161030000885, 1382.673534642720142, 218.0041932793789954 ) ) ;
#27931 = CARTESIAN_POINT ( 'NONE',  ( 6.559798056295000457, 1516.987478262539980, 213.7368632980669929 ) ) ;
#27932 = CARTESIAN_POINT ( 'NONE',  ( 27.15680186111980277, 1447.232003934320119, 137.0388483343459995 ) ) ;
#27933 = ORIENTED_EDGE ( 'NONE', *, *, #25860, .F. ) ;
#27934 = CARTESIAN_POINT ( 'NONE',  ( -15.75277756397573725, 1465.459959653623173, 221.5528956270499918 ) ) ;
#27935 = CARTESIAN_POINT ( 'NONE',  ( -9.878262157267270638, 1481.129258223239958, 205.3616989145060074 ) ) ;
#27936 = CARTESIAN_POINT ( 'NONE',  ( -0.4098070700370579633, 1409.180871098390071, 232.5580995887669928 ) ) ;
#27937 = CIRCLE ( 'NONE', #22542, 95.87933833688167340 ) ;
#27938 = CARTESIAN_POINT ( 'NONE',  ( 9788.078716724870901, 2833.596074015789782, 1421.913706743000148 ) ) ;
#27939 = CYLINDRICAL_SURFACE ( 'NONE', #81548, 1.999999999999996669 ) ;
#27940 = EDGE_CURVE ( 'NONE', #39550, #89436, #83183, .T. ) ;
#27941 = CARTESIAN_POINT ( 'NONE',  ( -4.327392289582439489, 1515.143326931960019, 208.6051541441859740 ) ) ;
#27942 = CARTESIAN_POINT ( 'NONE',  ( -9.019386502799999761, 1461.887471368730075, 248.0989693022980020 ) ) ;
#27943 = CARTESIAN_POINT ( 'NONE',  ( 45.55047695329995605, 1443.690990841655321, 266.1919662023980777 ) ) ;
#27944 = CARTESIAN_POINT ( 'NONE',  ( 11.06650222010000029, 1433.167564766650003, 151.7066924991980272 ) ) ;
#27945 = CARTESIAN_POINT ( 'NONE',  ( -2.383927472408579717, 1474.129566312720044, 270.1365026341109683 ) ) ;
#27946 = CARTESIAN_POINT ( 'NONE',  ( 26.90416343740999849, 1440.913060391219915, 226.3888494030570087 ) ) ;
#27947 = CARTESIAN_POINT ( 'NONE',  ( -21.43945572710000036, 1508.012730663529737, 227.0658374796979899 ) ) ;
#27948 = CARTESIAN_POINT ( 'NONE',  ( -14.14028587358620115, 1420.975139497910050, 196.1143637960159936 ) ) ;
#27949 = ORIENTED_EDGE ( 'NONE', *, *, #48082, .T. ) ;
#27950 = CARTESIAN_POINT ( 'NONE',  ( -34.18677586421195258, 1522.382868172863937, 198.4504086008750505 ) ) ;
#27951 = CARTESIAN_POINT ( 'NONE',  ( 23.61230825720000226, 1435.322028862560046, 137.2857987807979896 ) ) ;
#27952 = CARTESIAN_POINT ( 'NONE',  ( -7.033373300310000964, 1486.517874593030001, 182.5016472222980042 ) ) ;
#27953 = CARTESIAN_POINT ( 'NONE',  ( -1.775988990185336736, 1526.208281990536079, 240.5699127611742938 ) ) ;
#27954 = CARTESIAN_POINT ( 'NONE',  ( 2.890489019979999963, 1507.108937782129942, 235.9439513777979869 ) ) ;
#27955 = CARTESIAN_POINT ( 'NONE',  ( 24.81840806639999997, 1430.361839715729730, 209.9936183716149856 ) ) ;
#27956 = CARTESIAN_POINT ( 'NONE',  ( -17.01076621896756791, 1419.968529181750682, 207.7081154596805277 ) ) ;
#27957 = CARTESIAN_POINT ( 'NONE',  ( -11.97142003969999990, 1507.754042655929879, 233.5465281419980101 ) ) ;
#27958 = CARTESIAN_POINT ( 'NONE',  ( -28.58153792528539583, 1383.843833704670033, 226.4053923691060106 ) ) ;
#27959 = CARTESIAN_POINT ( 'NONE',  ( -4.246467356640679647, 1508.879014458369966, 205.3739677720240024 ) ) ;
#27960 = CARTESIAN_POINT ( 'NONE',  ( 18.64646848244989741, 1416.843574548044216, 209.6840263755165381 ) ) ;
#27961 = CARTESIAN_POINT ( 'NONE',  ( 1766.069695707609526, -8382.262153571264207, 2383.103299250912187 ) ) ;
#27962 = CARTESIAN_POINT ( 'NONE',  ( 0.1682346187407569860, 1481.367886108869925, 182.0356305680300011 ) ) ;
#27964 = ORIENTED_EDGE ( 'NONE', *, *, #110442, .F. ) ;
#27963 = CARTESIAN_POINT ( 'NONE',  ( 5.311671089129999856, 1436.871628643890062, 207.8685812842290375 ) ) ;
#27965 = CARTESIAN_POINT ( 'NONE',  ( -9.183039342186225085, 1388.489910760221164, 200.7797177079488335 ) ) ;
#27966 = CARTESIAN_POINT ( 'NONE',  ( -4.818091668840000175, 1474.858187015290014, 199.5909790158089834 ) ) ;
#27968 = ORIENTED_EDGE ( 'NONE', *, *, #109619, .T. ) ;
#27967 = CARTESIAN_POINT ( 'NONE',  ( -37.10988369677580323, 1450.944967383530184, 134.0999999986949831 ) ) ;
#27969 = CARTESIAN_POINT ( 'NONE',  ( -7.198248339227330206, 1508.551704405200098, 219.1372379941830388 ) ) ;
#27970 = ORIENTED_EDGE ( 'NONE', *, *, #88751, .F. ) ;
#27971 = CARTESIAN_POINT ( 'NONE',  ( -12.44728924775969858, 1391.409032655050169, 210.6741896695639866 ) ) ;
#27972 = DIRECTION ( 'NONE',  ( -0.4090087482554183862, 0.000000000000000000, 0.9125304618754027652 ) ) ;
#27973 = CARTESIAN_POINT ( 'NONE',  ( -2.818453812998270802, 1509.034654136871495, 238.5774661494029090 ) ) ;
#27974 = CARTESIAN_POINT ( 'NONE',  ( 4.291176059336820003, 1446.971469614359876, 154.7965853925720126 ) ) ;
#27975 = CARTESIAN_POINT ( 'NONE',  ( -2.479799395000000128, 1432.887831698689979, 218.3414119524190085 ) ) ;
#27976 = CARTESIAN_POINT ( 'NONE',  ( -11.02285301547030016, 1471.443673802609965, 206.7922591627839779 ) ) ;
#27977 = CARTESIAN_POINT ( 'NONE',  ( 11.61231359760869886, 1409.318571304570014, 218.5364820568740072 ) ) ;
#27978 = CARTESIAN_POINT ( 'NONE',  ( -7.966182304005879899, 1384.912218263729983, 199.4893151478169955 ) ) ;
#27979 = CARTESIAN_POINT ( 'NONE',  ( -98.12087982326850977, 1385.216017296190103, 295.8782037632710171 ) ) ;
#27980 = FACE_OUTER_BOUND ( 'NONE', #18453, .T. ) ;
#27981 = CARTESIAN_POINT ( 'NONE',  ( -14.53473304376390018, 1379.710786975620067, 208.2794084638009906 ) ) ;
#27982 = EDGE_LOOP ( 'NONE', ( #107628, #58428, #21238 ) ) ;
#27983 = CARTESIAN_POINT ( 'NONE',  ( 11.12217965309999812, 1433.940707244100167, 151.6712567464980168 ) ) ;
#27984 = DIRECTION ( 'NONE',  ( 0.01793599824082334204, -0.9688514294439565244, 0.2469923230213998122 ) ) ;
#27986 = VERTEX_POINT ( 'NONE', #101962 ) ;
#27985 = CARTESIAN_POINT ( 'NONE',  ( -1.581901184577762409, 1426.946688134061105, 137.0999999980979567 ) ) ;
#27987 = ORIENTED_EDGE ( 'NONE', *, *, #46007, .T. ) ;
#27988 = CARTESIAN_POINT ( 'NONE',  ( -11.90198537395339962, 1415.595619977640126, 195.0235258899830058 ) ) ;
#27989 = CARTESIAN_POINT ( 'NONE',  ( -5.986709854369999917, 1361.264879806939916, 207.6218459616989946 ) ) ;
#27990 = CARTESIAN_POINT ( 'NONE',  ( -2.425929306259190010, 1495.896635296460090, 197.0250612545490014 ) ) ;
#27991 = CARTESIAN_POINT ( 'NONE',  ( 29.83201784440627335, 1462.372200568356220, 269.4690239067755329 ) ) ;
#27992 = CARTESIAN_POINT ( 'NONE',  ( 11.52300753767129926, 1427.577114572419759, 209.4088601504140286 ) ) ;
#27993 = CARTESIAN_POINT ( 'NONE',  ( 5.033382749860000338, 1397.146220404329824, 220.9814784287979990 ) ) ;
#27994 = CARTESIAN_POINT ( 'NONE',  ( 31.11295512653393303, 1525.790287071783951, 201.8987506415136295 ) ) ;
#27995 = CARTESIAN_POINT ( 'NONE',  ( 20.84167173783890092, 1473.796610273650003, 209.3926063897190204 ) ) ;
#27996 = CARTESIAN_POINT ( 'NONE',  ( -1.206033063790000082, 1476.687496009330061, 182.5563120943979811 ) ) ;
#27997 = CARTESIAN_POINT ( 'NONE',  ( -9.248485401361245195, 1369.066561549477910, 208.3718459617010978 ) ) ;
#27998 = CARTESIAN_POINT ( 'NONE',  ( -26.16739620090311291, 1436.693404600586746, 136.8894152260586452 ) ) ;
#27999 = CARTESIAN_POINT ( 'NONE',  ( -6.563595907815000352, 1517.154223579619838, 206.8322214998769937 ) ) ;
#28000 = DIRECTION ( 'NONE',  ( -0.8090169943749465631, -0.000000000000000000, 0.5877852522924742473 ) ) ;
#28001 = CARTESIAN_POINT ( 'NONE',  ( -7.012921583638330070, 1508.551704408389924, 203.6084103760139783 ) ) ;
#28002 = CARTESIAN_POINT ( 'NONE',  ( 0.8070291312159990627, 1495.806080077989918, 221.0513106237990257 ) ) ;
#28003 = CARTESIAN_POINT ( 'NONE',  ( 41.20764152666490077, 1444.152539026100158, 136.7061128974409883 ) ) ;
#28004 = VERTEX_POINT ( 'NONE', #16836 ) ;
#28005 = CARTESIAN_POINT ( 'NONE',  ( 37.00345306050000005, 1420.039538152829891, 266.5575588314979996 ) ) ;
#28006 = CARTESIAN_POINT ( 'NONE',  ( -27.14725374240000022, 1488.689090778130094, 207.3572097627179858 ) ) ;
#28008 = CARTESIAN_POINT ( 'NONE',  ( 13.57909981250000087, 1416.568813547830132, 196.3459685238979944 ) ) ;
#28007 = CARTESIAN_POINT ( 'NONE',  ( 1.451130014660000134, 1504.651021693529856, 181.2207292498980280 ) ) ;
#28009 = CARTESIAN_POINT ( 'NONE',  ( -3.446329813785000251, 1516.812046502680005, 212.0014881234369852 ) ) ;
#28010 = DIRECTION ( 'NONE',  ( -0.6736849260863839728, 0.000000000000000000, 0.7390186874254150995 ) ) ;
#28011 = B_SPLINE_CURVE_WITH_KNOTS ( 'NONE', 3,
 ( #46687, #80818, #29851, #107111, #20888, #74081, #4124, #38249, #64037, #98154, #29303, #81344, #89759, #82470, #81898, #90297, #5205, #23090, #107667, #21427, #37710, #31498, #63500, #12508, #5768, #13578, #80272, #39911, #55637, #65678, #56161, #72433, #99796, #91423, #65128, #71911, #30399, #64590, #97619 ),
 .UNSPECIFIED., .F., .F.,
 ( 4, 2, 2, 2, 1, 1, 1, 2, 2, 2, 2, 1, 1, 1, 2, 2, 2, 2, 1, 1, 1, 2, 2, 4 ),
 ( 0.000000000000000000, 0.1249999999999992506, 0.1874999999999988343, 0.2187500000000000278, 0.2343749999999804323, 0.2421874999999872324, 0.2460937499999715228, 0.2480468749999621692, 0.2499999999999528433, 0.3749999999997775668, 0.4374999999996881939, 0.4687499999996582734, 0.4843749999996572742, 0.4921874999996567746, 0.4960937499996547762, 0.4999999999996528333, 0.6249999999998488986, 0.6874999999999484857, 0.7187499999999996669, 0.7343750000000252021, 0.7421875000000365263, 0.7460937500000437428, 0.7500000000000508482, 1.000000000000000000 ),
 .UNSPECIFIED. ) ;
#28012 = CARTESIAN_POINT ( 'NONE',  ( -22.71362857409999947, 1419.354696850730079, 250.3594883093980172 ) ) ;
#28013 = CARTESIAN_POINT ( 'NONE',  ( 3.323701945149999393, 1484.956221099589811, 220.0842286830989849 ) ) ;
#28014 = CARTESIAN_POINT ( 'NONE',  ( 28.61821586768189718, 1509.224669306330043, 209.4805676029000097 ) ) ;
#28015 = CARTESIAN_POINT ( 'NONE',  ( 19.52205342210000083, 1473.076230373790168, 204.3554439105789982 ) ) ;
#28016 = CARTESIAN_POINT ( 'NONE',  ( 33.91369255499999724, 1451.728777076330061, 134.7155730073980067 ) ) ;
#28017 = ORIENTED_EDGE ( 'NONE', *, *, #65048, .T. ) ;
#28018 = DIRECTION ( 'NONE',  ( 0.4978433412588781914, 0.000000000000000000, 0.8672669759446606230 ) ) ;
#28019 = DIRECTION ( 'NONE',  ( 0.000000000000000000, 0.000000000000000000, -1.000000000000000000 ) ) ;
#28020 = CARTESIAN_POINT ( 'NONE',  ( -18.63536074199999959, 1457.257477148429871, 229.6471845788980204 ) ) ;
#28021 = ORIENTED_EDGE ( 'NONE', *, *, #95276, .F. ) ;
#28022 = ORIENTED_EDGE ( 'NONE', *, *, #43399, .T. ) ;
#28023 = B_SPLINE_CURVE_WITH_KNOTS ( 'NONE', 3,
 ( #24362, #7575, #41729, #77001, #105366, #97511, #77549, #37605, #103264, #37048, #9241, #52366, #46579, #96973, #80713, #4022, #85367, #25455, #34434, #20237, #51799, #59649 ),
 .UNSPECIFIED., .F., .F.,
 ( 4, 3, 3, 3, 3, 3, 3, 4 ),
 ( 0.000000000000000000, 1.302509916939140089, 2.511839277136839854, 3.228995734685269792, 4.125930029771439855, 5.291961157905718416, 6.057839889249209797, 6.457992286039999641 ),
 .UNSPECIFIED. ) ;
#28024 = CARTESIAN_POINT ( 'NONE',  ( 9.164720064741960215, 1452.458489836430090, 211.4562277055130153 ) ) ;
#28025 = CARTESIAN_POINT ( 'NONE',  ( 8.043354450609999873, 1424.603816335180227, 195.4430761869989794 ) ) ;
#28026 = VERTEX_POINT ( 'NONE', #646 ) ;
#28027 = CARTESIAN_POINT ( 'NONE',  ( -7.604289863101939773, 1426.735970264149955, 206.0920986175900111 ) ) ;
#28028 = CARTESIAN_POINT ( 'NONE',  ( -5.864566082395460178, 1522.051704408389924, 192.0899093523580063 ) ) ;
#28029 = DIRECTION ( 'NONE',  ( 0.7414773880254614813, 0.000000000000000000, -0.6709778558543786353 ) ) ;
#28030 = CARTESIAN_POINT ( 'NONE',  ( -2.866976920500000414, 1479.772520933030137, 235.6353344876980032 ) ) ;
#28031 = CARTESIAN_POINT ( 'NONE',  ( 5.513258746607349714, 1508.551704615640119, 202.1093796504439979 ) ) ;
#28032 = CARTESIAN_POINT ( 'NONE',  ( 45.88361912325480318, 1441.846453202439989, 266.4122209686929637 ) ) ;
#28033 = CARTESIAN_POINT ( 'NONE',  ( -12.09197207240000083, 1391.856376936869992, 209.7328825797320064 ) ) ;
#28034 = CARTESIAN_POINT ( 'NONE',  ( 13.93012033159999952, 1463.781730353329976, 224.9320934324980215 ) ) ;
#28035 = EDGE_LOOP ( 'NONE', ( #10423, #48980, #96384, #78236 ) ) ;
#28036 = CARTESIAN_POINT ( 'NONE',  ( 3.258474578945000033, 1517.083030555940013, 202.5598499717069956 ) ) ;
#28037 = CARTESIAN_POINT ( 'NONE',  ( -1.701850495234999983, 1516.908147884120126, 210.2591426210370003 ) ) ;
#28038 = ORIENTED_EDGE ( 'NONE', *, *, #21447, .T. ) ;
#28039 = CARTESIAN_POINT ( 'NONE',  ( 11.85752262936500045, 1431.737903649139980, 149.9496635218089864 ) ) ;
#28040 = DIRECTION ( 'NONE',  ( -0.000000000000000000, -0.000000000000000000, -1.000000000000000000 ) ) ;
#28041 = ORIENTED_EDGE ( 'NONE', *, *, #39710, .T. ) ;
#28042 = CARTESIAN_POINT ( 'NONE',  ( 4.364191681395142908, 1509.032014410904821, 213.2377288302579359 ) ) ;
#28043 = CARTESIAN_POINT ( 'NONE',  ( -3.747744696529340391, 1508.283495248520012, 220.6268602264730134 ) ) ;
#28044 = CARTESIAN_POINT ( 'NONE',  ( -0.1681681984989999989, 1418.913060387330006, 172.2701767054979882 ) ) ;
#28045 = CARTESIAN_POINT ( 'NONE',  ( -7.584666794553579727, 1470.726758701579911, 215.8813880928350102 ) ) ;
#28046 = CARTESIAN_POINT ( 'NONE',  ( -4.275814211600000192, 1424.445698836229894, 185.6670158391980010 ) ) ;
#28047 = CARTESIAN_POINT ( 'NONE',  ( 3.196891693280000002, 1407.733286134229957, 270.1354749225980072 ) ) ;
#28048 = CARTESIAN_POINT ( 'NONE',  ( -106.5486053249999969, 1387.898087395329867, 298.3709353731589999 ) ) ;
#28049 = CARTESIAN_POINT ( 'NONE',  ( -109.8138132439963499, 1383.469406728881495, 297.1129651261376807 ) ) ;
#28050 = CARTESIAN_POINT ( 'NONE',  ( 9.946821680530000265, 1491.974962277590066, 214.0087608140690065 ) ) ;
#28051 = CARTESIAN_POINT ( 'NONE',  ( -26.05523246079999922, 1379.607910947010168, 211.4271914385990101 ) ) ;
#28052 = CARTESIAN_POINT ( 'NONE',  ( 8.327730581979166047, 1424.424880086262192, 195.7445179161305191 ) ) ;
#28054 = CARTESIAN_POINT ( 'NONE',  ( 2.719262146893400038E-32, 1524.051704408389924, 209.1218459616989946 ) ) ;
#28053 = CARTESIAN_POINT ( 'NONE',  ( -19.29582496549999959, 1504.771663335689937, 209.4684985698930006 ) ) ;
#28055 = CARTESIAN_POINT ( 'NONE',  ( -65.86034991192448729, 1379.747388898481177, 276.1189993386147989 ) ) ;
#28056 = CARTESIAN_POINT ( 'NONE',  ( -9.897863003022139949, 1439.796600576999936, 207.6605474465260102 ) ) ;
#28057 = B_SPLINE_CURVE_WITH_KNOTS ( 'NONE', 5,
 ( #86895, #10756, #53319, #103125, #103697, #104254 ),
 .UNSPECIFIED., .F., .F.,
 ( 6, 6 ),
 ( -48.30090645053910237, -44.26078367470000074 ),
 .UNSPECIFIED. ) ;
#28058 = CARTESIAN_POINT ( 'NONE',  ( -7.653848905685000759, 1514.071098020770023, 202.5580345204870127 ) ) ;
#28059 = ORIENTED_EDGE ( 'NONE', *, *, #73820, .T. ) ;
#28060 = CARTESIAN_POINT ( 'NONE',  ( 12.48077398309999886, 1422.454772915230024, 243.9198229250980035 ) ) ;
#28061 = CARTESIAN_POINT ( 'NONE',  ( -156.6846457583342840, 1526.382868172863937, 340.9912860285748479 ) ) ;
#28062 = AXIS2_PLACEMENT_3D ( 'NONE', #37062, #103142, #60637 ) ;
#28063 = CARTESIAN_POINT ( 'NONE',  ( -69.80115760975569117, 1385.024861833069963, 294.8489851850470131 ) ) ;
#28064 = CARTESIAN_POINT ( 'NONE',  ( -19.33418355719859960, 1523.342713519622748, 179.0109766843198997 ) ) ;
#28065 = CARTESIAN_POINT ( 'NONE',  ( 5.247543271890000582, 1505.478499777190109, 219.9306779546989787 ) ) ;
#28066 = CARTESIAN_POINT ( 'NONE',  ( 2.902322711624676882E-15, 1523.051704408389696, 232.8211094035767985 ) ) ;
#28068 = ORIENTED_EDGE ( 'NONE', *, *, #25614, .T. ) ;
#28067 = CARTESIAN_POINT ( 'NONE',  ( 1.345088944733950020, 1515.083299843980058, 204.7928818079469977 ) ) ;
#28069 = CARTESIAN_POINT ( 'NONE',  ( -15.77920420956434278, 1415.808500209527892, 209.6969280600988270 ) ) ;
#28071 = B_SPLINE_CURVE_WITH_KNOTS ( 'NONE', 3,
 ( #46953, #37432, #81073, #71630, #54794, #97326, #72695, #21696, #105750, #4389 ),
 .UNSPECIFIED., .F., .F.,
 ( 4, 2, 2, 2, 4 ),
 ( 0.000000000000000000, 0.2500000000000000000, 0.5000000000000000000, 0.7500000000000000000, 1.000000000000000000 ),
 .UNSPECIFIED. ) ;
#28070 = CARTESIAN_POINT ( 'NONE',  ( -24.04512698680000327, 1444.427565174400115, 211.8281269584280153 ) ) ;
#28072 = CARTESIAN_POINT ( 'NONE',  ( -2.494317414332789529, 1449.209847618189542, 154.5141281627416561 ) ) ;
#28073 = CARTESIAN_POINT ( 'NONE',  ( -6.403692060479999171, 1460.996305860290249, 208.5086931504900178 ) ) ;
#28074 = CARTESIAN_POINT ( 'NONE',  ( 14.83035613263499997, 1514.570049710740022, 225.4041969180670151 ) ) ;
#28075 = CARTESIAN_POINT ( 'NONE',  ( -10.55869165969999912, 1442.273726812979930, 186.3969298045979883 ) ) ;
#28076 = CARTESIAN_POINT ( 'NONE',  ( 27.60850322493959652, 1509.877168147730117, 194.6763840514340131 ) ) ;
#28077 = CARTESIAN_POINT ( 'NONE',  ( 18.19590854888166476, 1512.187213306747481, 238.2026672068774360 ) ) ;
#28078 = DIRECTION ( 'NONE',  ( -0.000000000000000000, -1.000000000000000000, -0.000000000000000000 ) ) ;
#28079 = CARTESIAN_POINT ( 'NONE',  ( 15.56606087930000015, 1415.086919075230071, 227.3762381457980268 ) ) ;
#28080 = ADVANCED_FACE ( 'NONE', ( #34777 ), #84072, .T. ) ;
#28081 = CARTESIAN_POINT ( 'NONE',  ( -3.439963044070000198, 1475.703222825189869, 218.9903645809689863 ) ) ;
#28082 = CARTESIAN_POINT ( 'NONE',  ( -16.06782005780000233, 1459.209651374430223, 230.7189234877979800 ) ) ;
#28083 = CARTESIAN_POINT ( 'NONE',  ( -0.7578858299649979813, 1516.872851364150165, 206.6414186775969881 ) ) ;
#28084 = CARTESIAN_POINT ( 'NONE',  ( 43.90552978530000416, 1429.946926731829990, 266.4740132303979863 ) ) ;
#28085 = CIRCLE ( 'NONE', #51336, 29.82803840400378803 ) ;
#28086 = CARTESIAN_POINT ( 'NONE',  ( -31.74003925669971338, 1524.382868172804365, 216.5565202880893878 ) ) ;
#28087 = CARTESIAN_POINT ( 'NONE',  ( 21.03533413319999923, 1435.660194803150034, 143.7853187944979823 ) ) ;
#28088 = CARTESIAN_POINT ( 'NONE',  ( 19.43264287389999723, 1488.590530053829980, 189.7255375135980273 ) ) ;
#28089 = CARTESIAN_POINT ( 'NONE',  ( 5.366477781255650115, 1426.058802480919894, 152.4456445666100137 ) ) ;
#28090 = CARTESIAN_POINT ( 'NONE',  ( -12.98408369926140082, 1379.322469185889986, 207.9131530563359718 ) ) ;
#28091 = CARTESIAN_POINT ( 'NONE',  ( 12.61640438649999929, 1416.837080248530128, 223.3238927091979917 ) ) ;
#28092 = CARTESIAN_POINT ( 'NONE',  ( -15.09085391114290076, 1417.962848745290103, 203.1738905416179932 ) ) ;
#28093 = FACE_OUTER_BOUND ( 'NONE', #89378, .T. ) ;
#28094 = CARTESIAN_POINT ( 'NONE',  ( -21.41666160454324697, 1506.776553291482287, 202.5225393536939009 ) ) ;
#28095 = CARTESIAN_POINT ( 'NONE',  ( -15.42581583419999980, 1414.720317085819943, 208.9801203947009753 ) ) ;
#28096 = CARTESIAN_POINT ( 'NONE',  ( -12.59298689929999959, 1442.703280217149995, 186.7739262576980082 ) ) ;
#28097 = CARTESIAN_POINT ( 'NONE',  ( -1.122592899216370017E-16, 1388.079727053959914, 209.1218459616989946 ) ) ;
#28098 = FACE_OUTER_BOUND ( 'NONE', #86697, .T. ) ;
#28099 = CARTESIAN_POINT ( 'NONE',  ( -113.4000000000000057, 1379.913060387289988, 304.2218459572590064 ) ) ;
#28100 = ORIENTED_EDGE ( 'NONE', *, *, #61687, .F. ) ;
#28101 = CARTESIAN_POINT ( 'NONE',  ( 4.590060377064090424, 1517.051704403100075, 201.3992656192910147 ) ) ;
#28102 = CARTESIAN_POINT ( 'NONE',  ( -2.881436550369800287, 1409.013682368930176, 223.8287015832810027 ) ) ;
#28103 = DIRECTION ( 'NONE',  ( -1.000000000000000000, 0.000000000000000000, -1.989556701369999986E-13 ) ) ;
#28104 = LINE ( 'NONE', #1265, #79556 ) ;
#28105 = VECTOR ( 'NONE', #48336, 1000.000000000000000 ) ;
#28106 = CARTESIAN_POINT ( 'NONE',  ( -45.02947505619999902, 1451.249933470530095, 267.6322170074980136 ) ) ;
#28107 = CARTESIAN_POINT ( 'NONE',  ( -11.75272968278660102, 1481.381864203570103, 210.6216001990260054 ) ) ;
#28108 = CARTESIAN_POINT ( 'NONE',  ( 32.86802468386284914, 1523.382868172864164, 201.0396662540042030 ) ) ;
#28109 = CARTESIAN_POINT ( 'NONE',  ( -27.93022619350000113, 1509.888405378130074, 214.3883701560380075 ) ) ;
#28110 = CARTESIAN_POINT ( 'NONE',  ( -108.8958719471799981, 1384.583688962449969, 311.2497166588959772 ) ) ;
#28111 = CARTESIAN_POINT ( 'NONE',  ( -46.71757468079219677, 1385.008228226510028, 220.5181717465020199 ) ) ;
#28112 = CARTESIAN_POINT ( 'NONE',  ( 16.61248850094990104, 1423.423305472560060, 227.8798840990210124 ) ) ;
#28113 = CARTESIAN_POINT ( 'NONE',  ( 20.61224126859999828, 1508.367040381230026, 227.7934947756980080 ) ) ;
#28114 = CARTESIAN_POINT ( 'NONE',  ( -11.88064286090000010, 1433.444786854229960, 151.0525681022980109 ) ) ;
#28115 = DIRECTION ( 'NONE',  ( 1.755985294532469921E-16, -1.000000000000000000, 1.338183447452831989E-16 ) ) ;
#28116 = CARTESIAN_POINT ( 'NONE',  ( -5.153093391039999638, 1380.759461119849902, 214.7804110970890008 ) ) ;
#28117 = CARTESIAN_POINT ( 'NONE',  ( -8.371177922870000288, 1384.930186027270111, 199.7749517192889925 ) ) ;
#28118 = EDGE_CURVE ( 'NONE', #78578, #54193, #51037, .T. ) ;
#28119 = CARTESIAN_POINT ( 'NONE',  ( -24.08425369710000297, 1411.115211429229930, 208.6111293678600020 ) ) ;
#28120 = EDGE_CURVE ( 'NONE', #29671, #68939, #103065, .T. ) ;
#28121 = CARTESIAN_POINT ( 'NONE',  ( 15.13954211869999966, 1415.426091369230107, 199.2823809441580067 ) ) ;
#28122 = CARTESIAN_POINT ( 'NONE',  ( -11.95871496589999872, 1415.628674276829770, 194.9673395089980090 ) ) ;
#28123 = CARTESIAN_POINT ( 'NONE',  ( -0.0001732888907949209931, 1456.398128790439841, 144.1938086916980239 ) ) ;
#28124 = EDGE_CURVE ( 'NONE', #92455, #27860, #109966, .T. ) ;
#28125 = CARTESIAN_POINT ( 'NONE',  ( 22.92656559199999933, 1409.713673699430046, 210.2581852642179854 ) ) ;
#28126 = CARTESIAN_POINT ( 'NONE',  ( -106.4176595609719982, 1391.913060387289988, 304.5584244006879544 ) ) ;
#28127 = EDGE_CURVE ( 'NONE', #10257, #89438, #26365, .T. ) ;
#28128 = CARTESIAN_POINT ( 'NONE',  ( 8.279103254549998070, 1462.500663624690105, 228.8590808785990021 ) ) ;
#28129 = CARTESIAN_POINT ( 'NONE',  ( -14.31906343784990021, 1380.323795378649947, 209.9058136714729983 ) ) ;
#28131 = CARTESIAN_POINT ( 'NONE',  ( -12.51034971420000019, 1378.851356594869912, 207.9031378654190121 ) ) ;
#28130 = DIRECTION ( 'NONE',  ( 0.000000000000000000, 0.000000000000000000, -1.000000000000000000 ) ) ;
#28132 = CARTESIAN_POINT ( 'NONE',  ( -5.177091008439999698, 1391.906304745790067, 203.7213657723089852 ) ) ;
#28133 = DIRECTION ( 'NONE',  ( -0.3090169943749515591, 0.000000000000000000, -0.9510565162951521989 ) ) ;
#28134 = CARTESIAN_POINT ( 'NONE',  ( -11.71870426870000159, 1490.183039387389726, 210.4915346308890207 ) ) ;
#28135 = FACE_OUTER_BOUND ( 'NONE', #85429, .T. ) ;
#28136 = AXIS2_PLACEMENT_3D ( 'NONE', #32495, #85081, #110292 ) ;
#28137 = CARTESIAN_POINT ( 'NONE',  ( -1.410150725348159995, 1420.916685646099950, 183.2158715699029869 ) ) ;
#28138 = CARTESIAN_POINT ( 'NONE',  ( -0.01289782690309849988, 1516.939723362869927, 204.1155860834069813 ) ) ;
#28139 = CARTESIAN_POINT ( 'NONE',  ( -22.09796275270000265, 1430.768449482030064, 219.6318221129980088 ) ) ;
#28140 = CARTESIAN_POINT ( 'NONE',  ( -18.69874064677919634, 1486.217926523959932, 189.0579342009679920 ) ) ;
#28141 = CARTESIAN_POINT ( 'NONE',  ( 9105.849827169598939, -2339.246371527900010, 1987.591931316750106 ) ) ;
#28142 = CARTESIAN_POINT ( 'NONE',  ( -4.253357141732059254, 1441.312379553120081, 160.5446465494569850 ) ) ;
#28145 = ORIENTED_EDGE ( 'NONE', *, *, #59133, .F. ) ;
#28144 = CARTESIAN_POINT ( 'NONE',  ( -67.10245500156331389, 1379.743906473960124, 278.1969394921879939 ) ) ;
#28143 = AXIS2_PLACEMENT_3D ( 'NONE', #42429, #24507, #48655 ) ;
#28146 = EDGE_LOOP ( 'NONE', ( #33907, #600, #46102, #11774, #9708 ) ) ;
#28147 = CARTESIAN_POINT ( 'NONE',  ( 21.51496489921850852, 1524.872178180563878, 183.6916733868881124 ) ) ;
#28148 = ORIENTED_EDGE ( 'NONE', *, *, #84419, .T. ) ;
#28149 = CARTESIAN_POINT ( 'NONE',  ( -105.4633178750000013, 1378.947302253090129, 304.0408696983589607 ) ) ;
#28150 = CARTESIAN_POINT ( 'NONE',  ( 11.74132753969999854, 1499.920429264490167, 205.7525976432890218 ) ) ;
#28152 = CARTESIAN_POINT ( 'NONE',  ( 0.1625281483599999854, 1507.112338238429857, 180.9288958984979843 ) ) ;
#28151 = CARTESIAN_POINT ( 'NONE',  ( -15.72514096998889066, 1409.739244463557043, 226.1586303163210800 ) ) ;
#28153 = CARTESIAN_POINT ( 'NONE',  ( 4.637775890913160559, 1462.124487089030026, 228.1829411063220050 ) ) ;
#28154 = ADVANCED_FACE ( 'NONE', ( #33656 ), #77888, .F. ) ;
#28155 =( BOUNDED_SURFACE ( )  B_SPLINE_SURFACE ( 3, 2, ( 
 ( #99209, #22488, #56689 ),
 ( #90825, #48298, #5737 ),
 ( #39879, #34226, #85175 ),
 ( #101402, #103, #33661 ) ),
 .UNSPECIFIED., .F., .F., .T. ) 
 B_SPLINE_SURFACE_WITH_KNOTS ( ( 4, 4 ),
 ( 3, 3 ),
 ( 0.000000000000000000, 0.0002960034161023843515 ),
 ( 0.000000000000000000, 1.000000000000000000 ),
 .UNSPECIFIED. ) 
 GEOMETRIC_REPRESENTATION_ITEM ( )  RATIONAL_B_SPLINE_SURFACE ( (
 ( 1.000000000000000000, 0.8072480644198086752, 1.000000000000000000),
 ( 1.000000000000000000, 0.8072480346917653149, 1.000000000000000000),
 ( 1.000000000000000000, 0.8071723757218337569, 1.000000000000000000),
 ( 1.000000000000000000, 0.8070209408750013136, 1.000000000000000000) ) ) 
 REPRESENTATION_ITEM ( '' )  SURFACE ( )  );
#28156 = CARTESIAN_POINT ( 'NONE',  ( 15.44339577220000059, 1507.633509799529975, 186.9079894093979988 ) ) ;
#28157 = CARTESIAN_POINT ( 'NONE',  ( -0.8252990750830009326, 1467.903802984689946, 219.8254095440989886 ) ) ;
#28158 = CARTESIAN_POINT ( 'NONE',  ( 7.168422058350000015, 1409.330743147429985, 230.2017730211979938 ) ) ;
#28159 = FILL_AREA_STYLE ('',( #87530 ) ) ;
#28160 = CARTESIAN_POINT ( 'NONE',  ( 3.267603515704999850, 1516.858171774179937, 212.3749871074670068 ) ) ;
#28161 = EDGE_CURVE ( 'NONE', #67656, #53131, #59688, .T. ) ;
#28162 = CARTESIAN_POINT ( 'NONE',  ( 41.06928241250569300, 1446.732447649089863, 134.0999999985529882 ) ) ;
#28163 = CARTESIAN_POINT ( 'NONE',  ( -4.721762350340170222, 1427.756354696789913, 206.2331009145199801 ) ) ;
#28164 = CARTESIAN_POINT ( 'NONE',  ( -5399.972634328954882, 2837.742859910729294, -8135.989823645887554 ) ) ;
#28165 = ORIENTED_EDGE ( 'NONE', *, *, #107488, .T. ) ;
#28166 = CARTESIAN_POINT ( 'NONE',  ( 3.217370068670000194, 1424.184623524309927, 188.9579833761989960 ) ) ;
#28167 = CARTESIAN_POINT ( 'NONE',  ( -0.02955819112566700213, 1522.051704408389924, 225.0080808726450243 ) ) ;
#28168 = ORIENTED_EDGE ( 'NONE', *, *, #36962, .T. ) ;
#28169 = ORIENTED_EDGE ( 'NONE', *, *, #44711, .F. ) ;
#28170 = ADVANCED_FACE ( 'NONE', ( #71736 ), #86902, .F. ) ;
#28171 = ORIENTED_EDGE ( 'NONE', *, *, #51535, .F. ) ;
#28172 = CARTESIAN_POINT ( 'NONE',  ( -8.640072926265000675, 1511.773927532309926, 215.2821261476370012 ) ) ;
#28173 = CARTESIAN_POINT ( 'NONE',  ( 16.78766063793228014, 1513.436209039135292, 196.1310004108296141 ) ) ;
#28174 = CARTESIAN_POINT ( 'NONE',  ( 13.15671565689999944, 1428.802034784529951, 222.6511392629980151 ) ) ;
#28175 = VECTOR ( 'NONE', #63236, 999.9999999999998863 ) ;
#28176 = CARTESIAN_POINT ( 'NONE',  ( -1.530900592538410043, 1457.980095062469900, 229.8454460011110143 ) ) ;
#28177 = CARTESIAN_POINT ( 'NONE',  ( 9.854289541820000053, 1461.890233428590136, 208.5812305969039926 ) ) ;
#28178 = EDGE_CURVE ( 'NONE', #22756, #58583, #90284, .T. ) ;
#28179 = CARTESIAN_POINT ( 'NONE',  ( -17.94888193757963890, 1447.286725237485371, 216.7531926085807470 ) ) ;
#28180 = CARTESIAN_POINT ( 'NONE',  ( -58.82645245001332768, 1379.720749110920906, 258.7270466031295086 ) ) ;
#28181 = CARTESIAN_POINT ( 'NONE',  ( 2.329876351239999810, 1465.568987598989906, 199.1151359320989798 ) ) ;
#28182 = VERTEX_POINT ( 'NONE', #87396 ) ;
#28183 = CARTESIAN_POINT ( 'NONE',  ( -5.013274999515000552, 1517.068517094990057, 206.8347616620369820 ) ) ;
#28184 = VERTEX_POINT ( 'NONE', #36426 ) ;
#28185 = CARTESIAN_POINT ( 'NONE',  ( 26.22923941070369835, 1440.913060387330006, 242.8863953517110019 ) ) ;
#28186 = CARTESIAN_POINT ( 'NONE',  ( -0.0001467037859797497713, 1452.764096049401132, 153.2008905006179020 ) ) ;
#28187 = VERTEX_POINT ( 'NONE', #28027 ) ;
#28188 = CARTESIAN_POINT ( 'NONE',  ( -7.167024603737270461, 1508.551565959610116, 203.6086025299220239 ) ) ;
#28189 = CARTESIAN_POINT ( 'NONE',  ( -14.43454037350000085, 1409.919030993929937, 190.6684835116980139 ) ) ;
#28190 = CARTESIAN_POINT ( 'NONE',  ( -47.05742503048701764, 1379.681822875473699, 240.2470098597866297 ) ) ;
#28192 = CARTESIAN_POINT ( 'NONE',  ( 6.784288798619999561, 1469.672316088890057, 209.8806407344229967 ) ) ;
#28191 = CARTESIAN_POINT ( 'NONE',  ( -24.39234957080000044, 1440.942612022289950, 211.3352087105480166 ) ) ;
#28193 = CARTESIAN_POINT ( 'NONE',  ( -4.738498500012391368, 1427.169020172040746, 137.0999999980979851 ) ) ;
#28194 = CARTESIAN_POINT ( 'NONE',  ( 0.0002693575158267318766, 1396.632379581024907, 196.5747687561042767 ) ) ;
#28195 = CARTESIAN_POINT ( 'NONE',  ( -13.09824453989481974, 1434.823787125280205, 146.9138453073250616 ) ) ;
#28196 = CARTESIAN_POINT ( 'NONE',  ( -11.87921130439999828, 1433.311613823580274, 149.2720837588979919 ) ) ;
#28197 = CARTESIAN_POINT ( 'NONE',  ( -4.721942846059999255, 1507.702795164189865, 221.1964433947989903 ) ) ;
#28199 = CARTESIAN_POINT ( 'NONE',  ( 5.365832140090000202, 1437.051389308390071, 208.1168906416689879 ) ) ;
#28198 = CARTESIAN_POINT ( 'NONE',  ( 10.04917727119999959, 1464.412817549529791, 232.3873387124980070 ) ) ;
#28200 = TOROIDAL_SURFACE ( 'NONE', #15602, 3.500000000000000000, 0.5000000000000000000 ) ;
#28201 = CARTESIAN_POINT ( 'NONE',  ( 2.292307230374999616, 1516.548716157039962, 216.0554627912370051 ) ) ;
#28202 = CARTESIAN_POINT ( 'NONE',  ( -31.12456774391156600, 1525.960063244517187, 217.0912716842400698 ) ) ;
#28203 = CARTESIAN_POINT ( 'NONE',  ( 5.469699236675529264, 1510.954290761809943, 216.7857353825710049 ) ) ;
#28204 = CARTESIAN_POINT ( 'NONE',  ( 27.78452743450000284, 1508.000976256729928, 207.7754991279980175 ) ) ;
#28205 = CARTESIAN_POINT ( 'NONE',  ( 4.624099291334999862, 1516.962555622980062, 212.3771868965270073 ) ) ;
#28206 = CARTESIAN_POINT ( 'NONE',  ( -18.06710007320000244, 1416.825245919329973, 209.3442279612220034 ) ) ;
#28207 = CARTESIAN_POINT ( 'NONE',  ( 18.03609881821840233, 1455.831125781012133, 201.4491494968732468 ) ) ;
#28209 = EDGE_LOOP ( 'NONE', ( #65889, #28971, #75484, #82688 ) ) ;
#28208 = CARTESIAN_POINT ( 'NONE',  ( -84.05014466280000818, 1386.741936841920051, 288.1383773578590421 ) ) ;
#28210 = CARTESIAN_POINT ( 'NONE',  ( -16.57702445344840569, 1524.523992613103246, 237.5566323917545901 ) ) ;
#28211 = CARTESIAN_POINT ( 'NONE',  ( 29.63060655169999791, 1444.770721089869994, 238.0637411752979915 ) ) ;
#28212 = CARTESIAN_POINT ( 'NONE',  ( 30.31118248176371210, 1526.186458717542109, 216.6939452248806504 ) ) ;
#28213 = CARTESIAN_POINT ( 'NONE',  ( -14.85774914289999948, 1415.975901282089808, 204.9891733264790048 ) ) ;
#28214 = CARTESIAN_POINT ( 'NONE',  ( -1.437936433978639794, 1507.910105588649913, 237.3166670950480182 ) ) ;
#28215 = CARTESIAN_POINT ( 'NONE',  ( -19.36515920259999746, 1456.378690096930086, 228.5344338431980304 ) ) ;
#28216 = AXIS2_PLACEMENT_3D ( 'NONE', #95311, #53325, #37607 ) ;
#28217 = ADVANCED_FACE ( 'NONE', ( #104738 ), #2732, .F. ) ;
#28219 = CARTESIAN_POINT ( 'NONE',  ( 2.500000000000000000, 1420.168334228329968, 149.0935893383980044 ) ) ;
#28218 = CARTESIAN_POINT ( 'NONE',  ( -22.75994491043178058, 1411.068131679461885, 204.0207675248701094 ) ) ;
#28220 = CARTESIAN_POINT ( 'NONE',  ( -0.3670406238980000180, 1434.822844257019824, 190.2779712162979990 ) ) ;
#28221 = CARTESIAN_POINT ( 'NONE',  ( -105.6660805195130024, 1379.161325318640138, 306.4514821997539684 ) ) ;
#28222 = ORIENTED_EDGE ( 'NONE', *, *, #64413, .T. ) ;
#28223 = CARTESIAN_POINT ( 'NONE',  ( 1.121950743945000051, 1517.123342927159911, 204.1084165760470057 ) ) ;
#28224 = CARTESIAN_POINT ( 'NONE',  ( 2.776335336629999873, 1405.836660839130218, 268.4805445416980092 ) ) ;
#28225 = EDGE_CURVE ( 'NONE', #78889, #60804, #81331, .T. ) ;
#28226 = CARTESIAN_POINT ( 'NONE',  ( -1.125259334100000119, 1515.531689041389882, 213.2129490267590199 ) ) ;
#28227 = AXIS2_PLACEMENT_3D ( 'NONE', #96015, #103288, #42303 ) ;
#28228 = STYLED_ITEM ( 'NONE', ( #87654 ), #46097 ) ;
#28229 = CARTESIAN_POINT ( 'NONE',  ( 19.03738911459980088, 1469.388104986470125, 270.0854773280680092 ) ) ;
#28230 = CARTESIAN_POINT ( 'NONE',  ( 2.478279119729999813, 1438.995264557609971, 157.7427228779980055 ) ) ;
#28231 = CARTESIAN_POINT ( 'NONE',  ( 3.544347521480000207, 1468.165829367189872, 218.4679976267089785 ) ) ;
#28232 = CARTESIAN_POINT ( 'NONE',  ( -40.72444163363370251, 1440.913060406799787, 260.2869945447760074 ) ) ;
#28233 = EDGE_CURVE ( 'NONE', #65239, #73345, #93868, .T. ) ;
#28234 = CARTESIAN_POINT ( 'NONE',  ( -26.34572671679999800, 1447.163110651519901, 137.4477041290980139 ) ) ;
#28235 = CARTESIAN_POINT ( 'NONE',  ( 2.382666182145900091, 1449.574453021285308, 154.4426451947454382 ) ) ;
#28236 = CARTESIAN_POINT ( 'NONE',  ( -1.397191924980000000, 1429.761471156189828, 199.8249656450389864 ) ) ;
#28237 = CARTESIAN_POINT ( 'NONE',  ( 1.172951571615530098, 1450.815013399510008, 154.5169618134089831 ) ) ;
#28238 = CARTESIAN_POINT ( 'NONE',  ( 2.495851582740000296, 1506.888954652989923, 220.6874564687990130 ) ) ;
#28239 = CARTESIAN_POINT ( 'NONE',  ( 12.26979804483799974, 1416.828039243390094, 223.5793509210460002 ) ) ;
#28240 = ORIENTED_EDGE ( 'NONE', *, *, #61786, .F. ) ;
#28241 = CARTESIAN_POINT ( 'NONE',  ( -42.15865170690000241, 1431.016965136909903, 271.1218459616979999 ) ) ;
#28242 = CARTESIAN_POINT ( 'NONE',  ( -1.266763281143285402, 1450.741562714445536, 181.7950901315468570 ) ) ;
#28243 = CARTESIAN_POINT ( 'NONE',  ( 4.342298062439800432, 1465.915122575709802, 200.0011775771919815 ) ) ;
#28244 = CARTESIAN_POINT ( 'NONE',  ( -0.8878292600469999130, 1475.977008401730018, 267.2346354036980074 ) ) ;
#28245 = AXIS2_PLACEMENT_3D ( 'NONE', #4447, #45905, #46463 ) ;
#28246 = CARTESIAN_POINT ( 'NONE',  ( -28.24318413590000176, 1508.132100804830088, 209.6063173613950141 ) ) ;
#28247 = CARTESIAN_POINT ( 'NONE',  ( -3.513170386600249273, 1448.288673971990193, 184.8796385662358546 ) ) ;
#28248 = CARTESIAN_POINT ( 'NONE',  ( -18.63960087727699744, 1384.866464396289757, 220.4278299832249957 ) ) ;
#28249 = CARTESIAN_POINT ( 'NONE',  ( -17.33645360970000127, 1414.996444518330009, 207.8511176870179895 ) ) ;
#28250 = CARTESIAN_POINT ( 'NONE',  ( -6.232532106187401055, 1407.162969929529936, 197.7132727037109987 ) ) ;
#28251 = CARTESIAN_POINT ( 'NONE',  ( 26.43520611626190231, 1435.427582101930057, 135.4748900071289768 ) ) ;
#28252 = ADVANCED_FACE ( 'NONE', ( #91239 ), #96589, .T. ) ;
#28253 = CARTESIAN_POINT ( 'NONE',  ( -11.03746375029680138, 1396.298497114720021, 210.0060340494559910 ) ) ;
#28254 = CARTESIAN_POINT ( 'NONE',  ( -15.49281168989999813, 1421.632443114230000, 227.2929369300979943 ) ) ;
#28255 = CARTESIAN_POINT ( 'NONE',  ( -17.21806449221460156, 1410.146609974180137, 225.6635716917170100 ) ) ;
#28256 = FACE_OUTER_BOUND ( 'NONE', #57255, .T. ) ;
#28257 = VERTEX_POINT ( 'NONE', #5024 ) ;
#28258 = CARTESIAN_POINT ( 'NONE',  ( -11.33647332202903080, 1502.116505749242378, 207.3325129751629845 ) ) ;
#28259 = CARTESIAN_POINT ( 'NONE',  ( 1.724138604399999997, 1408.973268634130136, 230.9767750068980092 ) ) ;
#28260 = CARTESIAN_POINT ( 'NONE',  ( -15.45533207179999913, 1484.705735421829786, 187.3543539206980029 ) ) ;
#28262 = CARTESIAN_POINT ( 'NONE',  ( -9.913260568299229192, 1438.794448387919829, 209.9868099401009829 ) ) ;
#28261 = CARTESIAN_POINT ( 'NONE',  ( 11.30045313650000161, 1426.459762359429988, 112.6498394735979929 ) ) ;
#28263 = CARTESIAN_POINT ( 'NONE',  ( -29.86461515634926656, 1525.960063244517187, 197.2746849027940925 ) ) ;
#28264 = CARTESIAN_POINT ( 'NONE',  ( -12.53380498098199602, 1442.773887284840612, 151.6125157144320212 ) ) ;
#28265 = ADVANCED_FACE ( 'NONE', ( #49258 ), #7972, .T. ) ;
#28266 = VECTOR ( 'NONE', #3505, 1000.000000000000000 ) ;
#28267 = CARTESIAN_POINT ( 'NONE',  ( 1.126138108584999964, 1517.208444099459939, 201.3951612445669923 ) ) ;
#28268 = CARTESIAN_POINT ( 'NONE',  ( 7.595196814659999518, 1425.935899813689957, 212.0840209023990042 ) ) ;
#28269 = CARTESIAN_POINT ( 'NONE',  ( -3.071476887830000280, 1470.850261538789937, 187.3986309372990036 ) ) ;
#28271 = CARTESIAN_POINT ( 'NONE',  ( 1.447786046720000108, 1507.396806431330106, 181.1008358460979935 ) ) ;
#28270 = B_SPLINE_CURVE_WITH_KNOTS ( 'NONE', 3,
 ( #8518, #100389, #102568, #15794, #75750, #83040, #33175, #109358, #42143, #67366, #42696, #76293, #32084, #6333, #74656, #76851, #84130, #6872, #40482, #49454, #108792, #66272, #59507, #16354, #109895, #41029, #48913, #50552, #84676, #101465, #24752, #23674, #57857, #161 ),
 .UNSPECIFIED., .F., .F.,
 ( 4, 2, 1, 1, 2, 2, 2, 2, 1, 1, 1, 2, 2, 2, 2, 1, 1, 1, 2, 2, 4 ),
 ( 0.000000000000000000, 0.1250000000007119583, 0.1875000000010639267, 0.2187500000012362611, 0.2343750000012936319, 0.2500000000013509749, 0.3750000000019591551, 0.4375000000022347679, 0.4687500000023421265, 0.4843750000024272806, 0.4921875000024374947, 0.4960937500024130697, 0.5000000000023886448, 0.6250000000012784218, 0.6875000000007230883, 0.7187500000004477529, 0.7343750000003123057, 0.7421875000002446932, 0.7460937500002088330, 0.7500000000001729727, 1.000000000000000000 ),
 .UNSPECIFIED. ) ;
#28272 = CARTESIAN_POINT ( 'NONE',  ( 7.589847736954999924, 1511.982868782460173, 206.7094295734470109 ) ) ;
#28273 = CARTESIAN_POINT ( 'NONE',  ( -83.24330069484520322, 1379.154961504219955, 299.6759861110299994 ) ) ;
#28274 = CARTESIAN_POINT ( 'NONE',  ( 9.369782510150898247, 1366.497526915296021, 210.6218459616987957 ) ) ;
#28275 = ADVANCED_FACE ( 'NONE', ( #25117 ), #101823, .T. ) ;
#28277 = ORIENTED_EDGE ( 'NONE', *, *, #57993, .F. ) ;
#28276 = CARTESIAN_POINT ( 'NONE',  ( -14.05757238939644260, 1460.648840875784572, 232.1449228860425080 ) ) ;
#28278 = EDGE_LOOP ( 'NONE', ( #106200, #40823, #32717, #24992 ) ) ;
#28279 = CARTESIAN_POINT ( 'NONE',  ( -41.66021910349999757, 1443.875694946319754, 135.6929188412979954 ) ) ;
#28280 = CARTESIAN_POINT ( 'NONE',  ( 0.4380014478882280349, 1474.776185545679937, 235.9802319278450113 ) ) ;
#28281 = CARTESIAN_POINT ( 'NONE',  ( 9.668109322589998555, 1408.913060387329779, 224.6723891271980165 ) ) ;
#28282 = CARTESIAN_POINT ( 'NONE',  ( 1.968601690575629615, 1498.935401749600032, 197.9561509338619771 ) ) ;
#28284 = CARTESIAN_POINT ( 'NONE',  ( -2.056387895720000358, 1486.516979218729830, 181.7077744939979880 ) ) ;
#28283 = CARTESIAN_POINT ( 'NONE',  ( -8.630315558130000397, 1384.315009893769911, 218.6220459152689841 ) ) ;
#28285 = DIRECTION ( 'NONE',  ( -0.5877852522924785772, 0.000000000000000000, 0.8090169943749434545 ) ) ;
#28286 = CARTESIAN_POINT ( 'NONE',  ( -2.989231773490640176, 1464.638009085429985, 198.9533349682120047 ) ) ;
#28287 = CARTESIAN_POINT ( 'NONE',  ( 12.55840807187700037, 1425.933963207659872, 223.8625469537460049 ) ) ;
#28288 = DIRECTION ( 'NONE',  ( 0.7414773880254630356, 0.000000000000000000, -0.6709778558543769700 ) ) ;
#28289 = CARTESIAN_POINT ( 'NONE',  ( 6.235478689385840489, 1396.130808101319872, 218.2352667451380057 ) ) ;
#28290 = CARTESIAN_POINT ( 'NONE',  ( -0.06979926259237639874, 1408.910622943330054, 194.1218459608980140 ) ) ;
#28291 = CARTESIAN_POINT ( 'NONE',  ( 5.574750653145040338E-05, 1406.066344387250183, 269.0457483805509469 ) ) ;
#28292 = CARTESIAN_POINT ( 'NONE',  ( 41.66146276220000289, 1443.809306595659791, 136.1342541931979895 ) ) ;
#28293 = ORIENTED_EDGE ( 'NONE', *, *, #47350, .F. ) ;
#28294 = CARTESIAN_POINT ( 'NONE',  ( -11.86593337649999924, 1432.333319972560048, 150.3971781300980126 ) ) ;
#28295 = CARTESIAN_POINT ( 'NONE',  ( 12.67807438250000018, 1442.703181404250017, 187.4495022272980123 ) ) ;
#28296 = ORIENTED_EDGE ( 'NONE', *, *, #48004, .F. ) ;
#28297 = EDGE_CURVE ( 'NONE', #96166, #6510, #13372, .T. ) ;
#28298 = VECTOR ( 'NONE', #20068, 1000.000000000000114 ) ;
#28299 = EDGE_LOOP ( 'NONE', ( #87133, #23820, #42296, #25585 ) ) ;
#28300 = DIRECTION ( 'NONE',  ( 0.000000000000000000, 0.000000000000000000, -1.000000000000000000 ) ) ;
#28301 = CARTESIAN_POINT ( 'NONE',  ( 9.984115569220000097, 1365.258395869459946, 207.6218459616989946 ) ) ;
#28302 = AXIS2_PLACEMENT_3D ( 'NONE', #30037, #22716, #56917 ) ;
#28303 = EDGE_CURVE ( 'NONE', #17819, #38227, #106482, .T. ) ;
#28304 = CARTESIAN_POINT ( 'NONE',  ( -7.713117841115000317, 1516.690345681169902, 214.1262880092169780 ) ) ;
#28305 = CARTESIAN_POINT ( 'NONE',  ( 2.711770194995000161, 1512.058324472099912, 216.8053402088569896 ) ) ;
#28306 = B_SPLINE_SURFACE_WITH_KNOTS ( 'NONE', 5, 5, ( 
 ( #51083, #8499, #42125, #142, #15774, #76273 ),
 ( #34816, #59490, #109339, #9065, #49976, #92507 ),
 ( #51629, #50534, #84658, #33701, #102549, #102003 ),
 ( #25289, #69003, #93600, #16878, #103107, #42671 ),
 ( #76828, #34264, #68446, #83556, #60043, #94721 ),
 ( #94162, #6849, #84112, #43235, #77383, #41577 ) ),
 .UNSPECIFIED., .F., .F., .F.,
 ( 6, 6 ),
 ( 6, 6 ),
 ( 29.50720980459999865, 158.0245753780000086 ),
 ( -5.551115123129999410E-17, 1.000000000000000000 ),
 .UNSPECIFIED. ) ;
#28307 = TOROIDAL_SURFACE ( 'NONE', #89123, 1.000000000000000000, 1.000000000000000000 ) ;
#28308 = ORIENTED_EDGE ( 'NONE', *, *, #54960, .F. ) ;
#28309 = CARTESIAN_POINT ( 'NONE',  ( 8.220300753029999186, 1427.204169894219831, 212.0038158565590152 ) ) ;
#28310 = CARTESIAN_POINT ( 'NONE',  ( -101.7780519309999931, 1374.485289779690220, 304.0160546798589962 ) ) ;
#28311 = AXIS2_PLACEMENT_3D ( 'NONE', #89211, #13028, #61839 ) ;
#28312 = VECTOR ( 'NONE', #104159, 1000.000000000000000 ) ;
#28313 = CARTESIAN_POINT ( 'NONE',  ( -106.0964083643799967, 1378.913060387289988, 302.6612236841029926 ) ) ;
#28314 = CARTESIAN_POINT ( 'NONE',  ( 2.479246847704999812, 1516.983612918759945, 205.0778556245070092 ) ) ;
#28315 = CARTESIAN_POINT ( 'NONE',  ( 11.86100282799569960, 1492.894947744830006, 212.5846961511890072 ) ) ;
#28316 = CARTESIAN_POINT ( 'NONE',  ( -98.86909676750001097, 1384.870948519250078, 296.2469157437590184 ) ) ;
#28317 = CARTESIAN_POINT ( 'NONE',  ( 9.600314864117150293, 1462.464356163139882, 207.4456482718869950 ) ) ;
#28318 = CARTESIAN_POINT ( 'NONE',  ( -8.286009866380000588, 1409.704129222430083, 230.3000291798979902 ) ) ;
#28320 = ORIENTED_EDGE ( 'NONE', *, *, #69240, .T. ) ;
#28319 = CARTESIAN_POINT ( 'NONE',  ( -11.96787629350000159, 1446.201514831819850, 187.3303138752980033 ) ) ;
#28321 = CARTESIAN_POINT ( 'NONE',  ( 8.907440304832482170, 1432.353341358199941, 149.1004941873906660 ) ) ;
#28322 = CARTESIAN_POINT ( 'NONE',  ( 11.44665326297827335, 1425.798162341591706, 139.1345266541928538 ) ) ;
#28323 = CARTESIAN_POINT ( 'NONE',  ( -3.078458293560000225, 1384.906579013939790, 218.5736861911289850 ) ) ;
#28324 = CARTESIAN_POINT ( 'NONE',  ( -25.72910798539999888, 1436.492646657430214, 137.0497317554980157 ) ) ;
#28325 = AXIS2_PLACEMENT_3D ( 'NONE', #86518, #43977, #78677 ) ;
#28326 = CARTESIAN_POINT ( 'NONE',  ( 42.44869904479999434, 1432.149879290850095, 270.3370793111479884 ) ) ;
#28327 = CARTESIAN_POINT ( 'NONE',  ( -6.546302780145000000, 1516.577434278289957, 211.6089493897669911 ) ) ;
#28328 = CARTESIAN_POINT ( 'NONE',  ( -67.87070494639999652, 1379.748617063760094, 278.3152404517590526 ) ) ;
#28329 = CARTESIAN_POINT ( 'NONE',  ( 5.511665417999469900E-05, 1508.970066526555001, 238.8757070596369942 ) ) ;
#28330 = CARTESIAN_POINT ( 'NONE',  ( -30.30264253605756508, 1524.678541297860875, 221.8072158554251416 ) ) ;
#28331 = CARTESIAN_POINT ( 'NONE',  ( -13.90061681514290015, 1502.276395855860073, 227.4029517098429949 ) ) ;
#28332 = CARTESIAN_POINT ( 'NONE',  ( -0.7402208985179988820, 1516.992029636990083, 209.8751463226419958 ) ) ;
#28333 = ORIENTED_EDGE ( 'NONE', *, *, #43903, .F. ) ;
#28334 = DIRECTION ( 'NONE',  ( -0.03339394388798658936, -0.9993515141380058253, 0.01346832215537827580 ) ) ;
#28335 = CARTESIAN_POINT ( 'NONE',  ( -11.66816036250000010, 1420.438647421430005, 229.1834824673979938 ) ) ;
#28336 = CARTESIAN_POINT ( 'NONE',  ( -19.17614523219999967, 1385.141607863239869, 220.5180809881589994 ) ) ;
#28337 = ORIENTED_EDGE ( 'NONE', *, *, #99058, .F. ) ;
#28338 = CARTESIAN_POINT ( 'NONE',  ( -34.66742137116909817, 1385.210832685530022, 233.7091802904559756 ) ) ;
#28339 = CARTESIAN_POINT ( 'NONE',  ( -2.875332210020000279, 1429.155786104789968, 200.6010274126990112 ) ) ;
#28340 = CARTESIAN_POINT ( 'NONE',  ( 16.08217969103819911, 1469.006061218260129, 229.7393514651440114 ) ) ;
#28341 = CARTESIAN_POINT ( 'NONE',  ( 16.73628186595824019, 1526.382868172863937, 184.0591879540915272 ) ) ;
#28342 = CARTESIAN_POINT ( 'NONE',  ( -5.311724842150000292, 1500.891271500089942, 229.7588813323989996 ) ) ;
#28343 = CARTESIAN_POINT ( 'NONE',  ( -0.02529539845109999782, 1409.857530525830043, 233.2156916876980119 ) ) ;
#28344 = CARTESIAN_POINT ( 'NONE',  ( -17.84338787571901364, 1512.187213306747481, 237.8836641337663309 ) ) ;
#28345 = EDGE_CURVE ( 'NONE', #67449, #87841, #27710, .T. ) ;
#28347 = CARTESIAN_POINT ( 'NONE',  ( -7.708815826551380646, 1516.526058373149908, 211.4663580544020078 ) ) ;
#28346 = CARTESIAN_POINT ( 'NONE',  ( -4.032397940005000514, 1516.981965530290154, 214.9074288837770155 ) ) ;
#28348 = CARTESIAN_POINT ( 'NONE',  ( 5.923682464646780943, 1517.151704408390060, 194.3813127491490036 ) ) ;
#28349 = CARTESIAN_POINT ( 'NONE',  ( 10.36759898501759913, 1469.933492258360047, 207.4161449764170015 ) ) ;
#28350 = ORIENTED_EDGE ( 'NONE', *, *, #7058, .F. ) ;
#28351 = CARTESIAN_POINT ( 'NONE',  ( -12.58433072603950009, 1415.426207913209964, 196.9819739087400023 ) ) ;
#28352 = CARTESIAN_POINT ( 'NONE',  ( -16.67342217799999915, 1504.313428625830056, 185.6524960304979857 ) ) ;
#28353 = ORIENTED_EDGE ( 'NONE', *, *, #95927, .F. ) ;
#28354 = CARTESIAN_POINT ( 'NONE',  ( 4.234467186019998941, 1420.712403710529998, 185.6414431274980075 ) ) ;
#28355 = PLANE ( 'NONE',  #72626 ) ;
#28356 = DIRECTION ( 'NONE',  ( -0.7414773880254614813, 0.000000000000000000, 0.6709778558543786353 ) ) ;
#28357 = CARTESIAN_POINT ( 'NONE',  ( 3.090732370630000059, 1442.657375189589857, 217.4492349673389811 ) ) ;
#28358 = CARTESIAN_POINT ( 'NONE',  ( -30.29107669316903539, 1523.847248782568613, 195.7510835661477984 ) ) ;
#28359 = CARTESIAN_POINT ( 'NONE',  ( -1847.405368200898920, -8387.357407334300660, -1167.591558398288043 ) ) ;
#28360 = EDGE_CURVE ( 'NONE', #49801, #47452, #20986, .T. ) ;
#28361 = CARTESIAN_POINT ( 'NONE',  ( 17.92792478850000037, 1415.296882282229944, 210.0737307021219920 ) ) ;
#28362 = CARTESIAN_POINT ( 'NONE',  ( -17.49524353049999803, 1436.343070723249866, 147.8329090225980167 ) ) ;
#28363 = CARTESIAN_POINT ( 'NONE',  ( 33.91369968912619726, 1451.728767897860052, 134.7155302171979940 ) ) ;
#28364 = LINE ( 'NONE', #20487, #37416 ) ;
#28366 = CARTESIAN_POINT ( 'NONE',  ( -5.152852264748282174, 1391.896122684712282, 203.6724224095950149 ) ) ;
#28365 = CARTESIAN_POINT ( 'NONE',  ( 0.6531460927897710933, 1409.103080214060128, 232.5176971054530100 ) ) ;
#28367 = CARTESIAN_POINT ( 'NONE',  ( 2.180465155517623099, 1524.667648926078527, 244.2585483383492999 ) ) ;
#28368 = ORIENTED_EDGE ( 'NONE', *, *, #84370, .F. ) ;
#28369 = FACE_OUTER_BOUND ( 'NONE', #103505, .T. ) ;
#28370 = CARTESIAN_POINT ( 'NONE',  ( 25.51721860929999863, 1469.158424523229769, 207.1962240684080143 ) ) ;
#28371 = CARTESIAN_POINT ( 'NONE',  ( -23.86337105550000004, 1436.937184565879988, 212.0334657536579925 ) ) ;
#28372 = LINE ( 'NONE', #28934, #50937 ) ;
#28373 = COLOUR_RGB ( '', 0.08235294, 0.09019608, 0.10196078) ;
#28374 = CARTESIAN_POINT ( 'NONE',  ( -18.55970593940000057, 1508.848287783829846, 229.9905654330979985 ) ) ;
#28375 = CARTESIAN_POINT ( 'NONE',  ( -2.880413542612040079, 1425.982839100257934, 185.3253768740765963 ) ) ;
#28376 = CARTESIAN_POINT ( 'NONE',  ( 11.86890500783672842, 1435.287397482030201, 151.2475232226828439 ) ) ;
#28377 = LINE ( 'NONE', #64770, #96741 ) ;
#28378 = CARTESIAN_POINT ( 'NONE',  ( -14.31460220670079941, 1509.452787612570091, 183.0438844114540018 ) ) ;
#28379 = AXIS2_PLACEMENT_3D ( 'NONE', #36959, #103620, #70602 ) ;
#28380 = CARTESIAN_POINT ( 'NONE',  ( -9.202353901899998689, 1488.302798292690113, 217.0664071269289934 ) ) ;
#28381 = CARTESIAN_POINT ( 'NONE',  ( -13.67845557849999949, 1504.250295190390034, 227.6838176112990197 ) ) ;
#28382 = CARTESIAN_POINT ( 'NONE',  ( -86.11627744455289246, 1383.772810929480102, 307.0143598361519821 ) ) ;
#28383 = CIRCLE ( 'NONE', #42694, 1.000000000000015099 ) ;
#28384 = CARTESIAN_POINT ( 'NONE',  ( -109.1783411524900060, 1383.732934801179908, 311.1044898606749598 ) ) ;
#28385 = CARTESIAN_POINT ( 'NONE',  ( 15.55634916703500004, 1516.551704408390151, 224.6781951372670108 ) ) ;
#28386 = CARTESIAN_POINT ( 'NONE',  ( 6.406055020080000162, 1428.231850363690000, 214.6517644217489931 ) ) ;
#28388 = ORIENTED_EDGE ( 'NONE', *, *, #64583, .T. ) ;
#28387 = CARTESIAN_POINT ( 'NONE',  ( -18.83642247210000065, 1444.248298674089938, 209.1218459616989946 ) ) ;
#28389 = CARTESIAN_POINT ( 'NONE',  ( 17.12480624395889706, 1507.616838180409786, 193.8046521743370079 ) ) ;
#28390 = CARTESIAN_POINT ( 'NONE',  ( -74.01743362070000387, 1382.335636213369980, 298.4777005571589825 ) ) ;
#28391 = EDGE_CURVE ( 'NONE', #20574, #73846, #104599, .T. ) ;
#28392 = CARTESIAN_POINT ( 'NONE',  ( -11.74015320060000001, 1428.979986575930070, 144.1938086916980239 ) ) ;
#28393 = VERTEX_POINT ( 'NONE', #58747 ) ;
#28394 = VERTEX_POINT ( 'NONE', #8874 ) ;
#28395 = CARTESIAN_POINT ( 'NONE',  ( 13.74650104269999851, 1441.983649238280123, 189.3366583681979876 ) ) ;
#28396 = CARTESIAN_POINT ( 'NONE',  ( -109.5349821800000001, 1384.927863536390078, 297.1230985535589753 ) ) ;
#28397 = CARTESIAN_POINT ( 'NONE',  ( 12.83564499065948716, 1442.860052983879996, 169.4451046929141853 ) ) ;
#28399 = CARTESIAN_POINT ( 'NONE',  ( -5.805165725770000229, 1470.400760091029952, 255.2684105097979739 ) ) ;
#28398 = CARTESIAN_POINT ( 'NONE',  ( 27.06247215711447396, 1417.591791844086856, 269.4421024428557985 ) ) ;
#28400 = EDGE_CURVE ( 'NONE', #85568, #8717, #66565, .T. ) ;
#28401 = CARTESIAN_POINT ( 'NONE',  ( -19.39983987835443457, 1501.977400791986611, 178.9515629539737631 ) ) ;
#28402 = CARTESIAN_POINT ( 'NONE',  ( -11.88717770409999908, 1433.553338367350079, 150.4897835633980208 ) ) ;
#28403 = EDGE_CURVE ( 'NONE', #104141, #28836, #8042, .T. ) ;
#28404 = CARTESIAN_POINT ( 'NONE',  ( -4.137865169369999485, 1481.950712913389907, 229.2071242064990315 ) ) ;
#28405 = CARTESIAN_POINT ( 'NONE',  ( -19.14160362779999858, 1485.709425685830183, 189.6559982148980055 ) ) ;
#28406 = AXIS2_PLACEMENT_3D ( 'NONE', #25528, #26642, #67026 ) ;
#28407 = CARTESIAN_POINT ( 'NONE',  ( 11.34224779750000067, 1409.809526181430101, 189.6148948717980147 ) ) ;
#28408 = DIRECTION ( 'NONE',  ( 5.980589973904019347E-17, -1.000000000000000000, 1.736889445713099699E-16 ) ) ;
#28409 = CARTESIAN_POINT ( 'NONE',  ( -1.548360550261279833, 1515.071586600709907, 213.4511168375470049 ) ) ;
#28410 = CARTESIAN_POINT ( 'NONE',  ( 11.83477883539999986, 1434.684743758880131, 151.1661215832980076 ) ) ;
#28411 = CARTESIAN_POINT ( 'NONE',  ( -9.197351350889000798, 1424.498960654269922, 204.7249030865850159 ) ) ;
#28412 = ADVANCED_FACE ( 'NONE', ( #102928 ), #74328, .T. ) ;
#28413 = CARTESIAN_POINT ( 'NONE',  ( -20.19751881499999868, 1450.975641626430161, 145.7773103342979937 ) ) ;
#28415 = ORIENTED_EDGE ( 'NONE', *, *, #41949, .T. ) ;
#28414 = CARTESIAN_POINT ( 'NONE',  ( 0.000000000000000000, 1512.187213306747481, 209.1218459616979999 ) ) ;
#28416 = ORIENTED_EDGE ( 'NONE', *, *, #92741, .T. ) ;
#28417 = DIRECTION ( 'NONE',  ( -0.6736849260863841948, 0.000000000000000000, 0.7390186874254148774 ) ) ;
#28418 = CARTESIAN_POINT ( 'NONE',  ( -22.16283322808959966, 1485.376191718830114, 217.1686774328890124 ) ) ;
#28419 = CARTESIAN_POINT ( 'NONE',  ( -13.03174027510000066, 1470.346600428830243, 269.8790079804980451 ) ) ;
#28420 = DIRECTION ( 'NONE',  ( 0.000000000000000000, -1.000000000000000000, 6.123233995736769734E-17 ) ) ;
#28421 = CARTESIAN_POINT ( 'NONE',  ( 16.87240840930000019, 1409.502257872129803, 222.1138758984979802 ) ) ;
#28422 = CARTESIAN_POINT ( 'NONE',  ( -14.84750872589999915, 1485.048555357530176, 224.0947347056979879 ) ) ;
#28423 = CARTESIAN_POINT ( 'NONE',  ( 15.28420222199999934, 1497.713060387329961, 193.8376437393980325 ) ) ;
#28424 = CARTESIAN_POINT ( 'NONE',  ( -4.363122647530000009, 1421.075575420230052, 170.1076616725979989 ) ) ;
#28425 = CARTESIAN_POINT ( 'NONE',  ( -9.941476430729998981, 1461.322233694490023, 211.0754656104689957 ) ) ;
#28426 = CARTESIAN_POINT ( 'NONE',  ( 9.570655340201339456, 1361.000351557653630, 208.3718459617010978 ) ) ;
#28427 = CARTESIAN_POINT ( 'NONE',  ( -45.35503536899049948, 1436.791125258660031, 266.1974304159290341 ) ) ;
#28428 = ORIENTED_EDGE ( 'NONE', *, *, #61063, .F. ) ;
#28429 = CARTESIAN_POINT ( 'NONE',  ( -8.101682389679998764, 1423.901782527849946, 210.4428033686490096 ) ) ;
#28430 = ORIENTED_EDGE ( 'NONE', *, *, #89948, .T. ) ;
#28431 = CARTESIAN_POINT ( 'NONE',  ( -1.119592219845000125, 1516.958737650239982, 210.2577447559170025 ) ) ;
#28432 = DIRECTION ( 'NONE',  ( -0.6736849260863840838, 0.000000000000000000, 0.7390186874254150995 ) ) ;
#28433 = EDGE_CURVE ( 'NONE', #47384, #104047, #35673, .T. ) ;
#28434 = PLANE ( 'NONE',  #85510 ) ;
#28435 = CARTESIAN_POINT ( 'NONE',  ( 7.091651353261220869, 1426.649169667290153, 213.2026143799430145 ) ) ;
#28436 = AXIS2_PLACEMENT_3D ( 'NONE', #9734, #59599, #109996 ) ;
#28437 = CARTESIAN_POINT ( 'NONE',  ( -27.03140942220920095, 1451.490713798300249, 136.0731937540990089 ) ) ;
#28438 = B_SPLINE_SURFACE_WITH_KNOTS ( 'NONE', 5, 5, ( 
 ( #102538, #101429, #25829, #24720, #95269, #60587 ),
 ( #77915, #26963, #18531, #103665, #10153, #1222 ),
 ( #69544, #75719, #33142, #58917, #93048, #50522 ),
 ( #62243, #54931, #36454, #2341, #78470, #96928 ),
 ( #28053, #3432, #20195, #89060, #12345, #35920 ),
 ( #37563, #70652, #29703, #104769, #28612, #79582 ),
 ( #11276, #37005, #53284, #54394, #96369, #27504 ),
 ( #45981, #61691, #97467, #72286, #87423, #98002 ),
 ( #19648, #87988, #2887, #53851, #45439, #70103 ),
 ( #88526, #10719, #71197, #20736, #63349, #71763 ),
 ( #11811, #46536, #80670, #104216, #80113, #105880 ),
 ( #3984, #105319, #62812, #29161, #38108, #106418 ) ),
 .UNSPECIFIED., .F., .F., .F.,
 ( 6, 3, 3, 6 ),
 ( 6, 6 ),
 ( 6.066676742310000314, 9.538385084389998880, 13.68355489660000046, 19.24621227249999933 ),
 ( 0.000000000000000000, 0.5000000000000000000 ),
 .UNSPECIFIED. ) ;
#28439 = ORIENTED_EDGE ( 'NONE', *, *, #17844, .T. ) ;
#28440 = DIRECTION ( 'NONE',  ( -0.5202960232132588514, 0.000000000000000000, -0.8539859765994216589 ) ) ;
#28441 = EDGE_CURVE ( 'NONE', #11785, #15037, #4928, .T. ) ;
#28442 = CARTESIAN_POINT ( 'NONE',  ( 2.872836622524999939, 1517.158319634930194, 201.3964737998670103 ) ) ;
#28443 = AXIS2_PLACEMENT_3D ( 'NONE', #63963, #90780, #57215 ) ;
#28444 = CIRCLE ( 'NONE', #37397, 9.500000000000008882 ) ;
#28445 = CARTESIAN_POINT ( 'NONE',  ( 9.079459637170000263, 1470.934168148190111, 213.6782594943889819 ) ) ;
#28446 = CARTESIAN_POINT ( 'NONE',  ( -8.178798132767068907, 1438.657504337420050, 206.1307692081600180 ) ) ;
#28447 = ORIENTED_EDGE ( 'NONE', *, *, #61317, .T. ) ;
#28448 = CARTESIAN_POINT ( 'NONE',  ( -9.682670043730421838, 1409.984507541440053, 270.3686428832239699 ) ) ;
#28449 = CARTESIAN_POINT ( 'NONE',  ( 2.480427254505000345, 1516.872851364150165, 208.3639601402670110 ) ) ;
#28450 = CARTESIAN_POINT ( 'NONE',  ( -0.7484295816749999553, 1428.043997280830126, 101.8807690336980016 ) ) ;
#28451 = CARTESIAN_POINT ( 'NONE',  ( 8.537244690487868937, 1435.714930654649834, 207.3103916605290067 ) ) ;
#28453 = ORIENTED_EDGE ( 'NONE', *, *, #18575, .F. ) ;
#28452 = CARTESIAN_POINT ( 'NONE',  ( -8.158278992428673604, 1366.026982084109250, 210.6218459617142003 ) ) ;
#28454 = ORIENTED_EDGE ( 'NONE', *, *, #15810, .F. ) ;
#28455 = CARTESIAN_POINT ( 'NONE',  ( 45.63029764463163929, 1441.507770731200935, 268.9749386593517784 ) ) ;
#28456 = CARTESIAN_POINT ( 'NONE',  ( 11.39540147253980074, 1471.141865352140258, 209.7217653457960012 ) ) ;
#28457 = CARTESIAN_POINT ( 'NONE',  ( -10.74904557270209082, 1438.632470347905837, 152.4698233941169008 ) ) ;
#28458 = CARTESIAN_POINT ( 'NONE',  ( 15.45719918680149974, 1473.646226760320360, 195.7768488996430847 ) ) ;
#28459 = CIRCLE ( 'NONE', #1700, 0.4999999999999976130 ) ;
#28460 = CARTESIAN_POINT ( 'NONE',  ( -18.28144489529720218, 1415.492117401540099, 207.5679474733179859 ) ) ;
#28461 = CARTESIAN_POINT ( 'NONE',  ( 9.247631459069999948, 1454.170661380389902, 214.4254682548290134 ) ) ;
#28462 = AXIS2_PLACEMENT_3D ( 'NONE', #8270, #59266, #102874 ) ;
#28463 = CARTESIAN_POINT ( 'NONE',  ( 10.61930341568279879, 1475.185691052500033, 269.0172316872100282 ) ) ;
#28464 = CARTESIAN_POINT ( 'NONE',  ( -1.565064790564475894, 1467.010193131020060, 235.3666753383823504 ) ) ;
#28465 = CARTESIAN_POINT ( 'NONE',  ( -17.64968521348830421, 1423.160730800522060, 226.3068084200317287 ) ) ;
#28466 =( BOUNDED_CURVE ( )  B_SPLINE_CURVE ( 3, ( #109563, #59177, #69229, #16023 ),
 .UNSPECIFIED., .F., .F. ) 
 B_SPLINE_CURVE_WITH_KNOTS ( ( 4, 4 ),
 ( 0.05347086468394689901, 0.09168413669265079724 ),
 .UNSPECIFIED. ) 
 CURVE ( )  GEOMETRIC_REPRESENTATION_ITEM ( )  RATIONAL_B_SPLINE_CURVE ( ( 1.000000000000000000, 0.9998783158554702677, 0.9998783158554702677, 1.000000000000000000 ) ) 
 REPRESENTATION_ITEM ( '' )  );
#28467 = CARTESIAN_POINT ( 'NONE',  ( -2.299014068865000038, 1516.811292230880099, 206.2578025137869986 ) ) ;
#28468 = ORIENTED_EDGE ( 'NONE', *, *, #41104, .F. ) ;
#28469 = CARTESIAN_POINT ( 'NONE',  ( 23.24354977585844040, 1411.085069985731025, 212.7460856263411415 ) ) ;
#28470 = CARTESIAN_POINT ( 'NONE',  ( 1.498256283064010042, 1466.857882684819970, 182.8697145444330090 ) ) ;
#28471 = ORIENTED_EDGE ( 'NONE', *, *, #82371, .T. ) ;
#28472 = CARTESIAN_POINT ( 'NONE',  ( 7.303366077162626091, 1456.574606934232634, 227.6099195461272870 ) ) ;
#28473 = CARTESIAN_POINT ( 'NONE',  ( 24.70673247591740207, 1451.987717812959772, 136.4510166997479814 ) ) ;
#28474 = B_SPLINE_CURVE_WITH_KNOTS ( 'NONE', 3,
 ( #67867, #75706, #94136, #100872, #85738, #43751, #24706, #103078, #9036, #52164, #33130, #34790, #17407, #101978, #86295, #68977, #24164, #76247, #93035, #77357, #16308, #33675, #25264, #50510, #115, #41550, #60574, #26379, #7386, #659, #51604, #58354, #25817, #110395, #94694, #9579, #109311, #32596, #92478, #59466, #15748, #84087, #109853, #67318, #93576, #16851, #53836, #11796, #71183 ),
 .UNSPECIFIED., .F., .F.,
 ( 4, 2, 1, 2, 2, 2, 1, 1, 2, 2, 2, 2, 1, 1, 1, 2, 2, 2, 2, 1, 1, 1, 2, 2, 2, 1, 1, 2, 2, 4 ),
 ( 0.000000000000000000, 0.06249999999985297872, 0.09374999999977946807, 0.1093749999998712974, 0.1249999999999631406, 0.1874999999995866362, 0.2187499999993044175, 0.2343749999991634470, 0.2421874999990958899, 0.2499999999990283328, 0.3749999999982073229, 0.4374999999977968179, 0.4687499999975917042, 0.4843749999974626963, 0.4921874999973949727, 0.4960937499973809839, 0.4999999999973669396, 0.6249999999980714316, 0.6874999999984235943, 0.7187499999985956789, 0.7343749999986817212, 0.7421874999987244648, 0.7460937499987384536, 0.7499999999987524424, 0.8124999999990795141, 0.8437499999992470467, 0.8593749999993267608, 0.8671874999993630651, 0.8749999999993993693, 1.000000000000000000 ),
 .UNSPECIFIED. ) ;
#28475 = CARTESIAN_POINT ( 'NONE',  ( -10.70847609427080016, 1506.854789404229905, 189.5201119528840081 ) ) ;
#28476 = CARTESIAN_POINT ( 'NONE',  ( -30.25680144860000098, 1389.598173243689871, 209.1456520601699935 ) ) ;
#28477 = CARTESIAN_POINT ( 'NONE',  ( -18.63535451612431970, 1508.532394786728901, 229.9190513451956690 ) ) ;
#28478 = CARTESIAN_POINT ( 'NONE',  ( 18.33529589289999961, 1410.049765793829692, 194.4554404145980016 ) ) ;
#28479 = CARTESIAN_POINT ( 'NONE',  ( 18.29245442332558014, 1445.052233488288721, 161.2175811807109937 ) ) ;
#28480 = CARTESIAN_POINT ( 'NONE',  ( 10.92857262880000135, 1460.888923995989899, 208.5047758091729690 ) ) ;
#28481 = CARTESIAN_POINT ( 'NONE',  ( -14.04578639380744853, 1379.586359795460567, 211.8392331697818634 ) ) ;
#28482 = CARTESIAN_POINT ( 'NONE',  ( 19.87695271833857902, 1456.362367750117528, 223.8442701291641015 ) ) ;
#28483 = AXIS2_PLACEMENT_3D ( 'NONE', #40215, #57595, #14991 ) ;
#28484 = CARTESIAN_POINT ( 'NONE',  ( 16.86071788331999954, 1430.053758721836402, 201.2513078365784622 ) ) ;
#28485 = CARTESIAN_POINT ( 'NONE',  ( 0.7543881828220019292, 1516.727502608469877, 215.6727161143369926 ) ) ;
#28486 = CARTESIAN_POINT ( 'NONE',  ( 26.50104796915090333, 1446.255561005059917, 137.5974644915019951 ) ) ;
#28487 = VERTEX_POINT ( 'NONE', #1067 ) ;
#28488 = CARTESIAN_POINT ( 'NONE',  ( -16.81730356679999971, 1417.162085555489966, 207.4277572267089909 ) ) ;
#28489 = DIRECTION ( 'NONE',  ( -0.7257730359255160080, 1.512900915589710975E-09, 0.6879342267422517976 ) ) ;
#28490 = DIRECTION ( 'NONE',  ( 1.000000000000000000, 0.000000000000000000, 0.000000000000000000 ) ) ;
#28491 = CARTESIAN_POINT ( 'NONE',  ( -11081.89558201059481, 2833.596074015790236, 8724.858692896474167 ) ) ;
#28492 = CARTESIAN_POINT ( 'NONE',  ( -39.50712975707070029, 1446.923889365939885, 136.6550386957819967 ) ) ;
#28493 = CARTESIAN_POINT ( 'NONE',  ( -10.61999372029469946, 1462.990852176999852, 206.0510140530389833 ) ) ;
#28494 = CARTESIAN_POINT ( 'NONE',  ( -27.19819525190000320, 1447.435760031770087, 248.0989693021979861 ) ) ;
#28495 = CARTESIAN_POINT ( 'NONE',  ( 45.23908986689997391, 1446.067266319080318, 266.2007832802979124 ) ) ;
#28496 = CARTESIAN_POINT ( 'NONE',  ( -12.31067562887320044, 1378.376168525579942, 209.7905782219929733 ) ) ;
#28497 = DIRECTION ( 'NONE',  ( 4.255490039221486549E-06, 0.03086473865808741363, -0.9995235704521724385 ) ) ;
#28498 = CARTESIAN_POINT ( 'NONE',  ( -9.743700617285488974, 1461.082141979609787, 210.4654820370750201 ) ) ;
#28499 = CARTESIAN_POINT ( 'NONE',  ( -23.19979839009999978, 1508.008613658229933, 224.0655036725979983 ) ) ;
#28500 = CARTESIAN_POINT ( 'NONE',  ( 9.559657396529310347, 1499.907619752240180, 202.5223157849819984 ) ) ;
#28501 = ORIENTED_EDGE ( 'NONE', *, *, #10758, .T. ) ;
#28502 = CARTESIAN_POINT ( 'NONE',  ( -27.04494122719999893, 1509.634156654429944, 201.2636815846580021 ) ) ;
#28503 = CARTESIAN_POINT ( 'NONE',  ( 20.51044083260000050, 1453.146242307730063, 210.6541360869379957 ) ) ;
#28504 = CARTESIAN_POINT ( 'NONE',  ( -3.526881412259999848, 1486.384130060029975, 181.8597813580979903 ) ) ;
#28505 = CARTESIAN_POINT ( 'NONE',  ( -1.208143323520000090, 1443.877572099090230, 199.8977861043090059 ) ) ;
#28506 = CARTESIAN_POINT ( 'NONE',  ( -16.83458865165958329, 1489.059916236708887, 195.6887827414307424 ) ) ;
#28507 = AXIS2_PLACEMENT_3D ( 'NONE', #55481, #64438, #4518 ) ;
#28508 = CARTESIAN_POINT ( 'NONE',  ( 23.86310425499999965, 1449.793994881729986, 216.0471939728780058 ) ) ;
#28509 = CARTESIAN_POINT ( 'NONE',  ( 7.360599658199999062, 1427.547306193929899, 213.0878178632989943 ) ) ;
#28510 = CARTESIAN_POINT ( 'NONE',  ( -27.38624145287259992, 1383.845277887050088, 225.3372244541170062 ) ) ;
#28511 = CARTESIAN_POINT ( 'NONE',  ( -15.68560764121220252, 1410.853875961199947, 226.7268370761429992 ) ) ;
#28512 = CARTESIAN_POINT ( 'NONE',  ( 5.456938789187089967, 1422.711578738400021, 123.3297044728370082 ) ) ;
#28513 = CARTESIAN_POINT ( 'NONE',  ( 1966.823930461590180, 11221.53578756869865, 443.7115846868979929 ) ) ;
#28514 = CARTESIAN_POINT ( 'NONE',  ( 0.1627114960534379873, 1484.640266453030108, 181.8950381876209690 ) ) ;
#28516 = ORIENTED_EDGE ( 'NONE', *, *, #8529, .T. ) ;
#28515 = CARTESIAN_POINT ( 'NONE',  ( 12.53380499169999851, 1445.052233488290085, 181.5854552579979782 ) ) ;
#28517 = CARTESIAN_POINT ( 'NONE',  ( -0.5620977655390000383, 1416.851343894929869, 227.7685710125980165 ) ) ;
#28518 = VECTOR ( 'NONE', #74961, 1000.000000000000000 ) ;
#28519 = CARTESIAN_POINT ( 'NONE',  ( -3.078458300270000336, 1380.877403101729897, 216.4127659855790284 ) ) ;
#28520 = ADVANCED_FACE ( 'NONE', ( #11120, #2182 ), #96773, .F. ) ;
#28521 = CARTESIAN_POINT ( 'NONE',  ( -4.462434020839999960, 1475.381478586690037, 199.6802092454289834 ) ) ;
#28523 = ORIENTED_EDGE ( 'NONE', *, *, #96527, .T. ) ;
#28522 = FACE_OUTER_BOUND ( 'NONE', #56317, .T. ) ;
#28524 = CARTESIAN_POINT ( 'NONE',  ( 2.740681441353109982, 1426.136206333369955, 188.7843748818769996 ) ) ;
#28525 = ORIENTED_EDGE ( 'NONE', *, *, #100665, .F. ) ;
#28526 = CARTESIAN_POINT ( 'NONE',  ( -9.884511408893031259, 1387.770251651480066, 217.5398018212560203 ) ) ;
#28527 = CARTESIAN_POINT ( 'NONE',  ( 2.453554202689999908, 1485.341762335490102, 201.5382166200789698 ) ) ;
#28528 = CARTESIAN_POINT ( 'NONE',  ( -2.674529714745956355, 1509.030966574465992, 238.5990776960643132 ) ) ;
#28529 = AXIS2_PLACEMENT_3D ( 'NONE', #4738, #98798, #105568 ) ;
#28530 = CARTESIAN_POINT ( 'NONE',  ( -11.60004869885203860, 1426.765778568870473, 134.3812644074278069 ) ) ;
#28531 = CARTESIAN_POINT ( 'NONE',  ( -2.762666289370000250, 1431.313464822989999, 217.0512884656089909 ) ) ;
#28532 = DIRECTION ( 'NONE',  ( 0.6840490078599928969, -0.2249866269914024275, -0.6938717262727969182 ) ) ;
#28533 = CARTESIAN_POINT ( 'NONE',  ( 11.17685589271990132, 1409.303364787639794, 219.0471118356899751 ) ) ;
#28534 = CARTESIAN_POINT ( 'NONE',  ( -7.966104681038361335, 1384.917613660750021, 199.4892774705519969 ) ) ;
#28535 = CARTESIAN_POINT ( 'NONE',  ( -105.9580761981150090, 1385.235267633950116, 296.9951120641670173 ) ) ;
#28536 = CARTESIAN_POINT ( 'NONE',  ( -17.93301568280000069, 1421.479046128729806, 192.7257549160979977 ) ) ;
#28537 = CARTESIAN_POINT ( 'NONE',  ( 10.77406844824080068, 1422.341328632539899, 209.8534941415630044 ) ) ;
#28538 = CIRCLE ( 'NONE', #91111, 32.13701971169416538 ) ;
#28539 = B_SPLINE_CURVE_WITH_KNOTS ( 'NONE', 3,
 ( #11193, #28530, #90625, #89530, #47543, #38033, #65460, #64908, #73852, #4968, #5531, #39684, #22851, #22294, #56496, #21189 ),
 .UNSPECIFIED., .F., .F.,
 ( 4, 2, 2, 2, 2, 2, 2, 4 ),
 ( 0.000000000000000000, 6.242631834405030047E-05, 0.0001248526366881006009, 0.0002497052733760278379, 0.0004994105467520596874, 0.0009988210935039975105, 0.001997642187007867085, 0.003995284374015670853 ),
 .UNSPECIFIED. ) ;
#28540 = CARTESIAN_POINT ( 'NONE',  ( 11.37862535051929846, 1491.234308450049866, 207.8509436897950025 ) ) ;
#28541 = EDGE_CURVE ( 'NONE', #9907, #19921, #90400, .T. ) ;
#28542 = EDGE_LOOP ( 'NONE', ( #55198, #65654 ) ) ;
#28543 = ORIENTED_EDGE ( 'NONE', *, *, #52472, .F. ) ;
#28544 = CARTESIAN_POINT ( 'NONE',  ( -12.17244369484309985, 1416.196255300809980, 194.7590107260170100 ) ) ;
#28545 = CARTESIAN_POINT ( 'NONE',  ( -11.95703516740000083, 1433.553083509069893, 150.3051793736979960 ) ) ;
#28546 = EDGE_CURVE ( 'NONE', #77058, #82322, #65376, .T. ) ;
#28547 = CARTESIAN_POINT ( 'NONE',  ( 27.65869848730375580, 1463.963929344026837, 269.4462227895727437 ) ) ;
#28548 = CARTESIAN_POINT ( 'NONE',  ( 12.04784982253540093, 1427.346391823369913, 208.1256229127970130 ) ) ;
#28549 = CARTESIAN_POINT ( 'NONE',  ( -0.04898381728909999983, 1396.985963199730122, 221.9366346587979706 ) ) ;
#28550 = CARTESIAN_POINT ( 'NONE',  ( 32.38114538885250226, 1523.604703353109699, 202.1233279672528624 ) ) ;
#28551 = CARTESIAN_POINT ( 'NONE',  ( 12.45034049356619832, 1421.619540909540092, 207.5029415923690124 ) ) ;
#28552 = CARTESIAN_POINT ( 'NONE',  ( -11.86834588888874187, 1366.062423491164964, 209.6218459617033432 ) ) ;
#28553 = CARTESIAN_POINT ( 'NONE',  ( 6.280317093924558058, 1507.235120824685737, 235.5599512983970669 ) ) ;
#28554 = CARTESIAN_POINT ( 'NONE',  ( -4.625359562974999506, 1517.025470194390209, 206.6416589153869836 ) ) ;
#28555 = AXIS2_PLACEMENT_3D ( 'NONE', #52651, #10078, #10644 ) ;
#28556 = DIRECTION ( 'NONE',  ( 0.000000000000000000, 1.000000000000000000, 0.000000000000000000 ) ) ;
#28557 = B_SPLINE_SURFACE_WITH_KNOTS ( 'NONE', 5, 5, ( 
 ( #108546, #75521, #93936, #92841, #8275, #31837 ),
 ( #58161, #17202, #92291, #59271, #109655, #49762 ),
 ( #41896, #66022, #7735, #101777, #15014, #15561 ),
 ( #100145, #23431, #91740, #32931, #6636, #32397 ),
 ( #7197, #68232, #49212, #41354, #42440, #74968 ),
 ( #59816, #100683, #67120, #101221, #24519, #50852 ),
 ( #58709, #16117, #76053, #110196, #16655, #33470 ),
 ( #93389, #76599, #110750, #34041, #102338, #25625 ),
 ( #51398, #19998, #70443, #36255, #60931, #77168 ) ),
 .UNSPECIFIED., .F., .F., .F.,
 ( 6, 3, 6 ),
 ( 6, 6 ),
 ( 51.68681987850000326, 64.13305301190000307, 71.37864106410030729 ),
 ( -0.0007601185783282820218, 2.000000000000000000 ),
 .UNSPECIFIED. ) ;
#28558 = CARTESIAN_POINT ( 'NONE',  ( 0.5620975286139998639, 1416.851343894929869, 190.4751211476980188 ) ) ;
#28559 = CARTESIAN_POINT ( 'NONE',  ( -0.3719917208641120299, 1456.560529944520113, 189.3260140039109842 ) ) ;
#28560 = CARTESIAN_POINT ( 'NONE',  ( -0.4151546846821903003, 1522.382868172863937, 175.3106345060153046 ) ) ;
#28561 = CARTESIAN_POINT ( 'NONE',  ( 41.28926753630349822, 1444.140857746640222, 136.6209720351870089 ) ) ;
#28562 = ORIENTED_EDGE ( 'NONE', *, *, #7034, .F. ) ;
#28563 = CARTESIAN_POINT ( 'NONE',  ( 19.16279675359999857, 1411.291488917830065, 262.3396920791980165 ) ) ;
#28564 = CARTESIAN_POINT ( 'NONE',  ( -25.67898337120000107, 1449.805023464449960, 208.3992226959499874 ) ) ;
#28565 = CARTESIAN_POINT ( 'NONE',  ( -9.946004468827549516, 1425.248700426040159, 91.15452372544520188 ) ) ;
#28566 = B_SPLINE_CURVE_WITH_KNOTS ( 'NONE', 3,
 ( #21602, #22692, #38416, #12674, #49052, #64201, #83188, #14309, #48501, #31670, #56892, #91023, #106183, #82640, #47389, #106720, #29465, #74257, #30574, #63658, #97773, #55807, #89924, #13199, #81510, #98875, #22141, #84817, #85368, #16497, #94322 ),
 .UNSPECIFIED., .F., .F.,
 ( 4, 3, 3, 3, 3, 3, 3, 3, 3, 3, 4 ),
 ( -7.456423346589999390, -7.344770142544849278, -7.144274285211090536, -6.832125223832170136, -6.600994903882189568, -6.405260161108500050, -6.335246464236609754, -5.648730639708280599, -4.892201118308060259, -4.020974890406479929, -3.062118867579999737 ),
 .UNSPECIFIED. ) ;
#28567 = EDGE_CURVE ( 'NONE', #78311, #22689, #94356, .T. ) ;
#28568 = B_SPLINE_CURVE_WITH_KNOTS ( 'NONE', 1,
 ( #74862, #109006 ),
 .UNSPECIFIED., .F., .F.,
 ( 2, 2 ),
 ( 0.000000000000000000, 1.000000000000000000 ),
 .UNSPECIFIED. ) ;
#28569 = CARTESIAN_POINT ( 'NONE',  ( -12.50000000000000000, 1384.913060387289988, 209.1218459572589836 ) ) ;
#28570 = CARTESIAN_POINT ( 'NONE',  ( -5.442004254910000505, 1413.088571900130091, 250.5651368536980215 ) ) ;
#28571 = CARTESIAN_POINT ( 'NONE',  ( 20.38555278956989980, 1509.665894582069996, 230.7615064735390149 ) ) ;
#28572 = CYLINDRICAL_SURFACE ( 'NONE', #15902, 1.999999999999999556 ) ;
#28573 = CARTESIAN_POINT ( 'NONE',  ( 31.77002005290000142, 1451.803664145230186, 134.7784598387979997 ) ) ;
#28574 = ORIENTED_EDGE ( 'NONE', *, *, #74145, .T. ) ;
#28575 = CARTESIAN_POINT ( 'NONE',  ( 7.031363022279999875, 1494.605019377190047, 219.3119659920989761 ) ) ;
#28576 = CARTESIAN_POINT ( 'NONE',  ( 11.63092933939999973, 1509.332558450729948, 236.5028663931980191 ) ) ;
#28577 = VERTEX_POINT ( 'NONE', #5452 ) ;
#28578 = ORIENTED_EDGE ( 'NONE', *, *, #63930, .T. ) ;
#28579 = CARTESIAN_POINT ( 'NONE',  ( 1.317811661047104010, 1517.151704408390060, 223.5300434977941677 ) ) ;
#28580 = FACE_OUTER_BOUND ( 'NONE', #83744, .T. ) ;
#28581 = ORIENTED_EDGE ( 'NONE', *, *, #49662, .T. ) ;
#28582 = DIRECTION ( 'NONE',  ( -0.4794256325653583617, -1.076139176629626574E-09, -0.8775825105591531505 ) ) ;
#28583 = CARTESIAN_POINT ( 'NONE',  ( -5.122105890483237722, 1419.728707206990748, 194.5792988059779702 ) ) ;
#28584 = CARTESIAN_POINT ( 'NONE',  ( 0.4834647446390000214, 1450.896177426419854, 181.9315483554979949 ) ) ;
#28585 = CARTESIAN_POINT ( 'NONE',  ( -6.683495332149999690, 1479.767561397530017, 234.4915808808979989 ) ) ;
#28586 = CARTESIAN_POINT ( 'NONE',  ( 7.166260505965389882, 1508.551565390810083, 203.0889814045920048 ) ) ;
#28587 = VERTEX_POINT ( 'NONE', #56978 ) ;
#28588 = CARTESIAN_POINT ( 'NONE',  ( 11.73707087880000088, 1426.695959143629807, 144.1731741463979972 ) ) ;
#28589 = LINE ( 'NONE', #43744, #7432 ) ;
#28590 = FACE_OUTER_BOUND ( 'NONE', #51249, .T. ) ;
#28591 = VERTEX_POINT ( 'NONE', #99490 ) ;
#28592 = CARTESIAN_POINT ( 'NONE',  ( -0.01289782690309849988, 1516.939723362869927, 204.1155860834069813 ) ) ;
#28593 = ORIENTED_EDGE ( 'NONE', *, *, #2873, .F. ) ;
#28594 = CARTESIAN_POINT ( 'NONE',  ( 11.83743466531329958, 1430.378478851539967, 149.6260558822839926 ) ) ;
#28595 = AXIS2_PLACEMENT_3D ( 'NONE', #93680, #8588, #228 ) ;
#28596 = CARTESIAN_POINT ( 'NONE',  ( 5.513435558552499671, 1508.783371651585412, 201.6678281800477350 ) ) ;
#28597 = ORIENTED_EDGE ( 'NONE', *, *, #6407, .T. ) ;
#28598 = ORIENTED_EDGE ( 'NONE', *, *, #39971, .T. ) ;
#28599 = CARTESIAN_POINT ( 'NONE',  ( 30.79107737087824148, 1526.107876515966382, 201.1252789359793383 ) ) ;
#28600 = CARTESIAN_POINT ( 'NONE',  ( -1.465793917108519917, 1484.360957496709943, 182.4810413606819850 ) ) ;
#28601 = CARTESIAN_POINT ( 'NONE',  ( 2.144541734774120023, 1498.044082580750000, 197.8976195832460121 ) ) ;
#28602 =( BOUNDED_SURFACE ( )  B_SPLINE_SURFACE ( 3, 2, ( 
 ( #74645, #83031, #75198 ),
 ( #39375, #5787, #101453 ),
 ( #32073, #33166, #84122 ),
 ( #74097, #109349, #73550 ),
 ( #49443, #81916, #66264 ),
 ( #6322, #109886, #108781 ),
 ( #32630, #107684, #67356 ),
 ( #13593, #23666, #31513 ) ),
 .UNSPECIFIED., .F., .F., .F. ) 
 B_SPLINE_SURFACE_WITH_KNOTS ( ( 4, 2, 2, 4 ),
 ( 3, 3 ),
 ( -1.766815860282378026E-15, 0.004949486174159700019, 0.007424229261240433871, 0.009898972348321167722 ),
 ( 0.000000000000000000, 1.000000000000000000 ),
 .UNSPECIFIED. ) 
 GEOMETRIC_REPRESENTATION_ITEM ( )  RATIONAL_B_SPLINE_SURFACE ( (
 ( 1.000000000000000000, 0.7008167338404790447, 1.000000000000000000),
 ( 1.000000000000000000, 0.6998717715541517004, 1.000000000000000000),
 ( 1.000000000000000000, 0.6996362482572846542, 1.000000000000000000),
 ( 1.000000000000000000, 0.6996543733527801345, 1.000000000000000000),
 ( 1.000000000000000000, 0.6997206268242501803, 1.000000000000000000),
 ( 1.000000000000000000, 0.6997875685291419234, 1.000000000000000000),
 ( 1.000000000000000000, 0.6997874718065202337, 1.000000000000000000),
 ( 1.000000000000000000, 0.6996393088224879264, 1.000000000000000000) ) ) 
 REPRESENTATION_ITEM ( '' )  SURFACE ( )  );
#28603 = CARTESIAN_POINT ( 'NONE',  ( -7.548376016692439627, 1471.189479627299988, 215.9520417340509937 ) ) ;
#28604 = CARTESIAN_POINT ( 'NONE',  ( -4.255765417200000122, 1424.084099830230116, 185.1505376682980000 ) ) ;
#28605 = CONICAL_SURFACE ( 'NONE', #91183, 0.9999999999999836797, 0.7853981633970000820 ) ;
#28606 = CARTESIAN_POINT ( 'NONE',  ( 3.511242806360000301, 1408.661939287229870, 270.4277067456980035 ) ) ;
#28607 = CARTESIAN_POINT ( 'NONE',  ( -8.337034337958545649, 1374.413060387289988, 204.5673033449591003 ) ) ;
#28608 = CARTESIAN_POINT ( 'NONE',  ( -31.23437356469425907, 1512.187213306747481, 222.8968241038848248 ) ) ;
#28609 = CARTESIAN_POINT ( 'NONE',  ( 8.556723711100000074, 1492.088035619889979, 216.2210623239989786 ) ) ;
#28610 = CYLINDRICAL_SURFACE ( 'NONE', #21534, 1.999999999999999556 ) ;
#28611 = CARTESIAN_POINT ( 'NONE',  ( -10.26338073471560008, 1521.551704408389924, 184.6900425920350131 ) ) ;
#28613 = CARTESIAN_POINT ( 'NONE',  ( -30.51231035492526900, 1526.382868172863937, 200.0858385050243555 ) ) ;
#28612 = CARTESIAN_POINT ( 'NONE',  ( -18.15983708720000323, 1504.845299867989979, 208.9729485910140170 ) ) ;
#28614 = CARTESIAN_POINT ( 'NONE',  ( -61.47253991323098177, 1379.746604392680183, 268.2739652327719000 ) ) ;
#28615 = CARTESIAN_POINT ( 'NONE',  ( -9.953599203913679361, 1439.570906027390038, 208.2134350005999863 ) ) ;
#28616 = CARTESIAN_POINT ( 'NONE',  ( -7.869279002454999450, 1514.500328598799797, 202.7397161129169945 ) ) ;
#28617 = ORIENTED_EDGE ( 'NONE', *, *, #95293, .T. ) ;
#28618 = CARTESIAN_POINT ( 'NONE',  ( 30.40113727430000168, 1433.623945461559742, 255.3819207742980097 ) ) ;
#28619 = VECTOR ( 'NONE', #103309, 1000.000000000000000 ) ;
#28620 = CARTESIAN_POINT ( 'NONE',  ( 13.06732508390000014, 1434.812095170660086, 149.1115247062979847 ) ) ;
#28621 = CARTESIAN_POINT ( 'NONE',  ( -75.79396460638429289, 1385.005618079479973, 300.7326138283579553 ) ) ;
#28622 = CARTESIAN_POINT ( 'NONE',  ( -21.08704007906051459, 1525.317349363567700, 233.7719395062865146 ) ) ;
#28623 = CARTESIAN_POINT ( 'NONE',  ( 0.000000000000000000, 1512.187213306747481, 209.1218459616979999 ) ) ;
#28624 = LINE ( 'NONE', #46547, #13327 ) ;
#28626 = ORIENTED_EDGE ( 'NONE', *, *, #77582, .F. ) ;
#28625 = CARTESIAN_POINT ( 'NONE',  ( -16.91019554306700101, 1419.805496799009916, 208.4777216397309871 ) ) ;
#28627 = CARTESIAN_POINT ( 'NONE',  ( -16.53125420670000167, 1418.541487540729804, 202.7561987471289910 ) ) ;
#28628 = CARTESIAN_POINT ( 'NONE',  ( -24.86063957340000030, 1443.226756493010043, 210.5718459218879843 ) ) ;
#28629 = CARTESIAN_POINT ( 'NONE',  ( -2.200595920237713443, 1449.951443106519264, 154.3737305154650414 ) ) ;
#28630 = CARTESIAN_POINT ( 'NONE',  ( -6.430337163319999050, 1460.599122871690042, 209.4294524016669925 ) ) ;
#28631 = CARTESIAN_POINT ( 'NONE',  ( 14.74158144963499950, 1513.636261293280086, 225.1273934092670288 ) ) ;
#28632 = LINE ( 'NONE', #70674, #4419 ) ;
#28633 = CARTESIAN_POINT ( 'NONE',  ( 19.56575328779210210, 1509.675102991920312, 232.0410837715500065 ) ) ;
#28634 = DIRECTION ( 'NONE',  ( 0.000000000000000000, 0.000000000000000000, 1.000000000000000000 ) ) ;
#28635 = CARTESIAN_POINT ( 'NONE',  ( 12.03371223569974546, 1433.763409174216577, 149.8203876007945041 ) ) ;
#28636 = CARTESIAN_POINT ( 'NONE',  ( 7.307429526299999978, 1412.733471104129876, 230.8457520919979800 ) ) ;
#28637 = CARTESIAN_POINT ( 'NONE',  ( -15.93611219510135690, 1463.426168696786590, 221.8455668742993225 ) ) ;
#28638 = CARTESIAN_POINT ( 'NONE',  ( -16.16439218409000134, 1459.158912558008069, 229.6201563168629889 ) ) ;
#28639 = AXIS2_PLACEMENT_3D ( 'NONE', #39678, #64347, #97910 ) ;
#28640 = CARTESIAN_POINT ( 'NONE',  ( 6.546001350565000543, 1516.557392317769882, 207.4118413833070065 ) ) ;
#28641 = CARTESIAN_POINT ( 'NONE',  ( 45.45312728100000044, 1434.909613172649870, 268.5145791497980099 ) ) ;
#28642 = CARTESIAN_POINT ( 'NONE',  ( -17.06951414919999621, 1409.509140956229885, 223.5446133271979932 ) ) ;
#28643 = B_SPLINE_CURVE_WITH_KNOTS ( 'NONE', 5,
 ( #97747, #44609, #103943, #70939, #71498, #54678 ),
 .UNSPECIFIED., .F., .F.,
 ( 6, 6 ),
 ( 0.000000000000000000, 1.000000000000000000 ),
 .UNSPECIFIED. ) ;
#28644 = CARTESIAN_POINT ( 'NONE',  ( 17.84168301100000065, 1435.550183323570081, 147.0878683823979998 ) ) ;
#28645 = B_SPLINE_SURFACE_WITH_KNOTS ( 'NONE', 5, 1, ( 
 ( #32318, #67589 ),
 ( #41268, #58630 ),
 ( #50239, #37706 ),
 ( #53992, #43902 ),
 ( #36600, #45031 ),
 ( #71907, #27105 ),
 ( #70799, #29298 ),
 ( #45583, #27649 ),
 ( #52869, #61835 ) ),
 .UNSPECIFIED., .F., .F., .F.,
 ( 6, 3, 6 ),
 ( 2, 2 ),
 ( 0.000000000000000000, 3.961384672979999966, 7.908240876339999836 ),
 ( 0.000000000000000000, 14.00000000000000000 ),
 .UNSPECIFIED. ) ;
#28646 = CARTESIAN_POINT ( 'NONE',  ( 20.59881216440000173, 1488.586115637029934, 191.4156880852980009 ) ) ;
#28647 = CARTESIAN_POINT ( 'NONE',  ( 29.58091120952471087, 1509.965401515384656, 207.4724573392817035 ) ) ;
#28648 = CARTESIAN_POINT ( 'NONE',  ( -12.59362883767730068, 1379.001259401459947, 208.4073637545409952 ) ) ;
#28649 = CARTESIAN_POINT ( 'NONE',  ( -17.14836123659999600, 1420.862901227730163, 226.7325726209979848 ) ) ;
#28650 = DIRECTION ( 'NONE',  ( -0.4990868181313579677, -0.2476038100682859955, 0.8304244102910179892 ) ) ;
#28651 = CARTESIAN_POINT ( 'NONE',  ( -40.15194941080000035, 1442.235659217200009, 136.9582246599980238 ) ) ;
#28652 = CARTESIAN_POINT ( 'NONE',  ( 27.43355929049999986, 1507.980920699130138, 207.4175378521480013 ) ) ;
#28653 = CARTESIAN_POINT ( 'NONE',  ( -18.12194535329999923, 1416.217772597929979, 205.1982926197480026 ) ) ;
#28654 = AXIS2_PLACEMENT_3D ( 'NONE', #3926, #19588, #62752 ) ;
#28655 = CARTESIAN_POINT ( 'NONE',  ( -12.37413385660000031, 1442.559515703879924, 186.8960802690980074 ) ) ;
#28656 = CARTESIAN_POINT ( 'NONE',  ( -7.543897025694540126, 1384.866236297619935, 219.0872343606769732 ) ) ;
#28657 = CARTESIAN_POINT ( 'NONE',  ( 13.50155420149999941, 1434.968988600800230, 146.4346117040979891 ) ) ;
#28658 = CARTESIAN_POINT ( 'NONE',  ( -33.53719532080000221, 1435.668427015990119, 135.5141658639980164 ) ) ;
#28659 = FACE_OUTER_BOUND ( 'NONE', #25818, .T. ) ;
#28660 = ORIENTED_EDGE ( 'NONE', *, *, #31801, .T. ) ;
#28661 = CARTESIAN_POINT ( 'NONE',  ( -2.892503416934999905, 1511.980236064749988, 201.3440512220070104 ) ) ;
#28662 = CARTESIAN_POINT ( 'NONE',  ( -10.10721564661269944, 1409.266012135149822, 220.1412772847010046 ) ) ;
#28663 = CARTESIAN_POINT ( 'NONE',  ( 33.93019615848945847, 1522.382868172863937, 197.6607374645996060 ) ) ;
#28664 = CARTESIAN_POINT ( 'NONE',  ( 7.000000000000000000, 1432.413060387330006, 146.1721969590979882 ) ) ;
#28665 = CARTESIAN_POINT ( 'NONE',  ( -4.554264956864240155, 1421.567767465303632, 137.7199131393125526 ) ) ;
#28666 = CARTESIAN_POINT ( 'NONE',  ( -37.64035307139999986, 1461.657675810230103, 268.7654384304980226 ) ) ;
#28667 = CARTESIAN_POINT ( 'NONE',  ( -17.20774676790000157, 1505.417530106830100, 224.1865155378980035 ) ) ;
#28668 = CARTESIAN_POINT ( 'NONE',  ( 0.2427754188691099713, 1419.580316797580053, 184.3807419939530234 ) ) ;
#28669 = CARTESIAN_POINT ( 'NONE',  ( 19.02270174365980893, 1526.382868172864164, 232.8547275633986828 ) ) ;
#28670 = CARTESIAN_POINT ( 'NONE',  ( -98.46962093215799428, 1384.603681201170048, 310.6350572453490031 ) ) ;
#28671 = CARTESIAN_POINT ( 'NONE',  ( -48.42360680834229925, 1385.013694626130018, 222.8933081124880005 ) ) ;
#28672 = CARTESIAN_POINT ( 'NONE',  ( -5.025617208240078959, 1375.287809068920069, 214.7234685881729774 ) ) ;
#28673 = CARTESIAN_POINT ( 'NONE',  ( 14.33002530890000159, 1414.913060387329779, 216.6125821906579745 ) ) ;
#28674 = CARTESIAN_POINT ( 'NONE',  ( 13.91144599429999928, 1452.416393839029979, 223.0990526455979932 ) ) ;
#28675 = DIRECTION ( 'NONE',  ( -0.07713599384728245245, -0.9969860201949397593, -0.008301444997533467124 ) ) ;
#28676 = EDGE_CURVE ( 'NONE', #97154, #37608, #43613, .T. ) ;
#28678 = EDGE_LOOP ( 'NONE', ( #81324, #98670, #67744, #1425, #108996 ) ) ;
#28677 = CARTESIAN_POINT ( 'NONE',  ( 1.050222213330426424, 1370.064815538551329, 206.9592408025515624 ) ) ;
#28679 = CARTESIAN_POINT ( 'NONE',  ( -8.156361363509999407, 1384.926233631970035, 199.6467913925089874 ) ) ;
#28680 = CARTESIAN_POINT ( 'NONE',  ( 3.014988837336279204, 1420.039847312813663, 137.0999999980979851 ) ) ;
#28681 = CARTESIAN_POINT ( 'NONE',  ( -3.873647543780000202, 1495.674801125089971, 219.6259912128990095 ) ) ;
#28682 = CARTESIAN_POINT ( 'NONE',  ( -11.68483146220000002, 1415.296882296330068, 195.2371074489979890 ) ) ;
#28683 = AXIS2_PLACEMENT_3D ( 'NONE', #83382, #66071, #99072 ) ;
#28684 = CARTESIAN_POINT ( 'NONE',  ( -0.3528731710729979820, 1421.448950200250010, 193.6845254781989922 ) ) ;
#28685 = EDGE_CURVE ( 'NONE', #5040, #10960, #65935, .T. ) ;
#28686 = CARTESIAN_POINT ( 'NONE',  ( 22.00569631529999981, 1409.681516235830031, 211.9427731882580304 ) ) ;
#28687 = B_SPLINE_SURFACE_WITH_KNOTS ( 'NONE', 5, 5, ( 
 ( #78632, #833, #19241, #53451, #103829, #110569, #27675, #93741, #69144 ),
 ( #61315, #8646, #103248, #95980, #8098, #34415, #42266, #18696, #27129 ),
 ( #52893, #42821, #26559, #76981, #1947, #68588, #102692, #60752, #69710 ),
 ( #25987, #9761, #60187, #94875, #94304, #86468, #18152, #52347, #43926 ),
 ( #78072, #87022, #1375, #35518, #47237, #62412, #3057, #10884, #79200 ),
 ( #62983, #97094, #45056, #96539, #105491, #20907, #88149, #81364, #12528 ),
 ( #46706, #38817, #98728, #98176, #2506, #28782, #4678, #19813, #37183 ),
 ( #36627, #107131, #20359, #54564, #70825, #54019, #88698, #55109, #11437 ),
 ( #80836, #72994, #11979, #46160, #71933, #97638, #87596, #80291, #71380 ),
 ( #37729, #64057, #3606, #89233, #106045, #29322, #21989, #63522, #4144 ),
 ( #45608, #104937, #38268, #72453, #28224, #106583, #29870, #21446, #55656 ),
 ( #79750, #89779, #30422, #13048, #64609, #49990, #22539, #99817, #13597 ),
 ( #39379, #58395, #15256, #56741, #100911, #67360, #40475, #49447, #48350 ),
 ( #107688, #5226, #41591, #90877, #33170, #75202, #109353, #92521, #91981 ),
 ( #56181, #100385, #108230, #14165, #109890, #23670, #57315, #32078, #75746 ),
 ( #91442, #101457, #90319, #41024, #47786, #81921, #73554, #65699, #57853 ),
 ( #99261, #48908, #30972, #65148, #82489, #5791, #66810, #32634, #39932 ),
 ( #83571, #74101, #31517, #23111, #6864, #24209, #14718, #83035, #15789 ),
 ( #84126, #7425, #108786, #6326, #74650, #66268, #95298, #102564, #103120 ),
 ( #17447, #1812, #94736, #59502, #70134, #85222, #699, #69015, #103692 ),
 ( #34279, #16892, #35948, #102018, #93075, #26421, #78498, #16349, #7971 ),
 ( #25857, #9081, #34828, #24746, #68460, #51097, #93613, #85782, #1246 ),
 ( #60614, #157, #60058, #58945, #51645, #94176, #18559, #67910, #50547 ),
 ( #43248, #84672, #18014, #42688, #9620, #52207, #52753, #43789, #110438 ),
 ( #42138, #86886, #77397, #10180, #76845, #86334, #77939, #35384, #8514 ),
 ( #69573, #26992, #61181, #44355, #76288, #33717, #25301, #20224, #2372 ),
 ( #105351, #70684, #36487, #104797, #96401, #37034, #71229, #55508, #53312 ),
 ( #106447, #44920, #89636, #21303, #19108, #87454, #2917, #10748, #38134 ),
 ( #88019, #28084, #79067, #3462, #4009, #46012, #12923, #89091, #29730 ),
 ( #47103, #88558, #81229, #62272, #11303, #37590, #28641, #62845, #71792 ),
 ( #19677, #4544, #54964, #105911, #53882, #96958, #63916, #38678, #29190 ),
 ( #45471, #63381, #97497, #98031, #54425, #104246, #27536, #79613, #61719 ),
 ( #12378, #95841, #46565, #11841, #80143, #20765, #80699, #72315, #100772 ) ),
 .UNSPECIFIED., .F., .F., .F.,
 ( 6, 3, 3, 3, 3, 3, 3, 3, 3, 3, 6 ),
 ( 6, 3, 6 ),
 ( 24.21111657910000048, 25.10793423650000022, 26.03050881489999924, 28.79878516220000151, 31.56706150950000023, 38.94765790310000142, 55.51095904740000009, 72.07426019160000408, 88.69155109330000641, 122.0027592590000012, 143.4996508910000159 ),
 ( 0.000000000000000000, 1.000000000000000000, 2.000000000000000000 ),
 .UNSPECIFIED. ) ;
#28688 = CARTESIAN_POINT ( 'NONE',  ( -106.7343056398989916, 1391.913060387289988, 306.0197523768699739 ) ) ;
#28689 = CARTESIAN_POINT ( 'NONE',  ( -9.866420828029999868, 1449.262144085689897, 190.8627134521989888 ) ) ;
#28690 = CARTESIAN_POINT ( 'NONE',  ( -5.385042926340570801, 1432.007300083129849, 154.5986668458859867 ) ) ;
#28692 = CARTESIAN_POINT ( 'NONE',  ( -12.01638735929999946, 1378.563403400179823, 206.1479454454890003 ) ) ;
#28691 = CARTESIAN_POINT ( 'NONE',  ( 4.789673499540000101, 1465.867933640490037, 219.0700355186390027 ) ) ;
#28693 = CARTESIAN_POINT ( 'NONE',  ( 0.7201256557630000277, 1415.745261378530131, 233.3682385266980077 ) ) ;
#28694 = AXIS2_PLACEMENT_3D ( 'NONE', #23469, #41393, #75558 ) ;
#28695 = CARTESIAN_POINT ( 'NONE',  ( -11.40503451100000021, 1490.739837095889925, 209.6941766733859822 ) ) ;
#28696 = CARTESIAN_POINT ( 'NONE',  ( -8.624710350819999150, 1367.191948709370081, 210.6218459616991936 ) ) ;
#28697 = CARTESIAN_POINT ( 'NONE',  ( 2.868433798504999910, 1517.020727862619879, 204.1095288638669842 ) ) ;
#28698 = CARTESIAN_POINT ( 'NONE',  ( -20.33636649369999816, 1427.581624735430069, 223.9337651306980206 ) ) ;
#28699 = CARTESIAN_POINT ( 'NONE',  ( -18.41867143110519933, 1486.196793196990029, 188.8168638707130071 ) ) ;
#28700 = AXIS2_PLACEMENT_3D ( 'NONE', #107703, #14734, #23126 ) ;
#28701 = CARTESIAN_POINT ( 'NONE',  ( -9.255392140700001491, 1423.205578550119753, 209.4023171091370159 ) ) ;
#28702 = CARTESIAN_POINT ( 'NONE',  ( -11.88408465604287656, 1421.854389613024978, 210.6434707533515507 ) ) ;
#28704 = ORIENTED_EDGE ( 'NONE', *, *, #29001, .T. ) ;
#28703 = CARTESIAN_POINT ( 'NONE',  ( -68.32997003290930138, 1379.746898581680171, 279.8958236475029935 ) ) ;
#28705 = VERTEX_POINT ( 'NONE', #97847 ) ;
#28706 = CARTESIAN_POINT ( 'NONE',  ( 27.78683896639999773, 1509.618348729030004, 214.6924127718480122 ) ) ;
#28707 = ORIENTED_EDGE ( 'NONE', *, *, #15751, .F. ) ;
#28708 = CARTESIAN_POINT ( 'NONE',  ( 1.145290945507940084, 1458.110487998910003, 199.6352770989870180 ) ) ;
#28709 = CARTESIAN_POINT ( 'NONE',  ( -109.9853967420000060, 1384.924299815560062, 311.4561928992590083 ) ) ;
#28711 = CARTESIAN_POINT ( 'NONE',  ( 1.539395910930000166, 1508.628951913829951, 180.5172630586980063 ) ) ;
#28710 = CARTESIAN_POINT ( 'NONE',  ( -15.68560764121220252, 1410.853875961199947, 226.7268370761429992 ) ) ;
#28712 = PLANE ( 'NONE',  #45447 ) ;
#28713 = CARTESIAN_POINT ( 'NONE',  ( -25.20238731644419872, 1451.152274905429977, 137.4649534155230128 ) ) ;
#28714 = CARTESIAN_POINT ( 'NONE',  ( 9.055564386196214954, 1440.382423718937844, 153.5303063279175433 ) ) ;
#28715 = CARTESIAN_POINT ( 'NONE',  ( 13.40311307709999866, 1409.883220066930107, 228.1200985806979702 ) ) ;
#28716 = CARTESIAN_POINT ( 'NONE',  ( 4.042417777704999438, 1516.904492006980036, 212.5700528489170154 ) ) ;
#28717 = CARTESIAN_POINT ( 'NONE',  ( 41.53765979141579834, 1445.128430570580122, 134.0999999984609872 ) ) ;
#28718 = CARTESIAN_POINT ( 'NONE',  ( -6.016306044853139134, 1426.646534911480103, 205.6760721705690003 ) ) ;
#28719 = CARTESIAN_POINT ( 'NONE',  ( -11.36018337610000195, 1414.996442546130083, 195.9645814914979951 ) ) ;
#28720 = ORIENTED_EDGE ( 'NONE', *, *, #8381, .T. ) ;
#28721 = CARTESIAN_POINT ( 'NONE',  ( -3.005258425510039633, 1450.300055283400070, 188.5532298547360028 ) ) ;
#28722 = CARTESIAN_POINT ( 'NONE',  ( -2.071979039770960096, 1431.299421665210275, 200.9961302677540118 ) ) ;
#28723 = ORIENTED_EDGE ( 'NONE', *, *, #15394, .T. ) ;
#28724 = ORIENTED_EDGE ( 'NONE', *, *, #52443, .F. ) ;
#28725 = ORIENTED_EDGE ( 'NONE', *, *, #73545, .T. ) ;
#28726 = CARTESIAN_POINT ( 'NONE',  ( -8.308248955145000281, 1512.693483295319993, 216.2230634388170074 ) ) ;
#28727 = FACE_OUTER_BOUND ( 'NONE', #685, .T. ) ;
#28728 = VECTOR ( 'NONE', #99929, 1000.000000000000114 ) ;
#28729 = CARTESIAN_POINT ( 'NONE',  ( 15.10981120460822957, 1451.148210361404836, 149.6511074968155981 ) ) ;
#28730 = CARTESIAN_POINT ( 'NONE',  ( -3.008276117979999942, 1485.138067935930167, 183.1683143970979870 ) ) ;
#28731 = CARTESIAN_POINT ( 'NONE',  ( 9.750232545500001180, 1462.891281938590282, 208.5260954797809916 ) ) ;
#28732 = CARTESIAN_POINT ( 'NONE',  ( -12.34367812709999868, 1378.698035246239897, 209.0347064062579818 ) ) ;
#28733 = CARTESIAN_POINT ( 'NONE',  ( -63.83653764405461573, 1379.736250008309526, 269.8484324899241642 ) ) ;
#28734 = CARTESIAN_POINT ( 'NONE',  ( 4.251649916467110657, 1446.494082692860047, 160.8451567543189924 ) ) ;
#28735 = B_SPLINE_CURVE_WITH_KNOTS ( 'NONE', 3,
 ( #59891, #16725, #110264, #42511, #32472, #50388 ),
 .UNSPECIFIED., .F., .F.,
 ( 4, 2, 4 ),
 ( 0.000000000000000000, 0.5000000000000000000, 1.000000000000000000 ),
 .UNSPECIFIED. ) ;
#28736 = LINE ( 'NONE', #21401, #32456 ) ;
#28737 = VERTEX_POINT ( 'NONE', #72145 ) ;
#28738 = CARTESIAN_POINT ( 'NONE',  ( -6.563254928984999736, 1517.139039350860003, 206.6385234782069915 ) ) ;
#28739 = VERTEX_POINT ( 'NONE', #22772 ) ;
#28740 = CARTESIAN_POINT ( 'NONE',  ( 26.52681755028470079, 1440.913060387330006, 243.7300046518169836 ) ) ;
#28741 = CARTESIAN_POINT ( 'NONE',  ( -16.93968655440000148, 1509.443694557030085, 185.0606162848980034 ) ) ;
#28742 = ORIENTED_EDGE ( 'NONE', *, *, #12480, .T. ) ;
#28743 = CARTESIAN_POINT ( 'NONE',  ( 26.57123036162979801, 1448.090663227739924, 137.0341373801179827 ) ) ;
#28744 = CARTESIAN_POINT ( 'NONE',  ( -13.57503295039999891, 1410.760072987729927, 189.9862946811979896 ) ) ;
#28745 = CARTESIAN_POINT ( 'NONE',  ( -56.57320206062674117, 1379.715264457238845, 258.9695720208346756 ) ) ;
#28747 = LINE ( 'NONE', #45576, #11608 ) ;
#28746 = CARTESIAN_POINT ( 'NONE',  ( -24.39265439800000124, 1441.035345296090100, 211.3385326736879790 ) ) ;
#28748 = B_SPLINE_CURVE_WITH_KNOTS ( 'NONE', 3,
 ( #60070, #9630, #43258, #102029, #110449, #51656, #167, #94187, #85795, #51107, #8525, #710, #109901, #1258, #18026, #42701, #92531, #34289, #76857, #52219, #68471, #102573 ),
 .UNSPECIFIED., .F., .F.,
 ( 4, 3, 3, 3, 3, 3, 3, 4 ),
 ( -15.61491491670000009, -14.96471882913919949, -13.64186865260530013, -12.35990197051819983, -12.10144895473209914, -11.03773465448690061, -9.945779857935429291, -9.104900364405690283 ),
 .UNSPECIFIED. ) ;
#28749 = CARTESIAN_POINT ( 'NONE',  ( -8.789510382754970763, 1436.967902467539943, 213.5031532571800028 ) ) ;
#28750 = CARTESIAN_POINT ( 'NONE',  ( -6.044713241076149934, 1511.753217516670247, 200.8247887982400073 ) ) ;
#28751 = CARTESIAN_POINT ( 'NONE',  ( 15.24750708283499989, 1514.857962383129916, 194.6708682431670070 ) ) ;
#28752 = CARTESIAN_POINT ( 'NONE',  ( -11.94130205119999921, 1433.615242452219945, 148.5637080951979669 ) ) ;
#28753 = CARTESIAN_POINT ( 'NONE',  ( 23.61230825720000226, 1435.322028862560046, 137.2857987807979896 ) ) ;
#28755 = CARTESIAN_POINT ( 'NONE',  ( 17.78284146230000218, 1432.724246433989947, 213.5810953123289835 ) ) ;
#28754 = CARTESIAN_POINT ( 'NONE',  ( 12.23138524880000055, 1463.686947130230010, 231.4510838504980086 ) ) ;
#28756 = CARTESIAN_POINT ( 'NONE',  ( -5.003220765204999587, 1516.983995446890049, 216.0685944891870065 ) ) ;
#28757 = CARTESIAN_POINT ( 'NONE',  ( -2.225547318884174786, 1525.712830164893376, 241.5729992621096756 ) ) ;
#28758 = CARTESIAN_POINT ( 'NONE',  ( 5.395039045001690070, 1511.384172056590160, 217.2813686725590117 ) ) ;
#28759 = CARTESIAN_POINT ( 'NONE',  ( 29.12559690860000217, 1509.873774306529867, 207.7706034996080007 ) ) ;
#28760 = CARTESIAN_POINT ( 'NONE',  ( -6.546951720715000533, 1516.606339319019980, 211.9964348928969855 ) ) ;
#28761 = EDGE_CURVE ( 'NONE', #69813, #7138, #105093, .T. ) ;
#28762 = CARTESIAN_POINT ( 'NONE',  ( -18.34422345790000008, 1416.813004075630033, 208.8605758367380076 ) ) ;
#28763 = CARTESIAN_POINT ( 'NONE',  ( -3.283955654634000076, 1483.490552537069789, 198.9754571030750014 ) ) ;
#28765 = ORIENTED_EDGE ( 'NONE', *, *, #7765, .F. ) ;
#28764 = CARTESIAN_POINT ( 'NONE',  ( 3.822978225239960004, 1508.729442836390035, 213.6787569587939970 ) ) ;
#28766 = CIRCLE ( 'NONE', #37716, 2.000000000000001776 ) ;
#28767 = CARTESIAN_POINT ( 'NONE',  ( -17.10350668511973993, 1524.477587234265911, 237.2713348840137542 ) ) ;
#28768 = CARTESIAN_POINT ( 'NONE',  ( -1.133866162019999861E-09, 1468.084175535529994, 248.5896189568980219 ) ) ;
#28769 = EDGE_CURVE ( 'NONE', #88920, #76110, #74605, .T. ) ;
#28770 = CARTESIAN_POINT ( 'NONE',  ( -11.57713237839999998, 1432.387637135029991, 151.1965105832979930 ) ) ;
#28771 = CARTESIAN_POINT ( 'NONE',  ( -14.42895189880000117, 1415.865101995610075, 203.8800253788289751 ) ) ;
#28772 = EDGE_CURVE ( 'NONE', #23409, #47384, #63667, .T. ) ;
#28773 = CARTESIAN_POINT ( 'NONE',  ( -0.2885899904230180280, 1507.883288131039990, 237.4859410355080058 ) ) ;
#28774 = CARTESIAN_POINT ( 'NONE',  ( -19.13404846440000284, 1457.718989482430061, 226.6686308623980040 ) ) ;
#28775 = B_SPLINE_CURVE_WITH_KNOTS ( 'NONE', 5,
 ( #26572, #61877, #44502, #95448, #87041, #18168, #86483, #27692, #9779 ),
 .UNSPECIFIED., .F., .F.,
 ( 6, 3, 6 ),
 ( 0.000000000000000000, 0.5000000000000000000, 1.000000000000000000 ),
 .UNSPECIFIED. ) ;
#28777 = CARTESIAN_POINT ( 'NONE',  ( 2.500000000000000000, 1432.353950668519929, 157.4944280282979889 ) ) ;
#28776 = CARTESIAN_POINT ( 'NONE',  ( -21.30784275718657028, 1411.017705672756620, 200.6768285256719082 ) ) ;
#28778 = CARTESIAN_POINT ( 'NONE',  ( -8.736970513497151813, 1448.822091765960067, 211.8396115544819907 ) ) ;
#28779 = CARTESIAN_POINT ( 'NONE',  ( -105.3217700133209860, 1379.643688862580120, 306.4247263515759983 ) ) ;
#28780 = ORIENTED_EDGE ( 'NONE', *, *, #46294, .T. ) ;
#28781 = CARTESIAN_POINT ( 'NONE',  ( -2.491188396525000126, 1516.733363207009916, 205.0947945262969938 ) ) ;
#28782 = CARTESIAN_POINT ( 'NONE',  ( 0.8851054190410000411, 1406.072537395830068, 269.0453913371979979 ) ) ;
#28783 = AXIS2_PLACEMENT_3D ( 'NONE', #15838, #110484, #7470 ) ;
#28784 = CARTESIAN_POINT ( 'NONE',  ( -0.008453540501490530365, 1515.389376838289991, 213.4149486290589834 ) ) ;
#28785 = CARTESIAN_POINT ( 'NONE',  ( 6.516345065877910514, 1472.619501843580110, 270.3713698276869195 ) ) ;
#28787 = B_SPLINE_CURVE_WITH_KNOTS ( 'NONE', 3,
 ( #17457, #58407, #51657, #42702, #51109, #6882, #85233, #100923, #41036, #75215, #16360, #109902, #60072, #24758, #93625, #15800, #84138, #7438, #8526, #59513, #50559, #67921, #76858, #25869, #33182, #67372 ),
 .UNSPECIFIED., .F., .F.,
 ( 4, 2, 1, 1, 1, 1, 1, 2, 2, 2, 2, 1, 1, 1, 2, 2, 4 ),
 ( 0.000000000000000000, 0.1249999999996812827, 0.1874999999995336231, 0.2187499999994684807, 0.2343749999994343414, 0.2421874999993992028, 0.2460937499993816058, 0.2480468749993638977, 0.2499999999993462174, 0.3749999999998965827, 0.4375000000001806888, 0.4687500000003306244, 0.4843750000004123923, 0.4921875000004532485, 0.4960937500004726219, 0.5000000000004920508, 1.000000000000000000 ),
 .UNSPECIFIED. ) ;
#28786 = CARTESIAN_POINT ( 'NONE',  ( 2.478932746460000391, 1432.564745886140145, 157.5224116325979935 ) ) ;
#28788 = CARTESIAN_POINT ( 'NONE',  ( 11.60004869885203682, 1422.222932908421853, 135.5999999980979567 ) ) ;
#28789 = AXIS2_PLACEMENT_3D ( 'NONE', #38242, #62382, #53989 ) ;
#28790 = B_SPLINE_CURVE_WITH_KNOTS ( 'NONE', 5,
 ( #67142, #48127, #32952, #100168, #14494, #75541 ),
 .UNSPECIFIED., .F., .F.,
 ( 6, 6 ),
 ( 0.000000000000000000, 1.000000000000000000 ),
 .UNSPECIFIED. ) ;
#28791 = CARTESIAN_POINT ( 'NONE',  ( -43.11122459500789716, 1440.913060409440050, 263.3173459173530091 ) ) ;
#28792 = CYLINDRICAL_SURFACE ( 'NONE', #32410, 1.999999999999999556 ) ;
#28793 = CARTESIAN_POINT ( 'NONE',  ( -31.23437356469455040, 1512.187213306747481, 195.3468678195118287 ) ) ;
#28794 = CARTESIAN_POINT ( 'NONE',  ( 0.6956281545320009974, 1431.241352936390058, 200.3845806967489978 ) ) ;
#28795 = CARTESIAN_POINT ( 'NONE',  ( 14.41619641355878478, 1509.538862670986418, 235.4310391072028494 ) ) ;
#28796 = CARTESIAN_POINT ( 'NONE',  ( 1.946416182649999937, 1507.064669603390030, 220.8001475467989962 ) ) ;
#28797 = CARTESIAN_POINT ( 'NONE',  ( -4.290508147089998836, 1515.379315998089851, 209.1218459616989946 ) ) ;
#28798 = EDGE_CURVE ( 'NONE', #27843, #85013, #93860, .T. ) ;
#28799 = AXIS2_PLACEMENT_3D ( 'NONE', #93886, #23917, #68183 ) ;
#28800 = ORIENTED_EDGE ( 'NONE', *, *, #15912, .T. ) ;
#28801 = CARTESIAN_POINT ( 'NONE',  ( -11.06589456070000033, 1424.668795903030286, 234.3916895697979612 ) ) ;
#28802 = CARTESIAN_POINT ( 'NONE',  ( 10.12295999200579999, 1469.488668891520092, 206.2402591453380012 ) ) ;
#28803 = AXIS2_PLACEMENT_3D ( 'NONE', #92377, #56047, #108083 ) ;
#28804 = CARTESIAN_POINT ( 'NONE',  ( -0.7749238296759999312, 1475.832189872029858, 266.9609160975979876 ) ) ;
#28805 = CARTESIAN_POINT ( 'NONE',  ( -4.288435981061489599, 1446.932127814390014, 155.2226307056990038 ) ) ;
#28806 = CARTESIAN_POINT ( 'NONE',  ( -30.79697748855988593, 1526.178928173328131, 196.3997152352021942 ) ) ;
#28807 = CARTESIAN_POINT ( 'NONE',  ( -27.81979543383449993, 1384.836325904559999, 225.9468839794940038 ) ) ;
#28808 = CARTESIAN_POINT ( 'NONE',  ( -18.58720762869999987, 1416.311719779230089, 208.5274638254259969 ) ) ;
#28809 = CARTESIAN_POINT ( 'NONE',  ( -8.899263831619999010, 1482.224852125390044, 203.1955085269790118 ) ) ;
#28810 = CARTESIAN_POINT ( 'NONE',  ( 26.68805691732229946, 1436.277521234780124, 136.6581429669300007 ) ) ;
#28811 = CARTESIAN_POINT ( 'NONE',  ( -7.475863647388560018, 1396.174123299650091, 217.2595793039530179 ) ) ;
#28812 =( BOUNDED_CURVE ( )  B_SPLINE_CURVE ( 3, ( #26087, #94973, #86563, #42354 ),
 .UNSPECIFIED., .F., .F. ) 
 B_SPLINE_CURVE_WITH_KNOTS ( ( 4, 4 ),
 ( 1.282864256331062158, 2.438226007407914953 ),
 .UNSPECIFIED. ) 
 CURVE ( )  GEOMETRIC_REPRESENTATION_ITEM ( )  RATIONAL_B_SPLINE_CURVE ( ( 1.000000000000000000, 0.8918208900698291197, 0.8918208900698291197, 1.000000000000000000 ) ) 
 REPRESENTATION_ITEM ( '' )  );
#28813 = VECTOR ( 'NONE', #93606, 1000.000000000000000 ) ;
#28814 = CARTESIAN_POINT ( 'NONE',  ( -15.23090723337400121, 1422.122923179038025, 227.7537106409200192 ) ) ;
#28815 = CARTESIAN_POINT ( 'NONE',  ( -16.08386308296240230, 1409.482933452620046, 225.3901198913439998 ) ) ;
#28816 = CARTESIAN_POINT ( 'NONE',  ( -44.91834551880000248, 1440.343506779659947, 269.6914828722979678 ) ) ;
#28817 = ORIENTED_EDGE ( 'NONE', *, *, #43571, .T. ) ;
#28818 = EDGE_CURVE ( 'NONE', #10547, #97701, #38251, .T. ) ;
#28819 = CARTESIAN_POINT ( 'NONE',  ( 16.66936639845652834, 1512.187213306747481, 237.7608804993219280 ) ) ;
#28820 = CARTESIAN_POINT ( 'NONE',  ( -15.59907717326891330, 1415.960253477549941, 208.0471002303526689 ) ) ;
#28821 = CARTESIAN_POINT ( 'NONE',  ( -19.06723915664710134, 1485.490521620860136, 189.6150037022410118 ) ) ;
#28823 = CARTESIAN_POINT ( 'NONE',  ( -13.51662157586499902, 1512.620989416249813, 192.6780328270669997 ) ) ;
#28822 = CARTESIAN_POINT ( 'NONE',  ( 11.51812271839999902, 1426.832871545830130, 128.4954513222980097 ) ) ;
#28824 = DIRECTION ( 'NONE',  ( 0.000000000000000000, 0.000000000000000000, -1.000000000000000000 ) ) ;
#28825 = CARTESIAN_POINT ( 'NONE',  ( -12.53380498098199602, 1442.773887284840612, 205.2015002797237173 ) ) ;
#28826 = CARTESIAN_POINT ( 'NONE',  ( 7.717505752974999744, 1516.857914730730045, 201.4043401791270185 ) ) ;
#28827 = CARTESIAN_POINT ( 'NONE',  ( 7.916532357550000398, 1425.151355441629903, 211.5881757975789981 ) ) ;
#28828 = CARTESIAN_POINT ( 'NONE',  ( -2.424063131930000115, 1427.257651041929876, 147.9020499575979954 ) ) ;
#28829 = CARTESIAN_POINT ( 'NONE',  ( 3.573194667510000144, 1509.053513020129913, 179.7696517855980005 ) ) ;
#28830 = CARTESIAN_POINT ( 'NONE',  ( 0.04548916784448110012, 1416.835419214280137, 190.9576572557899965 ) ) ;
#28831 = CARTESIAN_POINT ( 'NONE',  ( -52.83507688520099776, 1378.584541267579880, 254.3209184245819756 ) ) ;
#28832 = VECTOR ( 'NONE', #96549, 1000.000000000000000 ) ;
#28833 = CARTESIAN_POINT ( 'NONE',  ( 6.358435812139999754, 1368.427897723179740, 207.6218459616989946 ) ) ;
#28836 = VERTEX_POINT ( 'NONE', #41808 ) ;
#28835 = CARTESIAN_POINT ( 'NONE',  ( -1.835915877731372658, 1464.997577545588001, 237.8268834563425287 ) ) ;
#28834 = PRODUCT_RELATED_PRODUCT_CATEGORY ( 'part', '', ( #39314 ) ) ;
#28837 = EDGE_LOOP ( 'NONE', ( #12690, #62060, #10562, #96318 ) ) ;
#28838 = CARTESIAN_POINT ( 'NONE',  ( -8.582734512730000986, 1398.167885046430001, 198.9971942070980049 ) ) ;
#28839 = CARTESIAN_POINT ( 'NONE',  ( -15.43255204080000098, 1409.451976979829851, 192.6616394286979812 ) ) ;
#28840 = CARTESIAN_POINT ( 'NONE',  ( 11.34090880850000005, 1475.513060387329915, 227.1982711657979905 ) ) ;
#28841 = CARTESIAN_POINT ( 'NONE',  ( -1.732266665236295466, 1442.302600356889116, 200.4062168750837145 ) ) ;
#28843 = CARTESIAN_POINT ( 'NONE',  ( -1.363077736744499946, 1415.332184859939844, 185.3921874643629906 ) ) ;
#28842 = CARTESIAN_POINT ( 'NONE',  ( -8.873043061549999777, 1384.563416185930009, 218.6696054037190038 ) ) ;
#28844 = B_SPLINE_CURVE_WITH_KNOTS ( 'NONE', 3,
 ( #93547, #76767, #76218, #42067, #51574, #74178, #99334, #94104, #38882, #5859, #51021, #108308, #102499, #22608, #101945, #47854, #93003, #64682, #65770 ),
 .UNSPECIFIED., .F., .F.,
 ( 4, 2, 1, 2, 2, 2, 2, 2, 2, 4 ),
 ( 0.000000000000000000, 0.1250000000001602329, 0.1875000000002953748, 0.2187500000003569645, 0.2500000000004185541, 0.3750000000005341283, 0.4375000000005920264, 0.5000000000006499246, 0.7500000000003249623, 1.000000000000000000 ),
 .UNSPECIFIED. ) ;
#28845 = CARTESIAN_POINT ( 'NONE',  ( 10.74246380849999838, 1429.760558640729869, 188.0236792812979729 ) ) ;
#28846 = FILL_AREA_STYLE_COLOUR ( '', #76500 ) ;
#28847 = CARTESIAN_POINT ( 'NONE',  ( -38.72664573631579543, 1449.455593765829917, 136.0882868071720395 ) ) ;
#28848 = CARTESIAN_POINT ( 'NONE',  ( -2.500000000000000000, 1448.201359996650126, 168.5754994529100088 ) ) ;
#28849 = CARTESIAN_POINT ( 'NONE',  ( 3.005276066430000448, 1369.205039411269809, 207.6218459616989946 ) ) ;
#28850 = DIRECTION ( 'NONE',  ( 0.000000000000000000, 6.429979419034159461E-12, -1.000000000000000000 ) ) ;
#28851 = CARTESIAN_POINT ( 'NONE',  ( -5.353064078697809869, 1406.074448326960010, 267.2230922050150070 ) ) ;
#28852 = DIRECTION ( 'NONE',  ( 0.000000000000000000, 0.000000000000000000, -1.000000000000000000 ) ) ;
#28853 = VERTEX_POINT ( 'NONE', #68149 ) ;
#28854 = DIRECTION ( 'NONE',  ( -0.9822959463204248287, 0.1391731009605849945, -0.1254014426211909616 ) ) ;
#28855 = CARTESIAN_POINT ( 'NONE',  ( 12.81356597149999921, 1442.366100173290079, 188.3022465221979758 ) ) ;
#28856 = ORIENTED_EDGE ( 'NONE', *, *, #45319, .T. ) ;
#28857 = ORIENTED_EDGE ( 'NONE', *, *, #75568, .T. ) ;
#28858 = ADVANCED_FACE ( 'NONE', ( #109573 ), #109892, .F. ) ;
#28859 = CARTESIAN_POINT ( 'NONE',  ( 0.03326177659115069768, 1408.911898860609881, 187.0499707311110171 ) ) ;
#28860 = CARTESIAN_POINT ( 'NONE',  ( 9.842969107809999230, 1365.740588703660023, 207.6218459616989946 ) ) ;
#28861 = EDGE_CURVE ( 'NONE', #102542, #43545, #17033, .T. ) ;
#28862 = CARTESIAN_POINT ( 'NONE',  ( 2.294209629405000062, 1516.603620185149794, 214.8927295341169952 ) ) ;
#28863 = CARTESIAN_POINT ( 'NONE',  ( 2.950959321895000098, 1512.115618635729788, 217.0053894627469901 ) ) ;
#28864 = MECHANICAL_DESIGN_GEOMETRIC_PRESENTATION_REPRESENTATION (  '', ( #68204 ), #39564 ) ;
#28865 = ORIENTED_EDGE ( 'NONE', *, *, #44711, .T. ) ;
#28866 = CARTESIAN_POINT ( 'NONE',  ( 2.500000000000039968, 1448.773875821790170, 156.9803059956940103 ) ) ;
#28867 = CARTESIAN_POINT ( 'NONE',  ( -84.75344743939999148, 1379.600296256739966, 297.4377104216590055 ) ) ;
#28868 = AXIS2_PLACEMENT_3D ( 'NONE', #60285, #61406, #94404 ) ;
#28869 = CARTESIAN_POINT ( 'NONE',  ( -106.3336369974139899, 1378.913060387289988, 302.1715538163180099 ) ) ;
#28870 = CARTESIAN_POINT ( 'NONE',  ( -1.134358008724999811, 1516.744381837270112, 205.0932347109869909 ) ) ;
#28871 = CARTESIAN_POINT ( 'NONE',  ( -12.23489732466240021, 1490.237667237379810, 209.6383001084460034 ) ) ;
#28872 = CARTESIAN_POINT ( 'NONE',  ( -41.71656132900650960, 1437.001393571195194, 269.6421165700213578 ) ) ;
#28873 = CARTESIAN_POINT ( 'NONE',  ( -10.71339925790000080, 1409.287180533330002, 227.5724378756979718 ) ) ;
#28875 = ORIENTED_EDGE ( 'NONE', *, *, #89043, .T. ) ;
#28874 = CARTESIAN_POINT ( 'NONE',  ( 2.038646110889678287, 1525.960063244516959, 177.0579350083066004 ) ) ;
#28876 = CARTESIAN_POINT ( 'NONE',  ( 0.000000000000000000, 1512.051704408390151, 209.1218459616989946 ) ) ;
#28877 = CARTESIAN_POINT ( 'NONE',  ( 3.346707516019999940, 1443.005054410889898, 217.3642451189890323 ) ) ;
#28878 = CARTESIAN_POINT ( 'NONE',  ( 18.97665094185096990, 1526.382868172863937, 232.9676995165609412 ) ) ;
#28879 = FACE_OUTER_BOUND ( 'NONE', #67864, .T. ) ;
#28880 = EDGE_CURVE ( 'NONE', #30887, #25245, #58251, .T. ) ;
#28881 = CARTESIAN_POINT ( 'NONE',  ( 41.20035157204440424, 1427.456943461399987, 270.1350674680870156 ) ) ;
#28882 = CARTESIAN_POINT ( 'NONE',  ( 7.336844642415000450, 1517.106845464700200, 212.5753907958570039 ) ) ;
#28883 = CARTESIAN_POINT ( 'NONE',  ( -67.25967724030000738, 1379.748837366600128, 277.1187736907589851 ) ) ;
#28884 = CARTESIAN_POINT ( 'NONE',  ( 0.02009666217332761046, 1507.207408199481961, 237.3586634061521750 ) ) ;
#28885 = CARTESIAN_POINT ( 'NONE',  ( -30.57065064348379835, 1523.844782250847175, 221.8563543952624855 ) ) ;
#28887 = EDGE_CURVE ( 'NONE', #68290, #105027, #89990, .T. ) ;
#28886 = CARTESIAN_POINT ( 'NONE',  ( 16.50820735058650257, 1494.476772471000004, 193.0249898974809923 ) ) ;
#28888 = CARTESIAN_POINT ( 'NONE',  ( -2.873919040654999701, 1516.940252185109784, 209.1351185066319829 ) ) ;
#28889 = ORIENTED_EDGE ( 'NONE', *, *, #85128, .F. ) ;
#28890 = CARTESIAN_POINT ( 'NONE',  ( -106.6611006919228117, 1391.449730528028113, 300.4457761524841999 ) ) ;
#28891 = CARTESIAN_POINT ( 'NONE',  ( -12.94419629340000100, 1420.439331177430176, 228.3355065355980003 ) ) ;
#28892 = CARTESIAN_POINT ( 'NONE',  ( -113.4000000000000057, 1384.574445395800012, 311.2057750932590352 ) ) ;
#28893 = EDGE_CURVE ( 'NONE', #101455, #28836, #67427, .T. ) ;
#28894 = ORIENTED_EDGE ( 'NONE', *, *, #17134, .F. ) ;
#28896 = CIRCLE ( 'NONE', #44985, 0.9999999999999930056 ) ;
#28895 = CARTESIAN_POINT ( 'NONE',  ( -37.05217134432169956, 1385.198326583020162, 237.2200995400409909 ) ) ;
#28897 = CARTESIAN_POINT ( 'NONE',  ( -3.209303788360000187, 1428.804527045590021, 200.3203052568389921 ) ) ;
#28898 = CARTESIAN_POINT ( 'NONE',  ( 18.65451742820949832, 1507.632629731499947, 188.5326158842280222 ) ) ;
#28899 = CARTESIAN_POINT ( 'NONE',  ( 7.552141914295000369, 1510.542924508009946, 205.3415595432570058 ) ) ;
#28900 = CARTESIAN_POINT ( 'NONE',  ( -0.1880784674069999884, 1408.919628232130208, 231.7730996565980206 ) ) ;
#28901 = CARTESIAN_POINT ( 'NONE',  ( -0.1168129828940950021, 1420.457736004669869, 182.7197010214190129 ) ) ;
#28902 = EDGE_CURVE ( 'NONE', #81426, #59762, #47460, .T. ) ;
#28904 = CARTESIAN_POINT ( 'NONE',  ( -7.812463265990185590, 1516.551704358176721, 211.9845609180970030 ) ) ;
#28903 = CARTESIAN_POINT ( 'NONE',  ( -7.715625241105000143, 1516.786099423779888, 215.6766101314970001 ) ) ;
#28905 = CARTESIAN_POINT ( 'NONE',  ( 1.376928043298433657, 1517.051704408389924, 191.7575736759021936 ) ) ;
#28906 = CARTESIAN_POINT ( 'NONE',  ( 10.02037163873229986, 1469.310947271520035, 208.3108194760559968 ) ) ;
#28907 = ORIENTED_EDGE ( 'NONE', *, *, #72168, .T. ) ;
#28908 = CARTESIAN_POINT ( 'NONE',  ( -12.95840410776020057, 1416.218047878440075, 196.6656636057070102 ) ) ;
#28909 = CYLINDRICAL_SURFACE ( 'NONE', #83842, 0.5000000000000022204 ) ;
#28910 = ORIENTED_EDGE ( 'NONE', *, *, #110424, .T. ) ;
#28911 = AXIS2_PLACEMENT_3D ( 'NONE', #103940, #69260, #105052 ) ;
#28912 = DIRECTION ( 'NONE',  ( -0.9948834766775040972, 0.000000000000000000, 0.1010290445074212007 ) ) ;
#28913 = EDGE_CURVE ( 'NONE', #13345, #58330, #26001, .T. ) ;
#28914 = DIRECTION ( 'NONE',  ( -1.000000000000000000, 0.000000000000000000, -1.989567262110869994E-13 ) ) ;
#28915 = CARTESIAN_POINT ( 'NONE',  ( 8.247029077068420477, 1511.494703458840149, 203.4175148351339999 ) ) ;
#28916 = ADVANCED_FACE ( 'NONE', ( #76499 ), #67571, .T. ) ;
#28917 = UNCERTAINTY_MEASURE_WITH_UNIT (LENGTH_MEASURE( 1.000000000000000082E-05 ), #80223, 'distance_accuracy_value', 'NONE');
#28918 = CARTESIAN_POINT ( 'NONE',  ( -0.09849533087990110236, 1444.626931724390033, 218.0966844286490129 ) ) ;
#28919 = CARTESIAN_POINT ( 'NONE',  ( -27.81797958387629777, 1509.852926761900108, 200.9687172335360117 ) ) ;
#28920 = CARTESIAN_POINT ( 'NONE',  ( -2.500000000000000000, 1448.197706736029886, 167.4845663601980164 ) ) ;
#28921 = CARTESIAN_POINT ( 'NONE',  ( -18.07950054330000000, 1423.749692319529913, 225.6737955892980096 ) ) ;
#28922 = CARTESIAN_POINT ( 'NONE',  ( -18.37019422750000075, 1435.283622672170168, 146.1498534422979958 ) ) ;
#28923 = CARTESIAN_POINT ( 'NONE',  ( -4.643169496351990055, 1464.538216081999963, 199.1279085030210183 ) ) ;
#28924 = CARTESIAN_POINT ( 'NONE',  ( -2.500000000000000000, 1439.615672362369878, 170.5246407198980023 ) ) ;
#28926 = CARTESIAN_POINT ( 'NONE',  ( -18.59402987153349684, 1437.048336213511902, 212.3086441927383134 ) ) ;
#28925 = CARTESIAN_POINT ( 'NONE',  ( 0.4455705167121439825, 1409.096190068570195, 232.6073811540130123 ) ) ;
#28927 = EDGE_CURVE ( 'NONE', #14943, #40151, #68134, .T. ) ;
#28928 = CARTESIAN_POINT ( 'NONE',  ( -0.04830720914946320249, 1457.855805554629796, 229.0971631259880041 ) ) ;
#28929 = VERTEX_POINT ( 'NONE', #75951 ) ;
#28930 = CARTESIAN_POINT ( 'NONE',  ( -9.420366384649998537, 1508.551704410389902, 218.6205651585790122 ) ) ;
#28931 = CARTESIAN_POINT ( 'NONE',  ( 3.347801439296143933, 1523.382868172864164, 242.0893193391992497 ) ) ;
#28932 = EDGE_CURVE ( 'NONE', #43923, #64525, #41791, .T. ) ;
#28933 = CARTESIAN_POINT ( 'NONE',  ( -23.78094776239999675, 1436.491024829749904, 211.7413630244279830 ) ) ;
#28934 = CARTESIAN_POINT ( 'NONE',  ( -20.83094015030000179, 1452.185627928030044, 134.0999999980979851 ) ) ;
#28935 = CARTESIAN_POINT ( 'NONE',  ( -18.62446834819999708, 1507.629699710430032, 229.7127857518979965 ) ) ;
#28936 = CARTESIAN_POINT ( 'NONE',  ( -2.385609062339151709, 1525.697947650495507, 241.0978138787441480 ) ) ;
#28937 = CARTESIAN_POINT ( 'NONE',  ( 12.84239221398829933, 1435.935692713660046, 150.8114773724069835 ) ) ;
#28938 =( GEOMETRIC_REPRESENTATION_CONTEXT ( 3 ) GLOBAL_UNCERTAINTY_ASSIGNED_CONTEXT ( ( #27808 ) ) GLOBAL_UNIT_ASSIGNED_CONTEXT ( ( #24282, #67431, #34900 ) ) REPRESENTATION_CONTEXT ( 'NONE', 'WORKASPACE' ) );
#28939 = CARTESIAN_POINT ( 'NONE',  ( -16.81223226430000039, 1414.913060387329779, 207.5743821216680089 ) ) ;
#28940 = DIRECTION ( 'NONE',  ( -0.6736849260149578855, 0.000000000000000000, 0.7390186874905266823 ) ) ;
#28941 = ADVANCED_FACE ( 'NONE', ( #68674 ), #33936, .F. ) ;
#28942 = CARTESIAN_POINT ( 'NONE',  ( -10.07725390801599907, 1490.597947965959975, 213.5248140628600027 ) ) ;
#28943 = CARTESIAN_POINT ( 'NONE',  ( 20.33642835536319993, 1475.138372969219972, 218.0161211975080278 ) ) ;
#28944 = CARTESIAN_POINT ( 'NONE',  ( -87.30327056457821300, 1383.772041066240035, 307.5216316904810014 ) ) ;
#28945 = CARTESIAN_POINT ( 'NONE',  ( -109.0400471772699973, 1383.917152605130013, 311.1276274378030280 ) ) ;
#28946 = CARTESIAN_POINT ( 'NONE',  ( 8.454779184179999518, 1428.363642554090120, 213.4110050395389919 ) ) ;
#28948 = ORIENTED_EDGE ( 'NONE', *, *, #28118, .T. ) ;
#28947 = CARTESIAN_POINT ( 'NONE',  ( 21.87325955929999921, 1509.710279403030199, 189.0200286462979875 ) ) ;
#28949 = CARTESIAN_POINT ( 'NONE',  ( -113.4000000000000057, 1382.340570731539856, 310.5600271202590648 ) ) ;
#28950 = CARTESIAN_POINT ( 'NONE',  ( 13.27508835580430002, 1512.548660307860018, 224.4065169982920054 ) ) ;
#28951 = ORIENTED_EDGE ( 'NONE', *, *, #17206, .T. ) ;
#28952 = ORIENTED_EDGE ( 'NONE', *, *, #52749, .F. ) ;
#28953 = CARTESIAN_POINT ( 'NONE',  ( -20.52849295349999892, 1487.269269018690011, 206.0837407197489881 ) ) ;
#28954 = CARTESIAN_POINT ( 'NONE',  ( -110.0629084960000057, 1384.909053970479818, 296.9513011976590064 ) ) ;
#28955 = CARTESIAN_POINT ( 'NONE',  ( 4.780307568339999591, 1467.625956517089890, 217.8721402715589761 ) ) ;
#28957 = CARTESIAN_POINT ( 'NONE',  ( -34.48978217770000043, 1443.099005945160116, 250.0021841883980471 ) ) ;
#28956 = CARTESIAN_POINT ( 'NONE',  ( 35.03185245808725767, 1424.085991366112466, 269.5319528758505498 ) ) ;
#28958 = CARTESIAN_POINT ( 'NONE',  ( 8.631804350130249048, 1438.018828263250043, 210.0183207127990102 ) ) ;
#28959 = CARTESIAN_POINT ( 'NONE',  ( -11.93337251310000013, 1433.461400490700044, 149.9038012133979976 ) ) ;
#28960 = VECTOR ( 'NONE', #46905, 1000.000000000000114 ) ;
#28961 = CARTESIAN_POINT ( 'NONE',  ( 27.50468030500000083, 1509.873544990630080, 201.6580215447480100 ) ) ;
#28962 = CARTESIAN_POINT ( 'NONE',  ( -19.04715201249999978, 1486.119048487729970, 189.4490706170979877 ) ) ;
#28963 = CARTESIAN_POINT ( 'NONE',  ( 11.42779433089999941, 1410.681993053729911, 189.4262149395979975 ) ) ;
#28964 = CARTESIAN_POINT ( 'NONE',  ( 4.776594320200000077, 1423.601635148929972, 184.0375701292979898 ) ) ;
#28965 = CARTESIAN_POINT ( 'NONE',  ( -0.4426438243505830261, 1515.147163425719782, 213.4491377890840056 ) ) ;
#28966 = CARTESIAN_POINT ( 'NONE',  ( 6.686616336669999328, 1441.247407971460007, 154.4574208692980051 ) ) ;
#28967 = CARTESIAN_POINT ( 'NONE',  ( 13.15339637540530049, 1428.694520551590131, 223.1160257848979995 ) ) ;
#28968 = CARTESIAN_POINT ( 'NONE',  ( 0.01367056495459999937, 1452.767332469230041, 153.3854680590980024 ) ) ;
#28969 = EDGE_CURVE ( 'NONE', #58146, #94338, #88639, .T. ) ;
#28971 = ORIENTED_EDGE ( 'NONE', *, *, #56827, .T. ) ;
#28970 = CARTESIAN_POINT ( 'NONE',  ( 1.784426211945118412, 1474.496765829112519, 219.6664114916495691 ) ) ;
#28972 = ORIENTED_EDGE ( 'NONE', *, *, #8680, .F. ) ;
#28973 = CARTESIAN_POINT ( 'NONE',  ( -12.40530867719999897, 1506.963233163389987, 209.0163269402000026 ) ) ;
#28974 = EDGE_CURVE ( 'NONE', #95247, #20553, #79688, .T. ) ;
#28975 = CARTESIAN_POINT ( 'NONE',  ( 16.60194679285929809, 1493.289934017370115, 193.2049637902070174 ) ) ;
#28976 = CARTESIAN_POINT ( 'NONE',  ( -27.88458103209999805, 1464.440568686830147, 269.9356493381980044 ) ) ;
#28977 = DIRECTION ( 'NONE',  ( -1.000000000000000000, 0.000000000000000000, 0.000000000000000000 ) ) ;
#28978 = CARTESIAN_POINT ( 'NONE',  ( 16.26032963000000109, 1409.480883610230194, 223.2931273867980053 ) ) ;
#28979 = CARTESIAN_POINT ( 'NONE',  ( -15.65975627419999938, 1506.806593729730139, 224.7138568134979835 ) ) ;
#28980 = AXIS2_PLACEMENT_3D ( 'NONE', #93486, #10046, #16756 ) ;
#28981 = CARTESIAN_POINT ( 'NONE',  ( 4.328122124485929589, 1515.115455661490159, 210.0391460303160045 ) ) ;
#28982 = DIRECTION ( 'NONE',  ( 0.000000000000000000, 1.000000000000000000, 0.000000000000000000 ) ) ;
#28983 = CARTESIAN_POINT ( 'NONE',  ( -1.295008548611806143, 1484.564168690730639, 182.3200671755110420 ) ) ;
#28984 = CARTESIAN_POINT ( 'NONE',  ( 10.40058593205784909, 1361.671709241824374, 208.3718459617010978 ) ) ;
#28985 = CARTESIAN_POINT ( 'NONE',  ( -43.92682917671319842, 1430.745472343149913, 266.4731560355739930 ) ) ;
#28986 = EDGE_LOOP ( 'NONE', ( #2796, #77479, #47513, #78232 ) ) ;
#28987 = CARTESIAN_POINT ( 'NONE',  ( -3.537187223599389529, 1495.340936109010045, 181.4789602020310042 ) ) ;
#28988 = ORIENTED_EDGE ( 'NONE', *, *, #45020, .F. ) ;
#28989 = CARTESIAN_POINT ( 'NONE',  ( -2.863787893864999656, 1516.788317650260069, 210.8382387120070121 ) ) ;
#28990 = ADVANCED_FACE ( 'NONE', ( #59714 ), #27722, .F. ) ;
#28991 = CARTESIAN_POINT ( 'NONE',  ( -0.4151546846821905223, 1524.726013923371283, 244.9330574173806383 ) ) ;
#28992 = CARTESIAN_POINT ( 'NONE',  ( -21.33073281779999775, 1509.431426448229786, 190.3502236015980031 ) ) ;
#28993 = CARTESIAN_POINT ( 'NONE',  ( -13.52632867340000189, 1425.416544542129941, 189.2536498548980148 ) ) ;
#28994 = VECTOR ( 'NONE', #19932, 1000.000000000000114 ) ;
#28995 = CARTESIAN_POINT ( 'NONE',  ( 0.3312367761006819733, 1496.117391023140044, 221.4620161682219930 ) ) ;
#28996 = ORIENTED_EDGE ( 'NONE', *, *, #32906, .F. ) ;
#28997 = FACE_OUTER_BOUND ( 'NONE', #48554, .T. ) ;
#28998 = CIRCLE ( 'NONE', #20028, 1.999999999999999556 ) ;
#28999 = CARTESIAN_POINT ( 'NONE',  ( 4.616272296565000488, 1517.030858226499959, 201.7868885755270014 ) ) ;
#29000 = B_SPLINE_CURVE_WITH_KNOTS ( 'NONE', 5,
 ( #55122, #62428, #45069, #46174, #51359, #89245, #80303, #4154, #45624, #61874, #11448, #71942 ),
 .UNSPECIFIED., .F., .F.,
 ( 6, 3, 3, 6 ),
 ( 0.000000000000000000, 0.5001987333065609498, 0.8483151769418431076, 1.000000000000000000 ),
 .UNSPECIFIED. ) ;
#29001 = EDGE_CURVE ( 'NONE', #55385, #3290, #101004, .T. ) ;
#29002 = CARTESIAN_POINT ( 'NONE',  ( 6.665264545140000330, 1472.962710687689878, 217.4318328743790119 ) ) ;
#29003 = CARTESIAN_POINT ( 'NONE',  ( -8.178320334364201472, 1439.186072014569845, 206.0664576276559785 ) ) ;
#29004 = VERTEX_POINT ( 'NONE', #8604 ) ;
#29005 = CARTESIAN_POINT ( 'NONE',  ( -23.29476211502619876, 1412.627406204969930, 270.1903322620909762 ) ) ;
#29006 = CARTESIAN_POINT ( 'NONE',  ( 3.684551893115589394, 1417.858094126330116, 234.2256683103420016 ) ) ;
#29007 = CARTESIAN_POINT ( 'NONE',  ( 8.650215806398520613, 1435.966538205339930, 207.8981607294979881 ) ) ;
#29008 = ADVANCED_FACE ( 'NONE', ( #76937 ), #42777, .T. ) ;
#29010 = ORIENTED_EDGE ( 'NONE', *, *, #17348, .T. ) ;
#29009 = CARTESIAN_POINT ( 'NONE',  ( -8.075791892808387828, 1366.351623811200170, 207.6218459616988241 ) ) ;
#29011 = ORIENTED_EDGE ( 'NONE', *, *, #6667, .T. ) ;
#29012 = B_SPLINE_CURVE_WITH_KNOTS ( 'NONE', 3,
 ( #98673, #88648, #56128, #90263, #101395, #84617 ),
 .UNSPECIFIED., .F., .F.,
 ( 4, 2, 4 ),
 ( 9.242101507433989461E-07, 0.4978491653051179688, 0.9954968279883259497 ),
 .UNSPECIFIED. ) ;
#29013 = CARTESIAN_POINT ( 'NONE',  ( 44.75793395845553846, 1447.593610556694557, 268.9993686022775137 ) ) ;
#29014 = CARTESIAN_POINT ( 'NONE',  ( 8.788316489185000080, 1511.741868877540128, 202.8695794779170001 ) ) ;
#29015 = CARTESIAN_POINT ( 'NONE',  ( 3.649417161288583511, 1424.955166412201606, 184.9140735895639978 ) ) ;
#29016 = CARTESIAN_POINT ( 'NONE',  ( -1.525828703510382134, 1406.001374342115014, 266.9605462712685835 ) ) ;
#29017 = CARTESIAN_POINT ( 'NONE',  ( -17.60066553444309889, 1415.059973079419933, 207.5652353588600079 ) ) ;
#29018 = CARTESIAN_POINT ( 'NONE',  ( -18.51553952359999755, 1435.777052104869881, 225.9247619741979918 ) ) ;
#29019 = CARTESIAN_POINT ( 'NONE',  ( -14.66481730340000134, 1423.493437503330142, 221.6029759380979840 ) ) ;
#29020 = CARTESIAN_POINT ( 'NONE',  ( 12.33246611440000073, 1415.579607672129896, 222.7360816577980245 ) ) ;
#29021 = CARTESIAN_POINT ( 'NONE',  ( 3.853748796670000143, 1447.370069209109943, 184.1245004005980093 ) ) ;
#29022 = CARTESIAN_POINT ( 'NONE',  ( -1.717084749545000122, 1516.819260244609950, 206.6456753351970121 ) ) ;
#29023 = ORIENTED_EDGE ( 'NONE', *, *, #102194, .T. ) ;
#29024 = CARTESIAN_POINT ( 'NONE',  ( -4.682234856550000046, 1438.893385222290135, 227.1256850459990062 ) ) ;
#29025 = CARTESIAN_POINT ( 'NONE',  ( -13.02322703936409987, 1416.825784014559986, 196.6108461303639672 ) ) ;
#29026 = ORIENTED_EDGE ( 'NONE', *, *, #87183, .T. ) ;
#29027 = CARTESIAN_POINT ( 'NONE',  ( 10.36609672684421390, 1455.263332276473875, 226.3870373070946300 ) ) ;
#29028 = EDGE_CURVE ( 'NONE', #106196, #36359, #98334, .T. ) ;
#29029 = CARTESIAN_POINT ( 'NONE',  ( 24.72916343099570113, 1451.812305069729973, 137.1077481279560004 ) ) ;
#29030 = LINE ( 'NONE', #10011, #11459 ) ;
#29031 = CARTESIAN_POINT ( 'NONE',  ( -38.63354197089999786, 1386.820476479690115, 239.2314243943589815 ) ) ;
#29032 = CARTESIAN_POINT ( 'NONE',  ( 2.416798835000000256, 1426.601114010129777, 146.0361887655980127 ) ) ;
#29033 = CARTESIAN_POINT ( 'NONE',  ( 19.23829242040000054, 1410.080596241930152, 196.1913699390979957 ) ) ;
#29034 = CARTESIAN_POINT ( 'NONE',  ( 23.10251669230000360, 1410.654477903330189, 207.3358591529579940 ) ) ;
#29035 = CARTESIAN_POINT ( 'NONE',  ( -24.89775095376042202, 1442.835547651392517, 210.5176539946395451 ) ) ;
#29036 = CARTESIAN_POINT ( 'NONE',  ( -24.22803231680000025, 1427.085958910729914, 210.4997307367480062 ) ) ;
#29037 = DIRECTION ( 'NONE',  ( 0.2046277826698074953, 0.9081497821047129770, -0.3652279340669334906 ) ) ;
#29038 = ADVANCED_FACE ( 'NONE', ( #86427 ), #95659, .T. ) ;
#29039 = CARTESIAN_POINT ( 'NONE',  ( 2.500000000000000000, 1439.534675992210168, 164.5282227258210241 ) ) ;
#29040 = CARTESIAN_POINT ( 'NONE',  ( 7.333070134885000257, 1516.955859323880077, 214.9008457440070003 ) ) ;
#29041 = CARTESIAN_POINT ( 'NONE',  ( 2.622430729443033126, 1523.621879633029039, 242.1535192357228823 ) ) ;
#29042 = ORIENTED_EDGE ( 'NONE', *, *, #53428, .F. ) ;
#29043 = CARTESIAN_POINT ( 'NONE',  ( -17.43298349350000009, 1417.731752926339823, 206.9848508551290251 ) ) ;
#29044 = CARTESIAN_POINT ( 'NONE',  ( 2.792568477009999661, 1462.433237919889962, 228.6456570646990087 ) ) ;
#29045 = CARTESIAN_POINT ( 'NONE',  ( 17.07488731192356823, 1517.051704408389924, 205.4036014788801481 ) ) ;
#29046 = EDGE_CURVE ( 'NONE', #44418, #9574, #102896, .T. ) ;
#29047 = CARTESIAN_POINT ( 'NONE',  ( 3.793219999985080193, 1517.051709179919953, 202.4207530290020145 ) ) ;
#29048 = CARTESIAN_POINT ( 'NONE',  ( -38.76639204100970204, 1448.036160168320066, 136.4890662579730076 ) ) ;
#29049 = CARTESIAN_POINT ( 'NONE',  ( 11.60004869885002776, 1425.287569105003968, 138.0581718968657583 ) ) ;
#29050 = CYLINDRICAL_SURFACE ( 'NONE', #47828, 1.999999999999999556 ) ;
#29051 = CARTESIAN_POINT ( 'NONE',  ( -1.756474080180989938, 1451.931903963289869, 184.1876047667690273 ) ) ;
#29052 = CARTESIAN_POINT ( 'NONE',  ( 11.22179870490000120, 1433.227936539949951, 151.5695467236979823 ) ) ;
#29053 = DIRECTION ( 'NONE',  ( -0.5518846470010263516, -0.8335230848462815700, -0.02574108453214526276 ) ) ;
#29054 = CARTESIAN_POINT ( 'NONE',  ( -17.22540062639860281, 1409.514585605769980, 195.8673745312759991 ) ) ;
#29055 = CARTESIAN_POINT ( 'NONE',  ( -109.3419108030000046, 1385.202749062920020, 297.1491777238589407 ) ) ;
#29056 = CARTESIAN_POINT ( 'NONE',  ( 11.35984264028680002, 1500.240320957290123, 205.8139343689259988 ) ) ;
#29057 = EDGE_LOOP ( 'NONE', ( #34376, #103613, #34651, #24997 ) ) ;
#29058 = EDGE_CURVE ( 'NONE', #108309, #9292, #61798, .T. ) ;
#29059 = CARTESIAN_POINT ( 'NONE',  ( -1.600048698852036821, 1411.254281879943164, 134.0999999980979851 ) ) ;
#29060 = CARTESIAN_POINT ( 'NONE',  ( 12.53380498098208840, 1442.773887284840384, 206.9039879563480326 ) ) ;
#29061 = DIRECTION ( 'NONE',  ( 0.6709778558543786353, 0.000000000000000000, 0.7414773880254614813 ) ) ;
#29062 = CARTESIAN_POINT ( 'NONE',  ( -0.9617952840779990797, 1442.613780569990013, 200.2933273620589887 ) ) ;
#29063 = CARTESIAN_POINT ( 'NONE',  ( -4.980815112767512431, 1491.198183695671787, 188.8376021758186027 ) ) ;
#29064 = EDGE_CURVE ( 'NONE', #60506, #74686, #107669, .T. ) ;
#29065 = CIRCLE ( 'NONE', #23691, 20.82269076393892249 ) ;
#29066 = CARTESIAN_POINT ( 'NONE',  ( -16.45294080079732879, 1420.118435820799732, 208.7595929061371578 ) ) ;
#29067 = CARTESIAN_POINT ( 'NONE',  ( -10.23452338969999964, 1508.269285187629748, 234.6133565388980173 ) ) ;
#29068 = CARTESIAN_POINT ( 'NONE',  ( -23.46329824210609871, 1383.849819444430068, 222.4997480768529954 ) ) ;
#29069 = CARTESIAN_POINT ( 'NONE',  ( 29.00779973304130266, 1526.382868172863937, 200.9494832830834810 ) ) ;
#29070 = CARTESIAN_POINT ( 'NONE',  ( 6.448255093290000239, 1408.606950372430219, 221.0175999117980155 ) ) ;
#29071 = CARTESIAN_POINT ( 'NONE',  ( -7.191383064323740193, 1407.162969927880113, 195.9581075134270236 ) ) ;
#29073 = ORIENTED_EDGE ( 'NONE', *, *, #22093, .F. ) ;
#29072 = CARTESIAN_POINT ( 'NONE',  ( 15.17646693133499980, 1516.904916668740043, 193.1856145293670011 ) ) ;
#29074 = CARTESIAN_POINT ( 'NONE',  ( -1.197747051619999947, 1451.638021728929971, 183.5066748651979935 ) ) ;
#29075 = CARTESIAN_POINT ( 'NONE',  ( -5.973202138170000453, 1382.320070493830144, 217.8378770759090060 ) ) ;
#29076 = CARTESIAN_POINT ( 'NONE',  ( 2.500000000000000000, 1432.302110539269961, 157.4936333739979943 ) ) ;
#29078 = ORIENTED_EDGE ( 'NONE', *, *, #109189, .T. ) ;
#29077 = CARTESIAN_POINT ( 'NONE',  ( -17.94598849933589690, 1415.434635989099888, 208.4606526442179870 ) ) ;
#29079 = CARTESIAN_POINT ( 'NONE',  ( -4.354842003205010137, 1481.954780407009821, 231.1149995741479870 ) ) ;
#29080 = ORIENTED_EDGE ( 'NONE', *, *, #101450, .F. ) ;
#29081 = CARTESIAN_POINT ( 'NONE',  ( -10.51871147594740208, 1389.041396549049978, 216.3808038717850195 ) ) ;
#29082 = CARTESIAN_POINT ( 'NONE',  ( -18.05542495199999919, 1416.825784011830137, 209.4840452931180153 ) ) ;
#29083 = CARTESIAN_POINT ( 'NONE',  ( 11.47918630980880472, 1425.866204196556282, 139.0913388880763364 ) ) ;
#29084 = CARTESIAN_POINT ( 'NONE',  ( -2.980426153849875082, 1368.816447224659214, 210.5740313466029647 ) ) ;
#29085 = CARTESIAN_POINT ( 'NONE',  ( -0.2725765502280009800, 1430.103961438589977, 217.4715266419189845 ) ) ;
#29086 = CARTESIAN_POINT ( 'NONE',  ( -10.19055345377419997, 1472.389342895980008, 207.1730495706439967 ) ) ;
#29087 = CARTESIAN_POINT ( 'NONE',  ( 13.33898638527650071, 1409.378868052919870, 215.8521671009030172 ) ) ;
#29088 = CARTESIAN_POINT ( 'NONE',  ( -7.966184197910229692, 1384.910162465379926, 199.4893208852380155 ) ) ;
#29089 = CARTESIAN_POINT ( 'NONE',  ( -91.21746417506450655, 1385.196499901840070, 293.2697873285799801 ) ) ;
#29090 = CARTESIAN_POINT ( 'NONE',  ( -19.40739355430000046, 1478.163464013930025, 190.3421420625980147 ) ) ;
#29091 = CARTESIAN_POINT ( 'NONE',  ( -17.17241001986462123, 1518.913060387330006, 238.6251415217917895 ) ) ;
#29092 = CARTESIAN_POINT ( 'NONE',  ( 11.28832168721960016, 1491.057081966879878, 207.3180782202140051 ) ) ;
#29093 = EDGE_LOOP ( 'NONE', ( #35926, #85297, #4340, #28626 ) ) ;
#29094 = VERTEX_POINT ( 'NONE', #107082 ) ;
#29095 = CARTESIAN_POINT ( 'NONE',  ( -6.827653043921440457, 1508.551704612109916, 215.5772713760989916 ) ) ;
#29096 = CARTESIAN_POINT ( 'NONE',  ( -2.663421700517105251, 1419.688210328091600, 137.0999999980980135 ) ) ;
#29097 = CARTESIAN_POINT ( 'NONE',  ( -3.049988319169830042, 1495.700618439620030, 197.1733382635540011 ) ) ;
#29098 = CARTESIAN_POINT ( 'NONE',  ( 35.04542388930794772, 1457.725280349715376, 269.5321273768489618 ) ) ;
#29099 = CARTESIAN_POINT ( 'NONE',  ( -22.70509189929999749, 1409.705932116229860, 208.9454376012710100 ) ) ;
#29100 = CARTESIAN_POINT ( 'NONE',  ( -0.06016800169540000021, 1397.283812744130046, 222.0600360894979701 ) ) ;
#29101 = CARTESIAN_POINT ( 'NONE',  ( 31.12456774391176850, 1525.960063244516959, 201.1524202391561857 ) ) ;
#29102 = CARTESIAN_POINT ( 'NONE',  ( -0.1656437318690000271, 1467.449396149929953, 182.5917868815979830 ) ) ;
#29103 = CARTESIAN_POINT ( 'NONE',  ( -11.74749358745221173, 1366.026922449215363, 208.3718459617010978 ) ) ;
#29104 = CARTESIAN_POINT ( 'NONE',  ( -25.76949925306854894, 1436.653851094284846, 137.0767669179255677 ) ) ;
#29105 = CARTESIAN_POINT ( 'NONE',  ( 0.7352271172030020452, 1516.963431999339946, 207.4067364850470199 ) ) ;
#29106 = CARTESIAN_POINT ( 'NONE',  ( -13.09695741303050021, 1435.388910325369807, 150.3946318658950361 ) ) ;
#29107 = CARTESIAN_POINT ( 'NONE',  ( 31.12456774391179692, 1525.960063244516959, 201.1524202391561573 ) ) ;
#29108 = CARTESIAN_POINT ( 'NONE',  ( 0.5623041189709999665, 1416.835809767730098, 190.4756568789979951 ) ) ;
#29109 = CYLINDRICAL_SURFACE ( 'NONE', #75141, 23.99999999999999289 ) ;
#29110 = CARTESIAN_POINT ( 'NONE',  ( -7.799115399243870428, 1493.006526667940079, 207.9966609151059913 ) ) ;
#29111 = CARTESIAN_POINT ( 'NONE',  ( 41.24981031477440041, 1444.146950527760055, 136.6647296086840129 ) ) ;
#29112 = EDGE_LOOP ( 'NONE', ( #86214, #74223, #52965, #77838 ) ) ;
#29113 = CARTESIAN_POINT ( 'NONE',  ( 21.01922275720000144, 1409.015071317029879, 267.0603661001979958 ) ) ;
#29114 = CARTESIAN_POINT ( 'NONE',  ( -26.64485081080000128, 1469.250187273330084, 209.1448408980039915 ) ) ;
#29116 = CARTESIAN_POINT ( 'NONE',  ( -16.87240953879999950, 1409.502257911630068, 196.1298159851979790 ) ) ;
#29115 = CARTESIAN_POINT ( 'NONE',  ( -10.32454341532539921, 1425.433986580120063, 91.15122188942740422 ) ) ;
#29117 =( BOUNDED_CURVE ( )  B_SPLINE_CURVE ( 3, ( #78959, #71125, #60502, #36380 ),
 .UNSPECIFIED., .F., .F. ) 
 B_SPLINE_CURVE_WITH_KNOTS ( ( 4, 4 ),
 ( 4.156210927873500438, 5.268567114269190554 ),
 .UNSPECIFIED. ) 
 CURVE ( )  GEOMETRIC_REPRESENTATION_ITEM ( )  RATIONAL_B_SPLINE_CURVE ( ( 1.000000000000000000, 0.8995193748706308279, 0.8995193748706308279, 1.000000000000000000 ) ) 
 REPRESENTATION_ITEM ( '' )  );
#29118 = CARTESIAN_POINT ( 'NONE',  ( -35.38895424947720159, 1419.603261908680224, 269.8627654472495578 ) ) ;
#29119 = CARTESIAN_POINT ( 'NONE',  ( -36.81312562770000341, 1440.913060390769942, 254.5659314719980273 ) ) ;
#29120 = CARTESIAN_POINT ( 'NONE',  ( 2.033801735519999987, 1486.167426692489926, 219.8516060156989909 ) ) ;
#29121 = CARTESIAN_POINT ( 'NONE',  ( 11.26937793039999924, 1478.652698499990038, 205.8601898034189901 ) ) ;
#29122 = CARTESIAN_POINT ( 'NONE',  ( 33.54167281650000376, 1451.588757459429871, 135.5984676536979805 ) ) ;
#29123 = ORIENTED_EDGE ( 'NONE', *, *, #15837, .T. ) ;
#29124 = CARTESIAN_POINT ( 'NONE',  ( 9.796230887720000169, 1493.843361169789887, 216.7872332751290116 ) ) ;
#29125 = CARTESIAN_POINT ( 'NONE',  ( 13.16131580973219428, 1513.520094851659223, 225.9095696691143473 ) ) ;
#29126 = CARTESIAN_POINT ( 'NONE',  ( 14.17717777510000055, 1509.408138344429972, 234.9453854129980073 ) ) ;
#29127 = EDGE_LOOP ( 'NONE', ( #8512, #72686, #104754, #91428 ) ) ;
#29128 = ORIENTED_EDGE ( 'NONE', *, *, #29742, .F. ) ;
#29129 = CARTESIAN_POINT ( 'NONE',  ( 29.00779973304137371, 1526.382868172863937, 217.2942086403122914 ) ) ;
#29130 = CARTESIAN_POINT ( 'NONE',  ( 6.434481945890000887, 1424.403579311469912, 194.2120374376990242 ) ) ;
#29131 = ORIENTED_EDGE ( 'NONE', *, *, #51936, .T. ) ;
#29132 = CARTESIAN_POINT ( 'NONE',  ( 0.09694917001379999011, 1417.474897329329906, 184.6760764755979949 ) ) ;
#29133 = FACE_OUTER_BOUND ( 'NONE', #50682, .T. ) ;
#29134 = CARTESIAN_POINT ( 'NONE',  ( 0.3980295580039999725, 1450.899160888880260, 181.9202001828980144 ) ) ;
#29135 = CARTESIAN_POINT ( 'NONE',  ( -9.606425101199999261, 1479.765168659229857, 233.3218314666980291 ) ) ;
#29136 = DIRECTION ( 'NONE',  ( 1.755985294532469921E-16, -1.000000000000000000, 1.338183447452831989E-16 ) ) ;
#29137 = EDGE_LOOP ( 'NONE', ( #35531, #65068, #30212, #35840 ) ) ;
#29138 = CARTESIAN_POINT ( 'NONE',  ( 45.67158527630730447, 1440.912968828189832, 266.1883948345449653 ) ) ;
#29139 = B_SPLINE_CURVE_WITH_KNOTS ( 'NONE', 3,
 ( #102492, #58316, #25782, #41512, #8435, #109815, #15715, #76211, #69, #77322, #83492, #24666, #84050, #110356, #85700, #25226, #40949, #8996, #92438, #24126, #32558, #43167, #34752, #109274, #7889, #59429, #92996, #94657, #34201, #60535, #26338, #59980, #33633, #42060, #94098, #68940, #101938, #16272, #49916, #103041, #16814, #75126, #51014, #17369, #50474, #49363, #84598, #7349, #6788, #66734 ),
 .UNSPECIFIED., .F., .F.,
 ( 4, 2, 2, 1, 1, 2, 2, 2, 2, 1, 1, 1, 2, 2, 2, 2, 1, 1, 1, 2, 2, 2, 2, 1, 1, 1, 1, 2, 2, 2, 4 ),
 ( 0.000000000000000000, 0.1249999999980411503, 0.1874999999970687059, 0.2187499999965762942, 0.2343749999963234409, 0.2421874999961906860, 0.2499999999960579311, 0.3749999999936606265, 0.4374999999924693017, 0.4687499999918546822, 0.4843749999915473725, 0.4921874999913936621, 0.4960937499913433690, 0.4999999999912930204, 0.6249999999905073711, 0.6874999999901078018, 0.7187499999898824266, 0.7343749999897392078, 0.7421874999897040137, 0.7460937499896861391, 0.7499999999896681535, 0.8124999999891825420, 0.8437499999888987690, 0.8593749999887184687, 0.8671874999885907931, 0.8710937499885216262, 0.8730468749884923163, 0.8740234374885097468, 0.8749999999885270663, 0.9374999999942634776, 1.000000000000000000 ),
 .UNSPECIFIED. ) ;
#29140 = CARTESIAN_POINT ( 'NONE',  ( -12.87618670773889917, 1416.835419214280137, 221.9337012713420165 ) ) ;
#29141 = CARTESIAN_POINT ( 'NONE',  ( 15.30113400989999839, 1507.624001478829996, 226.2897674745979941 ) ) ;
#29142 = ORIENTED_EDGE ( 'NONE', *, *, #31676, .T. ) ;
#29143 = CARTESIAN_POINT ( 'NONE',  ( -7.720650173434999708, 1516.977993847330026, 203.3422188780170075 ) ) ;
#29144 = ORIENTED_EDGE ( 'NONE', *, *, #45494, .T. ) ;
#29145 = CARTESIAN_POINT ( 'NONE',  ( 11.86473597889290055, 1432.240644767480035, 149.9815416248509905 ) ) ;
#29146 = ADVANCED_FACE ( 'NONE', ( #89184 ), #77981, .F. ) ;
#29147 = CARTESIAN_POINT ( 'NONE',  ( 12.85619364388517738, 1444.956372886574400, 186.6503089507870357 ) ) ;
#29148 = ORIENTED_EDGE ( 'NONE', *, *, #74314, .T. ) ;
#29149 = EDGE_LOOP ( 'NONE', ( #14804, #48563, #62722, #61911 ) ) ;
#29150 = CARTESIAN_POINT ( 'NONE',  ( 2.737416067801661690, 1524.382868172804365, 176.6378340846514448 ) ) ;
#29151 = EDGE_CURVE ( 'NONE', #21797, #12639, #82441, .T. ) ;
#29152 = CARTESIAN_POINT ( 'NONE',  ( -3.225889381169420034, 1508.257277731970134, 220.7239406431660029 ) ) ;
#29153 = CARTESIAN_POINT ( 'NONE',  ( 18.29188182340000068, 1431.768652859389704, 209.1218459616989946 ) ) ;
#29154 = CARTESIAN_POINT ( 'NONE',  ( -8.425552351598220469, 1471.460212197980127, 214.8702615395930025 ) ) ;
#29155 = CARTESIAN_POINT ( 'NONE',  ( 23.20970012627410028, 1452.102559799250002, 138.3498196778160150 ) ) ;
#29156 = CARTESIAN_POINT ( 'NONE',  ( 0.4790140997571979975, 1409.206633244769819, 270.3713656712309898 ) ) ;
#29157 = CARTESIAN_POINT ( 'NONE',  ( -2.712002233883790137, 1476.204657457879875, 220.2613469579490015 ) ) ;
#29158 = CARTESIAN_POINT ( 'NONE',  ( 11.05525581825247450, 1433.694738207780119, 151.7203265431317618 ) ) ;
#29159 = CARTESIAN_POINT ( 'NONE',  ( -10.97749909317680128, 1432.820767003169749, 151.7697165876629981 ) ) ;
#29160 = CARTESIAN_POINT ( 'NONE',  ( 0.03267392400940041103, 1410.103089868323195, 233.2006946390937969 ) ) ;
#29162 = CARTESIAN_POINT ( 'NONE',  ( -105.9154581355609963, 1391.837543591110034, 304.8725143098620265 ) ) ;
#29161 = CARTESIAN_POINT ( 'NONE',  ( -12.72512470610000079, 1502.960342028389960, 208.6669139330979874 ) ) ;
#29163 = CARTESIAN_POINT ( 'NONE',  ( -67.60933340036338279, 1379.747570940400010, 278.8523720605941207 ) ) ;
#29164 = CARTESIAN_POINT ( 'NONE',  ( -25.32400484384510264, 1509.734017743870027, 222.9228364901310044 ) ) ;
#29165 = CARTESIAN_POINT ( 'NONE',  ( -6.610870935635000833, 1511.929989569670170, 201.7390943842370064 ) ) ;
#29166 = ORIENTED_EDGE ( 'NONE', *, *, #25595, .T. ) ;
#29167 = CARTESIAN_POINT ( 'NONE',  ( 19.47651264659999626, 1426.266543404630283, 243.9198229294980251 ) ) ;
#29168 = CARTESIAN_POINT ( 'NONE',  ( 18.70459388984919968, 1509.566239199539950, 186.5372755781170042 ) ) ;
#29169 = CARTESIAN_POINT ( 'NONE',  ( -77.05697207116840275, 1385.001984995040175, 301.7532523806860354 ) ) ;
#29170 = B_SPLINE_CURVE_WITH_KNOTS ( 'NONE', 3,
 ( #58269, #66681, #93495, #67775, #75628, #76708, #49868, #94052 ),
 .UNSPECIFIED., .F., .F.,
 ( 4, 2, 2, 4 ),
 ( 0.000000000000000000, 0.001073044933456180836, 0.001609567400184301177, 0.002146089866912421519 ),
 .UNSPECIFIED. ) ;
#29171 = EDGE_CURVE ( 'NONE', #84750, #78311, #60883, .T. ) ;
#29172 = CARTESIAN_POINT ( 'NONE',  ( -8.888506772567941638, 1385.313486035710184, 218.6606744470870183 ) ) ;
#29173 = CARTESIAN_POINT ( 'NONE',  ( 0.4151546846821903003, 1511.187213306747708, 175.3106345060153046 ) ) ;
#29174 = CARTESIAN_POINT ( 'NONE',  ( -15.10325504049999878, 1415.737031090589880, 211.5641457255090359 ) ) ;
#29176 = VERTEX_POINT ( 'NONE', #51044 ) ;
#29175 = DIRECTION ( 'NONE',  ( -1.836970198721029688E-16, -1.000000000000000000, 0.000000000000000000 ) ) ;
#29177 = CARTESIAN_POINT ( 'NONE',  ( 17.40764061960000220, 1414.996442553730049, 210.6782162702180017 ) ) ;
#29178 = CARTESIAN_POINT ( 'NONE',  ( -24.61293842550000122, 1444.770194088929884, 210.8869350105979947 ) ) ;
#29179 = CARTESIAN_POINT ( 'NONE',  ( -1.194091358764769906, 1450.771796404168981, 154.2531665394261609 ) ) ;
#29180 = CARTESIAN_POINT ( 'NONE',  ( -1.189564560608550092, 1429.854023961810071, 199.8020812351830102 ) ) ;
#29181 = CARTESIAN_POINT ( 'NONE',  ( 12.73246619883500053, 1512.053076656670100, 224.9511024890669830 ) ) ;
#29182 = CARTESIAN_POINT ( 'NONE',  ( 5.363491954609552970, 1422.300497992083137, 141.6191263096993396 ) ) ;
#29183 = CARTESIAN_POINT ( 'NONE',  ( 19.65254182433579899, 1509.729709204669916, 232.1452871772020217 ) ) ;
#29184 = CARTESIAN_POINT ( 'NONE',  ( -41.49257164404139786, 1443.691024955536477, 136.5669757872581442 ) ) ;
#29185 = CARTESIAN_POINT ( 'NONE',  ( -2.500000000000000000, 1432.302173844710069, 157.4936352153980010 ) ) ;
#29186 = CARTESIAN_POINT ( 'NONE',  ( 15.55932329569999872, 1410.406700292830010, 227.1523413082980198 ) ) ;
#29187 = CARTESIAN_POINT ( 'NONE',  ( 9.837386292569160418, 1469.761137999260200, 211.2461267937810305 ) ) ;
#29188 = CARTESIAN_POINT ( 'NONE',  ( 41.66134420550000073, 1443.796851579070108, 135.6885409488979803 ) ) ;
#29189 = CARTESIAN_POINT ( 'NONE',  ( 4.026614479655000522, 1516.699825673279975, 207.4075116849170115 ) ) ;
#29190 = CARTESIAN_POINT ( 'NONE',  ( 45.44661339499999997, 1436.958365765089866, 268.9799159559980239 ) ) ;
#29191 = CARTESIAN_POINT ( 'NONE',  ( -18.09603717179999904, 1409.709851216229936, 223.5038430802979974 ) ) ;
#29192 = EDGE_CURVE ( 'NONE', #52345, #36240, #108926, .T. ) ;
#29193 = CARTESIAN_POINT ( 'NONE',  ( 16.63847852929999860, 1435.207672684450017, 147.6320463620980092 ) ) ;
#29194 = CARTESIAN_POINT ( 'NONE',  ( 20.03220479750000038, 1469.158896213129992, 192.0694551358980107 ) ) ;
#29195 = FACE_OUTER_BOUND ( 'NONE', #58689, .T. ) ;
#29196 = CARTESIAN_POINT ( 'NONE',  ( -12.26057121044589948, 1378.259448421470097, 207.8534500484209957 ) ) ;
#29197 = CARTESIAN_POINT ( 'NONE',  ( -16.78053953839999934, 1420.867358303729816, 226.9349730632980311 ) ) ;
#29198 = CARTESIAN_POINT ( 'NONE',  ( -14.49162069865310087, 1417.292349856110150, 203.2575443744490258 ) ) ;
#29199 = CARTESIAN_POINT ( 'NONE',  ( -35.96042261120520322, 1435.915483823489922, 135.4632522523019986 ) ) ;
#29200 = EDGE_CURVE ( 'NONE', #72956, #323, #59485, .T. ) ;
#29201 = DIRECTION ( 'NONE',  ( 0.9455185755993178454, 0.000000000000000000, -0.3255681544571539243 ) ) ;
#29202 = CARTESIAN_POINT ( 'NONE',  ( -13.31488284758549945, 1407.448340439549838, 207.9555150571470108 ) ) ;
#29203 = CARTESIAN_POINT ( 'NONE',  ( 2.918143513847768445E-16, 1426.814114634534008, 137.0999999980979851 ) ) ;
#29204 = CARTESIAN_POINT ( 'NONE',  ( -4.261736551909999449, 1515.372048949689997, 207.2788837304390199 ) ) ;
#29205 = CARTESIAN_POINT ( 'NONE',  ( -7.671317258861270361, 1383.657626917639845, 218.9493643440779920 ) ) ;
#29206 = CARTESIAN_POINT ( 'NONE',  ( 11.94165044080000015, 1433.614891514819874, 146.7587909720979837 ) ) ;
#29207 = CARTESIAN_POINT ( 'NONE',  ( -34.31734398647500228, 1435.703512753839959, 134.0999999980490145 ) ) ;
#29208 = CARTESIAN_POINT ( 'NONE',  ( -0.6104134479315243000, 1418.823153084925707, 184.7568843877850782 ) ) ;
#29209 = ORIENTED_EDGE ( 'NONE', *, *, #21892, .T. ) ;
#29210 = CARTESIAN_POINT ( 'NONE',  ( 6.187521057617754394, 1510.844697586414213, 216.5810360690583138 ) ) ;
#29211 = CARTESIAN_POINT ( 'NONE',  ( 27.13956170239999821, 1438.563708552820117, 136.9826111156980062 ) ) ;
#29212 = FACE_OUTER_BOUND ( 'NONE', #38640, .T. ) ;
#29213 = B_SPLINE_CURVE_WITH_KNOTS ( 'NONE', 3,
 ( #27699, #87049, #1972, #60210, #102720, #36652, #87618, #26014, #17607, #34988, #19836, #43407, #70849, #51807, #95456, #94329, #35539, #61885, #52917, #85949, #69168, #44509, #104958, #103853, #26581, #77558, #19271, #862, #104405, #18177, #103273, #60778, #86493, #43954, #28248, #52373, #78096, #45079, #10906, #96001, #70294, #18721, #62438, #2529, #61338, #10337, #78656, #36108, #53474, #96564, #79222, #54041, #88170, #56764, #20379, #39401, #47807, #107709, #37759, #30994, #22011, #106602, #21470, #4163, #65170, #3080, #13619, #80312, #56207, #28807, #11458, #107151, #20928, #81943, #5246, #98198, #37208, #72472, #97658, #80862, #55134, #73579, #38290, #99284, #22560, #90339, #89801, #45634, #79774, #88719, #29887, #89254, #71401, #63005, #12550, #81382, #29341, #55680, #12001, #105517, #73015, #64079, #97113, #54584, #46183, #3628, #47258, #13072, #4696, #46729, #71951, #106063, #63542, #38837, #30445, #64630, #98750, #48371, #99841, #84148, #67935, #109377, #75225, #90902, #14741, #83057, #7449, #76312, #6350, #100406, #92544, #100938, #66831, #67385, #32102, #83592, #40498, #24770, #109914, #75766, #32654, #110463, #57337, #6891, #23689, #82514, #108254, #66289, #50016, #108809, #24234, #91463, #50569, #41612, #41047, #101482, #58418, #15812, #74124, #33194, #33740, #58966, #57874, #23132, #102041, #48930, #16371, #74675, #92006, #93099, #5813, #15278, #84695, #25328, #14185, #39952, #65720, #49471, #7994, #42160, #31543, #44944, #94763, #59524, #18039, #36517, #35410, #61745, #104273, #9105, #51671, #68484, #723, #78526, #52232, #103144, #85244, #95321, #8540, #61207, #87485, #86360, #93636, #34302, #86915, #52778, #77963, #1837, #35971, #95867, #18583, #10206, #16916, #103716, #34853, #19133, #51120, #44382, #10772, #69598, #79091, #76869, #27561, #70162, #17470, #182, #2399, #27017, #53337, #1271, #70710, #43273, #104824, #42716, #102585, #43817, #25883, #60083, #77418, #94199, #85808, #69042, #26444, #60639, #9642, #20794, #54451, #62875, #64497, #47129, #11328, #38705, #45500, #73435, #12949, #37618, #98613, #21876, #4035, #19706, #89119, #38163, #72344, #4571, #80173, #54996, #88587, #72881, #81256, #107018, #80727, #30307, #106473, #29758, #63948, #98061, #3490, #56075, #12408, #105382, #96428, #28670, #90202, #89663, #46592, #13486, #21333, #55539, #79642, #47676, #81805, #62301, #96987, #20250, #5106, #53909, #39261, #29219, #28110, #88044, #2944 ),
 .UNSPECIFIED., .F., .F.,
 ( 4, 3, 3, 3, 3, 3, 3, 3, 3, 3, 3, 3, 3, 3, 3, 3, 3, 3, 3, 3, 3, 3, 3, 3, 3, 3, 3, 3, 3, 3, 3, 3, 3, 3, 3, 3, 3, 3, 3, 3, 3, 3, 3, 3, 3, 3, 3, 3, 3, 3, 3, 3, 3, 3, 3, 3, 3, 3, 3, 3, 3, 3, 3, 3, 3, 3, 3, 3, 3, 3, 3, 3, 3, 3, 3, 3, 3, 3, 3, 3, 3, 3, 3, 3, 3, 3, 3, 3, 3, 3, 3, 3, 3, 3, 3, 3, 3, 3, 3, 3, 4 ),
 ( 9.498561704960000185, 10.82581271786099997, 11.98157754783849960, 13.07709420200399997, 14.12652422663150098, 15.12593959681159994, 15.39383910900589925, 16.42924805362760310, 17.50909810246649911, 18.64760857678350092, 19.92915870810679735, 21.39300856659529870, 23.20497190757799899, 24.59301561497350264, 25.84108368276750056, 26.97655774348510249, 27.58084801744849912, 28.68885941005749984, 29.82533532047489899, 30.99492639834819840, 32.20374463193149950, 33.48731841844190171, 34.83172918346869551, 36.25101147155060488, 37.79185539324890897, 39.35626037121420495, 40.84191036018259524, 41.39509552359669442, 43.74764748933439762, 46.15588617650058723, 48.41852181316069448, 50.55859315911320095, 52.47366333285489759, 54.31027375113220046, 56.08354471098009242, 57.80421286508820344, 59.48018875923999360, 61.09911270707588926, 62.69052795272030210, 64.24295526564009151, 65.53909258078100208, 67.16858239626179738, 68.87693503373300530, 70.69370224108921263, 72.67760720951280007, 75.06533303647849209, 77.83954810070869712, 79.89814551137540377, 81.75296411951019593, 83.48762472816490288, 85.13822779119200845, 86.69705361584379943, 88.21559619941889707, 89.68066952009159820, 90.91108773676960197, 92.82807407335819505, 94.79416735270849870, 96.79315978722270586, 98.79695866710609664, 100.7748251777260009, 102.7057122494059911, 104.5720934641509956, 106.3681167381800066, 108.1183885991049891, 109.8272200050709984, 111.4986773274300020, 113.1197408288939954, 114.7157798799740078, 116.2752876061319967, 117.6367619673630003, 119.0756917262879995, 120.5569498931889854, 122.0758578800959810, 123.5880462789450149, 125.0719021203930055, 126.5156553974589997, 127.9164406824140201, 129.2579234214590258, 130.5686603755449937, 131.8387902540730181, 132.4493970714150066, 133.5476357628679978, 134.6466073012290110, 135.7458795129909959, 136.8796545122989983, 137.9777618726589878, 139.0747495574819936, 140.1702608175249907, 141.2639536178200217, 142.3544029523149845, 143.4426570491259838, 144.5274464010880138, 144.8160795074579994, 146.5556413704150032, 148.3807959781919976, 150.2772506426800021, 152.1535931427380035, 153.9584735936539914, 155.6870227822439858, 157.3233957306069897, 157.6324468028149965 ),
 .UNSPECIFIED. ) ;
#29214 = CARTESIAN_POINT ( 'NONE',  ( 17.74170650421104511, 1432.761001460916759, 213.7496100754616180 ) ) ;
#29215 = CARTESIAN_POINT ( 'NONE',  ( -31.50880186010000017, 1466.258756145929965, 266.5723332967979786 ) ) ;
#29216 = CARTESIAN_POINT ( 'NONE',  ( -29.91204167771525135, 1525.042412244735488, 196.0616339290309611 ) ) ;
#29217 = CARTESIAN_POINT ( 'NONE',  ( -19.79380256296796858, 1500.877691764588917, 189.1734504439409363 ) ) ;
#29218 = CARTESIAN_POINT ( 'NONE',  ( -26.86204968970000095, 1508.007394745729925, 212.0120970167880046 ) ) ;
#29219 = CARTESIAN_POINT ( 'NONE',  ( -108.7880151385730017, 1384.583904816670156, 311.2495016965060017 ) ) ;
#29220 = B_SPLINE_SURFACE_WITH_KNOTS ( 'NONE', 4, 5, ( 
 ( #75433, #28584, #65932, #62785, #105856, #100054 ),
 ( #97443, #96900, #54367, #74876, #54907, #39609 ),
 ( #11782, #29134, #57533, #90549, #91105, #48576 ),
 ( #5449, #91657, #14931, #22769, #48012, #14383 ),
 ( #82150, #107903, #109027, #100599, #45949, #32309 ) ),
 .UNSPECIFIED., .F., .F., .F.,
 ( 5, 5 ),
 ( 6, 6 ),
 ( 7.045302831979999958, 7.554698048799999732 ),
 ( 0.000000000000000000, 2.000000000000000000 ),
 .UNSPECIFIED. ) ;
#29221 = CARTESIAN_POINT ( 'NONE',  ( -32.15488896474609248, 1384.972929923339962, 206.8029585035789921 ) ) ;
#29222 = CARTESIAN_POINT ( 'NONE',  ( -5.513264357029999729, 1374.913060387289988, 214.9370262455390161 ) ) ;
#29223 = CARTESIAN_POINT ( 'NONE',  ( 14.64149002350000117, 1416.824060884929850, 219.7189340838980058 ) ) ;
#29224 = CARTESIAN_POINT ( 'NONE',  ( 14.89301817989999854, 1485.042290100730042, 224.3999831303979988 ) ) ;
#29225 = CARTESIAN_POINT ( 'NONE',  ( 18.02574679518840028, 1424.482682570480165, 224.6196048480980210 ) ) ;
#29227 = VERTEX_POINT ( 'NONE', #16297 ) ;
#29226 = DIRECTION ( 'NONE',  ( -0.7063774289747313251, 0.04540766091858271930, -0.7063774289747313251 ) ) ;
#29228 = DIRECTION ( 'NONE',  ( -0.8775825618903763115, 0.000000000000000000, -0.4794255386041965106 ) ) ;
#29229 = CARTESIAN_POINT ( 'NONE',  ( 5.370527602886283169, 1422.356908813907012, 139.1416118586824666 ) ) ;
#29230 = CARTESIAN_POINT ( 'NONE',  ( 3.099041906601330165, 1369.866330758129379, 210.4936753499222561 ) ) ;
#29231 = CARTESIAN_POINT ( 'NONE',  ( -12.44325168979999852, 1415.996778985530000, 195.0334447333979995 ) ) ;
#29232 = CARTESIAN_POINT ( 'NONE',  ( -2.022208241610000012, 1421.024495610020040, 193.8502730733989949 ) ) ;
#29233 = CARTESIAN_POINT ( 'NONE',  ( 23.11858565820000067, 1409.884865691529967, 211.2355702977880014 ) ) ;
#29234 = DIRECTION ( 'NONE',  ( 0.000000000000000000, 1.000000000000000000, 0.000000000000000000 ) ) ;
#29235 = CARTESIAN_POINT ( 'NONE',  ( 1.046130468810000158, 1463.550315089890091, 230.5479457569989847 ) ) ;
#29236 = DIRECTION ( 'NONE',  ( -0.6736849260863837507, 0.000000000000000000, 0.7390186874254154326 ) ) ;
#29238 = CARTESIAN_POINT ( 'NONE',  ( -10.82018256120000110, 1380.538809929369791, 202.7722443582989911 ) ) ;
#29237 = CARTESIAN_POINT ( 'NONE',  ( 2.880867337579580134, 1368.384084939549894, 207.8228488383560091 ) ) ;
#29239 = CARTESIAN_POINT ( 'NONE',  ( 1.077911720219999925, 1415.753832296730025, 233.1550800001979837 ) ) ;
#29240 = DIRECTION ( 'NONE',  ( 0.000000000000000000, -1.000000000000000000, -0.000000000000000000 ) ) ;
#29241 = CARTESIAN_POINT ( 'NONE',  ( -20.71343476517491311, 1512.187213306747481, 238.3377464195766890 ) ) ;
#29242 = CARTESIAN_POINT ( 'NONE',  ( -22.57618069069999933, 1411.056460445829998, 211.7928261235179832 ) ) ;
#29243 = CARTESIAN_POINT ( 'NONE',  ( -0.6544075182467720131, 1420.442518575000122, 184.0330262823659950 ) ) ;
#29244 = CARTESIAN_POINT ( 'NONE',  ( 3.449777315724999571, 1516.974592746400049, 204.1104779853070283 ) ) ;
#29245 = CARTESIAN_POINT ( 'NONE',  ( -13.34370645066865713, 1422.266645666820523, 196.3187566567426359 ) ) ;
#29246 = CARTESIAN_POINT ( 'NONE',  ( -14.82166838865560088, 1486.064940468489795, 186.2093746475509874 ) ) ;
#29247 = CARTESIAN_POINT ( 'NONE',  ( 7163.889423669126700, 5182.767774292100512, -7818.362407857699509 ) ) ;
#29248 = CARTESIAN_POINT ( 'NONE',  ( -11.07527852154495385, 1422.183102189465899, 210.6367496950426244 ) ) ;
#29250 = ORIENTED_EDGE ( 'NONE', *, *, #27647, .T. ) ;
#29249 = CARTESIAN_POINT ( 'NONE',  ( -67.55991329888020402, 1379.745335248140009, 278.8868931239820199 ) ) ;
#29251 = VERTEX_POINT ( 'NONE', #110385 ) ;
#29252 = CARTESIAN_POINT ( 'NONE',  ( 28.53450901119999727, 1509.594688344129963, 211.3361516935080147 ) ) ;
#29253 = ORIENTED_EDGE ( 'NONE', *, *, #72026, .T. ) ;
#29254 = FACE_OUTER_BOUND ( 'NONE', #24622, .T. ) ;
#29255 = CARTESIAN_POINT ( 'NONE',  ( 1.547463840030000037, 1414.913060387329779, 192.3096136973980208 ) ) ;
#29257 = CARTESIAN_POINT ( 'NONE',  ( 0.8719743115910000286, 1508.600324595230177, 180.4235865536979873 ) ) ;
#29256 = CARTESIAN_POINT ( 'NONE',  ( 15.99649503710709730, 1421.554318619909964, 191.1865063950630201 ) ) ;
#29258 = CARTESIAN_POINT ( 'NONE',  ( 11.96661585360000046, 1440.449248668989867, 150.8629738177980073 ) ) ;
#29259 = CARTESIAN_POINT ( 'NONE',  ( -25.57905335200330299, 1450.800917333740017, 137.0692583773119964 ) ) ;
#29260 = CARTESIAN_POINT ( 'NONE',  ( 4.399927595769999478, 1410.004273022730104, 231.3928942499979939 ) ) ;
#29261 = CARTESIAN_POINT ( 'NONE',  ( 10.24022436676090031, 1482.543054787119900, 212.0614503867469978 ) ) ;
#29262 = CARTESIAN_POINT ( 'NONE',  ( -3.252530653725000054, 1516.827328999679821, 212.0018028951869837 ) ) ;
#29263 = CARTESIAN_POINT ( 'NONE',  ( 40.90250537874639747, 1447.119793117639801, 134.0999999985199906 ) ) ;
#29264 =( BOUNDED_CURVE ( )  B_SPLINE_CURVE ( 3, ( #62542, #45728, #4786, #82042 ),
 .UNSPECIFIED., .F., .T. ) 
 B_SPLINE_CURVE_WITH_KNOTS ( ( 4, 4 ),
 ( 5.921924288096549915, 6.231904421257119964 ),
 .UNSPECIFIED. ) 
 CURVE ( )  GEOMETRIC_REPRESENTATION_ITEM ( )  RATIONAL_B_SPLINE_CURVE ( ( 1.000000000000000000, 0.9920087094985445830, 0.9920087094985445830, 1.000000000000000000 ) ) 
 REPRESENTATION_ITEM ( '' )  );
#29265 = CARTESIAN_POINT ( 'NONE',  ( -20.60448988230000111, 1484.737042837089803, 209.1218459616989946 ) ) ;
#29266 = VERTEX_POINT ( 'NONE', #33663 ) ;
#29267 = CARTESIAN_POINT ( 'NONE',  ( -16.83568192250000095, 1418.884533543920043, 201.2565368162689765 ) ) ;
#29268 = CARTESIAN_POINT ( 'NONE',  ( 10.03186001745409150, 1491.455176020307590, 213.8859670922726650 ) ) ;
#29269 = VERTEX_POINT ( 'NONE', #67856 ) ;
#29270 = ORIENTED_EDGE ( 'NONE', *, *, #7669, .T. ) ;
#29271 = ORIENTED_EDGE ( 'NONE', *, *, #31692, .T. ) ;
#29272 = CARTESIAN_POINT ( 'NONE',  ( -6.402238504554999210, 1513.914017980350081, 216.7093358650170103 ) ) ;
#29273 = CARTESIAN_POINT ( 'NONE',  ( 15.90990511613090241, 1514.921193439799936, 193.9190475034619965 ) ) ;
#29274 = CARTESIAN_POINT ( 'NONE',  ( 7.904476258595151350, 1451.392616462666638, 152.9734174004545366 ) ) ;
#29275 = CARTESIAN_POINT ( 'NONE',  ( -8.298003019930000335, 1384.922753400079955, 218.7035906743590203 ) ) ;
#29276 = CARTESIAN_POINT ( 'NONE',  ( 9.706405685860000077, 1463.133235100189950, 210.3097023741290172 ) ) ;
#29277 = CARTESIAN_POINT ( 'NONE',  ( -17.00854892524643347, 1449.165472411616520, 219.4054542577865163 ) ) ;
#29278 = CARTESIAN_POINT ( 'NONE',  ( -66.36278826096751970, 1379.742732206253777, 275.1173963032269398 ) ) ;
#29279 = CARTESIAN_POINT ( 'NONE',  ( -1.062448666549999921, 1463.820984688390126, 199.3576882633090008 ) ) ;
#29280 = CARTESIAN_POINT ( 'NONE',  ( 1.160958422820000058, 1414.971439108430104, 191.5548729526980196 ) ) ;
#29281 = CARTESIAN_POINT ( 'NONE',  ( -62.52086756535808831, 1384.688842335020126, 249.5288663568049969 ) ) ;
#29282 = ORIENTED_EDGE ( 'NONE', *, *, #87921, .F. ) ;
#29283 = CARTESIAN_POINT ( 'NONE',  ( -2.300729664794999962, 1516.923170579120097, 207.4211391557370234 ) ) ;
#29284 = VERTEX_POINT ( 'NONE', #42636 ) ;
#29285 = CARTESIAN_POINT ( 'NONE',  ( 24.76605716182779915, 1440.913060387330006, 238.3302827077500012 ) ) ;
#29286 = CARTESIAN_POINT ( 'NONE',  ( -13.77714796350000093, 1508.637939676529868, 184.0711857673979921 ) ) ;
#29287 = ORIENTED_EDGE ( 'NONE', *, *, #65339, .T. ) ;
#29288 = FACE_OUTER_BOUND ( 'NONE', #61606, .T. ) ;
#29289 = CARTESIAN_POINT ( 'NONE',  ( -13.97293528600000023, 1409.401006039529875, 191.8161164125979781 ) ) ;
#29290 = CARTESIAN_POINT ( 'NONE',  ( -17.36568713798484609, 1508.455955994650367, 212.8023812719880254 ) ) ;
#29292 = DIRECTION ( 'NONE',  ( 0.8775825618903714265, 0.000000000000000000, -0.4794255386042053368 ) ) ;
#29291 = CARTESIAN_POINT ( 'NONE',  ( -24.41216396249999931, 1440.964695643669984, 212.0310679874179982 ) ) ;
#29293 = CARTESIAN_POINT ( 'NONE',  ( -7.530771855114540614, 1435.872963818640073, 215.3039292562540084 ) ) ;
#29294 = CARTESIAN_POINT ( 'NONE',  ( 0.0002087548573902462442, 1397.282671569474587, 196.2061409705553103 ) ) ;
#29295 = CARTESIAN_POINT ( 'NONE',  ( -12.28708495595255279, 1434.198421465742285, 147.4194680967047475 ) ) ;
#29296 = CARTESIAN_POINT ( 'NONE',  ( -7.617720993269999852, 1508.534261654589955, 219.3295389908989819 ) ) ;
#29298 = CARTESIAN_POINT ( 'NONE',  ( 3.184944912390000216, 1492.459204846589955, 188.3860389383989968 ) ) ;
#29297 = CARTESIAN_POINT ( 'NONE',  ( 2.848137854069999975, 1464.611669510630009, 235.5053002295980207 ) ) ;
#29299 = CARTESIAN_POINT ( 'NONE',  ( -1.124894088365000044, 1517.194816588360027, 216.0733631026070043 ) ) ;
#29300 = CARTESIAN_POINT ( 'NONE',  ( 10.81518794224679958, 1424.921099295370141, 144.1705737284439977 ) ) ;
#29301 = CARTESIAN_POINT ( 'NONE',  ( 5.550449858616669729, 1510.476657126699820, 216.6722583594520017 ) ) ;
#29302 = EDGE_CURVE ( 'NONE', #59762, #81426, #38563, .T. ) ;
#29303 = CARTESIAN_POINT ( 'NONE',  ( 19.13409869423357534, 1443.853562509159246, 213.6555041989591643 ) ) ;
#29304 = CARTESIAN_POINT ( 'NONE',  ( -7.709681306425000713, 1516.559109716219837, 211.9945464874270158 ) ) ;
#29305 = CARTESIAN_POINT ( 'NONE',  ( 3.487592428934999766, 1509.038615934169911, 204.6345961781970004 ) ) ;
#29306 = CARTESIAN_POINT ( 'NONE',  ( -5.315917822019888384, 1420.217656571705220, 137.0999999980980135 ) ) ;
#29308 = ORIENTED_EDGE ( 'NONE', *, *, #5258, .F. ) ;
#29307 = CARTESIAN_POINT ( 'NONE',  ( -106.4403080060000093, 1388.016213653540035, 310.4695424982589884 ) ) ;
#29309 = FACE_OUTER_BOUND ( 'NONE', #86252, .T. ) ;
#29310 = CARTESIAN_POINT ( 'NONE',  ( 29.87497052580000201, 1442.835664583690004, 238.0574391274980144 ) ) ;
#29311 = EDGE_CURVE ( 'NONE', #21912, #110100, #22394, .T. ) ;
#29312 = CARTESIAN_POINT ( 'NONE',  ( -11.28980188229558657, 1489.194859813259427, 213.7481022665220678 ) ) ;
#29313 = CARTESIAN_POINT ( 'NONE',  ( -15.33967589549999921, 1415.677402202029953, 209.0176008730730075 ) ) ;
#29314 = CARTESIAN_POINT ( 'NONE',  ( 1.800869729310000000, 1413.124895085329854, 232.3173401135979930 ) ) ;
#29315 = FACE_OUTER_BOUND ( 'NONE', #110053, .T. ) ;
#29317 = FACE_OUTER_BOUND ( 'NONE', #13957, .T. ) ;
#29316 = CARTESIAN_POINT ( 'NONE',  ( -19.11605526869999849, 1444.805919307749946, 225.6841260797980055 ) ) ;
#29318 = CARTESIAN_POINT ( 'NONE',  ( -9.258624140391589208, 1449.585829297850069, 207.9796510681429709 ) ) ;
#29319 = CARTESIAN_POINT ( 'NONE',  ( -107.2817012039999867, 1380.464637550900079, 309.2662977502590707 ) ) ;
#29320 = ORIENTED_EDGE ( 'NONE', *, *, #110275, .T. ) ;
#29321 = CARTESIAN_POINT ( 'NONE',  ( 3.253462060665000433, 1516.874084700499907, 205.6604858388269861 ) ) ;
#29322 = CARTESIAN_POINT ( 'NONE',  ( 2.101138442839999954, 1406.100891733030039, 269.0439770072979968 ) ) ;
#29323 = CARTESIAN_POINT ( 'NONE',  ( 1.460285906039999970, 1515.203804957989860, 213.4476545592490027 ) ) ;
#29324 = CARTESIAN_POINT ( 'NONE',  ( 44.43457533159219963, 1446.348491390079971, 270.0922382052800117 ) ) ;
#29325 = CARTESIAN_POINT ( 'NONE',  ( 1.662080245303283021, 1464.065906623968203, 199.4475712355095425 ) ) ;
#29326 = DIRECTION ( 'NONE',  ( 0.9149707217702551798, 0.000000000000000000, -0.4035202328300510621 ) ) ;
#29327 = CARTESIAN_POINT ( 'NONE',  ( -9.915381109698630624, 1446.894009479360193, 211.9680447833129904 ) ) ;
#29328 = CARTESIAN_POINT ( 'NONE',  ( 2.531940903048510086E-08, 1457.850589566970029, 229.0733431205499926 ) ) ;
#29329 = CARTESIAN_POINT ( 'NONE',  ( -8.788316527315000570, 1511.741868877540128, 215.3741124244170067 ) ) ;
#29330 = CARTESIAN_POINT ( 'NONE',  ( 0.5709835175930680906, 1450.893121203520195, 154.5155266294819967 ) ) ;
#29331 = CARTESIAN_POINT ( 'NONE',  ( -12.42529224677513078, 1517.051704408389924, 215.5613278979431868 ) ) ;
#29332 = CARTESIAN_POINT ( 'NONE',  ( -1.546867746862319981, 1416.839692133689823, 228.0214409764060122 ) ) ;
#29333 = ORIENTED_EDGE ( 'NONE', *, *, #100041, .F. ) ;
#29334 = CARTESIAN_POINT ( 'NONE',  ( -21.34957048430000270, 1432.854863364579842, 234.3916895436979928 ) ) ;
#29335 = VECTOR ( 'NONE', #100184, 1000.000000000000000 ) ;
#29336 = CARTESIAN_POINT ( 'NONE',  ( 10.10666311268190043, 1469.215464056610017, 203.9609526372169910 ) ) ;
#29337 = CARTESIAN_POINT ( 'NONE',  ( -0.7746087140290000006, 1475.755075091830122, 269.0454657403980150 ) ) ;
#29338 = CARTESIAN_POINT ( 'NONE',  ( 10.77451535478706290, 1424.915582317967164, 138.4825886073255958 ) ) ;
#29339 = CARTESIAN_POINT ( 'NONE',  ( -11.88255532981709450, 1513.001579509954126, 192.5822564612562928 ) ) ;
#29340 = CARTESIAN_POINT ( 'NONE',  ( -17.69507376908103424, 1517.051704408389924, 216.2288492090250998 ) ) ;
#29341 = CARTESIAN_POINT ( 'NONE',  ( -36.72861643521579822, 1384.801874369770076, 236.7485459430360208 ) ) ;
#29342 = AXIS2_PLACEMENT_3D ( 'NONE', #86718, #87847, #29564 ) ;
#29343 = B_SPLINE_SURFACE_WITH_KNOTS ( 'NONE', 5, 5, ( 
 ( #19216, #79724, #87569, #47212, #97613, #29297, #46681, #89753, #4652 ),
 ( #38790, #70798, #63493, #62958, #54539, #64031, #4119, #79176, #97069 ),
 ( #2483, #38244, #55631, #36599, #72966, #88673, #3031, #71350, #20335 ),
 ( #27648, #45582, #37705, #71906, #104910, #72426, #20883, #55080, #106558 ),
 ( #21419, #28198, #19790, #53991, #29845, #88125, #98145, #11414, #105465 ),
 ( #28754, #90291, #57286, #13572, #99233, #83006, #24178, #66784, #108201 ),
 ( #100883, #39903, #32048, #82463, #32607, #40995, #74622, #6836, #90847 ),
 ( #41564, #48322, #56712, #83542, #57826, #65670, #58367, #74072, #84098 ),
 ( #15226, #108756, #5761, #91952, #91414, #47757, #14691, #49962, #92492 ),
 ( #49418, #7399, #5195, #81892, #98703, #48880, #75174, #14132, #65121 ),
 ( #39350, #6298, #40445, #15761, #21962, #31490, #73526, #107104, #109324 ),
 ( #66237, #99788, #23079, #30393, #64584, #56156, #107660, #30946, #100356 ),
 ( #22510, #23644, #109865, #17419, #110408, #59478, #34803, #51617, #9594 ),
 ( #67331, #9049, #68991, #67882, #61153, #101991, #60030, #129, #93589 ),
 ( #68435, #84646, #85752, #25277, #103092, #43222, #35357, #85198, #16865 ) ),
 .UNSPECIFIED., .F., .F., .F.,
 ( 6, 3, 3, 3, 6 ),
 ( 6, 3, 6 ),
 ( 24.26857305089999883, 41.67781792160000265, 49.51652399259999981, 57.35523006350000230, 61.88671852840000298 ),
 ( 0.000000000000000000, 1.000000000000000000, 2.000000000000000000 ),
 .UNSPECIFIED. ) ;
#29344 = CARTESIAN_POINT ( 'NONE',  ( 12.19805618840440076, 1491.617858633879905, 207.5154424382099876 ) ) ;
#29345 = FACE_OUTER_BOUND ( 'NONE', #19616, .T. ) ;
#29346 = CARTESIAN_POINT ( 'NONE',  ( 26.80344781114780162, 1436.440813660759886, 136.7218762079120040 ) ) ;
#29347 = CARTESIAN_POINT ( 'NONE',  ( -10.00562653641270039, 1396.262464565250184, 213.8494479798769703 ) ) ;
#29348 = CARTESIAN_POINT ( 'NONE',  ( -14.50783621480000107, 1422.103482364530009, 228.3959130620980034 ) ) ;
#29349 = CARTESIAN_POINT ( 'NONE',  ( 19.26683521067225868, 1456.110280151028292, 225.0772932314519892 ) ) ;
#29350 = ORIENTED_EDGE ( 'NONE', *, *, #19123, .F. ) ;
#29351 = CARTESIAN_POINT ( 'NONE',  ( -15.70021566718022399, 1414.913060387329779, 204.0157239446980668 ) ) ;
#29352 = CARTESIAN_POINT ( 'NONE',  ( 2.680552910549999890, 1409.943153456129949, 231.6453896010980031 ) ) ;
#29353 = CARTESIAN_POINT ( 'NONE',  ( -3.677613769069999778E-16, 1378.413060387289988, 209.1218459616989946 ) ) ;
#29355 = CARTESIAN_POINT ( 'NONE',  ( -11.35635716866499934, 1512.376261820769969, 192.9173751460670303 ) ) ;
#29354 = CARTESIAN_POINT ( 'NONE',  ( 11.15531093709999944, 1426.887873589030050, 101.9087401586980093 ) ) ;
#29356 = CARTESIAN_POINT ( 'NONE',  ( -16.19086242769280304, 1409.478452467050147, 225.0103265570539861 ) ) ;
#29357 = CARTESIAN_POINT ( 'NONE',  ( -13.51610093808349333, 1442.913060377700731, 205.0760988357353654 ) ) ;
#29358 = CARTESIAN_POINT ( 'NONE',  ( -109.9814841436489985, 1384.590269029640012, 311.4453213042449988 ) ) ;
#29359 = CARTESIAN_POINT ( 'NONE',  ( 7.300163574239999065, 1426.919040555409993, 212.8503364413490146 ) ) ;
#29360 = LINE ( 'NONE', #12021, #94024 ) ;
#29361 = CARTESIAN_POINT ( 'NONE',  ( 1.469929971880000075, 1507.915326702530137, 180.9459708343979969 ) ) ;
#29362 = CARTESIAN_POINT ( 'NONE',  ( 7.572192850525000019, 1511.308638870219966, 206.5572121486769959 ) ) ;
#29363 = CARTESIAN_POINT ( 'NONE',  ( -42.29523164129999202, 1376.793217291669862, 233.4051811251589754 ) ) ;
#29364 = CARTESIAN_POINT ( 'NONE',  ( 5.951028257965643498, 1367.294630164640239, 210.6218459617142003 ) ) ;
#29366 = ORIENTED_EDGE ( 'NONE', *, *, #33719, .F. ) ;
#29365 = CARTESIAN_POINT ( 'NONE',  ( 16.41723189518601700, 1410.863437090559046, 191.6246442130024263 ) ) ;
#29367 = B_SPLINE_CURVE_WITH_KNOTS ( 'NONE', 3,
 ( #77125, #91287, #95017, #99667, #48758, #86061, #43521, #42397, #60891, #8784, #52479, #18285, #6176, #68733, #59772, #8230, #86607, #44070, #40329 ),
 .UNSPECIFIED., .F., .F.,
 ( 4, 2, 2, 2, 1, 1, 1, 2, 2, 2, 4 ),
 ( 0.000000000000000000, 0.2499999999994982902, 0.3749999999992473243, 0.4374999999991323052, 0.4687499999990772936, 0.4843749999990471511, 0.4921874999990320521, 0.4960937499990347166, 0.4999999999990373256, 0.7499999999995186073, 1.000000000000000000 ),
 .UNSPECIFIED. ) ;
#29368 = ORIENTED_EDGE ( 'NONE', *, *, #109927, .T. ) ;
#29369 = CARTESIAN_POINT ( 'NONE',  ( -13.73335268700000000, 1441.669543367469942, 188.5645195036979942 ) ) ;
#29370 = CARTESIAN_POINT ( 'NONE',  ( 1.455060923660010053, 1507.152178126010085, 236.7684687559849976 ) ) ;
#29371 = LINE ( 'NONE', #55716, #47576 ) ;
#29372 = CARTESIAN_POINT ( 'NONE',  ( -7.735039587165000619, 1511.353635254350138, 212.6038253893969738 ) ) ;
#29374 = CARTESIAN_POINT ( 'NONE',  ( -21.52163278259530088, 1505.754112708010098, 209.2478060993030056 ) ) ;
#29373 = CARTESIAN_POINT ( 'NONE',  ( -8.293045909599999987, 1384.759859680410045, 218.7022228219589977 ) ) ;
#29375 = CARTESIAN_POINT ( 'NONE',  ( 6.757182283909999754, 1429.763710591829977, 186.1422234325980014 ) ) ;
#29376 =( NAMED_UNIT ( * ) PLANE_ANGLE_UNIT ( ) SI_UNIT ( $, .RADIAN. ) );
#29377 = CARTESIAN_POINT ( 'NONE',  ( -40.70526567241159910, 1444.199263182009872, 137.0833905334800136 ) ) ;
#29378 = CARTESIAN_POINT ( 'NONE',  ( 40.24340914364780275, 1439.067764445909916, 135.6665089828919974 ) ) ;
#29379 = CARTESIAN_POINT ( 'NONE',  ( 30.84775898762307023, 1435.574754682624643, 135.1614303800634502 ) ) ;
#29380 = CARTESIAN_POINT ( 'NONE',  ( 0.7133824534919999127, 1416.822690122329959, 190.3253679635979836 ) ) ;
#29381 = CARTESIAN_POINT ( 'NONE',  ( -1.529674265799359834, 1405.855034992639958, 267.2342419976400265 ) ) ;
#29382 = CYLINDRICAL_SURFACE ( 'NONE', #25023, 0.9999999999999982236 ) ;
#29383 = ORIENTED_EDGE ( 'NONE', *, *, #70015, .F. ) ;
#29384 = CARTESIAN_POINT ( 'NONE',  ( -16.85976061912594304, 1525.821544997590763, 182.0492613858613709 ) ) ;
#29385 = CARTESIAN_POINT ( 'NONE',  ( 21.08703188481580071, 1525.317359687823455, 233.7719348611598775 ) ) ;
#29386 = ORIENTED_EDGE ( 'NONE', *, *, #30579, .F. ) ;
#29387 = ORIENTED_EDGE ( 'NONE', *, *, #83127, .F. ) ;
#29388 = CARTESIAN_POINT ( 'NONE',  ( -22.19805590008481389, 1506.691119431217430, 208.9309066648677913 ) ) ;
#29389 = CARTESIAN_POINT ( 'NONE',  ( 3.005276066430000448, 1369.205039411269809, 207.6218459616989946 ) ) ;
#29390 = CARTESIAN_POINT ( 'NONE',  ( -3.255967424474999650, 1516.989560013210166, 214.1335248082570217 ) ) ;
#29391 = CARTESIAN_POINT ( 'NONE',  ( 2.689982558025000081, 1512.192993275409890, 216.8079459747669944 ) ) ;
#29392 = ORIENTED_EDGE ( 'NONE', *, *, #74301, .F. ) ;
#29393 = CARTESIAN_POINT ( 'NONE',  ( -11.69665699774160039, 1509.376109397690016, 181.5816757439210107 ) ) ;
#29394 = CARTESIAN_POINT ( 'NONE',  ( -94.35247987469999487, 1374.531630663889928, 302.8771378034590498 ) ) ;
#29395 = B_SPLINE_CURVE_WITH_KNOTS ( 'NONE', 3,
 ( #15867, #50070, #59025, #56806, #84199, #8041, #110510, #67986, #5854, #22603, #39995, #9161, #10252, #68534, #43325, #93684, #17522, #27612, #78572, #103770, #69649, #25932, #44428, #94814, #16963, #26495, #51163, #2447, #18090, #77473, #95919, #34358, #36563, #60691, #52285, #8590, #19180, #102097, #231, #102632, #51725, #43867, #85291 ),
 .UNSPECIFIED., .F., .F.,
 ( 4, 3, 3, 3, 3, 3, 3, 3, 3, 3, 3, 3, 3, 3, 4 ),
 ( 0.7655572723400000390, 0.9910019213991279052, 1.224379696602929890, 1.462078613820340101, 1.704827352800629914, 1.793853281190000093, 2.038466587763309690, 2.281256468240929980, 2.316155491850000026, 2.583989317130000352, 2.855920919032060024, 3.139267318808710350, 3.387490792969999998, 3.680707184002069976, 3.835724788489999426 ),
 .UNSPECIFIED. ) ;
#29396 = CARTESIAN_POINT ( 'NONE',  ( 0.3621993314770000083, 1416.825784011830137, 227.1772709136979813 ) ) ;
#29397 = CARTESIAN_POINT ( 'NONE',  ( 5.774609621945000271, 1516.777260590120022, 204.5018377250270021 ) ) ;
#29398 = B_SPLINE_CURVE_WITH_KNOTS ( 'NONE', 3,
 ( #69287, #11019, #61445, #45190, #36770, #103392, #36218, #95020, #18290, #79331 ),
 .UNSPECIFIED., .F., .F.,
 ( 4, 3, 3, 4 ),
 ( -157.4228452129300138, -134.4932552904479905, -78.88175342727269879, -29.50720979924130916 ),
 .UNSPECIFIED. ) ;
#29399 = CARTESIAN_POINT ( 'NONE',  ( -12.12929454590999967, 1489.942571554460073, 210.7157588992720321 ) ) ;
#29400 = CARTESIAN_POINT ( 'NONE',  ( 10.98083629090000102, 1433.016921068679949, 151.7694307944979926 ) ) ;
#29401 = CARTESIAN_POINT ( 'NONE',  ( -7.956249640850000304, 1409.190898750130145, 229.5825722790980024 ) ) ;
#29403 = VERTEX_POINT ( 'NONE', #59457 ) ;
#29402 = CARTESIAN_POINT ( 'NONE',  ( -13.91344329460000040, 1453.313060387329870, 193.8272260107980003 ) ) ;
#29404 = CARTESIAN_POINT ( 'NONE',  ( -13.91014548664164430, 1434.990849513932744, 148.7055284007215334 ) ) ;
#29406 = B_SPLINE_CURVE_WITH_KNOTS ( 'NONE', 5,
 ( #95384, #86973, #10264, #19193, #71883, #37679 ),
 .UNSPECIFIED., .F., .F.,
 ( 6, 6 ),
 ( 0.000000000000000000, 1.000000000000000000 ),
 .UNSPECIFIED. ) ;
#29405 = CARTESIAN_POINT ( 'NONE',  ( -26.77477579971149879, 1440.913060431829763, 225.7736581942319845 ) ) ;
#29407 = AXIS2_PLACEMENT_3D ( 'NONE', #31213, #73227, #40167 ) ;
#29408 = B_SPLINE_CURVE_WITH_KNOTS ( 'NONE', 5,
 ( #307, #17599, #85938, #93759, #26005, #9781 ),
 .UNSPECIFIED., .F., .F.,
 ( 6, 6 ),
 ( 0.000000000000000000, 1.000000000000000000 ),
 .UNSPECIFIED. ) ;
#29409 = CARTESIAN_POINT ( 'NONE',  ( -1.590905566307312169, 1484.788648649911920, 182.5874796340517605 ) ) ;
#29410 = CARTESIAN_POINT ( 'NONE',  ( 21.84020450222037724, 1523.382868172864164, 183.2638850454218016 ) ) ;
#29411 = CARTESIAN_POINT ( 'NONE',  ( 36.30653363867440220, 1420.740886386239936, 270.0454586556700178 ) ) ;
#29412 = AXIS2_PLACEMENT_3D ( 'NONE', #39125, #73863, #47012 ) ;
#29413 = CARTESIAN_POINT ( 'NONE',  ( 2.491188358395000080, 1516.733363207009916, 213.1488973760370129 ) ) ;
#29414 = CARTESIAN_POINT ( 'NONE',  ( -67.41494648059999406, 1379.746829620230073, 277.3878582505590202 ) ) ;
#29415 = VECTOR ( 'NONE', #16390, 1000.000000000000000 ) ;
#29416 = CARTESIAN_POINT ( 'NONE',  ( 23.28494588540000265, 1410.121302984230169, 208.0652278728080091 ) ) ;
#29417 = CARTESIAN_POINT ( 'NONE',  ( -9.968725191709733480, 1426.791337612255802, 224.6101419120311959 ) ) ;
#29418 = CARTESIAN_POINT ( 'NONE',  ( -30.83422926911917727, 1524.871836253796118, 221.7255529736243602 ) ) ;
#29419 = CARTESIAN_POINT ( 'NONE',  ( -7.716977042262949560, 1516.837731796779963, 209.4547301039729632 ) ) ;
#29420 =( BOUNDED_CURVE ( )  B_SPLINE_CURVE ( 3, ( #41981, #76131, #110272, #43088 ),
 .UNSPECIFIED., .F., .T. ) 
 B_SPLINE_CURVE_WITH_KNOTS ( ( 4, 4 ),
 ( 1.309525232983709930, 2.739590174588970140 ),
 .UNSPECIFIED. ) 
 CURVE ( )  GEOMETRIC_REPRESENTATION_ITEM ( )  RATIONAL_B_SPLINE_CURVE ( ( 1.000000000000000000, 0.8367146349265004446, 0.8367146349265004446, 1.000000000000000000 ) ) 
 REPRESENTATION_ITEM ( '' )  );
#29421 = CARTESIAN_POINT ( 'NONE',  ( -1.704170752255000032, 1516.927039499179955, 209.8797722570040207 ) ) ;
#29422 = ORIENTED_EDGE ( 'NONE', *, *, #22749, .F. ) ;
#29423 = CARTESIAN_POINT ( 'NONE',  ( 4.367919453601240676, 1420.283793878259985, 185.7030090601730024 ) ) ;
#29424 = CARTESIAN_POINT ( 'NONE',  ( -4.423956996199999381, 1420.445634857929917, 232.5284400546979953 ) ) ;
#29425 = CARTESIAN_POINT ( 'NONE',  ( -5.513435837193367384, 1508.551704405448163, 201.9544627215969115 ) ) ;
#29426 = ORIENTED_EDGE ( 'NONE', *, *, #2116, .T. ) ;
#29427 = CARTESIAN_POINT ( 'NONE',  ( -27.26703367711199988, 1385.245975695329889, 225.4376821524880086 ) ) ;
#29428 = CARTESIAN_POINT ( 'NONE',  ( -4.487249770485409961, 1509.038615931769982, 206.6339108289169815 ) ) ;
#29429 = ADVANCED_FACE ( 'NONE', ( #7376 ), #93567, .F. ) ;
#29430 = PRODUCT_DEFINITION_SHAPE ( 'NONE', 'NONE',  #110832 ) ;
#29431 = CARTESIAN_POINT ( 'NONE',  ( -20.54724545888079845, 1508.877283812049882, 228.7275089972629871 ) ) ;
#29432 = CARTESIAN_POINT ( 'NONE',  ( -4.442976950240000278, 1500.747712884389784, 229.9760442845989985 ) ) ;
#29433 = CARTESIAN_POINT ( 'NONE',  ( 3.958634245108940242, 1508.551704408389924, 214.1089244000060035 ) ) ;
#29434 = CARTESIAN_POINT ( 'NONE',  ( 0.08318261387021998188, 1420.450964567450228, 182.6885337629809953 ) ) ;
#29436 = CARTESIAN_POINT ( 'NONE',  ( -8.002723402924999618, 1516.551704408390151, 212.1748218667169965 ) ) ;
#29435 = CARTESIAN_POINT ( 'NONE',  ( -5.778372601744999670, 1516.932669162149978, 216.0673360190369863 ) ) ;
#29437 = CARTESIAN_POINT ( 'NONE',  ( 19.41936330180000070, 1509.602163029830081, 186.8298580870979890 ) ) ;
#29438 = CARTESIAN_POINT ( 'NONE',  ( 10.03880117160240104, 1469.015768458370076, 208.9124404369970023 ) ) ;
#29439 = ORIENTED_EDGE ( 'NONE', *, *, #107944, .T. ) ;
#29440 = CARTESIAN_POINT ( 'NONE',  ( -1.129386240404999908, 1516.613712827999962, 201.7984555248870038 ) ) ;
#29441 = CARTESIAN_POINT ( 'NONE',  ( 10.52837420263239920, 1481.199010226290284, 208.2608686310830137 ) ) ;
#29442 = ORIENTED_EDGE ( 'NONE', *, *, #78287, .F. ) ;
#29443 = CARTESIAN_POINT ( 'NONE',  ( -0.04767993734059999822, 1497.009589119729981, 230.7918941427979860 ) ) ;
#29444 = CARTESIAN_POINT ( 'NONE',  ( 10.07052880280942908, 1435.587077992309560, 152.4438796952450446 ) ) ;
#29445 = CARTESIAN_POINT ( 'NONE',  ( 8.383305398618512427, 1424.402938891004396, 195.8285644112468447 ) ) ;
#29446 = VECTOR ( 'NONE', #92104, 1000.000000000000000 ) ;
#29447 =( BOUNDED_CURVE ( )  B_SPLINE_CURVE ( 3, ( #61268, #95383, #42219, #76933 ),
 .UNSPECIFIED., .F., .F. ) 
 B_SPLINE_CURVE_WITH_KNOTS ( ( 4, 4 ),
 ( 6.111083944147519986, 6.515951168162740004 ),
 .UNSPECIFIED. ) 
 CURVE ( )  GEOMETRIC_REPRESENTATION_ITEM ( )  RATIONAL_B_SPLINE_CURVE ( ( 1.000000000000000000, 0.9863867946965088063, 0.9863867946965088063, 1.000000000000000000 ) ) 
 REPRESENTATION_ITEM ( '' )  );
#29448 = CARTESIAN_POINT ( 'NONE',  ( 2.552069496900000178, 1442.069545149990063, 217.9835893629989982 ) ) ;
#29449 = CARTESIAN_POINT ( 'NONE',  ( -26.37463876368559923, 1508.216329634349904, 201.5356496705930169 ) ) ;
#29450 = B_SPLINE_CURVE_WITH_KNOTS ( 'NONE', 5,
 ( #73372, #54929, #47075, #72825, #46534, #106958 ),
 .UNSPECIFIED., .F., .F.,
 ( 6, 6 ),
 ( 0.000000000000000000, 1.000000000000000000 ),
 .UNSPECIFIED. ) ;
#29451 = CARTESIAN_POINT ( 'NONE',  ( 4.853127557110000545, 1425.657129708029970, 185.6214293445979990 ) ) ;
#29452 = CARTESIAN_POINT ( 'NONE',  ( -18.55525628600000232, 1424.342884875230084, 224.9435532434980018 ) ) ;
#29453 = CARTESIAN_POINT ( 'NONE',  ( -18.76321975249999952, 1435.968681994980216, 146.5949445436979772 ) ) ;
#29454 = CARTESIAN_POINT ( 'NONE',  ( -3.623165609177270152, 1464.721259246360205, 198.7228523319660098 ) ) ;
#29455 = CARTESIAN_POINT ( 'NONE',  ( 17.56617749740000178, 1509.356465172729941, 187.2275717433980162 ) ) ;
#29457 = FACE_OUTER_BOUND ( 'NONE', #44251, .T. ) ;
#29456 = CARTESIAN_POINT ( 'NONE',  ( 0.3788395847950430384, 1408.926289757150016, 231.6114269033369908 ) ) ;
#29458 = CARTESIAN_POINT ( 'NONE',  ( 20.59987592950000135, 1509.677367935830262, 230.5839143914980127 ) ) ;
#29459 = ORIENTED_EDGE ( 'NONE', *, *, #54906, .F. ) ;
#29460 = CARTESIAN_POINT ( 'NONE',  ( -105.3886526319999888, 1378.843576906529961, 303.6910441815589934 ) ) ;
#29461 = CARTESIAN_POINT ( 'NONE',  ( -13.06308345429999918, 1508.551704408389924, 216.6557220756489812 ) ) ;
#29463 = ORIENTED_EDGE ( 'NONE', *, *, #87176, .T. ) ;
#29462 = CARTESIAN_POINT ( 'NONE',  ( 11.63679813930000151, 1439.363771630820111, 147.7934734181980048 ) ) ;
#29464 = EDGE_CURVE ( 'NONE', #88507, #38170, #42227, .T. ) ;
#29465 = CARTESIAN_POINT ( 'NONE',  ( 11.26595443788370154, 1470.492046862490042, 207.5653086360470070 ) ) ;
#29466 = CARTESIAN_POINT ( 'NONE',  ( 20.27427188109263057, 1517.151704408390060, 209.5053779269578342 ) ) ;
#29467 = CARTESIAN_POINT ( 'NONE',  ( -15.62861149524349891, 1418.244676918490086, 203.0179538217920197 ) ) ;
#29468 = CARTESIAN_POINT ( 'NONE',  ( -2.693001348318031063, 1524.059663615500085, 242.0866550885344282 ) ) ;
#29469 = CARTESIAN_POINT ( 'NONE',  ( 21.62349440730000083, 1475.513060387329915, 210.0994872298300038 ) ) ;
#29470 = B_SPLINE_SURFACE_WITH_KNOTS ( 'NONE', 5, 5, ( 
 ( #19768, #45006, #43880, #52848, #86423, #104886 ),
 ( #61811, #9713, #28177, #95933, #78024, #62363 ),
 ( #28731, #62936, #36577, #70775, #18103, #2461 ),
 ( #86975, #46108, #10265, #1901, #44441, #19194 ),
 ( #82826, #92881, #16158, #66615, #37680, #101255 ),
 ( #91232, #15053, #106000, #108587, #100718, #80238 ),
 ( #108024, #67157, #92324, #6674, #91775, #83931 ),
 ( #71884, #29276, #24554, #63468, #14512, #49250 ),
 ( #31873, #24000, #3557, #58742, #31321, #97587 ) ),
 .UNSPECIFIED., .F., .F., .F.,
 ( 6, 3, 6 ),
 ( 6, 6 ),
 ( 3.085444082959999612, 5.308104825929999215, 7.530765568899999707 ),
 ( 0.000000000000000000, 2.000000000000000000 ),
 .UNSPECIFIED. ) ;
#29471 = CARTESIAN_POINT ( 'NONE',  ( -17.38235994490000280, 1414.983771850430003, 207.6803065375279971 ) ) ;
#29472 = CARTESIAN_POINT ( 'NONE',  ( 4.524905829305170712, 1494.978413301719911, 220.1958960354820078 ) ) ;
#29473 = CARTESIAN_POINT ( 'NONE',  ( 20.56230369369999877, 1477.111288992490017, 217.7195332328089989 ) ) ;
#29474 = CARTESIAN_POINT ( 'NONE',  ( -94.52376074393620797, 1383.767472540709832, 309.7575467845289836 ) ) ;
#29475 = CARTESIAN_POINT ( 'NONE',  ( -109.4169698722499930, 1383.736799322780143, 311.1655289953600345 ) ) ;
#29476 = CARTESIAN_POINT ( 'NONE',  ( 0.3076635671722720011, 1517.019662593890189, 201.4001056456369838 ) ) ;
#29478 = ORIENTED_EDGE ( 'NONE', *, *, #81740, .T. ) ;
#29477 = CARTESIAN_POINT ( 'NONE',  ( 2.828342949539999651, 1493.511444851789975, 217.0450404263189910 ) ) ;
#29479 = CARTESIAN_POINT ( 'NONE',  ( -109.9987473190000031, 1383.447530301710003, 297.1744276475590141 ) ) ;
#29480 = CARTESIAN_POINT ( 'NONE',  ( -16.73628186595804479, 1526.382868172863937, 234.1845039693045862 ) ) ;
#29481 = ORIENTED_EDGE ( 'NONE', *, *, #15810, .T. ) ;
#29482 = ORIENTED_EDGE ( 'NONE', *, *, #73247, .F. ) ;
#29483 = CARTESIAN_POINT ( 'NONE',  ( 27.43028940841649899, 1502.108409533960184, 207.6706673447280025 ) ) ;
#29484 = PLANE ( 'NONE',  #92173 ) ;
#29485 = DIRECTION ( 'NONE',  ( -0.7454942576402588950, 0.000000000000000000, 0.6665120492724789791 ) ) ;
#29487 = CARTESIAN_POINT ( 'NONE',  ( -14.01630619240000009, 1463.409576320030055, 240.3753821224980243 ) ) ;
#29486 = CARTESIAN_POINT ( 'NONE',  ( 38.87758531470136347, 1429.322872991726626, 269.5908715927216690 ) ) ;
#29488 = VECTOR ( 'NONE', #7782, 1000.000000000000000 ) ;
#29489 = CARTESIAN_POINT ( 'NONE',  ( 8.647870999238421064, 1437.913672787270116, 209.8191767245930066 ) ) ;
#29490 = CARTESIAN_POINT ( 'NONE',  ( -11.90119129059999992, 1433.600010809670039, 150.4754670856979999 ) ) ;
#29491 = CARTESIAN_POINT ( 'NONE',  ( 25.63705379909999849, 1507.963168667929949, 199.9117834894379939 ) ) ;
#29492 = CARTESIAN_POINT ( 'NONE',  ( -19.75357342619999912, 1485.455168234730081, 190.4162906186979853 ) ) ;
#29493 = DIRECTION ( 'NONE',  ( 0.000000000000000000, 0.000000000000000000, 1.000000000000000000 ) ) ;
#29494 = CARTESIAN_POINT ( 'NONE',  ( 0.02955819112566530210, 1522.051704408389924, 193.2356110507530218 ) ) ;
#29495 = CARTESIAN_POINT ( 'NONE',  ( 4.749626518910000428, 1420.878300781530015, 185.8027267283979995 ) ) ;
#29497 = CARTESIAN_POINT ( 'NONE',  ( 0.3081309748295429918, 1515.153045852129935, 213.4489837523270239 ) ) ;
#29496 = CIRCLE ( 'NONE', #90234, 2.000000000000001776 ) ;
#29498 = CARTESIAN_POINT ( 'NONE',  ( 6.472929441039998899, 1440.851741079749900, 154.4738948603979907 ) ) ;
#29499 = CARTESIAN_POINT ( 'NONE',  ( -8.683283342131749905, 1478.809903676939939, 216.8972849895139916 ) ) ;
#29500 = CARTESIAN_POINT ( 'NONE',  ( 33.05665451062059645, 1523.390106123591067, 200.9313857523606544 ) ) ;
#29502 = EDGE_LOOP ( 'NONE', ( #10915, #61409, #16846, #46704, #4891 ) ) ;
#29501 = CARTESIAN_POINT ( 'NONE',  ( 1.393491831154829911E-08, 1407.187418594129895, 264.6521298086510114 ) ) ;
#29503 = ORIENTED_EDGE ( 'NONE', *, *, #75415, .T. ) ;
#29504 = CARTESIAN_POINT ( 'NONE',  ( -11.46284668979999921, 1503.757050468389934, 207.6153425473289929 ) ) ;
#29505 = EDGE_CURVE ( 'NONE', #104636, #86228, #34975, .T. ) ;
#29506 = ADVANCED_FACE ( 'NONE', ( #9025 ), #102743, .F. ) ;
#29507 = CARTESIAN_POINT ( 'NONE',  ( -21.51493310030000217, 1488.287434706290014, 202.1454994110590064 ) ) ;
#29508 = CARTESIAN_POINT ( 'NONE',  ( -10.80862676880000173, 1472.323376642129915, 270.4164080859980004 ) ) ;
#29509 = CARTESIAN_POINT ( 'NONE',  ( -23.81682389853370196, 1436.006617566450132, 211.5115497514818514 ) ) ;
#29510 = CARTESIAN_POINT ( 'NONE',  ( -124.7066708633992391, 1371.894749952189386, 298.0449835127411689 ) ) ;
#29511 = EDGE_CURVE ( 'NONE', #38227, #17543, #42104, .T. ) ;
#29512 = CARTESIAN_POINT ( 'NONE',  ( 38.19124013942580831, 1450.350426091419877, 134.7937114414860105 ) ) ;
#29514 = EDGE_CURVE ( 'NONE', #16271, #97990, #650, .T. ) ;
#29513 = CARTESIAN_POINT ( 'NONE',  ( 0.3008760843888489966, 1451.060995806890105, 182.0476195407850071 ) ) ;
#29515 = CARTESIAN_POINT ( 'NONE',  ( -11.39124975620000058, 1419.317003928930035, 229.3344809721980084 ) ) ;
#29516 = EDGE_CURVE ( 'NONE', #65987, #36273, #43742, .T. ) ;
#29517 = CARTESIAN_POINT ( 'NONE',  ( -30.12521068615179942, 1524.538969332612623, 222.3851261604999365 ) ) ;
#29518 = CARTESIAN_POINT ( 'NONE',  ( -1.357091273329259939, 1484.488606510706177, 182.3747662795626923 ) ) ;
#29519 = CARTESIAN_POINT ( 'NONE',  ( 9.515060695661910373, 1360.808172452092322, 209.6218459617033432 ) ) ;
#29520 = CARTESIAN_POINT ( 'NONE',  ( -45.78687059534480142, 1437.115450045800117, 266.6856014455760260 ) ) ;
#29521 = ORIENTED_EDGE ( 'NONE', *, *, #11777, .T. ) ;
#29522 = CARTESIAN_POINT ( 'NONE',  ( -3.535553491242379831, 1493.818507742730162, 181.5437437456840257 ) ) ;
#29523 = EDGE_CURVE ( 'NONE', #48957, #53407, #31373, .T. ) ;
#29524 = EDGE_LOOP ( 'NONE', ( #12332, #55487, #65515, #20643 ) ) ;
#29525 = ORIENTED_EDGE ( 'NONE', *, *, #82409, .F. ) ;
#29526 = CARTESIAN_POINT ( 'NONE',  ( 2.299983577604999940, 1516.861367446839949, 211.4044688825970013 ) ) ;
#29527 = CARTESIAN_POINT ( 'NONE',  ( -9.533255814881970380, 1446.965757609550110, 212.1719659162569940 ) ) ;
#29528 = CARTESIAN_POINT ( 'NONE',  ( 16.56042414419820119, 1409.526307809821674, 224.8086540885646798 ) ) ;
#29529 = CARTESIAN_POINT ( 'NONE',  ( -7.074511979060000399, 1410.392875876630114, 187.4399194922980030 ) ) ;
#29530 = FACE_OUTER_BOUND ( 'NONE', #93411, .T. ) ;
#29531 = VERTEX_POINT ( 'NONE', #39741 ) ;
#29532 = AXIS2_PLACEMENT_3D ( 'NONE', #71998, #3683, #38886 ) ;
#29533 = EDGE_CURVE ( 'NONE', #40922, #40014, #45721, .T. ) ;
#29534 = B_SPLINE_CURVE_WITH_KNOTS ( 'NONE', 5,
 ( #96881, #20150, #12856, #38068, #81162, #21226, #53803, #105274, #19601, #46493, #62764, #87940 ),
 .UNSPECIFIED., .F., .F.,
 ( 6, 3, 3, 6 ),
 ( -14.75003859432340114, -6.990622299139999996, 15.67373306499999863, 31.20981119710000229 ),
 .UNSPECIFIED. ) ;
#29535 = CARTESIAN_POINT ( 'NONE',  ( 7.329303077985000137, 1516.857992118400034, 201.7912917986770083 ) ) ;
#29536 = CARTESIAN_POINT ( 'NONE',  ( -20.27427188162093330, 1522.051704408389924, 208.7383139970561672 ) ) ;
#29537 = EDGE_CURVE ( 'NONE', #11318, #74815, #84825, .T. ) ;
#29538 = CARTESIAN_POINT ( 'NONE',  ( -25.34121475049380123, 1384.545363099709903, 203.4200895163570237 ) ) ;
#29539 = VERTEX_POINT ( 'NONE', #80646 ) ;
#29540 = CARTESIAN_POINT ( 'NONE',  ( -9.945122577541358311, 1408.453178102650099, 270.1158524044950013 ) ) ;
#29541 = CARTESIAN_POINT ( 'NONE',  ( 2.986439680811220132, 1417.855500646999872, 233.9854127040079845 ) ) ;
#29542 = CARTESIAN_POINT ( 'NONE',  ( 8.931424042116880457, 1435.562258453619961, 207.9893077555419723 ) ) ;
#29544 = ORIENTED_EDGE ( 'NONE', *, *, #54299, .F. ) ;
#29543 = CARTESIAN_POINT ( 'NONE',  ( -9.977700672470000143, 1365.292605733890014, 207.6218459616989946 ) ) ;
#29545 = VERTEX_POINT ( 'NONE', #63864 ) ;
#29546 = EDGE_CURVE ( 'NONE', #4755, #58393, #68982, .T. ) ;
#29547 = CARTESIAN_POINT ( 'NONE',  ( 44.51678373992154292, 1448.484642947900738, 269.0061672408559161 ) ) ;
#29548 = CARTESIAN_POINT ( 'NONE',  ( 11.21674625111110046, 1471.567453512700240, 211.3061429236929882 ) ) ;
#29549 = CARTESIAN_POINT ( 'NONE',  ( -14.09009566611259956, 1436.250362699700190, 150.1829504920789873 ) ) ;
#29550 = CARTESIAN_POINT ( 'NONE',  ( -0.03615109642835009907, 1409.488087751360126, 185.3130394953689688 ) ) ;
#29551 = EDGE_CURVE ( 'NONE', #76640, #91618, #27543, .T. ) ;
#29552 = CARTESIAN_POINT ( 'NONE',  ( -17.86421487526029850, 1415.184612913570163, 207.5656586035410101 ) ) ;
#29553 = CARTESIAN_POINT ( 'NONE',  ( -19.08968851999999927, 1435.774291999059869, 224.9956671329980225 ) ) ;
#29554 = CARTESIAN_POINT ( 'NONE',  ( -14.00467695169999871, 1423.498461949430293, 222.1148246841979983 ) ) ;
#29555 = CARTESIAN_POINT ( 'NONE',  ( 11.83559671189999918, 1415.245980412430072, 222.8086952457979919 ) ) ;
#29556 = CARTESIAN_POINT ( 'NONE',  ( 7.560826431379999768, 1445.756812236420046, 183.8406469472979836 ) ) ;
#29557 = CARTESIAN_POINT ( 'NONE',  ( 1.118353215965000036, 1516.977201124959947, 206.6281488911770055 ) ) ;
#29558 = ORIENTED_EDGE ( 'NONE', *, *, #82503, .T. ) ;
#29559 = CARTESIAN_POINT ( 'NONE',  ( -40.71747595839320155, 1438.773003563489965, 135.3761635789150262 ) ) ;
#29560 = DIRECTION ( 'NONE',  ( 0.000000000000000000, 1.000000000000000000, 0.000000000000000000 ) ) ;
#29561 = ORIENTED_EDGE ( 'NONE', *, *, #42858, .F. ) ;
#29562 = LINE ( 'NONE', #62664, #105354 ) ;
#29563 = CARTESIAN_POINT ( 'NONE',  ( 24.53925018798819835, 1451.993264915540067, 136.6785377935909764 ) ) ;
#29564 = DIRECTION ( 'NONE',  ( -1.000000000000000000, 0.000000000000000000, 0.000000000000000000 ) ) ;
#29565 = CARTESIAN_POINT ( 'NONE',  ( -9.018403443429999555, 1415.839591758850020, 205.4133982750190057 ) ) ;
#29566 = CARTESIAN_POINT ( 'NONE',  ( 18.97990684999999900, 1409.575853339430068, 198.5868976705980060 ) ) ;
#29567 = CARTESIAN_POINT ( 'NONE',  ( 22.30625523140000155, 1409.857389917029877, 207.2280132821280176 ) ) ;
#29568 = CARTESIAN_POINT ( 'NONE',  ( -24.94579848589999926, 1435.368615134259926, 135.7553688025980136 ) ) ;
#29569 = CARTESIAN_POINT ( 'NONE',  ( 32.86802468386284914, 1523.382868172864164, 201.0396662540042030 ) ) ;
#29570 = CARTESIAN_POINT ( 'NONE',  ( 0.9686598153761089014, 1450.845731688880051, 181.4217000318980126 ) ) ;
#29571 = CARTESIAN_POINT ( 'NONE',  ( 2.500000000000000000, 1439.624608404519904, 169.5728743624090100 ) ) ;
#29572 = CARTESIAN_POINT ( 'NONE',  ( 1.710004548794999968, 1516.557392317769882, 215.6678473207969944 ) ) ;
#29573 = ORIENTED_EDGE ( 'NONE', *, *, #61279, .F. ) ;
#29574 = CARTESIAN_POINT ( 'NONE',  ( -17.54173488089999822, 1417.696455080029864, 206.2934839100489910 ) ) ;
#29575 = CARTESIAN_POINT ( 'NONE',  ( -0.9912863951520000105, 1474.170141985030114, 270.1376065698979687 ) ) ;
#29576 = CARTESIAN_POINT ( 'NONE',  ( -18.34590456075780196, 1416.851343895820037, 208.8605686865189739 ) ) ;
#29577 = CARTESIAN_POINT ( 'NONE',  ( -8.690384483830820628, 1424.104242022259996, 112.3001764364740183 ) ) ;
#29578 = AXIS2_PLACEMENT_3D ( 'NONE', #103707, #9634, #52768 ) ;
#29579 = EDGE_CURVE ( 'NONE', #75280, #25855, #7512, .T. ) ;
#29580 = CARTESIAN_POINT ( 'NONE',  ( -39.63715609436299303, 1446.664237654140152, 136.6953018245600049 ) ) ;
#29581 = CARTESIAN_POINT ( 'NONE',  ( 11.60004869884913070, 1425.167079614044951, 137.9682444091046420 ) ) ;
#29582 = CARTESIAN_POINT ( 'NONE',  ( 2.068048313059574372, 1417.341179972549753, 233.1878878483405231 ) ) ;
#29583 = CARTESIAN_POINT ( 'NONE',  ( 17.82742679679007480, 1423.642332963798935, 225.9916762313126242 ) ) ;
#29584 = CARTESIAN_POINT ( 'NONE',  ( 11.58989588439999885, 1433.067267885580122, 151.1017417262979734 ) ) ;
#29585 = CARTESIAN_POINT ( 'NONE',  ( -0.6052730379878279443, 1475.056357020409905, 269.6445050902949561 ) ) ;
#29586 = B_SPLINE_SURFACE_WITH_KNOTS ( 'NONE', 5, 5, ( 
 ( #75091, #57197, #21875, #109240, #47675, #5674 ),
 ( #74539, #64496, #83457, #40358, #73981, #107568 ),
 ( #108671, #31961, #30855, #31405, #56074, #30306 ),
 ( #5105, #58281, #100275, #23555, #6752, #66154 ),
 ( #98612, #108111, #40911, #90201, #32524, #92406 ),
 ( #81804, #99700, #39260, #15141, #56628, #15678 ),
 ( #38704, #65030, #22992, #48793, #82915, #57747 ),
 ( #72880, #91867, #49331, #590, #94066, #75641 ),
 ( #9514, #61067, #51529, #43682, #102460, #58828 ) ),
 .UNSPECIFIED., .F., .F., .F.,
 ( 6, 3, 6 ),
 ( 6, 6 ),
 ( 13.44470524419999968, 14.51062177820000088, 15.26427305850000060 ),
 ( 0.000000000000000000, 2.000000000000000000 ),
 .UNSPECIFIED. ) ;
#29587 = CARTESIAN_POINT ( 'NONE',  ( 27.81399413693910105, 1440.913060387569885, 230.3950460944500094 ) ) ;
#29588 = CARTESIAN_POINT ( 'NONE',  ( -109.7214050949999944, 1385.089256956249983, 297.0893658214590118 ) ) ;
#29589 = CYLINDRICAL_SURFACE ( 'NONE', #63618, 1.999999999999999556 ) ;
#29590 = ORIENTED_EDGE ( 'NONE', *, *, #24225, .T. ) ;
#29591 = CARTESIAN_POINT ( 'NONE',  ( 13.51610093808350577, 1445.063428794548372, 150.6358704321319806 ) ) ;
#29592 = EDGE_CURVE ( 'NONE', #31342, #16564, #82294, .T. ) ;
#29593 = CARTESIAN_POINT ( 'NONE',  ( -19.28960628685421952, 1485.613772762859981, 189.7904103076950264 ) ) ;
#29594 = CARTESIAN_POINT ( 'NONE',  ( -1.439851189671583542, 1526.382868172864164, 239.5034140466476060 ) ) ;
#29595 = CARTESIAN_POINT ( 'NONE',  ( 2.633995852980000052, 1482.821221012130081, 234.8958063198980142 ) ) ;
#29596 = CARTESIAN_POINT ( 'NONE',  ( -10.47547176029999960, 1491.367109134090015, 212.5025952234090028 ) ) ;
#29597 = CARTESIAN_POINT ( 'NONE',  ( -16.94063806799999838, 1507.935533831129987, 230.1637782476980192 ) ) ;
#29598 = CARTESIAN_POINT ( 'NONE',  ( -29.19778036811970168, 1383.843077010679963, 226.9952897098220035 ) ) ;
#29599 = AXIS2_PLACEMENT_3D ( 'NONE', #37326, #38411, #64759 ) ;
#29600 = CARTESIAN_POINT ( 'NONE',  ( -21.46486174681220049, 1504.440211022489848, 215.6677628791860286 ) ) ;
#29601 = CARTESIAN_POINT ( 'NONE',  ( 5.363529431139269832, 1422.300429797930065, 141.6243240101889853 ) ) ;
#29602 = CARTESIAN_POINT ( 'NONE',  ( -11.61854873712450065, 1501.724215307040140, 208.7855428323910019 ) ) ;
#29603 = DIRECTION ( 'NONE',  ( -0.4794255386042071132, 0.000000000000000000, 0.8775825618903705383 ) ) ;
#29606 = ORIENTED_EDGE ( 'NONE', *, *, #55366, .T. ) ;
#29605 = B_SPLINE_CURVE_WITH_KNOTS ( 'NONE', 3,
 ( #1677, #88963, #39672, #90054, #55935, #80575, #96836, #107414, #63256, #4955 ),
 .UNSPECIFIED., .F., .F.,
 ( 4, 2, 2, 2, 4 ),
 ( 0.000000000000000000, 0.0007189769279725886052, 0.001437953855945177210, 0.002156930783917765816, 0.002875907711890354421 ),
 .UNSPECIFIED. ) ;
#29604 = CARTESIAN_POINT ( 'NONE',  ( -7.625096704207815712, 1438.527495425920733, 153.8927455731590328 ) ) ;
#29607 = CARTESIAN_POINT ( 'NONE',  ( -0.6632445612200000840, 1450.894163472750051, 181.6521849990980115 ) ) ;
#29608 = ADVANCED_FACE ( 'NONE', ( #54909 ), #52381, .F. ) ;
#29609 = CARTESIAN_POINT ( 'NONE',  ( -31.82321841959999986, 1383.006323701569954, 206.4748318456290122 ) ) ;
#29610 = CARTESIAN_POINT ( 'NONE',  ( 4.271224532216500336, 1508.551704408389924, 204.8816808314769844 ) ) ;
#29612 = ORIENTED_EDGE ( 'NONE', *, *, #16679, .T. ) ;
#29611 = CARTESIAN_POINT ( 'NONE',  ( 1.552364032401126082, 1414.913060581098307, 192.1087617152385008 ) ) ;
#29613 = CARTESIAN_POINT ( 'NONE',  ( -19.73708167012179970, 1467.795432308010049, 204.3773359938460032 ) ) ;
#29614 = ORIENTED_EDGE ( 'NONE', *, *, #83701, .F. ) ;
#29615 = AXIS2_PLACEMENT_3D ( 'NONE', #8176, #17663, #69221 ) ;
#29616 = CARTESIAN_POINT ( 'NONE',  ( -12.06798603031659844, 1389.351698808259925, 215.2113615822289887 ) ) ;
#29617 = DIRECTION ( 'NONE',  ( -0.5121697454732879740, 0.04449972806152376059, 0.8577306838537828160 ) ) ;
#29618 = DIRECTION ( 'NONE',  ( -0.9049609225110241129, -0.3874052256307211062, 0.1759628366502599961 ) ) ;
#29619 = ADVANCED_FACE ( 'NONE', ( #48158 ), #79616, .T. ) ;
#29620 = CARTESIAN_POINT ( 'NONE',  ( 7.613520793314999757, 1512.886889331459997, 214.7360521135969975 ) ) ;
#29621 = B_SPLINE_CURVE_WITH_KNOTS ( 'NONE', 5,
 ( #24351, #74786, #91009, #7011, #101053, #57986 ),
 .UNSPECIFIED., .F., .F.,
 ( 6, 6 ),
 ( 0.000000000000000000, 1.000000000000000000 ),
 .UNSPECIFIED. ) ;
#29622 = CARTESIAN_POINT ( 'NONE',  ( 4.639337580630000346, 1465.928856497889910, 219.1434977748990036 ) ) ;
#29623 = CARTESIAN_POINT ( 'NONE',  ( 2.472529913803013901, 1523.678648413191695, 242.8674788698241684 ) ) ;
#29624 = CARTESIAN_POINT ( 'NONE',  ( 14.84736599141850100, 1409.431541832679841, 207.5470409763789803 ) ) ;
#29625 = CARTESIAN_POINT ( 'NONE',  ( -7.966029247037079486, 1384.904051679539862, 199.4892879668419994 ) ) ;
#29626 = CARTESIAN_POINT ( 'NONE',  ( -89.54809965716370357, 1385.191320044069926, 292.2920403167919403 ) ) ;
#29627 = CARTESIAN_POINT ( 'NONE',  ( -19.45266374790000086, 1470.701691425329955, 191.2979019387979918 ) ) ;
#29628 = CARTESIAN_POINT ( 'NONE',  ( 5.273680924645899992, 1398.098440471860158, 218.7752541425170136 ) ) ;
#29629 = CARTESIAN_POINT ( 'NONE',  ( 11.77882348100120069, 1491.514007103689892, 207.7369858202129933 ) ) ;
#29630 = ORIENTED_EDGE ( 'NONE', *, *, #104187, .T. ) ;
#29631 = ORIENTED_EDGE ( 'NONE', *, *, #90099, .F. ) ;
#29632 = ADVANCED_FACE ( 'NONE', ( #67167 ), #69758, .F. ) ;
#29633 = CARTESIAN_POINT ( 'NONE',  ( 20.64339891394584114, 1523.429859730330236, 238.2599442700835937 ) ) ;
#29634 = FACE_OUTER_BOUND ( 'NONE', #83257, .T. ) ;
#29635 = CARTESIAN_POINT ( 'NONE',  ( 1.723570287401249956, 1496.958110707269952, 196.8512198874990133 ) ) ;
#29636 = EDGE_CURVE ( 'NONE', #21131, #5947, #100847, .T. ) ;
#29637 = CARTESIAN_POINT ( 'NONE',  ( 12.85540944714700018, 1420.911466006700039, 202.8798040533630171 ) ) ;
#29638 = CARTESIAN_POINT ( 'NONE',  ( -20.09679227796999967, 1491.565535399339979, 190.8618222658760146 ) ) ;
#29639 = CARTESIAN_POINT ( 'NONE',  ( 1.143705719820000022, 1395.952999471229759, 220.4423849542980065 ) ) ;
#29640 = CARTESIAN_POINT ( 'NONE',  ( 19.67294328819050264, 1440.103798296560171, 209.6949378802180206 ) ) ;
#29641 = CARTESIAN_POINT ( 'NONE',  ( -19.38775984613145908, 1486.273308771174698, 189.6873704809262051 ) ) ;
#29642 = CARTESIAN_POINT ( 'NONE',  ( -11.56214142042087367, 1363.316088303152810, 208.3718459617010978 ) ) ;
#29643 = CARTESIAN_POINT ( 'NONE',  ( -25.95396204517641081, 1436.671747891054565, 136.9772620809131354 ) ) ;
#29644 = CARTESIAN_POINT ( 'NONE',  ( 13.89512612635319933, 1452.719752330199981, 223.3357008107990112 ) ) ;
#29645 = EDGE_CURVE ( 'NONE', #36118, #34381, #27786, .T. ) ;
#29646 = CARTESIAN_POINT ( 'NONE',  ( 7.710966977635000497, 1516.608208975040043, 207.9930883710269711 ) ) ;
#29647 = CARTESIAN_POINT ( 'NONE',  ( 11.32042664782710162, 1433.973776647149862, 151.5090680528710152 ) ) ;
#29648 = CARTESIAN_POINT ( 'NONE',  ( -13.12645755140609971, 1434.861060459049895, 149.4023126016570018 ) ) ;
#29649 = CARTESIAN_POINT ( 'NONE',  ( -7.770472029140000458, 1385.200197327649903, 218.9075870494289688 ) ) ;
#29650 = CARTESIAN_POINT ( 'NONE',  ( 20.28125873362029807, 1409.621297548600069, 202.2274700573379960 ) ) ;
#29651 = CARTESIAN_POINT ( 'NONE',  ( 1.316858285199999923, 1498.792501773990125, 197.8475787186989976 ) ) ;
#29652 = CARTESIAN_POINT ( 'NONE',  ( -7.245822883755549171, 1494.393323836579839, 205.4491147294489792 ) ) ;
#29653 = EDGE_CURVE ( 'NONE', #13254, #88852, #92976, .T. ) ;
#29654 = CIRCLE ( 'NONE', #76184, 1.000002392508526627 ) ;
#29655 = ORIENTED_EDGE ( 'NONE', *, *, #8571, .F. ) ;
#29656 = CARTESIAN_POINT ( 'NONE',  ( 32.18001715519999806, 1422.275298650230070, 259.4130760070980273 ) ) ;
#29657 = CARTESIAN_POINT ( 'NONE',  ( -27.09023322290000380, 1488.688618555330095, 207.0766447722079988 ) ) ;
#29660 = CARTESIAN_POINT ( 'NONE',  ( -0.8261674427231310291, 1507.439223847129824, 231.9334160780449849 ) ) ;
#29659 = AXIS2_PLACEMENT_3D ( 'NONE', #31631, #84241, #6444 ) ;
#29658 = CARTESIAN_POINT ( 'NONE',  ( 0.4664314455240000101, 1502.016106112629814, 181.1536437472979912 ) ) ;
#29661 = LINE ( 'NONE', #108015, #12293 ) ;
#29662 = CARTESIAN_POINT ( 'NONE',  ( -25.73196790559999769, 1440.913060585610083, 220.8240077246979922 ) ) ;
#29663 = CARTESIAN_POINT ( 'NONE',  ( 0.8530558503729990250, 1485.832915321789869, 220.6087224736990038 ) ) ;
#29664 = DIRECTION ( 'NONE',  ( 0.000000000000000000, -1.000000000000000000, 0.000000000000000000 ) ) ;
#29665 = CARTESIAN_POINT ( 'NONE',  ( 33.53414597829999622, 1450.881089635289982, 136.1829610295979762 ) ) ;
#29666 = EDGE_LOOP ( 'NONE', ( #38560, #73361, #26261, #44812 ) ) ;
#29667 = CARTESIAN_POINT ( 'NONE',  ( -0.08249068136597970113, 1397.911857760039993, 196.1221076742430114 ) ) ;
#29668 = CARTESIAN_POINT ( 'NONE',  ( 11.28282561095590175, 1512.859148089919017, 225.3214806919623356 ) ) ;
#29669 = CARTESIAN_POINT ( 'NONE',  ( 8.792433923980000898, 1509.220098945629843, 237.4619125690979899 ) ) ;
#29670 = EDGE_LOOP ( 'NONE', ( #97202, #108071, #99452, #38972 ) ) ;
#29671 = VERTEX_POINT ( 'NONE', #64288 ) ;
#29672 = CARTESIAN_POINT ( 'NONE',  ( 2.894070330896479692, 1493.616686583509818, 235.3440883567899959 ) ) ;
#29673 = CARTESIAN_POINT ( 'NONE',  ( -23.32798702916920064, 1409.842805623620052, 208.9046620917229689 ) ) ;
#29674 = ORIENTED_EDGE ( 'NONE', *, *, #55600, .T. ) ;
#29675 = CARTESIAN_POINT ( 'NONE',  ( -1.479980094498569931, 1442.001091641500125, 203.0964119015820017 ) ) ;
#29676 = CARTESIAN_POINT ( 'NONE',  ( -105.0581303879369983, 1379.236400313860031, 304.0328620142400382 ) ) ;
#29677 = EDGE_CURVE ( 'NONE', #5728, #104546, #104891, .T. ) ;
#29678 = CARTESIAN_POINT ( 'NONE',  ( -11.97220943660000003, 1489.053879525330103, 232.5750221901979842 ) ) ;
#29680 = VECTOR ( 'NONE', #66232, 1000.000000000000227 ) ;
#29679 = DIRECTION ( 'NONE',  ( -1.836970198721029688E-16, -1.000000000000000000, 0.000000000000000000 ) ) ;
#29681 = ORIENTED_EDGE ( 'NONE', *, *, #88460, .F. ) ;
#29682 = CIRCLE ( 'NONE', #42166, 2.000000001200720856 ) ;
#29683 = CARTESIAN_POINT ( 'NONE',  ( 11.73648056819999930, 1426.280364960429779, 144.1673147891980022 ) ) ;
#29684 = CARTESIAN_POINT ( 'NONE',  ( -12.70648376454910000, 1416.221314539489867, 221.9053760979749654 ) ) ;
#29685 = CARTESIAN_POINT ( 'NONE',  ( 15.10082833669999935, 1496.663755438529961, 225.8002586636980027 ) ) ;
#29686 = CARTESIAN_POINT ( 'NONE',  ( -2.489617576474999705, 1516.665179208830068, 204.1258511445269903 ) ) ;
#29687 = ORIENTED_EDGE ( 'NONE', *, *, #95300, .T. ) ;
#29688 = DIRECTION ( 'NONE',  ( 0.000000000000000000, 0.7071067811865475727, 0.7071067811865475727 ) ) ;
#29689 = DIRECTION ( 'NONE',  ( -0.9831857282343242632, -0.1185196346870388412, 0.1389205527990460265 ) ) ;
#29690 = ORIENTED_EDGE ( 'NONE', *, *, #19116, .T. ) ;
#29691 = ORIENTED_EDGE ( 'NONE', *, *, #7279, .F. ) ;
#29692 = CARTESIAN_POINT ( 'NONE',  ( 2.057041824809119568, 1523.342713519622521, 173.3972930408587558 ) ) ;
#29693 = DIRECTION ( 'NONE',  ( 0.000000000000000000, 0.000000000000000000, 1.000000000000000000 ) ) ;
#29694 = CARTESIAN_POINT ( 'NONE',  ( 2.257484783599780442, 1497.637221951559923, 197.6769359036259743 ) ) ;
#29695 = CARTESIAN_POINT ( 'NONE',  ( -9.558539228608021077, 1469.579548421909976, 215.2843844815280079 ) ) ;
#29696 = B_SPLINE_CURVE_WITH_KNOTS ( 'NONE', 3,
 ( #38819, #100387, #66270, #22541, #108234, #57317, #23672, #13599, #83574, #79877, #91444, #98729, #74652, #23113, #6867, #65701 ),
 .UNSPECIFIED., .F., .F.,
 ( 4, 3, 3, 3, 3, 4 ),
 ( -7.748406663631770108, -7.197925092369000133, -6.190671629245319885, -5.186465823511379192, -4.183578071707561463, -3.182527802580000120 ),
 .UNSPECIFIED. ) ;
#29697 = CARTESIAN_POINT ( 'NONE',  ( 8.410267065803780360E-17, 1471.436294031830130, 269.3346704751489824 ) ) ;
#29698 = CARTESIAN_POINT ( 'NONE',  ( 0.4703715106335689677, 1410.239988018240183, 269.6149086376819923 ) ) ;
#29699 = CARTESIAN_POINT ( 'NONE',  ( 6.009430605671457926, 1511.590044791216769, 217.9119306497679531 ) ) ;
#29700 = CARTESIAN_POINT ( 'NONE',  ( -6.178279419090149993, 1494.593908523239861, 198.4675342823039728 ) ) ;
#29701 = CARTESIAN_POINT ( 'NONE',  ( -9.862951376772540968, 1521.951704408389787, 228.3939896807019920 ) ) ;
#29702 = CARTESIAN_POINT ( 'NONE',  ( 0.03395513245188531287, 1410.034063517130335, 233.1861139216583467 ) ) ;
#29704 = CARTESIAN_POINT ( 'NONE',  ( -106.6962466664339928, 1391.913060387289988, 306.0375484597149693 ) ) ;
#29703 = CARTESIAN_POINT ( 'NONE',  ( -18.24261182150000238, 1504.557842952090141, 209.1081479311360170 ) ) ;
#29705 = CARTESIAN_POINT ( 'NONE',  ( 11.63005500354680066, 1422.115563547319880, 207.2156999536339868 ) ) ;
#29706 = CARTESIAN_POINT ( 'NONE',  ( -24.27081182540139892, 1508.823454366900023, 222.4349774664410120 ) ) ;
#29707 = CARTESIAN_POINT ( 'NONE',  ( -7.378505853204999632, 1513.311928781849929, 201.4764924376770239 ) ) ;
#29708 = VERTEX_POINT ( 'NONE', #45833 ) ;
#29709 = CARTESIAN_POINT ( 'NONE',  ( 1.021405182659999929E-14, 1413.763055110029882, 262.6648722463980334 ) ) ;
#29710 = B_SPLINE_CURVE_WITH_KNOTS ( 'NONE', 5,
 ( #83927, #8864, #8316, #86139, #92319, #84483 ),
 .UNSPECIFIED., .F., .F.,
 ( 6, 6 ),
 ( 5.175829887319999933, 13.45293097300000085 ),
 .UNSPECIFIED. ) ;
#29711 = CARTESIAN_POINT ( 'NONE',  ( 19.74393297465665142, 1455.407987973826721, 226.2017192373469072 ) ) ;
#29713 = CARTESIAN_POINT ( 'NONE',  ( -81.42719599728999924, 1384.990247741029862, 304.7659821400590090 ) ) ;
#29712 = B_SPLINE_CURVE_WITH_KNOTS ( 'NONE', 3,
 ( #10513, #44687, #2143, #9408, #96175, #19450, #53649, #36821, #71011, #45800, #3250, #37376, #71577, #105698, #28981, #14353, #74300, #73750, #90519, #72641, #30622, #12719, #21094, #97815, #13795, #107873, #108431, #39578, #30058, #47435, #55297 ),
 .UNSPECIFIED., .F., .F.,
 ( 4, 3, 3, 3, 3, 3, 3, 3, 3, 3, 4 ),
 ( 2.324858856890000158, 2.629659992665080104, 2.924842189028200146, 3.130565735590880028, 3.432172540380809878, 3.731439316892459779, 4.025646101128260490, 4.318556006019989901, 4.608870341565640238, 4.895817131713270598, 4.991117563570000470 ),
 .UNSPECIFIED. ) ;
#29714 = CARTESIAN_POINT ( 'NONE',  ( 4.046802277660000335, 1505.460036802790000, 221.2327940266990254 ) ) ;
#29715 = CARTESIAN_POINT ( 'NONE',  ( 44.92382594201649937, 1434.805869292970101, 269.6913831597940430 ) ) ;
#29717 = ORIENTED_EDGE ( 'NONE', *, *, #24762, .F. ) ;
#29716 = CARTESIAN_POINT ( 'NONE',  ( -16.92376582506389937, 1419.669853879900074, 208.5035371377049955 ) ) ;
#29718 = CARTESIAN_POINT ( 'NONE',  ( -17.00797328670000397, 1417.537217351680056, 207.7155449971589860 ) ) ;
#29719 = CARTESIAN_POINT ( 'NONE',  ( 32.02808312589922224, 1512.187213306747481, 219.9649204700462235 ) ) ;
#29720 = CARTESIAN_POINT ( 'NONE',  ( -16.51698475970000146, 1416.970002106650099, 207.7815561879389747 ) ) ;
#29721 = CARTESIAN_POINT ( 'NONE',  ( 0.9458865576463879599, 1430.745089220539967, 199.7241109523880027 ) ) ;
#29722 = CARTESIAN_POINT ( 'NONE',  ( 14.21596110103500088, 1513.125294087170005, 224.5826807846669908 ) ) ;
#29723 = CARTESIAN_POINT ( 'NONE',  ( -11.98374141780000102, 1442.037920581979961, 187.4992083556979878 ) ) ;
#29724 = CARTESIAN_POINT ( 'NONE',  ( 9.357303305019659234, 1435.432409049479929, 208.4554647895430151 ) ) ;
#29725 = CARTESIAN_POINT ( 'NONE',  ( 12.44506479032133228, 1434.392593279323364, 149.5199551435223100 ) ) ;
#29726 = CARTESIAN_POINT ( 'NONE',  ( 14.15980981120000060, 1419.763654237730179, 228.3914994946979959 ) ) ;
#29727 = EDGE_CURVE ( 'NONE', #64548, #75280, #72974, .T. ) ;
#29728 = FACE_OUTER_BOUND ( 'NONE', #37904, .T. ) ;
#29729 = CARTESIAN_POINT ( 'NONE',  ( -2.881548462575000080, 1516.909589401870107, 206.8382752989369919 ) ) ;
#29730 = CARTESIAN_POINT ( 'NONE',  ( 43.61890073000000001, 1430.078080930229817, 269.0317426087980266 ) ) ;
#29731 = CARTESIAN_POINT ( 'NONE',  ( -18.48711282149999846, 1410.482182154930115, 223.8902303684980097 ) ) ;
#29732 = CARTESIAN_POINT ( 'NONE',  ( 19.79232125780000118, 1435.617562599800067, 145.2032765877980012 ) ) ;
#29733 = CARTESIAN_POINT ( 'NONE',  ( -7.469899998879999892, 1491.463634741090118, 211.3946206457289918 ) ) ;
#29734 = CARTESIAN_POINT ( 'NONE',  ( 5.383048381580209707, 1431.499937560449780, 154.5621489401540032 ) ) ;
#29735 = CARTESIAN_POINT ( 'NONE',  ( -45.67177895054734194, 1445.962983056130724, 266.1885922345551876 ) ) ;
#29736 = CARTESIAN_POINT ( 'NONE',  ( 0.000000000000000000, 1518.913060387330006, 209.1218459616979999 ) ) ;
#29737 = CARTESIAN_POINT ( 'NONE',  ( -39.29199511529999711, 1440.043273471179873, 136.7298370636979712 ) ) ;
#29738 = CARTESIAN_POINT ( 'NONE',  ( 0.2080955792599850085, 1458.419842128130085, 183.0208787316280166 ) ) ;
#29739 = CARTESIAN_POINT ( 'NONE',  ( -14.34547416000000020, 1409.237120669629803, 210.6641495597280027 ) ) ;
#29740 = CARTESIAN_POINT ( 'NONE',  ( -11.96393163419999972, 1414.971352895729979, 197.5065629898979864 ) ) ;
#29741 = CARTESIAN_POINT ( 'NONE',  ( -4.175275161990000150, 1515.456650324490056, 207.6382005906990003 ) ) ;
#29742 = EDGE_CURVE ( 'NONE', #73277, #68085, #72560, .T. ) ;
#29743 = LINE ( 'NONE', #40346, #44386 ) ;
#29744 = CARTESIAN_POINT ( 'NONE',  ( 12.06092026859999855, 1433.903687484779994, 149.4776502453979958 ) ) ;
#29745 = CARTESIAN_POINT ( 'NONE',  ( -38.19279632269630298, 1437.094169276000002, 134.0999999969999692 ) ) ;
#29746 = CARTESIAN_POINT ( 'NONE',  ( 7.671879397589999705, 1442.085042682959966, 183.9124572552979657 ) ) ;
#29747 = ORIENTED_EDGE ( 'NONE', *, *, #82319, .T. ) ;
#29748 = CARTESIAN_POINT ( 'NONE',  ( -2.919110404717550011, 1368.384062535930070, 207.8228080779019820 ) ) ;
#29749 = CARTESIAN_POINT ( 'NONE',  ( 27.58075381470000309, 1440.826362455070011, 137.2340171046979833 ) ) ;
#29750 = CARTESIAN_POINT ( 'NONE',  ( -11.05457274329999784, 1492.346892589090203, 209.2220259002270097 ) ) ;
#29751 = EDGE_LOOP ( 'NONE', ( #95571, #27249, #96031, #41086 ) ) ;
#29752 = CARTESIAN_POINT ( 'NONE',  ( -8.724201442159989384, 1437.633719118000045, 210.3032200441300290 ) ) ;
#29753 = CARTESIAN_POINT ( 'NONE',  ( -4.992640508427165003, 1391.632012742867346, 214.6223054488346236 ) ) ;
#29754 = CARTESIAN_POINT ( 'NONE',  ( -30.23606167549999668, 1467.592994008429969, 267.4627077489980138 ) ) ;
#29755 = CARTESIAN_POINT ( 'NONE',  ( -11.86216586729469924, 1481.732520156779856, 209.5386625665159954 ) ) ;
#29756 = CARTESIAN_POINT ( 'NONE',  ( 8.000564228190230054, 1425.311446220280004, 211.1882531427259835 ) ) ;
#29757 = CARTESIAN_POINT ( 'NONE',  ( -26.34628868930000323, 1509.610132138230028, 218.5686156305380052 ) ) ;
#29758 = CARTESIAN_POINT ( 'NONE',  ( -94.86324456277120021, 1384.610306623129873, 310.0067647644390263 ) ) ;
#29759 = CARTESIAN_POINT ( 'NONE',  ( -34.43103305585869833, 1384.977506179140164, 208.2997256558550134 ) ) ;
#29760 = CARTESIAN_POINT ( 'NONE',  ( -12.02051106306990036, 1491.153688555679992, 206.6632162730240054 ) ) ;
#29761 = CARTESIAN_POINT ( 'NONE',  ( -4.986960336344659517, 1508.551704408389924, 206.6058482952879842 ) ) ;
#29762 = DIRECTION ( 'NONE',  ( 0.3090169943749383474, 0.000000000000000000, -0.9510565162951566398 ) ) ;
#29763 = CIRCLE ( 'NONE', #22618, 5.000000000000000000 ) ;
#29764 = CARTESIAN_POINT ( 'NONE',  ( -2.472529913803013901, 1523.678648413191695, 175.3762130535718313 ) ) ;
#29766 = ORIENTED_EDGE ( 'NONE', *, *, #93229, .T. ) ;
#29765 = CARTESIAN_POINT ( 'NONE',  ( 11.49747572422220188, 1414.913060387329779, 220.3427040978150160 ) ) ;
#29767 = CARTESIAN_POINT ( 'NONE',  ( 3.192504087185560113, 1426.553239361320038, 224.5880228764589788 ) ) ;
#29768 = CARTESIAN_POINT ( 'NONE',  ( 4.554137863063505876, 1421.567652250969786, 137.7197909783843670 ) ) ;
#29769 =( BOUNDED_SURFACE ( )  B_SPLINE_SURFACE ( 3, 2, ( 
 ( #23410, #91722, #101760 ),
 ( #68213, #42421, #84961 ),
 ( #58690, #8255, #109096 ),
 ( #32378, #33451, #76579 ),
 ( #41332, #66558, #108526 ),
 ( #24500, #31818, #67652 ),
 ( #100126, #110731, #34020 ),
 ( #22842, #92823, #14453 ),
 ( #49194, #23946, #58142 ),
 ( #48646, #16094, #92274 ) ),
 .UNSPECIFIED., .F., .F., .F. ) 
 B_SPLINE_SURFACE_WITH_KNOTS ( ( 4, 2, 2, 2, 4 ),
 ( 3, 3 ),
 ( 1.570796326794896558, 1.963495408493620697, 2.356194490192344837, 2.748893571891068976, 3.141592653589793116 ),
 ( 0.000000000000000000, 1.000000000000000000 ),
 .UNSPECIFIED. ) 
 GEOMETRIC_REPRESENTATION_ITEM ( )  RATIONAL_B_SPLINE_SURFACE ( (
 ( 1.000000000000000000, 0.7071067811865813235, 1.000000000000000000),
 ( 1.000000000000000000, 0.7166207884823980745, 1.000000000000000000),
 ( 1.000000000000000000, 0.7259222650904582075, 1.000000000000000000),
 ( 1.000000000000000000, 0.7428408967932866869, 1.000000000000000000),
 ( 1.000000000000000000, 0.7504512394528688457, 1.000000000000000000),
 ( 1.000000000000000000, 0.7630177051946271938, 1.000000000000000000),
 ( 1.000000000000000000, 0.7679730451969652982, 1.000000000000000000),
 ( 1.000000000000000000, 0.7746454561800797389, 1.000000000000000000),
 ( 1.000000000000000000, 0.7763684247032546226, 1.000000000000000000),
 ( 1.000000000000000000, 0.7763623250684360544, 1.000000000000000000) ) ) 
 REPRESENTATION_ITEM ( '' )  SURFACE ( )  );
#29770 = CARTESIAN_POINT ( 'NONE',  ( 32.28466283162151029, 1511.187213306747708, 199.0684425896244250 ) ) ;
#29771 = CARTESIAN_POINT ( 'NONE',  ( -12.30733358380000020, 1416.021639799829927, 194.8879084977980085 ) ) ;
#29772 = DIRECTION ( 'NONE',  ( -0.000000000000000000, 1.000000000000000000, -0.000000000000000000 ) ) ;
#29773 = EDGE_CURVE ( 'NONE', #27781, #44537, #2188, .T. ) ;
#29774 = CARTESIAN_POINT ( 'NONE',  ( 23.43703390090000127, 1411.091823681130109, 212.1167532368579884 ) ) ;
#29775 = LINE ( 'NONE', #12963, #37640 ) ;
#29776 = CARTESIAN_POINT ( 'NONE',  ( -13.16170070989210039, 1468.332209647859827, 191.9366023383940103 ) ) ;
#29777 = CARTESIAN_POINT ( 'NONE',  ( -5.379917643342909450, 1430.657135788060032, 154.4490610592320081 ) ) ;
#29779 = CARTESIAN_POINT ( 'NONE',  ( -12.99813084100000005, 1380.049171561279991, 205.3172344645390126 ) ) ;
#29778 = CARTESIAN_POINT ( 'NONE',  ( -11.58636794539999926, 1433.009610086610110, 151.1946776885979773 ) ) ;
#29780 = CARTESIAN_POINT ( 'NONE',  ( 24.16765931996930306, 1411.086006809529863, 208.8198375941539950 ) ) ;
#29781 = CIRCLE ( 'NONE', #69136, 2.000000000000003553 ) ;
#29782 = CARTESIAN_POINT ( 'NONE',  ( -103.0889951380000156, 1378.528619065190696, 293.9108410952588883 ) ) ;
#29783 = EDGE_CURVE ( 'NONE', #86466, #50703, #46210, .T. ) ;
#29784 = CYLINDRICAL_SURFACE ( 'NONE', #74126, 0.9999999999999976685 ) ;
#29785 = CARTESIAN_POINT ( 'NONE',  ( -1.714310246450000186, 1417.458497559930038, 235.2631534898980021 ) ) ;
#29786 = CARTESIAN_POINT ( 'NONE',  ( 9.454737631250001328, 1363.431170718790099, 210.6218459616991936 ) ) ;
#29787 = ADVANCED_FACE ( 'NONE', ( #108470 ), #67210, .T. ) ;
#29788 = CARTESIAN_POINT ( 'NONE',  ( 1.120543697654999837, 1517.073005577650065, 205.0775260448770041 ) ) ;
#29789 = CARTESIAN_POINT ( 'NONE',  ( -12.88114576569580016, 1485.825225328749866, 185.4416202657009762 ) ) ;
#29790 = ORIENTED_EDGE ( 'NONE', *, *, #24089, .F. ) ;
#29791 = CARTESIAN_POINT ( 'NONE',  ( 7327.379741814554109, -2339.246371527899555, 11093.44175848640407 ) ) ;
#29792 = CARTESIAN_POINT ( 'NONE',  ( -13.59271798984216595, 1421.161248306587140, 210.6331271337394639 ) ) ;
#29794 = EDGE_LOOP ( 'NONE', ( #83200, #12437, #80397, #77565 ) ) ;
#29793 = CARTESIAN_POINT ( 'NONE',  ( -68.34593601010000441, 1379.747695174430191, 279.8829065415590094 ) ) ;
#29795 = ADVANCED_FACE ( 'NONE', ( #31754 ), #18893, .T. ) ;
#29796 = VERTEX_POINT ( 'NONE', #107911 ) ;
#29797 = CARTESIAN_POINT ( 'NONE',  ( 28.19408364699999936, 1508.123162656630029, 209.7484684564449822 ) ) ;
#29798 = ORIENTED_EDGE ( 'NONE', *, *, #45365, .F. ) ;
#29799 = CARTESIAN_POINT ( 'NONE',  ( -0.4215141012316919733, 1485.982418546980171, 221.0094681181439853 ) ) ;
#29800 = CARTESIAN_POINT ( 'NONE',  ( -109.8258757970000090, 1384.928269941609869, 311.3808033402589786 ) ) ;
#29802 = DIRECTION ( 'NONE',  ( 0.9993902469235412811, -0.03489947644508400310, -0.001077449749359506159 ) ) ;
#29801 = CARTESIAN_POINT ( 'NONE',  ( 1.554562095370000119, 1427.328278510630071, 123.0297916884979941 ) ) ;
#29803 = CARTESIAN_POINT ( 'NONE',  ( 4.045182479925000685, 1517.057265928030120, 210.8256255754569963 ) ) ;
#29804 = CARTESIAN_POINT ( 'NONE',  ( -25.39633370633140075, 1450.805127515380036, 137.3302824775919930 ) ) ;
#29805 = CARTESIAN_POINT ( 'NONE',  ( -105.7942887633819993, 1378.913060387289988, 304.0474587704230203 ) ) ;
#29806 = CARTESIAN_POINT ( 'NONE',  ( 14.78510249340000016, 1410.361618668330038, 227.6029314014980116 ) ) ;
#29807 = CARTESIAN_POINT ( 'NONE',  ( 10.38372441944459901, 1482.290969074429995, 211.4067775984080129 ) ) ;
#29808 = CARTESIAN_POINT ( 'NONE',  ( 0.000000000000000000, 0.000000000000000000, 0.000000000000000000 ) ) ;
#29809 = CARTESIAN_POINT ( 'NONE',  ( 40.02226351607779975, 1448.570981149600129, 134.0999999981999906 ) ) ;
#29810 = DIRECTION ( 'NONE',  ( 1.000000000000000000, 0.000000000000000000, 0.000000000000000000 ) ) ;
#29811 = ORIENTED_EDGE ( 'NONE', *, *, #51557, .F. ) ;
#29812 = CARTESIAN_POINT ( 'NONE',  ( 14.09229571774920053, 1435.068515943999955, 149.0020687653649816 ) ) ;
#29813 = CARTESIAN_POINT ( 'NONE',  ( -1.624243150411039949, 1431.539686916680012, 200.8843740557090030 ) ) ;
#29814 = VERTEX_POINT ( 'NONE', #65939 ) ;
#29815 = ORIENTED_EDGE ( 'NONE', *, *, #1905, .T. ) ;
#29816 = EDGE_LOOP ( 'NONE', ( #6264, #61447, #83967, #79508 ) ) ;
#29817 = CARTESIAN_POINT ( 'NONE',  ( -6.534620482165000688, 1514.642928591849795, 217.2407288984570073 ) ) ;
#29818 = DIRECTION ( 'NONE',  ( -6.505213034913001952E-16, 0.02617694830786544691, 0.9996573249755575929 ) ) ;
#29819 = CARTESIAN_POINT ( 'NONE',  ( 12.68801083313210043, 1500.413651417279880, 208.6561539661539939 ) ) ;
#29820 = CARTESIAN_POINT ( 'NONE',  ( -8.581591595879999090, 1384.915537926960042, 218.6697260928090145 ) ) ;
#29821 = ADVANCED_FACE ( 'NONE', ( #101148 ), #28645, .T. ) ;
#29822 = AXIS2_PLACEMENT_3D ( 'NONE', #105360, #14023, #88565 ) ;
#29823 = CARTESIAN_POINT ( 'NONE',  ( -18.29888576657991806, 1446.389289291960040, 215.5040569812714182 ) ) ;
#29824 = CARTESIAN_POINT ( 'NONE',  ( -67.63483993466537925, 1379.745623042401348, 277.6888451823470518 ) ) ;
#29825 = CARTESIAN_POINT ( 'NONE',  ( -1.828147983170000046, 1464.537159857190090, 199.0653224421989762 ) ) ;
#29826 = CARTESIAN_POINT ( 'NONE',  ( 5399.972634567438945, 2837.742859962510465, -8135.989823930170132 ) ) ;
#29827 = ADVANCED_FACE ( 'NONE', ( #20336 ), #81478, .T. ) ;
#29828 = CARTESIAN_POINT ( 'NONE',  ( 3.346431401090000257, 1414.913060387329779, 192.5065129705980098 ) ) ;
#29829 = CARTESIAN_POINT ( 'NONE',  ( -56.64330612835929912, 1384.653173750939914, 237.0538881573710057 ) ) ;
#29830 = EDGE_LOOP ( 'NONE', ( #35882, #52273, #71112, #58527 ) ) ;
#29831 = CARTESIAN_POINT ( 'NONE',  ( 5.770883563884999568, 1516.603620185149794, 206.8276363026970159 ) ) ;
#29832 = ORIENTED_EDGE ( 'NONE', *, *, #59162, .F. ) ;
#29833 = CARTESIAN_POINT ( 'NONE',  ( 30.90535300673260011, 1440.913060387330006, 253.9123373970340083 ) ) ;
#29834 = CARTESIAN_POINT ( 'NONE',  ( 19.03075101710000183, 1457.035589272129982, 226.5471405812980095 ) ) ;
#29835 = ORIENTED_EDGE ( 'NONE', *, *, #92867, .T. ) ;
#29836 = CARTESIAN_POINT ( 'NONE',  ( -0.3797365229449999879, 1451.158458254029938, 182.5593410785980097 ) ) ;
#29837 = CARTESIAN_POINT ( 'NONE',  ( -16.13865951880000082, 1410.848995608429959, 191.4167396153979723 ) ) ;
#29838 = CARTESIAN_POINT ( 'NONE',  ( -108.9547055214669058, 1384.162005982002484, 311.1881122995200144 ) ) ;
#29839 = CARTESIAN_POINT ( 'NONE',  ( -24.41186848160000267, 1440.913060429599909, 212.0284777738579862 ) ) ;
#29840 = CARTESIAN_POINT ( 'NONE',  ( 22.48215601709099687, 1410.706993422959840, 206.2088699951190165 ) ) ;
#29841 = CARTESIAN_POINT ( 'NONE',  ( -5.382074274746489806, 1511.451532973539770, 200.6334450727659942 ) ) ;
#29842 = CARTESIAN_POINT ( 'NONE',  ( 45.67177343720949523, 1440.913060382069943, 266.1885934449759930 ) ) ;
#29843 = CARTESIAN_POINT ( 'NONE',  ( -12.06120403350000103, 1433.903434619470090, 147.8551727352979981 ) ) ;
#29844 = CARTESIAN_POINT ( 'NONE',  ( 25.61452959376079974, 1479.968245174939966, 206.2236738490990149 ) ) ;
#29846 = CARTESIAN_POINT ( 'NONE',  ( -10.37023892357026611, 1423.186503347903454, 137.2231747537963429 ) ) ;
#29845 = CARTESIAN_POINT ( 'NONE',  ( 9.838112090859999270, 1463.224994908330018, 233.1087581964980018 ) ) ;
#29847 = AXIS2_PLACEMENT_3D ( 'NONE', #102550, #51630, #52194 ) ;
#29848 = CARTESIAN_POINT ( 'NONE',  ( -0.7391220051939990654, 1517.130100026000036, 216.0715493048870144 ) ) ;
#29849 = DIRECTION ( 'NONE',  ( 0.001614312349211209771, 0.06164810140419219736, -0.9980966414074828874 ) ) ;
#29850 = CARTESIAN_POINT ( 'NONE',  ( -1.925297167936410148, 1521.951704408389787, 187.5582988455250018 ) ) ;
#29851 = CARTESIAN_POINT ( 'NONE',  ( 19.41153299114838759, 1441.868806216761413, 212.6349187631244035 ) ) ;
#29852 = CARTESIAN_POINT ( 'NONE',  ( -6.935133418554999096, 1516.613881697390070, 212.3834819030570031 ) ) ;
#29853 = CARTESIAN_POINT ( 'NONE',  ( -19.63212482909999679, 1452.819910077329951, 209.4932260605140186 ) ) ;
#29854 = CARTESIAN_POINT ( 'NONE',  ( -7.790452417740089786, 1421.055847862326800, 137.0999999980979567 ) ) ;
#29856 = ORIENTED_EDGE ( 'NONE', *, *, #40817, .T. ) ;
#29855 = CARTESIAN_POINT ( 'NONE',  ( -113.4000000000000057, 1389.217440337809876, 308.7319511484590180 ) ) ;
#29857 = CARTESIAN_POINT ( 'NONE',  ( -9.094739560779999010, 1384.886008049520115, 199.9428817877490019 ) ) ;
#29858 = CARTESIAN_POINT ( 'NONE',  ( 24.51530987499999981, 1445.843072706799830, 217.4968709922580103 ) ) ;
#29859 = CARTESIAN_POINT ( 'NONE',  ( 7.883259769432120478, 1484.453481079082849, 216.4154215447759952 ) ) ;
#29860 = CARTESIAN_POINT ( 'NONE',  ( -15.33402440699999936, 1415.677402176539999, 208.4399661241280057 ) ) ;
#29861 = CARTESIAN_POINT ( 'NONE',  ( -1.417593344014799861, 1507.391024683259729, 237.1614008355199701 ) ) ;
#29862 = CARTESIAN_POINT ( 'NONE',  ( 16.73628186595820111, 1526.382868172864164, 184.0591879540915841 ) ) ;
#29863 = CARTESIAN_POINT ( 'NONE',  ( -17.26825932613299841, 1442.367707598380093, 217.4786320952890151 ) ) ;
#29865 = CARTESIAN_POINT ( 'NONE',  ( 19.02704169760000141, 1456.915441327430017, 225.6706379882980116 ) ) ;
#29864 = CARTESIAN_POINT ( 'NONE',  ( -20.17861002410000282, 1444.801920322949854, 223.8644076282979825 ) ) ;
#29867 = CARTESIAN_POINT ( 'NONE',  ( -2.201054711479999870, 1485.573836360929818, 182.5778603406980096 ) ) ;
#29866 = AXIS2_PLACEMENT_3D ( 'NONE', #19075, #53279, #36448 ) ;
#29868 = VERTEX_POINT ( 'NONE', #79725 ) ;
#29869 = CARTESIAN_POINT ( 'NONE',  ( 2.866857893004999713, 1516.951766529250108, 205.0784797119270024 ) ) ;
#29870 = CARTESIAN_POINT ( 'NONE',  ( 2.754936409899999994, 1406.324493345930023, 269.2919060128980391 ) ) ;
#29871 = CARTESIAN_POINT ( 'NONE',  ( -0.008839278001780500119, 1515.608558013090033, 213.1832674503789917 ) ) ;
#29872 = CARTESIAN_POINT ( 'NONE',  ( 23.75101318751531210, 1434.596239882524515, 214.4266028146048768 ) ) ;
#29873 = CARTESIAN_POINT ( 'NONE',  ( -0.7930666024419980031, 1471.115585716789838, 188.9853875966990131 ) ) ;
#29874 = CARTESIAN_POINT ( 'NONE',  ( 11.60004869885203860, 1422.462448494397904, 137.0350196580168642 ) ) ;
#29875 = CARTESIAN_POINT ( 'NONE',  ( -4.227540919128129460, 1441.218328383909920, 201.3833897788859986 ) ) ;
#29876 = CARTESIAN_POINT ( 'NONE',  ( -1.172951605644029893, 1450.815013396339964, 154.5169658199289984 ) ) ;
#29877 = CARTESIAN_POINT ( 'NONE',  ( -11.96786612770000069, 1446.201513125040037, 187.3303122566979937 ) ) ;
#29878 = CARTESIAN_POINT ( 'NONE',  ( 11.60004869885203682, 1428.983126981193436, 134.0999999980966777 ) ) ;
#29879 = CARTESIAN_POINT ( 'NONE',  ( -14.32414760834769929, 1416.073666499319870, 221.2545971180610138 ) ) ;
#29880 = CARTESIAN_POINT ( 'NONE',  ( -12.31997106265569997, 1378.116150552649970, 209.3647867733199917 ) ) ;
#29881 = CARTESIAN_POINT ( 'NONE',  ( -4.290289619920000241, 1420.418457352130190, 243.9198229428980085 ) ) ;
#29882 = CARTESIAN_POINT ( 'NONE',  ( 3.125595126769999954, 1441.073642980700015, 162.1945237037980121 ) ) ;
#29883 = CARTESIAN_POINT ( 'NONE',  ( -0.7656945474359999615, 1475.043758653330087, 269.6498827581980322 ) ) ;
#29884 = CARTESIAN_POINT ( 'NONE',  ( -33.29550038720000060, 1451.750386302530160, 134.7337860542980081 ) ) ;
#29885 = CARTESIAN_POINT ( 'NONE',  ( -10.96015512746500065, 1512.830284628050094, 193.2119433744669834 ) ) ;
#29886 = CARTESIAN_POINT ( 'NONE',  ( -3.958930064598830789, 1448.297290140811356, 185.0655646505161087 ) ) ;
#29887 = CARTESIAN_POINT ( 'NONE',  ( -34.64930450694949826, 1384.810489686140045, 233.7099306789210118 ) ) ;
#29888 = CARTESIAN_POINT ( 'NONE',  ( -105.7943137790000065, 1378.913060387289988, 304.0474592644590075 ) ) ;
#29889 = DIRECTION ( 'NONE',  ( 0.000000000000000000, 0.000000000000000000, -1.000000000000000000 ) ) ;
#29890 = CARTESIAN_POINT ( 'NONE',  ( 7.012921545474999796, 1508.551704408389924, 203.6084103740869864 ) ) ;
#29891 = CARTESIAN_POINT ( 'NONE',  ( -8.743415935682730122, 1396.218387199900008, 215.8871218720089757 ) ) ;
#29892 = CARTESIAN_POINT ( 'NONE',  ( -3.162549882268320012, 1508.551704408389924, 204.2260922363450106 ) ) ;
#29893 = CARTESIAN_POINT ( 'NONE',  ( -45.55153353979999764, 1438.765428390510124, 268.9770687238979576 ) ) ;
#29894 = EDGE_CURVE ( 'NONE', #46415, #101100, #95727, .T. ) ;
#29895 = EDGE_LOOP ( 'NONE', ( #48884, #23275, #92060, #18731 ) ) ;
#29896 = CARTESIAN_POINT ( 'NONE',  ( -11.38947975027659787, 1501.228585066793357, 208.0670107266517732 ) ) ;
#29897 = CARTESIAN_POINT ( 'NONE',  ( 2.559318562519999674, 1409.169965889630021, 231.1158913475979944 ) ) ;
#29898 = CARTESIAN_POINT ( 'NONE',  ( -18.97796697799288879, 1526.382868172864164, 232.9684741896490721 ) ) ;
#29899 =( BOUNDED_CURVE ( )  B_SPLINE_CURVE ( 3, ( #38391, #5347, #20469, #46284 ),
 .UNSPECIFIED., .F., .T. ) 
 B_SPLINE_CURVE_WITH_KNOTS ( ( 4, 4 ),
 ( 6.081914932523700301, 6.202477342412509920 ),
 .UNSPECIFIED. ) 
 CURVE ( )  GEOMETRIC_REPRESENTATION_ITEM ( )  RATIONAL_B_SPLINE_CURVE ( ( 1.000000000000000000, 0.9987890921955699941, 0.9987890921955699941, 1.000000000000000000 ) ) 
 REPRESENTATION_ITEM ( '' )  );
#29901 = CARTESIAN_POINT ( 'NONE',  ( -11.74136611096500005, 1511.863761374039996, 193.2704433220669955 ) ) ;
#29900 = CARTESIAN_POINT ( 'NONE',  ( 11.46601636529999979, 1425.973735423729750, 132.2042239505979921 ) ) ;
#29902 = CARTESIAN_POINT ( 'NONE',  ( 9230.682934795011533, 2837.541834147232294, -5630.801423131496449 ) ) ;
#29903 = CARTESIAN_POINT ( 'NONE',  ( -9.269849887880001305, 1450.024127290490014, 206.2237698193690107 ) ) ;
#29904 = CARTESIAN_POINT ( 'NONE',  ( 4.615644804385000022, 1517.009964551830080, 202.1744681489270192 ) ) ;
#29905 = CARTESIAN_POINT ( 'NONE',  ( 8.192509002470000468, 1427.073616020289819, 211.9190997776489951 ) ) ;
#29907 = CARTESIAN_POINT ( 'NONE',  ( -4.866999017969999564, 1428.784516533529995, 149.2390836726979728 ) ) ;
#29906 = AXIS2_PLACEMENT_3D ( 'NONE', #33823, #68015, #102125 ) ;
#29908 = CARTESIAN_POINT ( 'NONE',  ( 14.72576938353500076, 1512.123542805230272, 196.9321265835669976 ) ) ;
#29909 = CARTESIAN_POINT ( 'NONE',  ( 8.104522033453514851, 1514.095142040210703, 216.4523148511033526 ) ) ;
#29910 = CARTESIAN_POINT ( 'NONE',  ( -69.40599705544170206, 1377.319800895099888, 286.7245655447559898 ) ) ;
#29911 = CARTESIAN_POINT ( 'NONE',  ( 7.818221670743039198, 1367.736483592547984, 210.6218459616987957 ) ) ;
#29912 = B_SPLINE_CURVE_WITH_KNOTS ( 'NONE', 3,
 ( #43557, #101775, #75519, #77707 ),
 .UNSPECIFIED., .F., .F.,
 ( 4, 4 ),
 ( -157.6565403015839877, -140.7391984879999995 ),
 .UNSPECIFIED. ) ;
#29914 = VERTEX_POINT ( 'NONE', #55081 ) ;
#29913 = CARTESIAN_POINT ( 'NONE',  ( 4.429773585409299663, 1508.551704408389924, 204.3196163324640224 ) ) ;
#29915 = ORIENTED_EDGE ( 'NONE', *, *, #50102, .F. ) ;
#29916 = EDGE_CURVE ( 'NONE', #33810, #77151, #55513, .T. ) ;
#29917 = CARTESIAN_POINT ( 'NONE',  ( -9.777403739020000373, 1396.433055053929820, 201.5769308046579908 ) ) ;
#29918 = CARTESIAN_POINT ( 'NONE',  ( 2.922846155700570048, 1409.846762780129893, 231.4964038402399922 ) ) ;
#29919 = CARTESIAN_POINT ( 'NONE',  ( -4.035490750763682577, 1516.630499594219145, 201.4102953026068121 ) ) ;
#29920 = CARTESIAN_POINT ( 'NONE',  ( 0.4901645137037970446, 1507.127656893030007, 237.3576198934299839 ) ) ;
#29921 = DIRECTION ( 'NONE',  ( 0.000000000000000000, 0.000000000000000000, -1.000000000000000000 ) ) ;
#29922 = CARTESIAN_POINT ( 'NONE',  ( 18.11157372306810132, 1509.545530478630099, 186.5307137986639816 ) ) ;
#29924 = CARTESIAN_POINT ( 'NONE',  ( -1.361571319557159931, 1414.169512293919979, 185.4414444276949894 ) ) ;
#29923 = CARTESIAN_POINT ( 'NONE',  ( -103.5990824459999970, 1389.912137903419989, 305.4537645068589882 ) ) ;
#29925 = CARTESIAN_POINT ( 'NONE',  ( 4.507398563669999803, 1429.767108183030132, 185.3173098813979891 ) ) ;
#29926 = ADVANCED_FACE ( 'NONE', ( #19791 ), #11656, .T. ) ;
#29927 = CARTESIAN_POINT ( 'NONE',  ( -41.47274599670710415, 1445.558650626129975, 135.4388875029059989 ) ) ;
#29928 =( NAMED_UNIT ( * ) PLANE_ANGLE_UNIT ( ) SI_UNIT ( $, .RADIAN. ) );
#29929 = CARTESIAN_POINT ( 'NONE',  ( 41.49257586737849834, 1443.690994743030160, 136.5669662302249776 ) ) ;
#29930 = CARTESIAN_POINT ( 'NONE',  ( 7.279683625616689469, 1396.167272541620150, 217.4296586424180191 ) ) ;
#29931 = CARTESIAN_POINT ( 'NONE',  ( -39.43944535410179952, 1438.613980986869819, 136.5560418723989926 ) ) ;
#29932 = CARTESIAN_POINT ( 'NONE',  ( 11.76685707319999885, 1426.512066191629856, 146.4443102791980209 ) ) ;
#29933 = DIRECTION ( 'NONE',  ( 0.02616798426500965835, -0.9993150019883683122, 0.02616798426500970692 ) ) ;
#29934 = EDGE_LOOP ( 'NONE', ( #61677, #65918, #100995, #78271 ) ) ;
#29935 = FACE_OUTER_BOUND ( 'NONE', #89439, .T. ) ;
#29936 = CARTESIAN_POINT ( 'NONE',  ( 12.20994210559999971, 1442.197620241679942, 187.8251864636980031 ) ) ;
#29937 = VERTEX_POINT ( 'NONE', #63494 ) ;
#29938 = ORIENTED_EDGE ( 'NONE', *, *, #57916, .T. ) ;
#29939 = CARTESIAN_POINT ( 'NONE',  ( -17.44267318540000034, 1419.899571665260055, 205.5533046883089980 ) ) ;
#29940 = CARTESIAN_POINT ( 'NONE',  ( -11.39446592756109844, 1470.674086296440009, 209.5209556861319982 ) ) ;
#29941 = CARTESIAN_POINT ( 'NONE',  ( -13.89796033290000032, 1452.811554596829865, 194.9888671150980031 ) ) ;
#29942 = CARTESIAN_POINT ( 'NONE',  ( 29.78220350812341266, 1524.382868172863937, 196.5089261231631212 ) ) ;
#29943 = CARTESIAN_POINT ( 'NONE',  ( 5.007588646914999941, 1516.804776704140068, 214.8970827629769644 ) ) ;
#29944 = CARTESIAN_POINT ( 'NONE',  ( -14.49998591057999953, 1379.933159328379816, 208.5575498442950106 ) ) ;
#29945 = ORIENTED_EDGE ( 'NONE', *, *, #2868, .T. ) ;
#29946 = CARTESIAN_POINT ( 'NONE',  ( -16.73264916879790221, 1508.541854165810037, 213.2276336401049832 ) ) ;
#29947 = CARTESIAN_POINT ( 'NONE',  ( 2.500000000000000000, 1448.758219215480040, 157.1656513900349807 ) ) ;
#29948 = CARTESIAN_POINT ( 'NONE',  ( -55.15130194409999831, 1379.936376805820146, 253.2598301361589961 ) ) ;
#29949 = EDGE_CURVE ( 'NONE', #76707, #3640, #39435, .T. ) ;
#29950 = CARTESIAN_POINT ( 'NONE',  ( 18.18905553120000107, 1416.520322350429979, 213.0710787703080200 ) ) ;
#29951 = CARTESIAN_POINT ( 'NONE',  ( 7.711550677984999602, 1516.630499592039996, 205.0863552195469879 ) ) ;
#29953 = ORIENTED_EDGE ( 'NONE', *, *, #84660, .F. ) ;
#29952 = B_SPLINE_CURVE_WITH_KNOTS ( 'NONE', 3,
 ( #41924, #35727, #44142, #85009, #43585, #85556, #93965, #68804, #8852, #78278 ),
 .UNSPECIFIED., .F., .F.,
 ( 4, 2, 2, 2, 4 ),
 ( -0.2248365648612329903, -0.1535262906595619981, -0.1118204630139870148, -0.05103592384959870776, -1.415349781819230657E-10 ),
 .UNSPECIFIED. ) ;
#29954 = CARTESIAN_POINT ( 'NONE',  ( -29.86461515634900010, 1525.960063244516959, 220.9690070206027031 ) ) ;
#29955 = CARTESIAN_POINT ( 'NONE',  ( -31.14511482488981287, 1420.453826065711155, 269.4834250285384201 ) ) ;
#29956 = CARTESIAN_POINT ( 'NONE',  ( -3.805207261640000116, 1409.045941153030071, 230.7650822874980179 ) ) ;
#29958 = VERTEX_POINT ( 'NONE', #97614 ) ;
#29957 = CARTESIAN_POINT ( 'NONE',  ( -14.59882275810000074, 1475.513060387329915, 193.1404296630979900 ) ) ;
#29959 = CARTESIAN_POINT ( 'NONE',  ( 2.500000000000000000, 1421.075716575930073, 150.9130928818979953 ) ) ;
#29960 = CARTESIAN_POINT ( 'NONE',  ( -28.78732923508430019, 1440.913060387340010, 234.1936472594090048 ) ) ;
#29962 = CARTESIAN_POINT ( 'NONE',  ( -17.48604280480000028, 1384.189952027930076, 219.8991676458590234 ) ) ;
#29961 = AXIS2_PLACEMENT_3D ( 'NONE', #828, #84796, #24875 ) ;
#29963 = CARTESIAN_POINT ( 'NONE',  ( 9.788141164739998956, 1471.003676181789842, 212.2094840332690069 ) ) ;
#29964 = CARTESIAN_POINT ( 'NONE',  ( 42.85026807650999814, 1436.651183019170048, 270.2009488495780261 ) ) ;
#29965 = CARTESIAN_POINT ( 'NONE',  ( -3.446942109845000157, 1516.842852731759876, 212.3891375753969726 ) ) ;
#29966 = CARTESIAN_POINT ( 'NONE',  ( -64.02521122240000295, 1379.736828862030052, 270.2693837840589595 ) ) ;
#29967 = CIRCLE ( 'NONE', #67568, 8.800000000000000711 ) ;
#29968 = CARTESIAN_POINT ( 'NONE',  ( 23.85008871109999973, 1410.843070914130294, 208.1757528339269925 ) ) ;
#29969 = CARTESIAN_POINT ( 'NONE',  ( 29.13898522074257258, 1526.069472839378022, 197.1409705599812128 ) ) ;
#29970 = CARTESIAN_POINT ( 'NONE',  ( 7.950009656035348371, 1425.337175471099954, 192.9554219782069993 ) ) ;
#29971 = CARTESIAN_POINT ( 'NONE',  ( -7.710576472136819959, 1516.593294715559978, 210.4583376685390022 ) ) ;
#29972 = CARTESIAN_POINT ( 'NONE',  ( 4.037050997585000189, 1516.939819969850078, 209.1086255745840106 ) ) ;
#29973 = CARTESIAN_POINT ( 'NONE',  ( 4.228665902068920346, 1420.870217351630117, 185.4828094967849950 ) ) ;
#29974 = CARTESIAN_POINT ( 'NONE',  ( -0.9921696537889999057, 1415.381620563129900, 233.2736997477979912 ) ) ;
#29975 = CARTESIAN_POINT ( 'NONE',  ( -76.09571452209999620, 1384.765849691730182, 301.2247121768590432 ) ) ;
#29976 = ORIENTED_EDGE ( 'NONE', *, *, #70508, .T. ) ;
#29977 = CARTESIAN_POINT ( 'NONE',  ( -21.52308197379570132, 1385.270236681489905, 221.6137937885669942 ) ) ;
#29978 = CARTESIAN_POINT ( 'NONE',  ( -3.132406423129999951, 1429.005220112589996, 200.6955266824789987 ) ) ;
#29979 = CARTESIAN_POINT ( 'NONE',  ( 0.4681594785439999740, 1415.795094203329882, 233.3996825305979996 ) ) ;
#29980 = CARTESIAN_POINT ( 'NONE',  ( 4.491293115488566023, 1508.884207226183435, 206.6339108108618348 ) ) ;
#29981 = CARTESIAN_POINT ( 'NONE',  ( 7.588802682105000308, 1511.942942747529969, 206.8630203803070060 ) ) ;
#29982 = CARTESIAN_POINT ( 'NONE',  ( 10.78087825220000084, 1423.795965465850031, 203.9512493351290061 ) ) ;
#29983 = CARTESIAN_POINT ( 'NONE',  ( -11.86716023049999968, 1432.353341358199941, 147.6509521729980179 ) ) ;
#29985 = CARTESIAN_POINT ( 'NONE',  ( 22.08622291482331690, 1523.382868172864164, 184.4183880513174927 ) ) ;
#29984 = CARTESIAN_POINT ( 'NONE',  ( 5.005700201405000271, 1516.732530461250008, 216.0598116305469887 ) ) ;
#29986 = CARTESIAN_POINT ( 'NONE',  ( -0.08276393048689759113, 1408.915950567679829, 231.1937673021830051 ) ) ;
#29987 = CARTESIAN_POINT ( 'NONE',  ( 10.23249966253590060, 1470.172983095430254, 209.3814011399140043 ) ) ;
#29988 = CIRCLE ( 'NONE', #53197, 1.000000000000000888 ) ;
#29989 = EDGE_LOOP ( 'NONE', ( #76265, #60369, #9857, #83132, #79284 ) ) ;
#29990 = CARTESIAN_POINT ( 'NONE',  ( 4.034280915654999689, 1517.049325831759916, 202.1735242262370207 ) ) ;
#29991 = CARTESIAN_POINT ( 'NONE',  ( -3.827327205999999649, 1419.393213449430050, 165.4910337701979870 ) ) ;
#29992 = VERTEX_POINT ( 'NONE', #9736 ) ;
#29993 = CARTESIAN_POINT ( 'NONE',  ( -15.00522600296500819, 1511.839858410419993, 221.0503446609671414 ) ) ;
#29994 = CARTESIAN_POINT ( 'NONE',  ( 18.21091508359999978, 1429.914989560089907, 210.0150344289870077 ) ) ;
#29995 = CARTESIAN_POINT ( 'NONE',  ( 7.571416212307459759, 1423.019345442000031, 195.7264161909869813 ) ) ;
#29996 = CARTESIAN_POINT ( 'NONE',  ( 2.906162801440000276, 1443.249005831489967, 217.5410957172989868 ) ) ;
#29997 = CARTESIAN_POINT ( 'NONE',  ( -27.06354385267519902, 1509.473110589510043, 201.2587778061670178 ) ) ;
#29998 = CARTESIAN_POINT ( 'NONE',  ( -4.222550915200000254, 1446.229941110429991, 170.5491765577980061 ) ) ;
#29999 = CARTESIAN_POINT ( 'NONE',  ( -20.17846522170000156, 1427.578677867830038, 222.8742699695980320 ) ) ;
#30000 = CARTESIAN_POINT ( 'NONE',  ( 5.255993420997609356, 1486.130296503567479, 199.6624549764852361 ) ) ;
#30001 = CARTESIAN_POINT ( 'NONE',  ( -107.9977940029999957, 1389.297716649579797, 298.4487110492589750 ) ) ;
#30002 = CARTESIAN_POINT ( 'NONE',  ( 15.66025028199999980, 1508.960093224430011, 186.3692160812979921 ) ) ;
#30004 = CARTESIAN_POINT ( 'NONE',  ( 29.27919548120000215, 1509.872435206929822, 209.3677808018739768 ) ) ;
#30003 = CARTESIAN_POINT ( 'NONE',  ( -106.5586238660000049, 1390.939237335530152, 300.3883543639590243 ) ) ;
#30005 = CARTESIAN_POINT ( 'NONE',  ( 2.456601303385837820, 1523.611961620354123, 242.9433449337720958 ) ) ;
#30006 = VERTEX_POINT ( 'NONE', #10859 ) ;
#30007 = PLANE ( 'NONE',  #24830 ) ;
#30008 = CARTESIAN_POINT ( 'NONE',  ( -16.32163428129999971, 1508.551704408389924, 213.4489811870489859 ) ) ;
#30009 = CARTESIAN_POINT ( 'NONE',  ( -30.31643683090000962, 1523.530935881284904, 195.7504610701758168 ) ) ;
#30010 = AXIS2_PLACEMENT_3D ( 'NONE', #1568, #86652, #52521 ) ;
#30011 = CARTESIAN_POINT ( 'NONE',  ( -16.19493240869999795, 1409.478599888930148, 193.4350318414979881 ) ) ;
#30012 = CARTESIAN_POINT ( 'NONE',  ( -3.994321347890000151, 1485.012103865790095, 198.3399482330989940 ) ) ;
#30013 = CARTESIAN_POINT ( 'NONE',  ( -18.70459388229999931, 1509.566239198729818, 231.7064163648979900 ) ) ;
#30014 = CARTESIAN_POINT ( 'NONE',  ( -2.487422374635116284, 1523.954924407802764, 242.7965478622698754 ) ) ;
#30015 = CARTESIAN_POINT ( 'NONE',  ( -13.51471643657749233, 1443.999204071515123, 187.1185524397720314 ) ) ;
#30016 = CARTESIAN_POINT ( 'NONE',  ( -17.35267692490000258, 1414.988015876730060, 207.7949262638379935 ) ) ;
#30017 = CARTESIAN_POINT ( 'NONE',  ( 3.246772394788718596, 1512.187213306747481, 177.1492560608742508 ) ) ;
#30018 = CARTESIAN_POINT ( 'NONE',  ( -21.47379552819999660, 1487.892728108790152, 202.0847255913190281 ) ) ;
#30019 = CARTESIAN_POINT ( 'NONE',  ( -14.49777094512960041, 1415.677402205530143, 205.4885795654869867 ) ) ;
#30020 = CARTESIAN_POINT ( 'NONE',  ( 18.71421116979999866, 1425.460417338532807, 226.6184583000981547 ) ) ;
#30021 = CARTESIAN_POINT ( 'NONE',  ( 5.055176732809999685, 1428.911752091890094, 215.9094460472589958 ) ) ;
#30023 = ORIENTED_EDGE ( 'NONE', *, *, #89234, .F. ) ;
#30022 = CARTESIAN_POINT ( 'NONE',  ( 21.92317828190000029, 1509.363426959629805, 190.7737838525980294 ) ) ;
#30024 = CARTESIAN_POINT ( 'NONE',  ( -98.44283016700001099, 1380.746464150679913, 298.5816860277590195 ) ) ;
#30025 = CARTESIAN_POINT ( 'NONE',  ( 12.92498206718109977, 1512.351864386150055, 224.3146316424329711 ) ) ;
#30026 = VERTEX_POINT ( 'NONE', #95408 ) ;
#30027 = VERTEX_POINT ( 'NONE', #18670 ) ;
#30028 = CARTESIAN_POINT ( 'NONE',  ( -7.841538985989999766, 1492.606015770189970, 208.7602525851700079 ) ) ;
#30029 = CARTESIAN_POINT ( 'NONE',  ( 13.20876367099999982, 1507.490208233330122, 233.1223600710980008 ) ) ;
#30030 = CARTESIAN_POINT ( 'NONE',  ( -11.28831067177809011, 1378.749259193316448, 204.1390151436862368 ) ) ;
#30032 = CARTESIAN_POINT ( 'NONE',  ( -29.43658766909999969, 1455.581846392329908, 250.1802633725980343 ) ) ;
#30031 = CARTESIAN_POINT ( 'NONE',  ( 29.82222091440462819, 1419.446744514379134, 269.4689231808105205 ) ) ;
#30033 = CARTESIAN_POINT ( 'NONE',  ( 8.716659895241020806, 1437.048749725669950, 210.1866992012669755 ) ) ;
#30034 = AXIS2_PLACEMENT_3D ( 'NONE', #98601, #100266, #98047 ) ;
#30035 = CARTESIAN_POINT ( 'NONE',  ( -11.53856147429999979, 1433.624126597800114, 151.2408432088979851 ) ) ;
#30036 = B_SPLINE_CURVE_WITH_KNOTS ( 'NONE', 5,
 ( #98442, #5490, #39649, #31239, #73253, #13868, #74376, #46423, #72712, #91147, #21712, #99529, #57021, #81630, #106835, #39076, #55916, #30128, #90035, #14422, #48618 ),
 .UNSPECIFIED., .F., .F.,
 ( 6, 3, 3, 3, 3, 3, 6 ),
 ( 21.28770806440000030, 21.63383848259999809, 29.22288786549999884, 33.07574020050000030, 38.86051041610000567, 44.90455290039999880, 44.92446774270000276 ),
 .UNSPECIFIED. ) ;
#30037 = CARTESIAN_POINT ( 'NONE',  ( -19.63722818156799832, 1522.051704408389924, 200.0074286628000095 ) ) ;
#30038 = CARTESIAN_POINT ( 'NONE',  ( -19.11638574819999903, 1485.531016413629914, 189.6477890060980087 ) ) ;
#30039 = CARTESIAN_POINT ( 'NONE',  ( 9.120893397559440174, 1464.802252829569852, 212.8346682668349956 ) ) ;
#30040 = CIRCLE ( 'NONE', #6863, 0.9999999999999980016 ) ;
#30041 = CARTESIAN_POINT ( 'NONE',  ( -0.4260839224734093711, 1523.429859730329781, 244.8289481157578393 ) ) ;
#30042 = CARTESIAN_POINT ( 'NONE',  ( 0.5056391278744889473, 1515.143808641159922, 213.4492256370539849 ) ) ;
#30043 = CARTESIAN_POINT ( 'NONE',  ( 6.823170627169999669, 1439.352237894180007, 154.2706161131980025 ) ) ;
#30044 = CARTESIAN_POINT ( 'NONE',  ( -8.819768609920290103, 1478.884144629650109, 216.7505662143140057 ) ) ;
#30045 = AXIS2_PLACEMENT_3D ( 'NONE', #46027, #61192, #19693 ) ;
#30046 = CARTESIAN_POINT ( 'NONE',  ( -0.7618909056627740650, 1360.403425203244069, 210.6218459616987957 ) ) ;
#30047 = CARTESIAN_POINT ( 'NONE',  ( 31.74003925669979154, 1524.382868172804365, 201.6871716353068109 ) ) ;
#30049 = ORIENTED_EDGE ( 'NONE', *, *, #39779, .F. ) ;
#30048 = CARTESIAN_POINT ( 'NONE',  ( 6.691069722549889836E-09, 1409.748499752379985, 259.1747490247929591 ) ) ;
#30050 = ORIENTED_EDGE ( 'NONE', *, *, #22111, .T. ) ;
#30051 = CARTESIAN_POINT ( 'NONE',  ( -11.86440526039950072, 1432.217533829589911, 149.9810751051169859 ) ) ;
#30052 = VECTOR ( 'NONE', #33118, 1000.000000000000114 ) ;
#30053 = CARTESIAN_POINT ( 'NONE',  ( -21.45322466873749789, 1487.695354916500037, 202.0543356184059860 ) ) ;
#30054 = CARTESIAN_POINT ( 'NONE',  ( -27.75954458800000069, 1464.244195522129985, 269.7078801315980172 ) ) ;
#30055 = CARTESIAN_POINT ( 'NONE',  ( 9.209290677350001175, 1421.000200739789989, 196.8939171836989885 ) ) ;
#30056 = CARTESIAN_POINT ( 'NONE',  ( -204.2714532754874881, 1524.382868172863937, 194.5341519463070767 ) ) ;
#30057 = CARTESIAN_POINT ( 'NONE',  ( 33.93383221862509913, 1451.576073990769828, 135.5842236506620111 ) ) ;
#30058 = CARTESIAN_POINT ( 'NONE',  ( 4.326994892130289649, 1515.158502928330108, 209.1643610636710093 ) ) ;
#30059 = CARTESIAN_POINT ( 'NONE',  ( -11.56485986500000074, 1418.759067621630265, 229.1292871074979871 ) ) ;
#30060 = CARTESIAN_POINT ( 'NONE',  ( -15.95951032299999817, 1459.271785846329976, 230.7209114582980192 ) ) ;
#30061 = CARTESIAN_POINT ( 'NONE',  ( -3.316807713620000264, 1457.277897877190071, 218.1845740658989996 ) ) ;
#30062 = CARTESIAN_POINT ( 'NONE',  ( 10.48770262178695667, 1361.581614096479370, 209.6218459617033432 ) ) ;
#30063 = CARTESIAN_POINT ( 'NONE',  ( -27.20455118562970043, 1413.128951532790097, 269.2362726868500431 ) ) ;
#30064 = ORIENTED_EDGE ( 'NONE', *, *, #97224, .F. ) ;
#30065 = CARTESIAN_POINT ( 'NONE',  ( -3.531105454731040094, 1489.723025786869812, 181.7179317627199850 ) ) ;
#30066 = ORIENTED_EDGE ( 'NONE', *, *, #106664, .T. ) ;
#30067 = EDGE_LOOP ( 'NONE', ( #71041, #66138, #42369, #29131 ) ) ;
#30068 = CARTESIAN_POINT ( 'NONE',  ( -5.772978316675000166, 1516.659138130710289, 210.2536427808470023 ) ) ;
#30069 = CARTESIAN_POINT ( 'NONE',  ( 4.726680758722174858, 1423.629136535139196, 183.9804056333954065 ) ) ;
#30070 = VECTOR ( 'NONE', #11331, 1000.000000000000000 ) ;
#30072 = FILL_AREA_STYLE_COLOUR ( '', #79422 ) ;
#30071 = CARTESIAN_POINT ( 'NONE',  ( -4.995994825704999975, 1516.665179208830068, 211.6114635085770033 ) ) ;
#30073 = CARTESIAN_POINT ( 'NONE',  ( -13.98188209669999971, 1440.433068879009852, 188.7552081789980036 ) ) ;
#30074 = CARTESIAN_POINT ( 'NONE',  ( -8.324962519149999840E-16, 1519.913060387329779, 209.1218459616979999 ) ) ;
#30075 = VERTEX_POINT ( 'NONE', #97070 ) ;
#30076 = DIRECTION ( 'NONE',  ( 0.000000000000000000, 0.000000000000000000, 1.000000000000000000 ) ) ;
#30077 =( BOUNDED_CURVE ( )  B_SPLINE_CURVE ( 3, ( #77951, #78513, #86901, #12392 ),
 .UNSPECIFIED., .F., .F. ) 
 B_SPLINE_CURVE_WITH_KNOTS ( ( 4, 4 ),
 ( 2.436781329611980240, 3.141592653589793116 ),
 .UNSPECIFIED. ) 
 CURVE ( )  GEOMETRIC_REPRESENTATION_ITEM ( )  RATIONAL_B_SPLINE_CURVE ( ( 1.000000000000000000, 0.9590300661663084814, 0.9590300661663084814, 1.000000000000000000 ) ) 
 REPRESENTATION_ITEM ( '' )  );
#30078 = CARTESIAN_POINT ( 'NONE',  ( -6.555393155154999540, 1516.809497469189864, 201.7937966518470034 ) ) ;
#30079 = DIRECTION ( 'NONE',  ( -0.000000000000000000, -0.000000000000000000, 1.000000000000000000 ) ) ;
#30080 = CARTESIAN_POINT ( 'NONE',  ( -21.59949889905290021, 1384.536962887880009, 202.1273486796540055 ) ) ;
#30081 = CARTESIAN_POINT ( 'NONE',  ( -18.71766394247640264, 1412.839174955069893, 270.0884054360959681 ) ) ;
#30082 = CARTESIAN_POINT ( 'NONE',  ( -29.16177349730000046, 1435.516078635969961, 135.2137962254980152 ) ) ;
#30083 = DIRECTION ( 'NONE',  ( 0.000000000000000000, 0.000000000000000000, -1.000000000000000000 ) ) ;
#30085 = ORIENTED_EDGE ( 'NONE', *, *, #59616, .T. ) ;
#30084 = CARTESIAN_POINT ( 'NONE',  ( -9.690020260109999839, 1366.026910387849966, 207.6218459616989946 ) ) ;
#30086 = ORIENTED_EDGE ( 'NONE', *, *, #32618, .F. ) ;
#30087 = CARTESIAN_POINT ( 'NONE',  ( 35.99660812079667949, 1461.957472332656607, 269.2276724049037284 ) ) ;
#30088 = CARTESIAN_POINT ( 'NONE',  ( -3.076366055149999834, 1424.853903601579987, 191.3970713258989917 ) ) ;
#30089 = CARTESIAN_POINT ( 'NONE',  ( 19.21983641119999930, 1456.858306478489794, 206.3357454782189677 ) ) ;
#30090 = AXIS2_PLACEMENT_3D ( 'NONE', #18332, #96167, #28417 ) ;
#30091 = DIRECTION ( 'NONE',  ( -6.123233995736769734E-17, -1.000000000000000000, 0.000000000000000000 ) ) ;
#30092 = CARTESIAN_POINT ( 'NONE',  ( 6.951517132375000685, 1517.194816588360027, 210.2467400204669730 ) ) ;
#30093 = CARTESIAN_POINT ( 'NONE',  ( -18.33450183844069770, 1415.542389211280124, 207.5683613237780207 ) ) ;
#30094 = CARTESIAN_POINT ( 'NONE',  ( 5.456719627610000067, 1455.595244131089885, 218.2350948550090095 ) ) ;
#30095 = CARTESIAN_POINT ( 'NONE',  ( -14.66444439270000011, 1426.817899515830049, 221.8925448643979905 ) ) ;
#30096 = CARTESIAN_POINT ( 'NONE',  ( 12.00387303569999986, 1415.296882282229944, 222.4718873070980294 ) ) ;
#30097 = CARTESIAN_POINT ( 'NONE',  ( 8.213194853374998772, 1511.437978678640093, 205.0621741365669948 ) ) ;
#30098 = EDGE_LOOP ( 'NONE', ( #77196, #78416, #40895, #5462 ) ) ;
#30099 = CARTESIAN_POINT ( 'NONE',  ( 3.251888829344999898, 1516.793978928989873, 206.6294022811970024 ) ) ;
#30100 = ORIENTED_EDGE ( 'NONE', *, *, #104370, .T. ) ;
#30101 = CARTESIAN_POINT ( 'NONE',  ( -7.514943502936695552, 1426.327996137914170, 205.9160340660706652 ) ) ;
#30102 = CARTESIAN_POINT ( 'NONE',  ( -23.55479550185249948, 1448.068792179548609, 215.4543074554471787 ) ) ;
#30103 = EDGE_LOOP ( 'NONE', ( #93430, #86946, #42384, #104737 ) ) ;
#30104 = CARTESIAN_POINT ( 'NONE',  ( 17.95976239039625355, 1458.835784221633276, 228.1005955697006300 ) ) ;
#30105 = DIRECTION ( 'NONE',  ( -0.6736849260863841948, 0.000000000000000000, 0.7390186874254148774 ) ) ;
#30106 = CARTESIAN_POINT ( 'NONE',  ( -4.116702583572917185, 1440.040413356634190, 185.4452710716742558 ) ) ;
#30107 = CARTESIAN_POINT ( 'NONE',  ( 2.409586283469999923, 1426.663880916129983, 144.1938086916980239 ) ) ;
#30108 = CARTESIAN_POINT ( 'NONE',  ( 21.63007974809999823, 1410.588455781430184, 201.8364362340880120 ) ) ;
#30109 = DIRECTION ( 'NONE',  ( 0.000000000000000000, 0.000000000000000000, 1.000000000000000000 ) ) ;
#30110 = CARTESIAN_POINT ( 'NONE',  ( -27.12363451785340018, 1494.958770392079941, 210.5675194828440056 ) ) ;
#30111 = FACE_OUTER_BOUND ( 'NONE', #90658, .T. ) ;
#30112 = CARTESIAN_POINT ( 'NONE',  ( 30.31644210119978311, 1523.530870145309564, 222.4932309826555183 ) ) ;
#30113 = CARTESIAN_POINT ( 'NONE',  ( 24.34316872452072644, 1445.447417981560648, 214.1587588598165723 ) ) ;
#30114 = CARTESIAN_POINT ( 'NONE',  ( 2.500000000000000000, 1439.595905107460112, 166.5328618461109897 ) ) ;
#30115 = VECTOR ( 'NONE', #49090, 1000.000000000000000 ) ;
#30116 = CARTESIAN_POINT ( 'NONE',  ( -3.451033427095000050, 1517.025653221279981, 214.9083735325669977 ) ) ;
#30117 = VERTEX_POINT ( 'NONE', #88674 ) ;
#30118 = CARTESIAN_POINT ( 'NONE',  ( 7.711293535545939548, 1516.620679718459996, 207.9351109995780007 ) ) ;
#30119 = B_SPLINE_SURFACE_WITH_KNOTS ( 'NONE', 5, 5, ( 
 ( #74588, #74036, #57253, #33110, #101390, #6263, #110371, #101957, #91379 ),
 ( #48846, #108724, #15191, #5727, #59446, #33651, #24685, #58881, #93014 ),
 ( #93557, #16286, #32014, #48288, #82431, #76776, #68403, #10120, #28020 ),
 ( #26928, #17945, #62208, #44291, #61117, #70069, #18496, #60553, #78435 ),
 ( #25797, #94115, #34769, #93, #68956, #95232, #16829, #69509, #61653 ),
 ( #8451, #9013, #102507, #103059, #59996, #103631, #17386, #104181, #52692 ),
 ( #19047, #51584, #35321, #1748, #52141, #34217, #70611, #79006, #43186 ),
 ( #86273, #94674, #86828, #9559, #44854, #35886, #42624, #43729, #85716 ),
 ( #27465, #95780, #77882, #104731, #1190, #53249, #2308, #51031, #77338 ) ),
 .UNSPECIFIED., .F., .F., .F.,
 ( 6, 3, 6 ),
 ( 6, 3, 6 ),
 ( 1.672764195910000140, 7.352908628769999844, 11.41845199609999995 ),
 ( 0.000000000000000000, 1.000000000000000000, 2.000000000000000000 ),
 .UNSPECIFIED. ) ;
#30120 = CARTESIAN_POINT ( 'NONE',  ( -4.329791528864999961, 1515.051704408389924, 209.1218459511669892 ) ) ;
#30121 = AXIS2_PLACEMENT_3D ( 'NONE', #30732, #57068, #72754 ) ;
#30122 = CARTESIAN_POINT ( 'NONE',  ( -12.42529224677513078, 1522.051704408389924, 215.5613278979431868 ) ) ;
#30123 = EDGE_CURVE ( 'NONE', #103478, #52311, #95556, .T. ) ;
#30124 = CARTESIAN_POINT ( 'NONE',  ( -2.977093675850119858, 1421.750415281239839, 122.8791396966890090 ) ) ;
#30125 = EDGE_CURVE ( 'NONE', #22625, #51991, #44813, .T. ) ;
#30126 = CARTESIAN_POINT ( 'NONE',  ( -36.56841705501010154, 1449.771330042539830, 136.2670577573030073 ) ) ;
#30127 = CARTESIAN_POINT ( 'NONE',  ( 2.050360166999971590, 1417.315232216300956, 233.1613795969499847 ) ) ;
#30128 = CARTESIAN_POINT ( 'NONE',  ( -2.500000000000000000, 1419.382781980330037, 144.1108508878979819 ) ) ;
#30129 = ADVANCED_FACE ( 'NONE', ( #14133 ), #108757, .T. ) ;
#30130 = DIRECTION ( 'NONE',  ( -1.000000000000000000, 0.000000000000000000, 0.000000000000000000 ) ) ;
#30131 = CARTESIAN_POINT ( 'NONE',  ( -44.84558622350979817, 1443.398794768399966, 269.6928110531539460 ) ) ;
#30133 = EDGE_CURVE ( 'NONE', #7608, #28737, #78099, .T. ) ;
#30132 = CARTESIAN_POINT ( 'NONE',  ( 36.30692425169570470, 1440.913060387340010, 253.4096818480309707 ) ) ;
#30134 = CARTESIAN_POINT ( 'NONE',  ( -10.42483197617790047, 1470.891264593049982, 210.8225716954860047 ) ) ;
#30135 = FACE_OUTER_BOUND ( 'NONE', #90874, .T. ) ;
#30136 = ORIENTED_EDGE ( 'NONE', *, *, #84024, .T. ) ;
#30137 = LINE ( 'NONE', #14432, #105199 ) ;
#30138 = CARTESIAN_POINT ( 'NONE',  ( -1.831351320822103057, 1484.703635175746513, 182.8316381206172139 ) ) ;
#30139 = CARTESIAN_POINT ( 'NONE',  ( 12.40037417066400138, 1501.289366441759967, 211.7106409669050038 ) ) ;
#30140 = CIRCLE ( 'NONE', #92737, 2.500000000000002220 ) ;
#30141 = SPHERICAL_SURFACE ( 'NONE', #55694, 2.000000000000000000 ) ;
#30142 = CARTESIAN_POINT ( 'NONE',  ( -11.97313827979999878, 1507.452590393829951, 233.5302037296980018 ) ) ;
#30143 = CARTESIAN_POINT ( 'NONE',  ( -38.10078795722100153, 1383.831025482150153, 238.5878336628740044 ) ) ;
#30144 = CARTESIAN_POINT ( 'NONE',  ( -4.303235863005570039, 1508.728292324839913, 205.3335050028159969 ) ) ;
#30145 = CARTESIAN_POINT ( 'NONE',  ( 5.731992211021079697, 1423.315380817839923, 95.16526208845120038 ) ) ;
#30146 = EDGE_CURVE ( 'NONE', #21516, #37900, #27872, .T. ) ;
#30147 = DIRECTION ( 'NONE',  ( -0.03489949670250495212, 0.9993908270190956511, 0.000000000000000000 ) ) ;
#30148 = CARTESIAN_POINT ( 'NONE',  ( 2.439426257200000059, 1464.676489092029897, 236.7027241286980086 ) ) ;
#30150 = ORIENTED_EDGE ( 'NONE', *, *, #110461, .T. ) ;
#30149 = DIRECTION ( 'NONE',  ( 0.000000000000000000, 0.000000000000000000, 1.000000000000000000 ) ) ;
#30151 = CARTESIAN_POINT ( 'NONE',  ( -0.7117640835210000683, 1450.958351866529938, 182.0239507108979922 ) ) ;
#30152 = B_SPLINE_CURVE_WITH_KNOTS ( 'NONE', 3,
 ( #83256, #41800, #385, #101685, #49672, #24976, #59182, #93301, #84893, #42920, #100051 ),
 .UNSPECIFIED., .F., .F.,
 ( 4, 2, 1, 2, 2, 4 ),
 ( 0.000000000000000000, 0.2500000000008079648, 0.3750000000012119195, 0.4375000000012428947, 0.5000000000012738699, 1.000000000000000000 ),
 .UNSPECIFIED. ) ;
#30153 = CARTESIAN_POINT ( 'NONE',  ( -19.42552366969999866, 1382.322281656330006, 219.8856874478589987 ) ) ;
#30154 = CARTESIAN_POINT ( 'NONE',  ( 2.885329903193750045, 1508.551704408389924, 204.1651163175990007 ) ) ;
#30156 = ORIENTED_EDGE ( 'NONE', *, *, #108277, .T. ) ;
#30155 = LINE ( 'NONE', #5522, #109136 ) ;
#30157 = CARTESIAN_POINT ( 'NONE',  ( -19.58883200382760137, 1465.811229466620034, 204.1485211371180242 ) ) ;
#30158 = ORIENTED_EDGE ( 'NONE', *, *, #53746, .F. ) ;
#30159 = EDGE_CURVE ( 'NONE', #85608, #85844, #8183, .T. ) ;
#30160 = CARTESIAN_POINT ( 'NONE',  ( -8.968339577419470743, 1387.329609371060087, 218.0566458167560029 ) ) ;
#30161 = CARTESIAN_POINT ( 'NONE',  ( 76.99707197884903564, 1526.382868172863937, 19.35599459046138193 ) ) ;
#30162 = CARTESIAN_POINT ( 'NONE',  ( -10.76610293753739889, 1461.751116445120033, 211.3389343603909936 ) ) ;
#30163 = B_SPLINE_CURVE_WITH_KNOTS ( 'NONE', 3,
 ( #93631, #16910, #51115, #85239, #58961, #60078, #110457, #50011, #41042, #8535, #26439, #176, #33734, #102036 ),
 .UNSPECIFIED., .F., .F.,
 ( 4, 2, 2, 2, 2, 2, 4 ),
 ( 0.000000000000000000, 0.2499999999999910072, 0.3749999999999862887, 0.4999999999999815703, 0.6249999999999769074, 0.7499999999999721334, 1.000000000000000000 ),
 .UNSPECIFIED. ) ;
#30164 = ADVANCED_FACE ( 'NONE', ( #57287 ), #1469, .T. ) ;
#30165 = CARTESIAN_POINT ( 'NONE',  ( -5.819613099869999751, 1462.361531754390171, 201.2907114160189792 ) ) ;
#30166 = CARTESIAN_POINT ( 'NONE',  ( 34.18677586421188863, 1512.187213306747481, 219.7932833225211766 ) ) ;
#30167 = DIRECTION ( 'NONE',  ( 0.000000000000000000, 0.000000000000000000, -1.000000000000000000 ) ) ;
#30168 = CARTESIAN_POINT ( 'NONE',  ( 0.3281382665975389745, 1408.924519228060035, 194.1235352895430140 ) ) ;
#30169 = CARTESIAN_POINT ( 'NONE',  ( 18.03509922239999952, 1424.785625889029916, 224.8563120260980099 ) ) ;
#30170 = CARTESIAN_POINT ( 'NONE',  ( 4.637787270109999582, 1462.124489585889933, 228.1829287868989979 ) ) ;
#30171 = CARTESIAN_POINT ( 'NONE',  ( -18.91006071820000045, 1470.687815694929895, 190.2614882949980029 ) ) ;
#30172 = CARTESIAN_POINT ( 'NONE',  ( -3.920301378251832780, 1425.361100976067974, 186.0700639595226278 ) ) ;
#30173 = ORIENTED_EDGE ( 'NONE', *, *, #14490, .F. ) ;
#30174 = ORIENTED_EDGE ( 'NONE', *, *, #43168, .F. ) ;
#30175 = CARTESIAN_POINT ( 'NONE',  ( -7.512716754807339470, 1509.034509426269778, 215.2632450604789938 ) ) ;
#30176 = CARTESIAN_POINT ( 'NONE',  ( 2.500000000000000000, 1423.874532569730036, 167.3087045231979744 ) ) ;
#30177 = CARTESIAN_POINT ( 'NONE',  ( -12.07610166159999920, 1433.870589910030048, 149.7869025145980117 ) ) ;
#30178 = CARTESIAN_POINT ( 'NONE',  ( 19.39983987835401535, 1501.977400791986611, 178.9515629539735073 ) ) ;
#30179 = CARTESIAN_POINT ( 'NONE',  ( -20.43090246067709970, 1502.387636806920000, 190.5483151450440005 ) ) ;
#30180 = CARTESIAN_POINT ( 'NONE',  ( -15.30918010269999918, 1420.444122943519915, 211.1786203771790156 ) ) ;
#30181 = CARTESIAN_POINT ( 'NONE',  ( -109.1462309409999989, 1385.214558625939844, 311.2612093662589814 ) ) ;
#30182 = CARTESIAN_POINT ( 'NONE',  ( 0.1668199292400000255, 1482.197866754329880, 181.9999787962979951 ) ) ;
#30183 = CARTESIAN_POINT ( 'NONE',  ( -10.11455584700109966, 1367.169308473507954, 207.6218459616987673 ) ) ;
#30184 = CARTESIAN_POINT ( 'NONE',  ( -5.843535329920999999, 1389.008761609309886, 209.1218459616989946 ) ) ;
#30185 = CARTESIAN_POINT ( 'NONE',  ( -13.15726454016349933, 1414.996443537369942, 220.4820293315119955 ) ) ;
#30186 = CARTESIAN_POINT ( 'NONE',  ( -2.493697079054999932, 1516.977201124959947, 208.0034927161370035 ) ) ;
#30187 = CARTESIAN_POINT ( 'NONE',  ( -9.109439661327298765, 1447.385667508870029, 211.8713842478840093 ) ) ;
#30188 = CARTESIAN_POINT ( 'NONE',  ( 6.688848995729999913, 1408.965348139829985, 221.4809136123979840 ) ) ;
#30189 = AXIS2_PLACEMENT_3D ( 'NONE', #87634, #27715, #36671 ) ;
#30190 = CARTESIAN_POINT ( 'NONE',  ( -13.69143447902490074, 1435.956672119230007, 150.3296684258739901 ) ) ;
#30191 = CARTESIAN_POINT ( 'NONE',  ( -8.296211591059998725, 1385.071719360819998, 218.6997762507590153 ) ) ;
#30192 = CARTESIAN_POINT ( 'NONE',  ( -1.531858734065989602E-13, 1515.051704408389924, 205.2922258481490303 ) ) ;
#30193 = CARTESIAN_POINT ( 'NONE',  ( 7.526607499040649962, 1425.472659576630122, 212.1966582396349850 ) ) ;
#30195 = CARTESIAN_POINT ( 'NONE',  ( -6.415996146495579922, 1495.304407762119808, 203.8734489153730181 ) ) ;
#30194 = AXIS2_PLACEMENT_3D ( 'NONE', #82728, #50249, #41822 ) ;
#30196 = EDGE_LOOP ( 'NONE', ( #62930, #100008, #21829, #76379, #20491 ) ) ;
#30197 = VECTOR ( 'NONE', #81623, 1000.000000000000000 ) ;
#30198 = CARTESIAN_POINT ( 'NONE',  ( -5.356004379399999768E-09, 1414.987262868229891, 244.5742075744979900 ) ) ;
#30199 = DIRECTION ( 'NONE',  ( -0.6736849260863841948, 0.000000000000000000, 0.7390186874254148774 ) ) ;
#30201 = CARTESIAN_POINT ( 'NONE',  ( -17.84751309889999860, 1410.898165759730091, 195.0518225682980074 ) ) ;
#30200 = CARTESIAN_POINT ( 'NONE',  ( -1.539676316830000058, 1499.384663382030112, 181.1309619126980124 ) ) ;
#30202 = CARTESIAN_POINT ( 'NONE',  ( -9.945114259093980280, 1408.453226861988469, 270.1158808274767011 ) ) ;
#30203 = B_SPLINE_CURVE_WITH_KNOTS ( 'NONE', 5,
 ( #106577, #39372, #99255, #47231, #14712, #107682 ),
 .UNSPECIFIED., .F., .F.,
 ( 6, 6 ),
 ( -2.000000000000000000, 0.000000000000000000 ),
 .UNSPECIFIED. ) ;
#30204 = CARTESIAN_POINT ( 'NONE',  ( -21.02448267839999829, 1430.224264779530131, 216.3628553705179911 ) ) ;
#30205 = CARTESIAN_POINT ( 'NONE',  ( 1.977078070039999913, 1485.260289170789974, 220.8317664630990294 ) ) ;
#30206 = CARTESIAN_POINT ( 'NONE',  ( -4.994775864380000208, 1391.713558696990049, 214.4361776263990009 ) ) ;
#30207 = CARTESIAN_POINT ( 'NONE',  ( 27.03405864349999987, 1451.816809924330073, 135.7882993078979723 ) ) ;
#30208 = ORIENTED_EDGE ( 'NONE', *, *, #61687, .T. ) ;
#30209 = CARTESIAN_POINT ( 'NONE',  ( 8.502412689479999841, 1494.223831056089921, 218.1490364173589853 ) ) ;
#30210 = CARTESIAN_POINT ( 'NONE',  ( 13.86354611765113454, 1513.912053484252510, 225.8081837123426965 ) ) ;
#30211 = CARTESIAN_POINT ( 'NONE',  ( 2.933320418000000096, 1509.029007662530148, 238.7073699979980006 ) ) ;
#30212 = ORIENTED_EDGE ( 'NONE', *, *, #83137, .F. ) ;
#30213 = VERTEX_POINT ( 'NONE', #80814 ) ;
#30214 = CARTESIAN_POINT ( 'NONE',  ( -3.078458355219999998, 1384.919541752539999, 199.6700055799090023 ) ) ;
#30215 = CARTESIAN_POINT ( 'NONE',  ( -23.59088797105159685, 1410.013994075070059, 208.8666440682279983 ) ) ;
#30216 = EDGE_CURVE ( 'NONE', #19615, #6924, #6189, .T. ) ;
#30217 = ORIENTED_EDGE ( 'NONE', *, *, #2105, .T. ) ;
#30218 = CARTESIAN_POINT ( 'NONE',  ( 4.987078429521930367, 1508.551704408389924, 205.6342618271569904 ) ) ;
#30219 = CIRCLE ( 'NONE', #19433, 3.458500000000000352 ) ;
#30220 = DIRECTION ( 'NONE',  ( -5.980589973904019347E-17, 1.000000000000000000, -1.736889445713099699E-16 ) ) ;
#30221 = EDGE_CURVE ( 'NONE', #100346, #102937, #21420, .T. ) ;
#30222 = CARTESIAN_POINT ( 'NONE',  ( -5.750276878030000205, 1489.057775212530032, 235.2475806271980048 ) ) ;
#30223 = CARTESIAN_POINT ( 'NONE',  ( 16.73628186595829703, 1526.382868172864164, 234.1845039693042452 ) ) ;
#30224 = ORIENTED_EDGE ( 'NONE', *, *, #100195, .F. ) ;
#30225 = CARTESIAN_POINT ( 'NONE',  ( 45.88361587542109987, 1440.912968092909750, 266.4122210649330214 ) ) ;
#30226 = CARTESIAN_POINT ( 'NONE',  ( -3.487585887351170033, 1508.611352722540005, 204.4436967865070187 ) ) ;
#30227 = CARTESIAN_POINT ( 'NONE',  ( -7.211414364699999524, 1427.415731310709816, 205.0259060341190320 ) ) ;
#30228 = CARTESIAN_POINT ( 'NONE',  ( -0.7553264739829980146, 1516.745833913490060, 203.3462208547369983 ) ) ;
#30229 = ORIENTED_EDGE ( 'NONE', *, *, #38446, .T. ) ;
#30230 = CARTESIAN_POINT ( 'NONE',  ( 9.695302103464010557, 1481.887598573820014, 215.8648280851800223 ) ) ;
#30231 = EDGE_CURVE ( 'NONE', #41801, #25418, #76699, .T. ) ;
#30232 = CARTESIAN_POINT ( 'NONE',  ( 12.91578402941177117, 1442.900078521421165, 187.0543600294182625 ) ) ;
#30233 = VERTEX_POINT ( 'NONE', #34253 ) ;
#30234 = ORIENTED_EDGE ( 'NONE', *, *, #50251, .F. ) ;
#30235 = CARTESIAN_POINT ( 'NONE',  ( -11.42573944687380028, 1481.783086644220020, 208.8678723980630139 ) ) ;
#30236 = CARTESIAN_POINT ( 'NONE',  ( -2.701523881276569838, 1508.230667595090154, 220.7992134743510064 ) ) ;
#30237 = CARTESIAN_POINT ( 'NONE',  ( 10.83158213179999940, 1507.705498442529915, 234.1612671678980178 ) ) ;
#30238 = CARTESIAN_POINT ( 'NONE',  ( -12.29919906773779914, 1512.135905030570029, 194.2944855735010208 ) ) ;
#30239 = CARTESIAN_POINT ( 'NONE',  ( 18.87058201889760412, 1452.254085142500116, 144.5211760892889856 ) ) ;
#30240 = CARTESIAN_POINT ( 'NONE',  ( 12.49185799700000032, 1420.539304375840175, 200.4619042918790228 ) ) ;
#30241 = CARTESIAN_POINT ( 'NONE',  ( -1.737082865695850131, 1434.406546800360047, 227.4539720509420135 ) ) ;
#30242 = CARTESIAN_POINT ( 'NONE',  ( -6.653371456881099988, 1494.411565237649938, 198.7567593804810144 ) ) ;
#30243 = CARTESIAN_POINT ( 'NONE',  ( 11.21925624861339976, 1478.674995329209878, 205.8722235859200111 ) ) ;
#30244 = CARTESIAN_POINT ( 'NONE',  ( 0.03557119914497085950, 1409.441096220073405, 232.8945654604514175 ) ) ;
#30246 = CARTESIAN_POINT ( 'NONE',  ( -3.526376118873112198, 1486.285438481868141, 181.8638835509612761 ) ) ;
#30245 = CARTESIAN_POINT ( 'NONE',  ( -13.78893342798370014, 1434.978972382549955, 148.5514418732119850 ) ) ;
#30247 = CARTESIAN_POINT ( 'NONE',  ( 12.09770740671049971, 1421.784375224090127, 207.3870252319539986 ) ) ;
#30248 = CARTESIAN_POINT ( 'NONE',  ( -9.843485560008819135, 1439.940105572409948, 207.3006424506950225 ) ) ;
#30249 = EDGE_CURVE ( 'NONE', #64180, #52333, #56818, .T. ) ;
#30250 = CARTESIAN_POINT ( 'NONE',  ( -7.468172886755000128, 1513.423632355020118, 202.6515140566669970 ) ) ;
#30251 = ORIENTED_EDGE ( 'NONE', *, *, #29058, .T. ) ;
#30252 = CARTESIAN_POINT ( 'NONE',  ( 12.96503937710000010, 1476.856299447390029, 225.6431713718990011 ) ) ;
#30253 = CIRCLE ( 'NONE', #42742, 1.999999999999998668 ) ;
#30254 = CARTESIAN_POINT ( 'NONE',  ( -17.33645362950000290, 1414.996442546130083, 207.8511177337479978 ) ) ;
#30255 = CARTESIAN_POINT ( 'NONE',  ( -86.03043292017589749, 1384.978873078290235, 307.1765789634189900 ) ) ;
#30256 = B_SPLINE_SURFACE_WITH_KNOTS ( 'NONE', 5, 5, ( 
 ( #60769, #104950, #28241, #51798, #61330, #10329, #62430, #9240, #94893 ),
 ( #19828, #85366, #78649, #43397, #42839, #76999, #1964, #77547, #36101 ),
 ( #95994, #70287, #89247, #106057, #97106, #20922, #12543, #90332, #99277 ),
 ( #81935, #88163, #80305, #22003, #54034, #65161, #37749, #62999, #106596 ),
 ( #11993, #37200, #38283, #38829, #56198, #47250, #97651, #13612, #47799 ),
 ( #20372, #30436, #81375, #89793, #64622, #46176, #71395, #55125, #105510 ),
 ( #98189, #46722, #5238, #80855, #11450, #30986, #45626, #29881, #71945 ),
 ( #3622, #39394, #3073, #29334, #63536, #28801, #79766, #54578, #4157 ),
 ( #64071, #55671, #4690, #21461, #107702, #13065, #88713, #73569, #98742 ),
 ( #72466, #73008, #107144, #67376, #57867, #7986, #41039, #14733, #6884 ),
 ( #76304, #48364, #58959, #91455, #74667, #41605, #15803, #75218, #100927 ),
 ( #66282, #23682, #75759, #100398, #84688, #33186, #90892, #92535, #14177 ) ),
 .UNSPECIFIED., .F., .F., .F.,
 ( 6, 3, 3, 6 ),
 ( 6, 3, 6 ),
 ( 0.000000000000000000, 17.84603210599999912, 40.51038747020000130, 67.03953034199999195 ),
 ( 168.7272174100000086, 210.9090217629999984, 253.0908261149999987 ),
 .UNSPECIFIED. ) ;
#30257 = ADVANCED_FACE ( 'NONE', ( #75175 ), #7400, .F. ) ;
#30258 = CARTESIAN_POINT ( 'NONE',  ( -9.236133890019999626, 1386.337655059579902, 200.2251704754490333 ) ) ;
#30259 = CARTESIAN_POINT ( 'NONE',  ( -15.62936356099999990, 1415.849185049640028, 210.3397193722490215 ) ) ;
#30261 = EDGE_LOOP ( 'NONE', ( #22116, #36918, #66490, #80621 ) ) ;
#30260 = CARTESIAN_POINT ( 'NONE',  ( -17.21782089171700036, 1419.893479116660046, 207.5604823166399910 ) ) ;
#30262 = EDGE_CURVE ( 'NONE', #60533, #106936, #92493, .T. ) ;
#30263 = CARTESIAN_POINT ( 'NONE',  ( -16.90409255678397571, 1417.172264864735780, 207.4840029039214357 ) ) ;
#30264 = CARTESIAN_POINT ( 'NONE',  ( -2.471608048749999842, 1438.194204504490017, 150.4833623973980252 ) ) ;
#30265 = AXIS2_PLACEMENT_3D ( 'NONE', #10788, #18596, #79657 ) ;
#30266 = CARTESIAN_POINT ( 'NONE',  ( -7.892061334917592319, 1477.019624418719332, 215.8670058585243794 ) ) ;
#30267 = CARTESIAN_POINT ( 'NONE',  ( -19.56156973859999937, 1464.807986927590036, 211.9767427593990021 ) ) ;
#30268 = CARTESIAN_POINT ( 'NONE',  ( 14.69977922143499960, 1513.518111364920060, 224.7800584559669801 ) ) ;
#30269 = CARTESIAN_POINT ( 'NONE',  ( -15.90990259576500065, 1516.551704408390151, 220.0820010595669771 ) ) ;
#30270 = CARTESIAN_POINT ( 'NONE',  ( 6.193779543994120118, 1460.064517498830128, 201.5421853323860262 ) ) ;
#30271 = CYLINDRICAL_SURFACE ( 'NONE', #21506, 1.000000000000000888 ) ;
#30272 = CARTESIAN_POINT ( 'NONE',  ( 14.65669493600000095, 1419.764842872129975, 228.1228079084980038 ) ) ;
#30273 = EDGE_CURVE ( 'NONE', #80494, #85181, #65456, .T. ) ;
#30274 = CARTESIAN_POINT ( 'NONE',  ( -21.41029105011321576, 1526.329757971584741, 234.0206363885986320 ) ) ;
#30275 = CARTESIAN_POINT ( 'NONE',  ( -2.299983615734999987, 1516.861367446839949, 206.8392230197369770 ) ) ;
#30276 = DIRECTION ( 'NONE',  ( 0.5877852522924709167, 0.000000000000000000, 0.8090169943749491166 ) ) ;
#30277 = CARTESIAN_POINT ( 'NONE',  ( -18.39234877020000170, 1409.555335359829996, 222.0045018765979705 ) ) ;
#30278 = CARTESIAN_POINT ( 'NONE',  ( 15.08830123919999977, 1435.136539919019924, 148.7677820923979937 ) ) ;
#30279 = CIRCLE ( 'NONE', #92864, 1.000004583512053902 ) ;
#30280 = CARTESIAN_POINT ( 'NONE',  ( -1.120746172849999889, 1422.344552812930033, 228.3276896694979996 ) ) ;
#30281 = EDGE_CURVE ( 'NONE', #23487, #8175, #76846, .T. ) ;
#30282 = CARTESIAN_POINT ( 'NONE',  ( -10.32735784461773498, 1511.163060387329779, 184.1749888460368538 ) ) ;
#30283 = CARTESIAN_POINT ( 'NONE',  ( 0.008608266560750518770, 1515.483924129489878, 204.8869941145489975 ) ) ;
#30284 = CARTESIAN_POINT ( 'NONE',  ( -14.70760701499460055, 1417.599750256749985, 203.2440078780049646 ) ) ;
#30285 = CARTESIAN_POINT ( 'NONE',  ( -36.36970013105189992, 1437.503838517560098, 136.5330191489490232 ) ) ;
#30286 = CARTESIAN_POINT ( 'NONE',  ( 0.2133752674872349819, 1455.455537353240061, 183.1480552562999833 ) ) ;
#30287 = CARTESIAN_POINT ( 'NONE',  ( -8.866214871307620982, 1407.269089423789865, 199.4203128504979929 ) ) ;
#30288 = CARTESIAN_POINT ( 'NONE',  ( -13.01304944610000192, 1416.520646107730045, 196.6194520801979877 ) ) ;
#30289 = CARTESIAN_POINT ( 'NONE',  ( 18.15646965371242771, 1522.906363951597314, 180.0767137688687001 ) ) ;
#30290 = CARTESIAN_POINT ( 'NONE',  ( 1.988539752888069279, 1484.903804446283630, 198.5396525162173305 ) ) ;
#30291 = CARTESIAN_POINT ( 'NONE',  ( 13.19881100609999969, 1434.900409811350073, 147.9457237049980165 ) ) ;
#30292 = CARTESIAN_POINT ( 'NONE',  ( -39.48425676843219634, 1438.208629469910193, 134.0999999978120059 ) ) ;
#30293 = CARTESIAN_POINT ( 'NONE',  ( 3.918670472299999208, 1441.329835342249908, 183.9132893515979958 ) ) ;
#30294 = VERTEX_POINT ( 'NONE', #110409 ) ;
#30295 = FACE_OUTER_BOUND ( 'NONE', #38093, .T. ) ;
#30296 = CARTESIAN_POINT ( 'NONE',  ( 4.757611653739999724, 1476.697157691990014, 198.4937409947989977 ) ) ;
#30297 = CARTESIAN_POINT ( 'NONE',  ( -8.169456507803459999, 1409.198344094930007, 221.6608919718729851 ) ) ;
#30298 = CARTESIAN_POINT ( 'NONE',  ( -11.15721983490000113, 1491.329444167089832, 209.2379587012340210 ) ) ;
#30299 = ADVANCED_FACE ( 'NONE', ( #674 ), #100884, .F. ) ;
#30300 = DIRECTION ( 'NONE',  ( 0.000000000000000000, 0.000000000000000000, -1.000000000000000000 ) ) ;
#30301 = CARTESIAN_POINT ( 'NONE',  ( 13.45330080894279945, 1508.683615153560140, 233.3158278350460080 ) ) ;
#30302 = CARTESIAN_POINT ( 'NONE',  ( 31.99856245131003263, 1416.544800951289290, 269.3157470449859829 ) ) ;
#30303 = VECTOR ( 'NONE', #34667, 1000.000000000000000 ) ;
#30304 = CARTESIAN_POINT ( 'NONE',  ( 19.44845634410000201, 1435.008643399599805, 209.6929102032310084 ) ) ;
#30305 = EDGE_CURVE ( 'NONE', #26067, #100027, #71404, .T. ) ;
#30306 = CARTESIAN_POINT ( 'NONE',  ( -14.26063306530000041, 1380.301850145579920, 210.3217779679890214 ) ) ;
#30307 = CARTESIAN_POINT ( 'NONE',  ( -94.05632786852450522, 1384.611781857200185, 309.8312009487510181 ) ) ;
#30308 = CARTESIAN_POINT ( 'NONE',  ( -38.90163946207999857, 1384.987285049699949, 211.8655680313669905 ) ) ;
#30309 = CARTESIAN_POINT ( 'NONE',  ( -12.17471863065270021, 1490.831372364329809, 207.6427668900300034 ) ) ;
#30310 = CARTESIAN_POINT ( 'NONE',  ( 21.92444878910000483, 1509.678679009930192, 227.6602567687980070 ) ) ;
#30311 = ADVANCED_FACE ( 'NONE', ( #61154 ), #87424, .F. ) ;
#30312 = CARTESIAN_POINT ( 'NONE',  ( -28.43277596700509946, 1508.901247236620065, 208.8032485517010173 ) ) ;
#30313 = CARTESIAN_POINT ( 'NONE',  ( -2.621078202466434082, 1523.542365884045466, 176.0837307636415972 ) ) ;
#30315 = ORIENTED_EDGE ( 'NONE', *, *, #61170, .F. ) ;
#30314 = CARTESIAN_POINT ( 'NONE',  ( -3.123993097060000057, 1502.556458247589944, 230.3127639627990106 ) ) ;
#30316 = FACE_OUTER_BOUND ( 'NONE', #79587, .T. ) ;
#30317 = CARTESIAN_POINT ( 'NONE',  ( 9.787859445082000676, 1471.003474910739897, 212.2097121542219895 ) ) ;
#30318 = LINE ( 'NONE', #63419, #108785 ) ;
#30319 = CARTESIAN_POINT ( 'NONE',  ( -0.07918980841199839416, 1420.035738981420081, 183.9208618171100227 ) ) ;
#30320 = CARTESIAN_POINT ( 'NONE',  ( 0.000000000000000000, 1524.090675761330203, 209.1218459616979999 ) ) ;
#30321 = CIRCLE ( 'NONE', #57213, 0.9999999999999935607 ) ;
#30322 = CARTESIAN_POINT ( 'NONE',  ( 21.35611516500000207, 1409.658832362230214, 213.8729625945780128 ) ) ;
#30323 = DIRECTION ( 'NONE',  ( 1.000000000000000000, 6.438963419392920087E-12, 0.000000000000000000 ) ) ;
#30324 = CARTESIAN_POINT ( 'NONE',  ( -18.29499256740350077, 1465.862032733680053, 217.7259485429990207 ) ) ;
#30325 = CARTESIAN_POINT ( 'NONE',  ( -17.55365457510000127, 1423.589371376930103, 226.5287493268980086 ) ) ;
#30327 = CARTESIAN_POINT ( 'NONE',  ( -11.65394379379999990, 1426.751588810729800, 138.2311371409980154 ) ) ;
#30326 = CARTESIAN_POINT ( 'NONE',  ( -2.937955147957567181, 1512.266405701426038, 201.2341433539613718 ) ) ;
#30328 = CARTESIAN_POINT ( 'NONE',  ( 28.27965853590280076, 1508.150912785780065, 208.6308833624889587 ) ) ;
#30329 = DIRECTION ( 'NONE',  ( 0.000000000000000000, 0.000000000000000000, -1.000000000000000000 ) ) ;
#30330 = CARTESIAN_POINT ( 'NONE',  ( -8.881784197000000993E-16, 1392.213060387289943, 209.1218459616989946 ) ) ;
#30331 = CARTESIAN_POINT ( 'NONE',  ( -2.077940277580000217, 1417.511812052730193, 234.8008807337979817 ) ) ;
#30332 = CARTESIAN_POINT ( 'NONE',  ( 5.215187551930000609, 1368.779556716640172, 210.6218459616991936 ) ) ;
#30333 = CARTESIAN_POINT ( 'NONE',  ( -2.298048961635000165, 1516.764084769670262, 205.6764383981169715 ) ) ;
#30334 = CARTESIAN_POINT ( 'NONE',  ( 9.061547143302210117, 1507.228277554160059, 181.2342642626959730 ) ) ;
#30335 = ORIENTED_EDGE ( 'NONE', *, *, #33693, .T. ) ;
#30336 = DIRECTION ( 'NONE',  ( -0.9417419115949053898, -0.3363363969979660806, 5.735553207809421716E-15 ) ) ;
#30337 = CARTESIAN_POINT ( 'NONE',  ( -4.269964158086879458, 1441.123616076540202, 157.9266249594060127 ) ) ;
#30339 = ORIENTED_EDGE ( 'NONE', *, *, #72317, .T. ) ;
#30338 = CARTESIAN_POINT ( 'NONE',  ( -67.95945271801031140, 1379.746190535669939, 279.4408408362929777 ) ) ;
#30340 = ORIENTED_EDGE ( 'NONE', *, *, #23580, .T. ) ;
#30341 = CARTESIAN_POINT ( 'NONE',  ( 27.12601720510000192, 1508.017486052629920, 214.4687222129780082 ) ) ;
#30342 = VERTEX_POINT ( 'NONE', #79041 ) ;
#30343 = CARTESIAN_POINT ( 'NONE',  ( -2.222806802245810065, 1486.444619701660031, 220.8419180854079968 ) ) ;
#30344 = CARTESIAN_POINT ( 'NONE',  ( 12.65031558649999965, 1500.263532149289858, 208.0494375133089875 ) ) ;
#30346 = CARTESIAN_POINT ( 'NONE',  ( 0.8080234665550000139, 1507.121502733429907, 181.0049083015979932 ) ) ;
#30345 = CARTESIAN_POINT ( 'NONE',  ( 15.71445409271430016, 1411.849835564349860, 191.4861124036179945 ) ) ;
#30347 = CARTESIAN_POINT ( 'NONE',  ( 4.625789976465000564, 1517.104192383289956, 210.2432295619669844 ) ) ;
#30348 = VECTOR ( 'NONE', #60902, 1000.000000000000000 ) ;
#30349 = CARTESIAN_POINT ( 'NONE',  ( -24.14851371715629824, 1452.064661293180052, 136.7193580640750099 ) ) ;
#30350 = CARTESIAN_POINT ( 'NONE',  ( -106.2552881945959911, 1378.913060387629912, 305.9595024995889503 ) ) ;
#30351 = CARTESIAN_POINT ( 'NONE',  ( 10.89346138620000026, 1409.460417998529920, 228.8764123045980057 ) ) ;
#30352 = CARTESIAN_POINT ( 'NONE',  ( 10.02771185788900077, 1481.745846822699832, 215.6032939566460129 ) ) ;
#30353 = CARTESIAN_POINT ( 'NONE',  ( 0.000000000000000000, 0.000000000000000000, 0.000000000000000000 ) ) ;
#30354 = CARTESIAN_POINT ( 'NONE',  ( 40.33550002370660081, 1439.280879844779975, 134.0999999981289932 ) ) ;
#30355 = CARTESIAN_POINT ( 'NONE',  ( 11.99512495389999955, 1410.769353063830067, 192.9566925809980091 ) ) ;
#30356 = EDGE_LOOP ( 'NONE', ( #14514, #89580, #102078, #67315 ) ) ;
#30357 = CARTESIAN_POINT ( 'NONE',  ( 14.50701484619730053, 1436.101394055689980, 149.8878390185780063 ) ) ;
#30358 = VECTOR ( 'NONE', #45402, 1000.000000000000114 ) ;
#30359 = CARTESIAN_POINT ( 'NONE',  ( -17.38483621660000011, 1410.884422118429939, 225.7833436061980024 ) ) ;
#30360 = ORIENTED_EDGE ( 'NONE', *, *, #86358, .T. ) ;
#30361 = ORIENTED_EDGE ( 'NONE', *, *, #80365, .F. ) ;
#30362 = CARTESIAN_POINT ( 'NONE',  ( 7.276816673734427532, 1410.543541011706338, 230.7087126424827659 ) ) ;
#30363 = CARTESIAN_POINT ( 'NONE',  ( -14.38014760757803145, 1522.051704408389924, 209.8840156948171511 ) ) ;
#30364 = ADVANCED_FACE ( 'NONE', ( #105320 ), #7955, .T. ) ;
#30365 = B_SPLINE_CURVE_WITH_KNOTS ( 'NONE', 3,
 ( #110419, #17994, #102000, #51626, #94718, #683 ),
 .UNSPECIFIED., .F., .F.,
 ( 4, 2, 4 ),
 ( 0.000000000000000000, 0.5000000000000000000, 1.000000000000000000 ),
 .UNSPECIFIED. ) ;
#30366 = CARTESIAN_POINT ( 'NONE',  ( 12.61145490078909859, 1500.191570443869978, 207.7439650073710027 ) ) ;
#30367 = CARTESIAN_POINT ( 'NONE',  ( -3.482404635510000013, 1485.996524294529991, 182.2044824803980134 ) ) ;
#30368 = AXIS2_PLACEMENT_3D ( 'NONE', #99017, #72745, #97379 ) ;
#30369 = CARTESIAN_POINT ( 'NONE',  ( 12.38749917709999870, 1442.753158610539913, 186.6620494205980094 ) ) ;
#30370 = CARTESIAN_POINT ( 'NONE',  ( -65.41890721609597392, 1379.740427344783711, 273.1811798692826869 ) ) ;
#30371 = CARTESIAN_POINT ( 'NONE',  ( -1.625943548539999783, 1463.710935416889924, 199.4574233753289718 ) ) ;
#30372 = CARTESIAN_POINT ( 'NONE',  ( -1.116031910300000041, 1487.751631717630062, 231.2019806963980102 ) ) ;
#30373 = CARTESIAN_POINT ( 'NONE',  ( 10.54743240270000015, 1416.216739748630062, 194.5501240980979958 ) ) ;
#30374 = CARTESIAN_POINT ( 'NONE',  ( -54.90523341576640348, 1384.643634548589944, 233.6959364829789934 ) ) ;
#30375 = EDGE_LOOP ( 'NONE', ( #33524, #23592 ) ) ;
#30376 = DIRECTION ( 'NONE',  ( 0.000000000000000000, 0.000000000000000000, 1.000000000000000000 ) ) ;
#30377 = CARTESIAN_POINT ( 'NONE',  ( 0.7374508827770021036, 1516.978425811520083, 207.9881927911069965 ) ) ;
#30378 = EDGE_LOOP ( 'NONE', ( #84007, #17525, #40344, #98944 ) ) ;
#30379 = CARTESIAN_POINT ( 'NONE',  ( 38.91212894784649734, 1440.913060387330006, 266.0890524397909758 ) ) ;
#30380 = EDGE_CURVE ( 'NONE', #50836, #94989, #53852, .T. ) ;
#30381 = CARTESIAN_POINT ( 'NONE',  ( 18.80757778630000132, 1477.359834168530142, 228.3934860436980046 ) ) ;
#30382 = EDGE_LOOP ( 'NONE', ( #52564, #35322, #30174, #32873 ) ) ;
#30383 = CARTESIAN_POINT ( 'NONE',  ( -0.1414919779163680280, 1452.990816719059922, 183.2406312828490229 ) ) ;
#30384 = CARTESIAN_POINT ( 'NONE',  ( -11.73709356416840066, 1426.695943276110029, 144.1748013770919954 ) ) ;
#30385 = CARTESIAN_POINT ( 'NONE',  ( -7.105427357599999217E-15, 1410.913060387329779, 146.1721969590979882 ) ) ;
#30386 = CARTESIAN_POINT ( 'NONE',  ( 20.78707005949999953, 1497.559210495389834, 213.2326338321889807 ) ) ;
#30387 = CARTESIAN_POINT ( 'NONE',  ( 22.34437782794419647, 1410.382989033719923, 206.2310609402520072 ) ) ;
#30388 = EDGE_CURVE ( 'NONE', #234, #32360, #35921, .T. ) ;
#30389 = LINE ( 'NONE', #56151, #35015 ) ;
#30390 = CARTESIAN_POINT ( 'NONE',  ( -2.924372520659999530, 1509.089207866029938, 179.4306743669980051 ) ) ;
#30391 = CARTESIAN_POINT ( 'NONE',  ( -13.80561504080000113, 1434.979606281209954, 147.8556475097979899 ) ) ;
#30392 = CARTESIAN_POINT ( 'NONE',  ( -21.98490254033148972, 1525.713797967456912, 182.9410524212120777 ) ) ;
#30394 = DIRECTION ( 'NONE',  ( 1.755985294532464991E-16, -1.000000000000000000, 1.338183447452830017E-16 ) ) ;
#30393 = CARTESIAN_POINT ( 'NONE',  ( 17.03246454329999793, 1459.348684287830110, 228.8776382905979858 ) ) ;
#30395 = B_SPLINE_SURFACE_WITH_KNOTS ( 'NONE', 5, 5, ( 
 ( #10118, #44290, #639, #104180, #94113, #27464 ),
 ( #69507, #93556, #35320, #61652, #103057, #17384 ),
 ( #78434, #76775, #95231, #9011, #103629, #1746 ),
 ( #101955, #42623, #26927, #91, #95779, #35884 ),
 ( #61116, #68955, #85715, #43728, #77881, #34216 ),
 ( #19046, #52140, #16828, #1189, #70068, #86272 ),
 ( #26355, #60551, #51029, #18495, #17944, #53248 ),
 ( #51583, #52691, #86827, #10684, #87389, #44852 ),
 ( #79004, #33650, #67844, #25242, #9558, #85164 ) ),
 .UNSPECIFIED., .F., .F., .F.,
 ( 6, 3, 6 ),
 ( 6, 6 ),
 ( 3.013220511892180209, 5.186741360400000111, 7.360262208917820459 ),
 ( -0.0004429328978235130116, 2.000000000000000000 ),
 .UNSPECIFIED. ) ;
#30396 = CARTESIAN_POINT ( 'NONE',  ( -4.034280953785000179, 1517.049325831759916, 216.0701676760970145 ) ) ;
#30397 = CARTESIAN_POINT ( 'NONE',  ( -5.788280361890000059, 1452.919697783089987, 200.3898760574089977 ) ) ;
#30398 = CARTESIAN_POINT ( 'NONE',  ( -0.1613635714646410035, 1507.107001889669846, 180.9028745560509890 ) ) ;
#30399 = CARTESIAN_POINT ( 'NONE',  ( 15.95332790094227171, 1450.491793965960142, 220.3255767516768344 ) ) ;
#30400 = CARTESIAN_POINT ( 'NONE',  ( -4.609996619675000851, 1516.769879638719885, 212.5810025483170023 ) ) ;
#30401 = CARTESIAN_POINT ( 'NONE',  ( 4.324121571198490166, 1515.222544082249897, 212.0786725323009989 ) ) ;
#30402 = DIRECTION ( 'NONE',  ( 1.755985294532464991E-16, -1.000000000000000000, 1.338183447452830017E-16 ) ) ;
#30404 = VERTEX_POINT ( 'NONE', #28613 ) ;
#30403 = CARTESIAN_POINT ( 'NONE',  ( -109.9987472809999929, 1384.922094923150098, 311.2741087182590149 ) ) ;
#30405 = CARTESIAN_POINT ( 'NONE',  ( -17.78112816951914610, 1523.954914175594695, 237.8273240688543524 ) ) ;
#30406 = AXIS2_PLACEMENT_3D ( 'NONE', #67411, #34334, #93662 ) ;
#30407 = CARTESIAN_POINT ( 'NONE',  ( -22.75273496409559826, 1511.187213306747708, 234.5707981297189235 ) ) ;
#30408 = ADVANCED_FACE ( 'NONE', ( #70104 ), #85784, .T. ) ;
#30409 = CARTESIAN_POINT ( 'NONE',  ( -11.86115818179999870, 1431.976378517910007, 150.3873481853979968 ) ) ;
#30410 = CARTESIAN_POINT ( 'NONE',  ( -14.50231995610000091, 1415.734965818289993, 204.4815369236590072 ) ) ;
#30411 = CARTESIAN_POINT ( 'NONE',  ( -109.6164617405599984, 1383.195791559909821, 311.2195161898379752 ) ) ;
#30412 = CARTESIAN_POINT ( 'NONE',  ( -0.2669431423167949458, 1507.379250670300053, 237.3398778801180242 ) ) ;
#30413 = ADVANCED_FACE ( 'NONE', ( #13992 ), #22235, .T. ) ;
#30414 = DIRECTION ( 'NONE',  ( 0.000000000000000000, -0.9996573249755569268, 0.02617694830788849791 ) ) ;
#30415 = CARTESIAN_POINT ( 'NONE',  ( 11.76669623969999989, 1446.210547857770052, 187.6280433733980146 ) ) ;
#30416 = EDGE_CURVE ( 'NONE', #65907, #66063, #65538, .T. ) ;
#30418 = CARTESIAN_POINT ( 'NONE',  ( 2.500000000000000000, 1422.854123512330034, 153.3880924786980131 ) ) ;
#30417 = CARTESIAN_POINT ( 'NONE',  ( -22.10800917430000112, 1457.439287980229892, 221.1683851152979798 ) ) ;
#30419 = CARTESIAN_POINT ( 'NONE',  ( -1.995213577869999755, 1485.172489985530092, 182.7707872721979925 ) ) ;
#30420 = ORIENTED_EDGE ( 'NONE', *, *, #3458, .T. ) ;
#30421 = CARTESIAN_POINT ( 'NONE',  ( -7.335901033725000353, 1517.068717944079935, 205.0869373723870126 ) ) ;
#30422 = CARTESIAN_POINT ( 'NONE',  ( 3.441335375089999982, 1405.846167703030005, 267.5320912995980507 ) ) ;
#30423 = CARTESIAN_POINT ( 'NONE',  ( 1.485893011569999977, 1515.551703577890066, 213.0284692437889760 ) ) ;
#30424 = CARTESIAN_POINT ( 'NONE',  ( 20.32935570889999966, 1410.869484758429962, 198.1387192155980017 ) ) ;
#30425 = EDGE_CURVE ( 'NONE', #80080, #56812, #61875, .T. ) ;
#30426 = CARTESIAN_POINT ( 'NONE',  ( 22.04553792400322365, 1430.060189992810137, 217.9753957608339192 ) ) ;
#30427 =( BOUNDED_SURFACE ( )  B_SPLINE_SURFACE ( 3, 2, ( 
 ( #7165, #39090, #32898 ),
 ( #48637, #65438, #91714 ),
 ( #22833, #92264, #83863 ),
 ( #6059, #4948, #13886 ) ),
 .UNSPECIFIED., .F., .F., .T. ) 
 B_SPLINE_SURFACE_WITH_KNOTS ( ( 4, 4 ),
 ( 3, 3 ),
 ( 0.000000000000000000, 0.0002960034161023845684 ),
 ( 0.000000000000000000, 1.000000000000000000 ),
 .UNSPECIFIED. ) 
 GEOMETRIC_REPRESENTATION_ITEM ( )  RATIONAL_B_SPLINE_SURFACE ( (
 ( 1.000000000000000000, 0.8070209408750042002, 1.000000000000000000),
 ( 1.000000000000000000, 0.8071723757218286499, 1.000000000000000000),
 ( 1.000000000000000000, 0.8072480346917807470, 1.000000000000000000),
 ( 1.000000000000000000, 0.8072480644198112287, 1.000000000000000000) ) ) 
 REPRESENTATION_ITEM ( '' )  SURFACE ( )  );
#30428 = CARTESIAN_POINT ( 'NONE',  ( 10.47358766403681329, 1423.539380447800568, 137.3342994606528009 ) ) ;
#30429 = CARTESIAN_POINT ( 'NONE',  ( -10.03515428011349897, 1447.044425249150208, 211.5514612114130273 ) ) ;
#30430 = CIRCLE ( 'NONE', #101863, 1.999999999999998668 ) ;
#30431 = CARTESIAN_POINT ( 'NONE',  ( -1.456572815626359985, 1450.690862357650076, 154.5176491767769846 ) ) ;
#30432 = CARTESIAN_POINT ( 'NONE',  ( -1.631223015250512276, 1450.677821982117393, 183.2260624137571199 ) ) ;
#30433 = CARTESIAN_POINT ( 'NONE',  ( -19.77942753878213722, 1485.921887965895849, 190.2803841538269012 ) ) ;
#30434 = CARTESIAN_POINT ( 'NONE',  ( -2.252606381920000178, 1507.752798261690032, 221.0168201868989968 ) ) ;
#30435 = CARTESIAN_POINT ( 'NONE',  ( -12.31888632814230000, 1377.996605654810082, 209.2056224712380015 ) ) ;
#30436 = CARTESIAN_POINT ( 'NONE',  ( -28.02005515429999960, 1437.694013771309983, 248.0989693021979861 ) ) ;
#30437 = ADVANCED_FACE ( 'NONE', ( #81203 ), #41948, .T. ) ;
#30438 = DIRECTION ( 'NONE',  ( -0.6736849260863839728, 0.000000000000000000, 0.7390186874254150995 ) ) ;
#30439 = CARTESIAN_POINT ( 'NONE',  ( 2.500000000000000000, 1439.638128487469885, 168.7284197398979870 ) ) ;
#30440 = CARTESIAN_POINT ( 'NONE',  ( -1.749553261970000051, 1475.024750578529847, 269.6491148499980568 ) ) ;
#30441 = CARTESIAN_POINT ( 'NONE',  ( -4.240547926179750071, 1446.386475563049999, 162.7475928564280139 ) ) ;
#30442 = CARTESIAN_POINT ( 'NONE',  ( -4.660393612750000081, 1436.848553822789881, 227.0391165213990234 ) ) ;
#30443 = EDGE_CURVE ( 'NONE', #39980, #55879, #55960, .T. ) ;
#30444 = CARTESIAN_POINT ( 'NONE',  ( -4.161170142461470434, 1448.299083512420111, 185.1109003841999936 ) ) ;
#30445 = CARTESIAN_POINT ( 'NONE',  ( -41.60735100269249642, 1384.780218127079934, 245.0215821269129890 ) ) ;
#30446 = DIRECTION ( 'NONE',  ( 1.000000000000000000, 0.000000000000000000, 0.000000000000000000 ) ) ;
#30447 = AXIS2_PLACEMENT_3D ( 'NONE', #104452, #27744, #28300 ) ;
#30448 = CARTESIAN_POINT ( 'NONE',  ( 3.116143480280765043, 1509.034509700538138, 213.6092031811108711 ) ) ;
#30449 = CARTESIAN_POINT ( 'NONE',  ( 12.33307560294760030, 1492.131889311669966, 209.3605306458800044 ) ) ;
#30450 = CARTESIAN_POINT ( 'NONE',  ( 31.88715249297890253, 1525.425686270225242, 217.0217434889228798 ) ) ;
#30451 = CARTESIAN_POINT ( 'NONE',  ( 8.463861902778212709, 1511.395344347295122, 204.2992659969390559 ) ) ;
#30453 = EDGE_CURVE ( 'NONE', #29814, #68290, #104759, .T. ) ;
#30452 = CARTESIAN_POINT ( 'NONE',  ( -6.426487077828900496, 1396.137478263319963, 218.0991803394280169 ) ) ;
#30454 = CARTESIAN_POINT ( 'NONE',  ( -14.65376645209999928, 1421.828940461630054, 227.7443339645980132 ) ) ;
#30455 = CARTESIAN_POINT ( 'NONE',  ( -44.87824051230000322, 1439.395394557790041, 269.6922195959979831 ) ) ;
#30456 = ORIENTED_EDGE ( 'NONE', *, *, #103879, .F. ) ;
#30457 = CARTESIAN_POINT ( 'NONE',  ( 31.34137657934018506, 1523.481610426287716, 221.9025654077410081 ) ) ;
#30458 = CARTESIAN_POINT ( 'NONE',  ( -13.59279696885990063, 1508.107997983119958, 209.5096475415970190 ) ) ;
#30459 = CARTESIAN_POINT ( 'NONE',  ( -17.17241001986463189, 1523.382868172864164, 238.6251415217917895 ) ) ;
#30461 = CARTESIAN_POINT ( 'NONE',  ( -13.19864381506500095, 1513.023086264660151, 192.2692346079670074 ) ) ;
#30460 = CARTESIAN_POINT ( 'NONE',  ( 10.90287724760000110, 1425.661448047130079, 108.0463068396980049 ) ) ;
#30462 = PLANE ( 'NONE',  #96897 ) ;
#30463 = CARTESIAN_POINT ( 'NONE',  ( -5.516115361319998911, 1453.414288957689905, 201.0820915901090018 ) ) ;
#30464 = AXIS2_PLACEMENT_3D ( 'NONE', #102589, #60087, #77424 ) ;
#30465 = CARTESIAN_POINT ( 'NONE',  ( 0.7396922377450010355, 1517.135701590510052, 201.7845486201169933 ) ) ;
#30466 = CARTESIAN_POINT ( 'NONE',  ( 11.57530253392429920, 1501.342159829270031, 208.5271154928819897 ) ) ;
#30467 = CARTESIAN_POINT ( 'NONE',  ( 19.12715434829999950, 1496.834837384790035, 222.0421819495990121 ) ) ;
#30468 = CARTESIAN_POINT ( 'NONE',  ( 1.514918641279999978, 1508.378724870829956, 180.6682338044980156 ) ) ;
#30469 = FACE_BOUND ( 'NONE', #81882, .T. ) ;
#30470 = CARTESIAN_POINT ( 'NONE',  ( -93.73871268780000321, 1376.241061248600090, 305.1982575765590013 ) ) ;
#30471 = CARTESIAN_POINT ( 'NONE',  ( 8.726849315049999944, 1367.111769039820047, 207.6218459616989946 ) ) ;
#30473 = ORIENTED_EDGE ( 'NONE', *, *, #77232, .T. ) ;
#30472 = CARTESIAN_POINT ( 'NONE',  ( -16.69452037209399720, 1379.657147668529888, 211.9950716805600166 ) ) ;
#30474 = ORIENTED_EDGE ( 'NONE', *, *, #18488, .T. ) ;
#30475 = CARTESIAN_POINT ( 'NONE',  ( -9.542476768429999368, 1396.305783361229942, 201.7625145225379981 ) ) ;
#30476 = CARTESIAN_POINT ( 'NONE',  ( -21.56891384639999742, 1409.666263457130071, 211.8934866540579947 ) ) ;
#30477 = CARTESIAN_POINT ( 'NONE',  ( -5.004442077193687943, 1516.690345683714668, 201.4087281776068039 ) ) ;
#30478 = CARTESIAN_POINT ( 'NONE',  ( -0.0002361465808533021280, 1396.089833730190094, 220.9538863869404395 ) ) ;
#30479 = CARTESIAN_POINT ( 'NONE',  ( 3.820241900599999510E-10, 1475.513060387329915, 229.7676991014980104 ) ) ;
#30480 = CARTESIAN_POINT ( 'NONE',  ( 2.329898369991009854, 1515.064791341159889, 204.7923971587090080 ) ) ;
#30482 = CARTESIAN_POINT ( 'NONE',  ( -1.366886485456169975, 1418.311017005800068, 185.2659375928420218 ) ) ;
#30481 = CARTESIAN_POINT ( 'NONE',  ( -103.8898877650000117, 1389.939929192370073, 304.1778643809590221 ) ) ;
#30483 = CARTESIAN_POINT ( 'NONE',  ( 3.255198176620000439, 1410.302478098729807, 185.7993969742980198 ) ) ;
#30484 = CARTESIAN_POINT ( 'NONE',  ( -11.99296593569999914, 1415.426952350729835, 195.1671397404979871 ) ) ;
#30485 = CARTESIAN_POINT ( 'NONE',  ( -39.80824191364419562, 1446.385170600749916, 136.7374670100940079 ) ) ;
#30486 = SURFACE_STYLE_FILL_AREA ( #83643 ) ;
#30487 = CARTESIAN_POINT ( 'NONE',  ( 11.05917849935010011, 1396.299255410490105, 208.6381233312569918 ) ) ;
#30488 = CARTESIAN_POINT ( 'NONE',  ( -40.14607055839999816, 1442.238457364259830, 136.9587614600980032 ) ) ;
#30489 = CARTESIAN_POINT ( 'NONE',  ( 11.78195448370000165, 1427.013926546230095, 147.4989304475980134 ) ) ;
#30490 = CARTESIAN_POINT ( 'NONE',  ( 40.71170371759999540, 1443.968700575979938, 137.1160033506980085 ) ) ;
#30491 = ORIENTED_EDGE ( 'NONE', *, *, #12475, .T. ) ;
#30492 = DIRECTION ( 'NONE',  ( 0.000000000000000000, 1.000000000000000000, 0.000000000000000000 ) ) ;
#30493 = CARTESIAN_POINT ( 'NONE',  ( 22.08327125186946915, 1523.604703353109926, 233.8169256665487410 ) ) ;
#30494 = EDGE_LOOP ( 'NONE', ( #11595, #34019, #5860, #46911, #36950 ) ) ;
#30495 = ORIENTED_EDGE ( 'NONE', *, *, #33197, .T. ) ;
#30496 = CARTESIAN_POINT ( 'NONE',  ( -2.795964621609999590, 1422.864594294989956, 191.4386244948990168 ) ) ;
#30497 = CARTESIAN_POINT ( 'NONE',  ( -15.24459383950000024, 1460.671739161529786, 228.9091320249980015 ) ) ;
#30498 = CARTESIAN_POINT ( 'NONE',  ( -109.6278266837281308, 1386.599212502288538, 311.2267068848897225 ) ) ;
#30499 = CARTESIAN_POINT ( 'NONE',  ( 4.026786250540000722, 1418.913060387330006, 172.2701767054979882 ) ) ;
#30500 = CARTESIAN_POINT ( 'NONE',  ( 3.455377977254999955, 1516.627618683580067, 216.0573038954169931 ) ) ;
#30501 = CARTESIAN_POINT ( 'NONE',  ( -12.34254106707480148, 1378.948974406790057, 209.4210321092819811 ) ) ;
#30502 = VERTEX_POINT ( 'NONE', #100747 ) ;
#30503 = CARTESIAN_POINT ( 'NONE',  ( -18.44775390838900009, 1508.456898729019940, 211.1927022132439902 ) ) ;
#30504 = CARTESIAN_POINT ( 'NONE',  ( -8.899613412776929522, 1509.290876792079871, 180.4257793158479899 ) ) ;
#30505 = CARTESIAN_POINT ( 'NONE',  ( -64.29757574260000297, 1375.128795883580096, 269.4006999320590126 ) ) ;
#30506 = CARTESIAN_POINT ( 'NONE',  ( 0.2465318334700000169, 1414.971352895729979, 225.7948685045980142 ) ) ;
#30507 = CARTESIAN_POINT ( 'NONE',  ( 3.254401403604999743, 1516.919782530640077, 205.0791161293069820 ) ) ;
#30508 = ORIENTED_EDGE ( 'NONE', *, *, #79491, .F. ) ;
#30509 = CARTESIAN_POINT ( 'NONE',  ( 0.007128837152181529378, 1517.006509894990131, 209.8686634857439799 ) ) ;
#30510 = AXIS2_PLACEMENT_3D ( 'NONE', #29091, #47007, #38575 ) ;
#30511 = CARTESIAN_POINT ( 'NONE',  ( -9.051869799378589931, 1451.060085121989914, 207.2134550054099975 ) ) ;
#30512 = B_SPLINE_SURFACE_WITH_KNOTS ( 'NONE', 5, 5, ( 
 ( #61763, #37636, #89140, #29778, #12426, #98081 ),
 ( #80194, #63966, #3512, #44961, #97005, #20268 ),
 ( #4055, #54469, #95889, #88607, #70730, #71841 ),
 ( #53356, #105959, #20815, #96446, #38181, #79109 ),
 ( #89684, #19725, #12966, #106493, #81274, #2416 ),
 ( #88061, #11346, #45518, #79660, #56096, #66716 ) ),
 .UNSPECIFIED., .F., .F., .F.,
 ( 6, 6 ),
 ( 6, 6 ),
 ( 12.29943241800000031, 13.29386860920000046 ),
 ( 0.000000000000000000, 2.241783168430000028 ),
 .UNSPECIFIED. ) ;
#30513 = CARTESIAN_POINT ( 'NONE',  ( -39.91344421577615265, 1431.322027499858677, 269.6087553545235096 ) ) ;
#30514 = CARTESIAN_POINT ( 'NONE',  ( -0.4960463521180000224, 1409.436440922629799, 232.9663683892980259 ) ) ;
#30516 = VERTEX_POINT ( 'NONE', #66095 ) ;
#30515 = CARTESIAN_POINT ( 'NONE',  ( -11.86629849059999842, 1432.349867583040123, 149.9824147457980246 ) ) ;
#30517 = CARTESIAN_POINT ( 'NONE',  ( 5.513435558243076073, 1508.731359867040283, 216.5668839540665260 ) ) ;
#30518 = CARTESIAN_POINT ( 'NONE',  ( -35.60841938633720360, 1440.913060387850010, 252.1178284797530011 ) ) ;
#30519 = CARTESIAN_POINT ( 'NONE',  ( -81.18324780579999356, 1384.635789063720040, 304.9525423562590163 ) ) ;
#30520 = CARTESIAN_POINT ( 'NONE',  ( 20.72173035919999506, 1494.363728635189773, 205.4654988462689857 ) ) ;
#30521 = CARTESIAN_POINT ( 'NONE',  ( 34.59210919570099918, 1422.480570821680203, 269.7685429993599655 ) ) ;
#30523 = CARTESIAN_POINT ( 'NONE',  ( -4.997573825325000385, 1516.742629295279812, 212.5803724681170195 ) ) ;
#30522 = AXIS2_PLACEMENT_3D ( 'NONE', #47567, #4998, #23984 ) ;
#30524 = CARTESIAN_POINT ( 'NONE',  ( -62.86822150409999921, 1379.735228420929843, 268.0109119421590549 ) ) ;
#30525 = CARTESIAN_POINT ( 'NONE',  ( 22.74061145230000136, 1409.707167064430223, 208.8534835263149887 ) ) ;
#30526 = CARTESIAN_POINT ( 'NONE',  ( 29.16136750931930166, 1526.143142182216479, 197.5843855542958352 ) ) ;
#30527 = CARTESIAN_POINT ( 'NONE',  ( -0.1955981723043500320, 1414.913060387329779, 193.0575580317509718 ) ) ;
#30528 = CARTESIAN_POINT ( 'NONE',  ( -7.715319381269040377, 1516.774419107829999, 209.6761046150799928 ) ) ;
#30530 = B_SPLINE_CURVE_WITH_KNOTS ( 'NONE', 3,
 ( #93269, #50723, #84854, #8154 ),
 .UNSPECIFIED., .F., .F.,
 ( 4, 4 ),
 ( 0.000000000000000000, 1.000000000000000000 ),
 .UNSPECIFIED. ) ;
#30529 = CARTESIAN_POINT ( 'NONE',  ( -4.995623491025000362, 1516.636036526019780, 210.8344906863870278 ) ) ;
#30531 = CARTESIAN_POINT ( 'NONE',  ( 4.174991371165319265, 1421.544129702939927, 184.8960725920030086 ) ) ;
#30532 = CARTESIAN_POINT ( 'NONE',  ( -1.350311178199999906, 1415.380319686529901, 233.1877845536980089 ) ) ;
#30533 = CARTESIAN_POINT ( 'NONE',  ( 10.73499317030565869, 1424.972940667893681, 139.1354242632224611 ) ) ;
#30534 = EDGE_LOOP ( 'NONE', ( #3552, #86500, #4704, #43636 ) ) ;
#30535 = CARTESIAN_POINT ( 'NONE',  ( -32.59564481479979747, 1385.221210322680236, 230.9840656712089810 ) ) ;
#30536 = EDGE_CURVE ( 'NONE', #67505, #96166, #50886, .T. ) ;
#30537 = CARTESIAN_POINT ( 'NONE',  ( 18.90690578109999720, 1416.819760216030090, 210.0263053688559864 ) ) ;
#30538 = EDGE_CURVE ( 'NONE', #58564, #93915, #20480, .T. ) ;
#30539 = CARTESIAN_POINT ( 'NONE',  ( -0.02606214974820000169, 1415.758200430030001, 233.4550495725979999 ) ) ;
#30540 = AXIS2_PLACEMENT_3D ( 'NONE', #86666, #87227, #62624 ) ;
#30541 = LINE ( 'NONE', #105613, #105813 ) ;
#30542 = CARTESIAN_POINT ( 'NONE',  ( 2.615357652070000150, 1499.621979779589992, 230.2633180907990038 ) ) ;
#30543 = CARTESIAN_POINT ( 'NONE',  ( 11.53794409400000021, 1426.017383558870051, 204.7551399598289947 ) ) ;
#30544 = FACE_OUTER_BOUND ( 'NONE', #102489, .T. ) ;
#30545 = CIRCLE ( 'NONE', #71687, 1.000000000000057732 ) ;
#30547 = FACE_OUTER_BOUND ( 'NONE', #41674, .T. ) ;
#30546 = CARTESIAN_POINT ( 'NONE',  ( -4.615644842514999624, 1517.009964551830080, 216.0692237534070159 ) ) ;
#30548 = CARTESIAN_POINT ( 'NONE',  ( -33.91369269983620427, 1450.440666099120108, 136.2454419983430114 ) ) ;
#30549 = CARTESIAN_POINT ( 'NONE',  ( 10.81000252826892094, 1424.640867483547481, 137.9989916216163692 ) ) ;
#30550 = ORIENTED_EDGE ( 'NONE', *, *, #98649, .T. ) ;
#30551 = CARTESIAN_POINT ( 'NONE',  ( -0.7533001734329990429, 1516.714320817460020, 201.7957737879569891 ) ) ;
#30552 = CARTESIAN_POINT ( 'NONE',  ( 10.24368108368489949, 1480.724658557739986, 206.6208660495449863 ) ) ;
#30553 = EDGE_LOOP ( 'NONE', ( #1148, #72651, #80576, #28468 ) ) ;
#30554 = CARTESIAN_POINT ( 'NONE',  ( 0.000000000000000000, 1511.187213306747708, 209.1218459616979999 ) ) ;
#30555 = B_SPLINE_CURVE_WITH_KNOTS ( 'NONE', 3,
 ( #24098, #92412, #24638, #58836 ),
 .UNSPECIFIED., .F., .F.,
 ( 4, 4 ),
 ( 0.000000000000000000, 1.000000000000000000 ),
 .UNSPECIFIED. ) ;
#30556 = AXIS2_PLACEMENT_3D ( 'NONE', #92831, #101212, #7724 ) ;
#30557 = CARTESIAN_POINT ( 'NONE',  ( 19.25328782020000062, 1456.551502757129811, 224.6704391798980112 ) ) ;
#30558 = CARTESIAN_POINT ( 'NONE',  ( 7.338487941162202155, 1438.798250299839538, 154.0100661331221090 ) ) ;
#30559 = CARTESIAN_POINT ( 'NONE',  ( 9.488876987856384559, 1425.357746453355048, 195.5402808110155775 ) ) ;
#30560 = CARTESIAN_POINT ( 'NONE',  ( 1.169937655020000022, 1444.094766671090156, 217.9969059596489842 ) ) ;
#30561 = CARTESIAN_POINT ( 'NONE',  ( -113.4000000000000057, 1378.913060387289988, 304.2218459572590064 ) ) ;
#30562 = CARTESIAN_POINT ( 'NONE',  ( -2.500000000000000000, 1448.346004333310020, 162.8188153768979873 ) ) ;
#30563 = CARTESIAN_POINT ( 'NONE',  ( -19.25079509060000049, 1425.764729490530044, 223.8566527953979914 ) ) ;
#30564 = CARTESIAN_POINT ( 'NONE',  ( 3.629220049600000220, 1485.493215689190038, 199.0019176958990101 ) ) ;
#30565 = CARTESIAN_POINT ( 'NONE',  ( -106.0714421419999951, 1390.773723034939849, 301.0054119742590046 ) ) ;
#30566 = CARTESIAN_POINT ( 'NONE',  ( 19.00619812820000121, 1498.085718000629868, 188.9130380066980024 ) ) ;
#30568 = CARTESIAN_POINT ( 'NONE',  ( -14.87168881317970026, 1430.147188212150240, 221.8136313441650032 ) ) ;
#30567 = CARTESIAN_POINT ( 'NONE',  ( 0.1586669955048189973, 1408.918601621900279, 232.2155333696709931 ) ) ;
#30569 = DIRECTION ( 'NONE',  ( -0.4794255386042076128, 0.000000000000000000, 0.8775825618903700942 ) ) ;
#30570 = ORIENTED_EDGE ( 'NONE', *, *, #55358, .F. ) ;
#30571 = CARTESIAN_POINT ( 'NONE',  ( -105.5930518189999958, 1377.934166709269903, 303.6724188547589733 ) ) ;
#30572 = CARTESIAN_POINT ( 'NONE',  ( -11.40093083319999856, 1508.517784003389806, 218.0167457774089996 ) ) ;
#30573 = CARTESIAN_POINT ( 'NONE',  ( 11.84289190199999986, 1435.906080920110071, 147.6777950973980182 ) ) ;
#30574 = CARTESIAN_POINT ( 'NONE',  ( 11.27050504314370016, 1470.501325604160229, 207.5937458527450019 ) ) ;
#30575 = CYLINDRICAL_SURFACE ( 'NONE', #90237, 3.000000000000017764 ) ;
#30576 = CARTESIAN_POINT ( 'NONE',  ( 1.458547904730420175, 1497.341003214500006, 181.5395634206250008 ) ) ;
#30577 = CARTESIAN_POINT ( 'NONE',  ( -2.494575337237918689, 1524.201816949777367, 242.7026873301162482 ) ) ;
#30578 = CARTESIAN_POINT ( 'NONE',  ( -13.19308827171470888, 1443.110898837626110, 186.7803926656672218 ) ) ;
#30579 = EDGE_CURVE ( 'NONE', #42283, #94490, #85057, .T. ) ;
#30580 = CARTESIAN_POINT ( 'NONE',  ( 3.125347622798469782, 1407.037771531689941, 196.1218459610850005 ) ) ;
#30581 = CARTESIAN_POINT ( 'NONE',  ( 5.274922050350429714, 1494.803973017990074, 219.8410646961100099 ) ) ;
#30582 = CARTESIAN_POINT ( 'NONE',  ( -14.72577118585429901, 1514.214451951579804, 224.1399941292770279 ) ) ;
#30583 = CARTESIAN_POINT ( 'NONE',  ( -15.20693464918219995, 1415.677402202029953, 208.3693492345659877 ) ) ;
#30584 = CARTESIAN_POINT ( 'NONE',  ( -9.555044808816591129, 1460.091378345289968, 210.4134086466189899 ) ) ;
#30586 = ADVANCED_FACE ( 'NONE', ( #41426 ), #99130, .F. ) ;
#30585 = CARTESIAN_POINT ( 'NONE',  ( -0.008139190548902429725, 1516.932212683830130, 201.4023955549550067 ) ) ;
#30588 = ORIENTED_EDGE ( 'NONE', *, *, #45659, .T. ) ;
#30587 = FACE_OUTER_BOUND ( 'NONE', #29794, .T. ) ;
#30589 = B_SPLINE_CURVE_WITH_KNOTS ( 'NONE', 5,
 ( #87999, #95821, #103673, #53293, #87433, #52187, #10729, #83286, #89070, #23371, #49154, #92235 ),
 .UNSPECIFIED., .F., .F.,
 ( 6, 3, 3, 6 ),
 ( 0.000000000000000000, 0.5352712372119943218, 0.7510396948904395353, 1.000000000000000000 ),
 .UNSPECIFIED. ) ;
#30590 = CARTESIAN_POINT ( 'NONE',  ( -106.4361662359999912, 1382.339669133240022, 310.6646033542589862 ) ) ;
#30591 = CARTESIAN_POINT ( 'NONE',  ( 13.46561924343290073, 1512.674009804170055, 224.4294812528409864 ) ) ;
#30592 = ORIENTED_EDGE ( 'NONE', *, *, #40504, .F. ) ;
#30593 = ORIENTED_EDGE ( 'NONE', *, *, #105901, .T. ) ;
#30594 = CARTESIAN_POINT ( 'NONE',  ( -11.61544799540000028, 1501.735044459389883, 209.3067194099380117 ) ) ;
#30595 = CARTESIAN_POINT ( 'NONE',  ( 13.60476386450000064, 1509.388149220730156, 235.0937967613979822 ) ) ;
#30596 = DIRECTION ( 'NONE',  ( -1.000000000000000000, 0.000000000000000000, 0.000000000000000000 ) ) ;
#30598 = CARTESIAN_POINT ( 'NONE',  ( -15.89627787809999937, 1466.157227580030167, 250.4785789529980207 ) ) ;
#30597 = CARTESIAN_POINT ( 'NONE',  ( 38.85519404911526209, 1429.283679779192880, 269.5904935888122509 ) ) ;
#30599 = CARTESIAN_POINT ( 'NONE',  ( -19.98678683960000058, 1488.002369500329905, 190.9648164086979705 ) ) ;
#30600 = B_SPLINE_CURVE_WITH_KNOTS ( 'NONE', 5,
 ( #108979, #101644, #93265, #24932, #94352, #33905 ),
 .UNSPECIFIED., .F., .F.,
 ( 6, 6 ),
 ( 1.920081532330000192E-14, 6.607473203730000577 ),
 .UNSPECIFIED. ) ;
#30601 = CARTESIAN_POINT ( 'NONE',  ( -11.08593463959999958, 1433.241398677389952, 151.6928038766980080 ) ) ;
#30602 = DIRECTION ( 'NONE',  ( -9.341989762165448955E-47, 1.000000000000000000, -1.836970198721029688E-16 ) ) ;
#30603 = CARTESIAN_POINT ( 'NONE',  ( 11.69113150085549968, 1426.726128796750118, 140.8862638668499869 ) ) ;
#30604 = CARTESIAN_POINT ( 'NONE',  ( 17.06941271609999689, 1409.674943327129995, 224.1775087769979962 ) ) ;
#30605 = CARTESIAN_POINT ( 'NONE',  ( -0.4151546846839010985, 1522.906561336852974, 244.9330574173806951 ) ) ;
#30606 = CARTESIAN_POINT ( 'NONE',  ( -24.89939555210000321, 1440.978114073919869, 210.4300215348880272 ) ) ;
#30607 = CARTESIAN_POINT ( 'NONE',  ( -107.6675087117007337, 1379.017122048784131, 308.8731021086181840 ) ) ;
#30608 = CARTESIAN_POINT ( 'NONE',  ( -11.22044638126500082, 1480.603378457079998, 212.7473660371869926 ) ) ;
#30609 = CIRCLE ( 'NONE', #27019, 11.23850026409999892 ) ;
#30610 = CARTESIAN_POINT ( 'NONE',  ( 1.748848150597736018, 1360.440694539904143, 210.6218459616987957 ) ) ;
#30611 = CARTESIAN_POINT ( 'NONE',  ( 32.39315898239293290, 1526.178928173327449, 201.3122567411275838 ) ) ;
#30613 = EDGE_LOOP ( 'NONE', ( #93167, #58484, #22329, #96907 ) ) ;
#30612 = CARTESIAN_POINT ( 'NONE',  ( -6.421987433647831033E-11, 1412.000809220129895, 253.5556736965889968 ) ) ;
#30614 = ORIENTED_EDGE ( 'NONE', *, *, #91290, .T. ) ;
#30615 = CARTESIAN_POINT ( 'NONE',  ( -11.42745732190000041, 1504.700167813889948, 207.1863490741189935 ) ) ;
#30616 = CARTESIAN_POINT ( 'NONE',  ( -18.73651826089999872, 1506.305784642089975, 222.7068728818989882 ) ) ;
#30617 = CARTESIAN_POINT ( 'NONE',  ( -14.82025763449999900, 1469.894974939130179, 269.8832922682979643 ) ) ;
#30618 = CARTESIAN_POINT ( 'NONE',  ( -0.01304300961527469875, 1452.999749643619907, 183.2385070609109903 ) ) ;
#30620 = CIRCLE ( 'NONE', #93189, 2.000000000000003109 ) ;
#30619 = DIRECTION ( 'NONE',  ( 0.000000000000000000, 1.000000000000000000, 0.000000000000000000 ) ) ;
#30621 = DIRECTION ( 'NONE',  ( 0.5369043659964899406, -0.4884709562386497228, 0.6878443331780863534 ) ) ;
#30622 = CARTESIAN_POINT ( 'NONE',  ( 4.327392289583150031, 1515.143326931930005, 209.6385377796920011 ) ) ;
#30623 = DIRECTION ( 'NONE',  ( 1.224646799147350002E-16, -1.836970198721029688E-16, -1.000000000000000000 ) ) ;
#30624 = B_SPLINE_CURVE_WITH_KNOTS ( 'NONE', 3,
 ( #98580, #14013, #15646, #73949, #49852, #22396, #21846, #56596, #92374, #66121, #15111, #83985, #31375, #57166, #75060, #38674, #107536, #100244, #23522, #90170, #83427, #13453, #99668, #106984, #48202, #109209, #22958, #39790, #32493, #5640, #91288, #40880, #64463, #47642 ),
 .UNSPECIFIED., .F., .F.,
 ( 4, 2, 2, 2, 2, 2, 1, 1, 2, 2, 2, 2, 1, 1, 1, 1, 2, 2, 2, 4 ),
 ( 0.000000000000000000, 0.1250000000011176893, 0.1875000000016989743, 0.2500000000022802316, 0.3750000000034041658, 0.4375000000039372949, 0.4687500000041737724, 0.4843750000042577053, 0.4921875000042996717, 0.5000000000043415271, 0.6250000000054165561, 0.6875000000059233729, 0.7187500000061731731, 0.7343750000063343775, 0.7421875000064136474, 0.7460937500064499517, 0.7480468750064269701, 0.7500000000064039885, 0.8750000000032021052, 1.000000000000000000 ),
 .UNSPECIFIED. ) ;
#30625 = CARTESIAN_POINT ( 'NONE',  ( 9.932426370723289821, 1468.626893526349932, 207.8384836896190109 ) ) ;
#30626 = CARTESIAN_POINT ( 'NONE',  ( -4.244495231940000224, 1458.029848581590159, 218.1181198957289951 ) ) ;
#30627 = CARTESIAN_POINT ( 'NONE',  ( 11.94297283982292335, 1364.098416124965070, 209.6218459617033432 ) ) ;
#30628 = CARTESIAN_POINT ( 'NONE',  ( -24.11323544790549889, 1410.974473862270088, 266.9955217767330282 ) ) ;
#30629 = VERTEX_POINT ( 'NONE', #59346 ) ;
#30630 = CARTESIAN_POINT ( 'NONE',  ( -3.545807321122369959, 1503.565769337949860, 181.1286887016880200 ) ) ;
#30631 = VERTEX_POINT ( 'NONE', #75592 ) ;
#30632 = ORIENTED_EDGE ( 'NONE', *, *, #54520, .T. ) ;
#30633 = CARTESIAN_POINT ( 'NONE',  ( -6.933587693644999383, 1516.542957540330008, 210.8312046333570038 ) ) ;
#30634 = VECTOR ( 'NONE', #59112, 1000.000000000000114 ) ;
#30635 = CARTESIAN_POINT ( 'NONE',  ( 4.838327971944561767, 1423.497383055442015, 184.1236938972197663 ) ) ;
#30637 = DIRECTION ( 'NONE',  ( 0.000000000000000000, 1.000000000000000000, 0.000000000000000000 ) ) ;
#30636 = CARTESIAN_POINT ( 'NONE',  ( 2.299014030735000436, 1516.811292230880099, 211.9858893885470081 ) ) ;
#30638 = CARTESIAN_POINT ( 'NONE',  ( -4.463743402560000462, 1455.444639251629951, 184.7997051687979706 ) ) ;
#30639 = CARTESIAN_POINT ( 'NONE',  ( -2.138103891696413239, 1450.041837599050496, 182.8913454565717984 ) ) ;
#30640 = ORIENTED_EDGE ( 'NONE', *, *, #90530, .T. ) ;
#30641 = CARTESIAN_POINT ( 'NONE',  ( -26.55738301740000296, 1435.430825181030059, 135.4649699188979923 ) ) ;
#30642 = CARTESIAN_POINT ( 'NONE',  ( -1.128757599205000073, 1516.608208975040043, 201.4108789544669946 ) ) ;
#30643 = VECTOR ( 'NONE', #1351, 1000.000000000000000 ) ;
#30644 = B_SPLINE_CURVE_WITH_KNOTS ( 'NONE', 3,
 ( #31965, #6211, #47133, #40362, #31409, #56632, #30859, #65591, #55542, #73985 ),
 .UNSPECIFIED., .F., .F.,
 ( 4, 2, 2, 2, 4 ),
 ( 0.000000000000000000, 0.2500000000000000000, 0.5000000000000000000, 0.7500000000000000000, 1.000000000000000000 ),
 .UNSPECIFIED. ) ;
#30645 = LINE ( 'NONE', #98938, #82019 ) ;
#30646 = CARTESIAN_POINT ( 'NONE',  ( -27.67980887459539829, 1384.550718709600005, 204.4238776538969944 ) ) ;
#30647 = CARTESIAN_POINT ( 'NONE',  ( -34.35685943343030146, 1420.725836707379813, 270.3439669880020233 ) ) ;
#30648 = CARTESIAN_POINT ( 'NONE',  ( -4.848921205238590382, 1489.192137552770191, 188.8958419331429752 ) ) ;
#30649 = CARTESIAN_POINT ( 'NONE',  ( -3.844029647620000212, 1397.403954980429944, 196.6621108047980044 ) ) ;
#30651 = EDGE_LOOP ( 'NONE', ( #99904, #40645 ) ) ;
#30650 = CARTESIAN_POINT ( 'NONE',  ( -9.830395177452579958, 1365.769828494191870, 210.6218459616987957 ) ) ;
#30652 = EDGE_LOOP ( 'NONE', ( #108707, #37101, #15711, #76539, #46519, #31097, #21741 ) ) ;
#30653 = CARTESIAN_POINT ( 'NONE',  ( 3.848752177033039068, 1425.850564267019990, 185.2803273145039213 ) ) ;
#30654 = CARTESIAN_POINT ( 'NONE',  ( -1.157887263654020060, 1425.290045511299695, 191.1461690046699857 ) ) ;
#30655 = CARTESIAN_POINT ( 'NONE',  ( -14.50871316107370035, 1436.250700070630046, 149.9254544324789720 ) ) ;
#30656 = DIRECTION ( 'NONE',  ( 0.8672669759446630655, 0.000000000000000000, -0.4978433412588735285 ) ) ;
#30657 = CARTESIAN_POINT ( 'NONE',  ( -2.284053509485000077, 1516.854133554269993, 210.2586600040969813 ) ) ;
#30658 = CIRCLE ( 'NONE', #45007, 3.113774230133182108 ) ;
#30659 = CARTESIAN_POINT ( 'NONE',  ( 6.013193143143904074, 1460.021089919706810, 201.5886256082018519 ) ) ;
#30660 = CARTESIAN_POINT ( 'NONE',  ( -22.03783030909999852, 1435.764492934740019, 218.8250799062580256 ) ) ;
#30661 = CARTESIAN_POINT ( 'NONE',  ( 8.762903475094349304, 1437.482247596529760, 212.7253735826240018 ) ) ;
#30662 = CARTESIAN_POINT ( 'NONE',  ( 12.37159932449999822, 1415.628674266529742, 222.5813136582980007 ) ) ;
#30663 = CARTESIAN_POINT ( 'NONE',  ( 7.735039549035001016, 1511.353635254350138, 205.6398665129370045 ) ) ;
#30664 = CARTESIAN_POINT ( 'NONE',  ( -7.727327152855000492, 1517.232977404109988, 207.4118332116069894 ) ) ;
#30665 = ORIENTED_EDGE ( 'NONE', *, *, #81740, .F. ) ;
#30666 = DIRECTION ( 'NONE',  ( -0.001614263105669359660, 0.06164622090537578980, 0.9980967576356069015 ) ) ;
#30667 = CARTESIAN_POINT ( 'NONE',  ( -23.49345842294626863, 1448.339281494577790, 215.7559275228670117 ) ) ;
#30668 = EDGE_LOOP ( 'NONE', ( #12361, #14559, #64801, #77748, #67992, #50545, #109011, #91725 ) ) ;
#30669 = CARTESIAN_POINT ( 'NONE',  ( 3.464549481511450590, 1457.536217099257783, 228.5903248826067795 ) ) ;
#30670 = CARTESIAN_POINT ( 'NONE',  ( 24.29597249405740200, 1452.001349292369923, 137.1828877068549843 ) ) ;
#30671 = CARTESIAN_POINT ( 'NONE',  ( -4.088909611310605818, 1440.365459761272177, 185.3369552776610192 ) ) ;
#30672 = CARTESIAN_POINT ( 'NONE',  ( -9.095668477162160315, 1384.718387101820099, 199.9489932286030296 ) ) ;
#30673 = CARTESIAN_POINT ( 'NONE',  ( 21.13430999730000082, 1409.651086755129882, 206.4149715960279821 ) ) ;
#30674 = CARTESIAN_POINT ( 'NONE',  ( 16.87998458460000251, 1410.001061276529981, 226.1250098154980037 ) ) ;
#30675 = CARTESIAN_POINT ( 'NONE',  ( 32.23393008293232498, 1523.462669333491704, 201.4036600224296478 ) ) ;
#30676 = DIRECTION ( 'NONE',  ( 0.9510565162951566398, 0.000000000000000000, 0.3090169943749382919 ) ) ;
#30677 = CARTESIAN_POINT ( 'NONE',  ( 24.65284846709989708, 1440.998862877870124, 212.5088464049670165 ) ) ;
#30678 = DIRECTION ( 'NONE',  ( 0.3255681544571569219, 1.836970198721028948E-16, 0.9455185755993167351 ) ) ;
#30679 = CARTESIAN_POINT ( 'NONE',  ( -7.326795561505000443, 1516.760434454289907, 214.9020780475669881 ) ) ;
#30680 = EDGE_LOOP ( 'NONE', ( #36733, #14259, #47946, #81349 ) ) ;
#30681 = CARTESIAN_POINT ( 'NONE',  ( 7.709564572731689935, 1516.554653292440207, 207.5021949886239838 ) ) ;
#30682 = CARTESIAN_POINT ( 'NONE',  ( -4.301461581549999913, 1474.025770959829970, 270.1336327149980434 ) ) ;
#30683 = CARTESIAN_POINT ( 'NONE',  ( -7.006565531035000127, 1516.551704408390151, 197.1655329708669910 ) ) ;
#30684 = EDGE_CURVE ( 'NONE', #8026, #87268, #56491, .T. ) ;
#30685 = CARTESIAN_POINT ( 'NONE',  ( 0.000000000000000000, 1516.051704408390151, 209.1218459616989946 ) ) ;
#30686 = CARTESIAN_POINT ( 'NONE',  ( -3.247593561700000020, 1474.689375161690123, 218.8843939287889953 ) ) ;
#30687 = CARTESIAN_POINT ( 'NONE',  ( 11.60004869885203682, 1426.384977201060110, 138.5819896183834601 ) ) ;
#30688 = CARTESIAN_POINT ( 'NONE',  ( 2.736421577379605896, 1417.780736651565576, 234.0078274331876571 ) ) ;
#30689 = CARTESIAN_POINT ( 'NONE',  ( -2.131931780892150297, 1484.252787751960113, 183.0899073119249749 ) ) ;
#30690 = CARTESIAN_POINT ( 'NONE',  ( -12.31929927220420140, 1378.277686418020039, 209.5358532329640013 ) ) ;
#30691 = EDGE_CURVE ( 'NONE', #69179, #81290, #3367, .T. ) ;
#30692 = CARTESIAN_POINT ( 'NONE',  ( -21.54116136312547880, 1523.382868172864391, 183.9310736446958856 ) ) ;
#30693 = CARTESIAN_POINT ( 'NONE',  ( 32.50007417919399444, 1440.913060383219772, 245.3806142123629854 ) ) ;
#30694 = CARTESIAN_POINT ( 'NONE',  ( -10.00165394283440001, 1471.801449162250037, 210.9121004031800055 ) ) ;
#30695 = CARTESIAN_POINT ( 'NONE',  ( -31.10385014139604820, 1525.795403383247276, 201.8948722003923990 ) ) ;
#30696 = ORIENTED_EDGE ( 'NONE', *, *, #65845, .T. ) ;
#30697 = ORIENTED_EDGE ( 'NONE', *, *, #54613, .F. ) ;
#30698 = CARTESIAN_POINT ( 'NONE',  ( 10.57774485012819810, 1481.435663256220096, 209.0131183278130038 ) ) ;
#30699 = CARTESIAN_POINT ( 'NONE',  ( -19.08897089080889131, 1485.508016899335416, 189.6297277018092871 ) ) ;
#30700 = VECTOR ( 'NONE', #49758, 1000.000000000000114 ) ;
#30701 = CARTESIAN_POINT ( 'NONE',  ( -1.590368490799999979, 1443.733141016789887, 199.9573130278289739 ) ) ;
#30702 = CARTESIAN_POINT ( 'NONE',  ( 8.279741772999999583, 1424.453333272249893, 195.9250968994990103 ) ) ;
#30703 = CARTESIAN_POINT ( 'NONE',  ( -10.94904004810000053, 1491.926361048389936, 210.5558081329789957 ) ) ;
#30704 = CARTESIAN_POINT ( 'NONE',  ( 0.5203691551014211214, 1508.551704408389924, 219.9487978885150028 ) ) ;
#30705 = CARTESIAN_POINT ( 'NONE',  ( -47.25133509456620118, 1383.816458045290119, 255.6949490582159967 ) ) ;
#30706 = CARTESIAN_POINT ( 'NONE',  ( -5.551188712105000533, 1510.480349266450048, 201.5713426081769910 ) ) ;
#30707 = CARTESIAN_POINT ( 'NONE',  ( -13.99233004660000113, 1471.311257370429985, 192.9715307993979820 ) ) ;
#30708 = CARTESIAN_POINT ( 'NONE',  ( -11.42597592515710048, 1501.110059307680103, 208.6216570093839948 ) ) ;
#30709 = CARTESIAN_POINT ( 'NONE',  ( 2.256582165209999769, 1464.688065807730254, 236.3855123389979838 ) ) ;
#30711 = ORIENTED_EDGE ( 'NONE', *, *, #17257, .F. ) ;
#30710 = DIRECTION ( 'NONE',  ( -1.755985294532469921E-16, 1.000000000000000000, -1.338183447452831989E-16 ) ) ;
#30712 = CARTESIAN_POINT ( 'NONE',  ( -0.5038386193489999831, 1452.963758663529916, 183.2902632327979973 ) ) ;
#30713 = AXIS2_PLACEMENT_3D ( 'NONE', #35100, #110705, #93343 ) ;
#30714 = CARTESIAN_POINT ( 'NONE',  ( -31.98577773140000247, 1378.974038310059996, 216.6963266813090172 ) ) ;
#30715 = CARTESIAN_POINT ( 'NONE',  ( 4.504070374249360853, 1508.551704408389924, 205.1553644208390210 ) ) ;
#30717 = ORIENTED_EDGE ( 'NONE', *, *, #105777, .T. ) ;
#30716 = CARTESIAN_POINT ( 'NONE',  ( -30.95751052620443033, 1525.821544997589854, 216.7905424461075654 ) ) ;
#30718 = CARTESIAN_POINT ( 'NONE',  ( -13.32685356434600088, 1469.522677642460167, 191.9925945811579879 ) ) ;
#30719 = EDGE_LOOP ( 'NONE', ( #75797, #4638, #28578, #11147, #84317 ) ) ;
#30720 = CARTESIAN_POINT ( 'NONE',  ( -9.932403141389999135, 1389.845799269120107, 216.5446580629090079 ) ) ;
#30721 = CARTESIAN_POINT ( 'NONE',  ( -3.586321559908030032, 1515.071394777460000, 205.0390677611139836 ) ) ;
#30722 = DIRECTION ( 'NONE',  ( -6.922360974429999144E-17, -1.000000000000000000, 2.302693041820029802E-16 ) ) ;
#30723 = CARTESIAN_POINT ( 'NONE',  ( -6.138624675819999155, 1464.038710366590067, 200.4690805114690022 ) ) ;
#30724 = CARTESIAN_POINT ( 'NONE',  ( -15.20804204212620725, 1420.041555928045000, 212.2965765635398157 ) ) ;
#30725 = CARTESIAN_POINT ( 'NONE',  ( 7.654612949109999676, 1489.887860909490200, 207.9968670573389886 ) ) ;
#30726 = CARTESIAN_POINT ( 'NONE',  ( 1.969460191385499659, 1408.981835452669884, 194.2610538800710174 ) ) ;
#30727 = CARTESIAN_POINT ( 'NONE',  ( 0.8170660012889999768, 1410.321412113530187, 185.1427924109980268 ) ) ;
#30728 = CARTESIAN_POINT ( 'NONE',  ( 2.967683387859999744, 1419.631902151829991, 185.2975656967979887 ) ) ;
#30729 = DIRECTION ( 'NONE',  ( 1.000000000000000000, 0.000000000000000000, 0.000000000000000000 ) ) ;
#30730 = CARTESIAN_POINT ( 'NONE',  ( 11.86572145839999948, 1432.317385115999969, 150.3971827882980108 ) ) ;
#30731 = VECTOR ( 'NONE', #100390, 1000.000000000000000 ) ;
#30732 = CARTESIAN_POINT ( 'NONE',  ( 0.000000000000000000, 1512.187213306747481, 209.1218459616979999 ) ) ;
#30733 = ORIENTED_EDGE ( 'NONE', *, *, #91619, .F. ) ;
#30734 = ORIENTED_EDGE ( 'NONE', *, *, #88087, .F. ) ;
#30735 =( BOUNDED_CURVE ( )  B_SPLINE_CURVE ( 3, ( #3887, #27960, #19546, #70546 ),
 .UNSPECIFIED., .F., .F. ) 
 B_SPLINE_CURVE_WITH_KNOTS ( ( 4, 4 ),
 ( 6.205854994376239553, 6.217764911156499430 ),
 .UNSPECIFIED. ) 
 CURVE ( )  GEOMETRIC_REPRESENTATION_ITEM ( )  RATIONAL_B_SPLINE_CURVE ( ( 1.000000000000000000, 0.9999881795251216454, 0.9999881795251216454, 1.000000000000000000 ) ) 
 REPRESENTATION_ITEM ( '' )  );
#30736 = CARTESIAN_POINT ( 'NONE',  ( 18.37487226820591246, 1526.382868172863937, 235.7398599686385694 ) ) ;
#30737 = CARTESIAN_POINT ( 'NONE',  ( 19.46683531208329754, 1455.865237448739890, 226.9917334617080087 ) ) ;
#30738 = CIRCLE ( 'NONE', #105894, 12.26364123839999998 ) ;
#30739 = CARTESIAN_POINT ( 'NONE',  ( -12.77411984480000129, 1435.106351996289959, 150.5216832075980165 ) ) ;
#30740 = CARTESIAN_POINT ( 'NONE',  ( 12.48571605687039998, 1420.624698929089845, 200.8204384990370102 ) ) ;
#30741 = CARTESIAN_POINT ( 'NONE',  ( -20.59467299441400101, 1507.692298009320211, 190.3942269768830045 ) ) ;
#30742 = DIRECTION ( 'NONE',  ( -0.9993908270190948739, 0.03489949670252338876, 0.000000000000000000 ) ) ;
#30743 = CARTESIAN_POINT ( 'NONE',  ( -109.7531415440000018, 1385.295312989849890, 311.3520341442589938 ) ) ;
#30744 = CARTESIAN_POINT ( 'NONE',  ( 0.3821805048270000005, 1506.433683729329914, 231.1012307613979999 ) ) ;
#30745 = CARTESIAN_POINT ( 'NONE',  ( -11.95567671777125085, 1365.667439879733138, 209.6218459617033432 ) ) ;
#30746 = CARTESIAN_POINT ( 'NONE',  ( -46.05034235197370407, 1440.465840779690097, 266.6770621315579888 ) ) ;
#30747 = CARTESIAN_POINT ( 'NONE',  ( 3.258294392304168507, 1524.756004293092474, 176.4770358516228725 ) ) ;
#30748 = CARTESIAN_POINT ( 'NONE',  ( -2.299668004004999933, 1516.965971551240045, 208.0037412025070012 ) ) ;
#30749 = CARTESIAN_POINT ( 'NONE',  ( -9.488257380476161629, 1447.075045628219868, 211.9049835964190152 ) ) ;
#30750 = CARTESIAN_POINT ( 'NONE',  ( 2.599891563601349986, 1407.016599241430185, 221.9593604902549941 ) ) ;
#30751 = CARTESIAN_POINT ( 'NONE',  ( -13.09971517241789840, 1434.834136867550114, 149.3121823613580261 ) ) ;
#30752 = CARTESIAN_POINT ( 'NONE',  ( -8.040000583239999443, 1385.375414080450128, 218.7592922916490181 ) ) ;
#30753 = CARTESIAN_POINT ( 'NONE',  ( 6.037826478620000437, 1422.573110035629952, 122.8776253759980079 ) ) ;
#30754 = CARTESIAN_POINT ( 'NONE',  ( 6.901445711767499880, 1424.875821108860237, 213.3711103352979990 ) ) ;
#30755 = ORIENTED_EDGE ( 'NONE', *, *, #64522, .F. ) ;
#30756 = CARTESIAN_POINT ( 'NONE',  ( 31.95512683339999427, 1438.870446869690113, 244.1805851180980085 ) ) ;
#30757 = CARTESIAN_POINT ( 'NONE',  ( -27.89257148229999927, 1508.131979113730040, 206.8378734316980285 ) ) ;
#30759 = CARTESIAN_POINT ( 'NONE',  ( -15.24308032758169951, 1512.436270050390021, 222.2069269479069931 ) ) ;
#30758 = CARTESIAN_POINT ( 'NONE',  ( -11.76686801360590096, 1491.289303165600131, 206.7423971511180127 ) ) ;
#30760 = EDGE_CURVE ( 'NONE', #45555, #77955, #49141, .T. ) ;
#30761 = CARTESIAN_POINT ( 'NONE',  ( -3.129456141073420294, 1407.723287498587752, 270.1357490256495453 ) ) ;
#30762 = CARTESIAN_POINT ( 'NONE',  ( -28.01490336700000228, 1439.098491831259935, 231.6874816054980215 ) ) ;
#30763 = CARTESIAN_POINT ( 'NONE',  ( -29.34276002924985605, 1509.949525637511897, 205.4620678841161237 ) ) ;
#30764 = ADVANCED_FACE ( 'NONE', ( #24033 ), #67187, .T. ) ;
#30765 = EDGE_CURVE ( 'NONE', #20110, #3002, #28735, .T. ) ;
#30766 = CARTESIAN_POINT ( 'NONE',  ( -16.28005140691599806, 1452.344548464809804, 146.9042424669629838 ) ) ;
#30767 = CARTESIAN_POINT ( 'NONE',  ( 27.86006176749999952, 1451.482664390230184, 136.1185673336979676 ) ) ;
#30768 = ORIENTED_EDGE ( 'NONE', *, *, #43130, .F. ) ;
#30769 = CARTESIAN_POINT ( 'NONE',  ( -108.2039566672529958, 1378.913060387289988, 299.7295690038039879 ) ) ;
#30770 = CARTESIAN_POINT ( 'NONE',  ( 14.45750538832999865, 1416.828039266780024, 196.8520486936070029 ) ) ;
#30771 = CARTESIAN_POINT ( 'NONE',  ( 14.44412043019999992, 1509.548839716430166, 235.4430145842979982 ) ) ;
#30772 = ORIENTED_EDGE ( 'NONE', *, *, #86300, .T. ) ;
#30773 = VERTEX_POINT ( 'NONE', #66646 ) ;
#30774 = CARTESIAN_POINT ( 'NONE',  ( -10.81004456478011022, 1424.641001814318315, 137.9990871386040965 ) ) ;
#30775 = CARTESIAN_POINT ( 'NONE',  ( -24.12012278076839777, 1411.115370491980002, 208.7864916066450007 ) ) ;
#30776 = ORIENTED_EDGE ( 'NONE', *, *, #86894, .T. ) ;
#30777 = CARTESIAN_POINT ( 'NONE',  ( -8.366077765514660314, 1446.966787759040017, 191.6214120380429904 ) ) ;
#30778 = CARTESIAN_POINT ( 'NONE',  ( -105.0454790209999913, 1379.237143502780100, 304.6380415787589868 ) ) ;
#30779 = CARTESIAN_POINT ( 'NONE',  ( -1.355861272130000073, 1507.642012711630059, 237.1707191107980179 ) ) ;
#30780 = DIRECTION ( 'NONE',  ( -1.755985294532469921E-16, 1.000000000000000000, -1.338183447452831989E-16 ) ) ;
#30781 = ORIENTED_EDGE ( 'NONE', *, *, #61862, .F. ) ;
#30782 = CARTESIAN_POINT ( 'NONE',  ( 44.67025355869130010, 1449.989991176380045, 267.0226189060550155 ) ) ;
#30783 = CARTESIAN_POINT ( 'NONE',  ( -3.487584143074780041, 1508.551704408389924, 204.1347675025799902 ) ) ;
#30784 = CARTESIAN_POINT ( 'NONE',  ( -7.217365652099999807, 1426.227155235339978, 204.3687986179290021 ) ) ;
#30785 = CARTESIAN_POINT ( 'NONE',  ( 1.121950743945000051, 1517.123342927159911, 204.1084165760470057 ) ) ;
#30786 = ORIENTED_EDGE ( 'NONE', *, *, #53835, .T. ) ;
#30787 = CARTESIAN_POINT ( 'NONE',  ( 5.170554601400000116, 1484.055082523290139, 219.7711189574989703 ) ) ;
#30788 = AXIS2_PLACEMENT_3D ( 'NONE', #72730, #55382, #74397 ) ;
#30789 = CARTESIAN_POINT ( 'NONE',  ( 3.701853738749347755, 1478.468837479528020, 199.3102443334512657 ) ) ;
#30790 = EDGE_LOOP ( 'NONE', ( #23868, #54508, #52927, #102217 ) ) ;
#30791 = ORIENTED_EDGE ( 'NONE', *, *, #105016, .T. ) ;
#30792 = CARTESIAN_POINT ( 'NONE',  ( -11.88168803400450102, 1481.931231228029901, 208.8867617824080014 ) ) ;
#30793 = CARTESIAN_POINT ( 'NONE',  ( 16.73628186595838940, 1526.382868172863937, 234.1845039693043589 ) ) ;
#30794 = CARTESIAN_POINT ( 'NONE',  ( -22.32273759649999789, 1409.692587561330129, 207.4115339668879869 ) ) ;
#30795 = CARTESIAN_POINT ( 'NONE',  ( -10.12185763815729977, 1470.644638848689965, 212.0624009803890146 ) ) ;
#30796 = CARTESIAN_POINT ( 'NONE',  ( 12.10295653074440025, 1501.689262389139913, 213.0402934496359819 ) ) ;
#30797 = CARTESIAN_POINT ( 'NONE',  ( 11.67962703000000069, 1420.525946465979814, 199.2877884308990133 ) ) ;
#30798 = CARTESIAN_POINT ( 'NONE',  ( -1.017302442628150061, 1475.632587704960088, 220.5137673393959972 ) ) ;
#30799 = CARTESIAN_POINT ( 'NONE',  ( 19.12386044593656464, 1456.237284512719043, 225.8522710147555870 ) ) ;
#30800 = CARTESIAN_POINT ( 'NONE',  ( -19.68012578990143879, 1509.621020740076119, 231.2488516338165994 ) ) ;
#30801 = CARTESIAN_POINT ( 'NONE',  ( 0.03683343699197529769, 1409.591418101985710, 233.0054887270072470 ) ) ;
#30803 = CARTESIAN_POINT ( 'NONE',  ( -106.2236770203270027, 1391.605574620240077, 306.9900364964820483 ) ) ;
#30802 = CARTESIAN_POINT ( 'NONE',  ( -17.12205713392949846, 1425.049461331939938, 191.3399107580359839 ) ) ;
#30804 = CARTESIAN_POINT ( 'NONE',  ( 12.28210492449239943, 1427.001931710319923, 206.6181840418510092 ) ) ;
#30805 = CARTESIAN_POINT ( 'NONE',  ( -9.869059709240291411, 1439.877441815369821, 207.4585820634549975 ) ) ;
#30806 = CARTESIAN_POINT ( 'NONE',  ( 11.73563908010000034, 1425.610159190430068, 144.1657657165980027 ) ) ;
#30807 = ORIENTED_EDGE ( 'NONE', *, *, #108264, .F. ) ;
#30808 = CARTESIAN_POINT ( 'NONE',  ( 14.97660093000000003, 1430.165149126429924, 219.6133832206979832 ) ) ;
#30809 = VECTOR ( 'NONE', #13166, 999.9999999999998863 ) ;
#30810 = CARTESIAN_POINT ( 'NONE',  ( -12.78690713350000152, 1416.828040475229955, 195.5394874918979724 ) ) ;
#30811 = CARTESIAN_POINT ( 'NONE',  ( -82.20220381884530525, 1384.988272905459780, 305.2249867120139584 ) ) ;
#30812 = CARTESIAN_POINT ( 'NONE',  ( -8.837192375920000842, 1385.223969493600180, 199.9173279994789993 ) ) ;
#30813 = CARTESIAN_POINT ( 'NONE',  ( 19.64599270300000100, 1476.662575758389949, 214.0395835971089866 ) ) ;
#30815 = EDGE_LOOP ( 'NONE', ( #9313, #91178, #107578, #61098, #52563 ) ) ;
#30814 = CARTESIAN_POINT ( 'NONE',  ( -16.25293001547770189, 1420.173544245570156, 209.1081125830500014 ) ) ;
#30816 = CARTESIAN_POINT ( 'NONE',  ( 1.734314904639999932, 1429.316081142190114, 217.2477305841389921 ) ) ;
#30817 = CARTESIAN_POINT ( 'NONE',  ( -1.643576684049999903, 1435.943783413959864, 150.4860296878979682 ) ) ;
#30818 = CARTESIAN_POINT ( 'NONE',  ( -17.01462546559999822, 1417.417564138139824, 207.6637930894090118 ) ) ;
#30819 = CARTESIAN_POINT ( 'NONE',  ( 11.93316829419999969, 1433.461071242199978, 150.0216595702979703 ) ) ;
#30820 = EDGE_CURVE ( 'NONE', #46121, #13274, #33540, .T. ) ;
#30821 = CARTESIAN_POINT ( 'NONE',  ( 23.03655028440000052, 1458.194572356429944, 255.3819207682979595 ) ) ;
#30822 = B_SPLINE_CURVE_WITH_KNOTS ( 'NONE', 3,
 ( #34936, #1355, #78046, #86449, #33274, #85895, #101569, #9201, #35495, #26536, #43362, #77508, #18128, #69122, #84777, #8622, #93719, #42798, #52326, #25410, #76958, #16995, #267, #10288, #103809, #60161, #93183, #51195, #16450, #50647, #94282, #102666, #33832, #43905, #85326, #110544, #61293, #95411, #18675, #34392, #17559, #60732, #44466, #8074, #67465, #42244 ),
 .UNSPECIFIED., .F., .F.,
 ( 4, 3, 3, 3, 3, 3, 3, 3, 3, 3, 3, 3, 3, 3, 3, 4 ),
 ( -22.34240630152029894, -22.26676910785790042, -22.11540990129389783, -21.96056640200000132, -21.94306335083159709, -21.76802964484999947, -21.57549288769999762, -21.37216274998920085, -21.15253510981440144, -20.96805652687310229, -20.80534586139999931, -20.76768359745410208, -20.56671237214550274, -20.32807888289099907, -19.85081190438209831, -19.61749528909999896 ),
 .UNSPECIFIED. ) ;
#30823 = PLANE ( 'NONE',  #58057 ) ;
#30824 = CARTESIAN_POINT ( 'NONE',  ( 2.506833295396249994, 1457.656460922180031, 199.7250060859690279 ) ) ;
#30825 = CARTESIAN_POINT ( 'NONE',  ( 8.093510796512729755, 1424.956611240659868, 194.6959284516389914 ) ) ;
#30826 = CARTESIAN_POINT ( 'NONE',  ( 16.30658698069999701, 1422.109838810029942, 227.2734734342979834 ) ) ;
#30827 = CARTESIAN_POINT ( 'NONE',  ( -22.69876404240055479, 1522.382868172864391, 236.8953202675780858 ) ) ;
#30828 = LINE ( 'NONE', #75063, #50235 ) ;
#30829 = CARTESIAN_POINT ( 'NONE',  ( -18.03119042859999865, 1409.707603974429958, 223.6208843684979968 ) ) ;
#30830 = CARTESIAN_POINT ( 'NONE',  ( 1.548533272784429871, 1416.259629939349907, 190.3356629014230066 ) ) ;
#30831 = FACE_OUTER_BOUND ( 'NONE', #93494, .T. ) ;
#30832 = DIRECTION ( 'NONE',  ( 0.9858563016923833633, 0.000000000000000000, 0.1675928173085483863 ) ) ;
#30833 = CARTESIAN_POINT ( 'NONE',  ( 21.19079385647347991, 1525.394057003703438, 183.9650237549345491 ) ) ;
#30834 = CARTESIAN_POINT ( 'NONE',  ( 2.869862706494750323E-07, 1407.180374304939960, 196.1048350723650060 ) ) ;
#30835 = DIRECTION ( 'NONE',  ( 5.980589973904019347E-17, -1.000000000000000000, 1.736889445713099699E-16 ) ) ;
#30836 = CARTESIAN_POINT ( 'NONE',  ( -3.005246163384160063, 1450.300006441359983, 188.5532306313729975 ) ) ;
#30837 = CARTESIAN_POINT ( 'NONE',  ( -10.59708786280000048, 1416.824060884729988, 223.7633362045980050 ) ) ;
#30838 = CARTESIAN_POINT ( 'NONE',  ( 0.2151085986704019959, 1454.487371074299745, 183.1895884522399740 ) ) ;
#30839 = CARTESIAN_POINT ( 'NONE',  ( -12.34660213732820111, 1407.716881338870053, 203.8968045877159909 ) ) ;
#30840 = CARTESIAN_POINT ( 'NONE',  ( -16.05891525839999900, 1416.823418193329871, 200.6086608930380066 ) ) ;
#30841 = CARTESIAN_POINT ( 'NONE',  ( -27.98425287095180281, 1508.960817695580090, 210.6693023723670137 ) ) ;
#30842 = CARTESIAN_POINT ( 'NONE',  ( 13.19854548049999998, 1434.900412801370067, 149.1898584671980075 ) ) ;
#30843 = CARTESIAN_POINT ( 'NONE',  ( -27.68326325459999993, 1436.793383437599914, 136.7538416525980267 ) ) ;
#30844 = CARTESIAN_POINT ( 'NONE',  ( -3.244182695775085890, 1430.599155961690030, 201.4114353244786457 ) ) ;
#30845 = ORIENTED_EDGE ( 'NONE', *, *, #87069, .F. ) ;
#30846 = CARTESIAN_POINT ( 'NONE',  ( -17.29393938232497518, 1523.621879633028584, 180.8572348224460882 ) ) ;
#30847 = CARTESIAN_POINT ( 'NONE',  ( -2.382436964801009083, 1426.901689560119166, 137.0999999980979567 ) ) ;
#30848 = CARTESIAN_POINT ( 'NONE',  ( -106.7685201332123199, 1382.142799015560513, 310.0933617201660013 ) ) ;
#30849 = CARTESIAN_POINT ( 'NONE',  ( -10.94209138219999922, 1492.979990466090157, 207.3926136405989951 ) ) ;
#30850 = EDGE_CURVE ( 'NONE', #5224, #41836, #108356, .T. ) ;
#30851 = CARTESIAN_POINT ( 'NONE',  ( 4.617353517619999792, 1460.098150474590057, 228.0971968620989969 ) ) ;
#30852 = CYLINDRICAL_SURFACE ( 'NONE', #59899, 2.000000000000001776 ) ;
#30853 = CARTESIAN_POINT ( 'NONE',  ( 14.25697645713727368, 1408.402952620560427, 269.5859324265298369 ) ) ;
#30854 = CARTESIAN_POINT ( 'NONE',  ( -16.64894006880174615, 1482.394100643090269, 222.3169130686996198 ) ) ;
#30855 = CARTESIAN_POINT ( 'NONE',  ( -12.56073376859999868, 1379.581444859680232, 210.0898675169879937 ) ) ;
#30856 = CARTESIAN_POINT ( 'NONE',  ( 3.431952426600000106, 1439.695211740410059, 184.5361447059979980 ) ) ;
#30857 = CARTESIAN_POINT ( 'NONE',  ( -64.86877180440029633, 1385.085976455889977, 254.7512439600910170 ) ) ;
#30858 = CARTESIAN_POINT ( 'NONE',  ( -12.20945877950170022, 1490.723361035459902, 207.9880844395189854 ) ) ;
#30859 = CARTESIAN_POINT ( 'NONE',  ( -26.81029417419344085, 1435.596821286595059, 135.9924056800833227 ) ) ;
#30860 = CARTESIAN_POINT ( 'NONE',  ( -29.75012120250000081, 1509.993914124430148, 208.5595671623779879 ) ) ;
#30861 = DIRECTION ( 'NONE',  ( 0.9445946449598763284, 0.000000000000000000, -0.3282391760791590340 ) ) ;
#30862 = CARTESIAN_POINT ( 'NONE',  ( -16.22808440654519657, 1409.858776212460043, 226.2137158441180134 ) ) ;
#30864 = ORIENTED_EDGE ( 'NONE', *, *, #9971, .T. ) ;
#30863 = DIRECTION ( 'NONE',  ( 1.755985294532469921E-16, -1.000000000000000000, 1.338183447452831989E-16 ) ) ;
#30865 = CARTESIAN_POINT ( 'NONE',  ( -109.1315215469999913, 1384.880650352859902, 311.2646143532589917 ) ) ;
#30866 = CARTESIAN_POINT ( 'NONE',  ( 9.740043262020458670, 1470.413801779320011, 211.7848579975940027 ) ) ;
#30867 = CARTESIAN_POINT ( 'NONE',  ( -22.53878221424140094, 1411.058442688259902, 212.0450776560099939 ) ) ;
#30868 = CARTESIAN_POINT ( 'NONE',  ( -109.8097233119999885, 1384.480660791949958, 311.3604857892590303 ) ) ;
#30869 = CARTESIAN_POINT ( 'NONE',  ( -0.08494223902299619100, 1420.329338498939933, 183.4000416936310103 ) ) ;
#30870 = CARTESIAN_POINT ( 'NONE',  ( 0.1397974034109999986, 1466.394005007729902, 235.6966919797980040 ) ) ;
#30871 = CARTESIAN_POINT ( 'NONE',  ( 17.72062905389999798, 1409.531878389729854, 220.9701597516980200 ) ) ;
#30872 = CARTESIAN_POINT ( 'NONE',  ( -1.793243496752610078, 1419.496505211239764, 185.6405350652080131 ) ) ;
#30873 = CARTESIAN_POINT ( 'NONE',  ( -18.32377947901730053, 1464.077717911239915, 217.4721370783159955 ) ) ;
#30874 = FACE_OUTER_BOUND ( 'NONE', #93611, .T. ) ;
#30875 = CARTESIAN_POINT ( 'NONE',  ( -4.726464430697979502, 1511.395334939705208, 200.6898615724287822 ) ) ;
#30876 = CARTESIAN_POINT ( 'NONE',  ( 7.287315400159999790, 1481.177127506090073, 208.3645142728410065 ) ) ;
#30877 = CARTESIAN_POINT ( 'NONE',  ( -122.8636594665523489, 1366.350733876290178, 299.0518252276563658 ) ) ;
#30878 = CARTESIAN_POINT ( 'NONE',  ( 14.22993178683297266, 1512.187213306747481, 236.2420368605362455 ) ) ;
#30879 = CARTESIAN_POINT ( 'NONE',  ( -23.64337474990000132, 1435.765697120489904, 212.0350067752380028 ) ) ;
#30880 = CARTESIAN_POINT ( 'NONE',  ( -5.013264327984152224, 1375.413060387289988, 203.5257471471711312 ) ) ;
#30881 = CARTESIAN_POINT ( 'NONE',  ( -7.336844680545000053, 1517.106845464700200, 205.6683011064770312 ) ) ;
#30882 = CARTESIAN_POINT ( 'NONE',  ( -4.362798112068619005, 1485.138149384289818, 183.3481005963789983 ) ) ;
#30883 = ORIENTED_EDGE ( 'NONE', *, *, #42012, .T. ) ;
#30884 = CARTESIAN_POINT ( 'NONE',  ( -109.1649968403673796, 1384.882110519183016, 297.1327717510318394 ) ) ;
#30885 = CARTESIAN_POINT ( 'NONE',  ( -4.235431282328379510, 1441.481098832679891, 163.6249080756429919 ) ) ;
#30887 = VERTEX_POINT ( 'NONE', #110821 ) ;
#30886 = CARTESIAN_POINT ( 'NONE',  ( -68.37438365947571128, 1379.747068193089945, 279.9710327514259802 ) ) ;
#30888 = ORIENTED_EDGE ( 'NONE', *, *, #17808, .T. ) ;
#30889 = CARTESIAN_POINT ( 'NONE',  ( 28.89895421770000183, 1509.870172254329873, 212.1721160078579942 ) ) ;
#30890 = ORIENTED_EDGE ( 'NONE', *, *, #47763, .T. ) ;
#30891 = CARTESIAN_POINT ( 'NONE',  ( 3.394586470828380165, 1484.752177860970050, 220.4731790445629827 ) ) ;
#30892 = EDGE_CURVE ( 'NONE', #77352, #68144, #38045, .T. ) ;
#30893 = CARTESIAN_POINT ( 'NONE',  ( 11.97278235750000164, 1500.105384839889894, 206.6109453941589607 ) ) ;
#30895 = CARTESIAN_POINT ( 'NONE',  ( 15.73565734446670206, 1409.462549778659877, 192.9527420705210261 ) ) ;
#30894 = CARTESIAN_POINT ( 'NONE',  ( -11.10916966042679910, 1425.188513315250020, 141.1903306950420074 ) ) ;
#30896 = CARTESIAN_POINT ( 'NONE',  ( 1.717139084115000047, 1516.949031626070109, 210.2396860569670025 ) ) ;
#30897 = EDGE_CURVE ( 'NONE', #96593, #106524, #43410, .T. ) ;
#30898 = CARTESIAN_POINT ( 'NONE',  ( -25.08087365037879835, 1451.311483103210094, 137.5322042608940194 ) ) ;
#30899 = CARTESIAN_POINT ( 'NONE',  ( -107.5294434371819818, 1378.913060387289988, 307.8840114082699984 ) ) ;
#30900 = CARTESIAN_POINT ( 'NONE',  ( -3.139202535909999980, 1484.175171382029930, 181.3327878135980313 ) ) ;
#30901 = ADVANCED_FACE ( 'NONE', ( #4917 ), #24335, .F. ) ;
#30902 = CARTESIAN_POINT ( 'NONE',  ( 11.20313537261820080, 1480.728593169510077, 212.9248304369289713 ) ) ;
#30903 = DIRECTION ( 'NONE',  ( 1.000000000000000000, 0.000000000000000000, 0.000000000000000000 ) ) ;
#30904 = EDGE_CURVE ( 'NONE', #20305, #70446, #72757, .T. ) ;
#30905 = CARTESIAN_POINT ( 'NONE',  ( 33.91369120165509798, 1451.728768194249824, 134.0999999980979851 ) ) ;
#30906 = CARTESIAN_POINT ( 'NONE',  ( -39.76726435491990230, 1441.080129826450047, 136.8354390711329813 ) ) ;
#30907 = EDGE_LOOP ( 'NONE', ( #67022, #41664, #83531, #81762, #45090 ) ) ;
#30908 = CARTESIAN_POINT ( 'NONE',  ( 20.56230944797239957, 1477.111339253379811, 217.7195256771020127 ) ) ;
#30909 = CARTESIAN_POINT ( 'NONE',  ( -1.838822892484560212, 1431.425781269919980, 200.9354431986780014 ) ) ;
#30910 = ORIENTED_EDGE ( 'NONE', *, *, #32415, .T. ) ;
#30911 = ORIENTED_EDGE ( 'NONE', *, *, #72659, .F. ) ;
#30912 = ADVANCED_FACE ( 'NONE', ( #55349 ), #22795, .F. ) ;
#30913 = CARTESIAN_POINT ( 'NONE',  ( 2.923521462801879967, 1410.394928839790055, 231.6309329194170061 ) ) ;
#30914 = CYLINDRICAL_SURFACE ( 'NONE', #16952, 2.000000000000007550 ) ;
#30915 = CARTESIAN_POINT ( 'NONE',  ( 0.1153852296620000162, 1450.909031046320024, 181.2445446237979922 ) ) ;
#30916 = CARTESIAN_POINT ( 'NONE',  ( -16.87986946983459546, 1508.249863702309995, 209.5894333877659790 ) ) ;
#30917 = DIRECTION ( 'NONE',  ( 0.000000000000000000, 0.000000000000000000, 1.000000000000000000 ) ) ;
#30918 = CARTESIAN_POINT ( 'NONE',  ( -14.48645815959999794, 1379.659240074840000, 208.2003399408750113 ) ) ;
#30919 = CARTESIAN_POINT ( 'NONE',  ( -68.43993043927554254, 1379.747308170265114, 279.3533182895065465 ) ) ;
#30920 = CARTESIAN_POINT ( 'NONE',  ( -0.9802168924079989187, 1463.379214693789891, 199.3683684440489685 ) ) ;
#30921 = B_SPLINE_CURVE_WITH_KNOTS ( 'NONE', 5,
 ( #99462, #22740, #89432, #81028, #108993, #108434 ),
 .UNSPECIFIED., .F., .F.,
 ( 6, 6 ),
 ( 0.000000000000000000, 1.000000000000000000 ),
 .UNSPECIFIED. ) ;
#30922 = CARTESIAN_POINT ( 'NONE',  ( -3.780286426965000057, 1510.542924508009946, 201.5697040178069983 ) ) ;
#30923 = CARTESIAN_POINT ( 'NONE',  ( 12.45618503180000047, 1416.218047894730262, 196.1634441665979978 ) ) ;
#30924 = ADVANCED_FACE ( 'NONE', ( #12778 ), #46955, .F. ) ;
#30925 = CARTESIAN_POINT ( 'NONE',  ( -75.33592628756510123, 1384.769391308340118, 276.0432066516839882 ) ) ;
#30926 = ORIENTED_EDGE ( 'NONE', *, *, #8986, .T. ) ;
#30927 = CARTESIAN_POINT ( 'NONE',  ( 7.848979634317430509, 1517.151704408390060, 215.9448598632019980 ) ) ;
#30928 = CARTESIAN_POINT ( 'NONE',  ( 4.997718238375000510, 1516.693851263360102, 207.9888968556769839 ) ) ;
#30930 = ORIENTED_EDGE ( 'NONE', *, *, #104902, .T. ) ;
#30929 = B_SPLINE_CURVE_WITH_KNOTS ( 'NONE', 3,
 ( #13111, #89838, #31030, #106096, #47294, #22050, #106635, #29374, #48411, #56801, #63574, #98788 ),
 .UNSPECIFIED., .F., .F.,
 ( 4, 2, 2, 2, 2, 4 ),
 ( 0.000000000000000000, 0.01073386081903290011, 0.02153086504656569894, 0.04175192121145759883, 0.06241451806017900283, 0.08155783388473800133 ),
 .UNSPECIFIED. ) ;
#30931 = CARTESIAN_POINT ( 'NONE',  ( 11.20854072760000086, 1414.996442553830093, 222.5314266876980014 ) ) ;
#30932 = CARTESIAN_POINT ( 'NONE',  ( 19.38230263350000016, 1477.357356100929792, 227.8777628270980244 ) ) ;
#30933 = ORIENTED_EDGE ( 'NONE', *, *, #11208, .F. ) ;
#30934 = CARTESIAN_POINT ( 'NONE',  ( -16.70830179842720042, 1417.149226859160080, 207.3570905742490140 ) ) ;
#30935 = CARTESIAN_POINT ( 'NONE',  ( 19.53786426059019021, 1511.187213306747708, 180.5239794925693388 ) ) ;
#30936 = CARTESIAN_POINT ( 'NONE',  ( -17.92257945210411307, 1508.456862604705293, 212.0064218226281127 ) ) ;
#30937 = ADVANCED_FACE ( 'NONE', ( #30111 ), #92889, .T. ) ;
#30938 = CARTESIAN_POINT ( 'NONE',  ( 23.79000940093961347, 1411.113050310996186, 208.0033309891347812 ) ) ;
#30939 = CARTESIAN_POINT ( 'NONE',  ( -7.399624460160000083, 1435.775033902190216, 215.4503904880270113 ) ) ;
#30940 = B_SPLINE_CURVE_WITH_KNOTS ( 'NONE', 5,
 ( #85306, #33256, #41672, #31604, #75290, #109436 ),
 .UNSPECIFIED., .F., .F.,
 ( 6, 6 ),
 ( -36.72426843339999891, -23.77825875729999794 ),
 .UNSPECIFIED. ) ;
#30941 = CARTESIAN_POINT ( 'NONE',  ( -5.550449896747339018, 1510.476657126699820, 201.5714335428820050 ) ) ;
#30942 = CARTESIAN_POINT ( 'NONE',  ( -2.176538401690000235, 1507.722933799829889, 180.8157319044980227 ) ) ;
#30943 = EDGE_CURVE ( 'NONE', #83569, #96293, #40169, .T. ) ;
#30944 = CARTESIAN_POINT ( 'NONE',  ( -6.023224945624109594, 1510.704533469413036, 201.6205954506678495 ) ) ;
#30945 = CARTESIAN_POINT ( 'NONE',  ( -21.61625474793611446, 1526.178928173327449, 183.7635344381546361 ) ) ;
#30947 = CARTESIAN_POINT ( 'NONE',  ( -10.81441200649847190, 1424.654785931436436, 138.0165107421119046 ) ) ;
#30946 = CARTESIAN_POINT ( 'NONE',  ( 17.25891509299999882, 1458.394333519329848, 230.3479255126979979 ) ) ;
#30948 = CARTESIAN_POINT ( 'NONE',  ( 19.76074652845624158, 1471.421996062696735, 270.0618306119852718 ) ) ;
#30949 = CARTESIAN_POINT ( 'NONE',  ( -1.126138146715000010, 1517.208444099459939, 216.8485306577670144 ) ) ;
#30950 = EDGE_CURVE ( 'NONE', #18078, #13119, #95543, .T. ) ;
#30951 = DIRECTION ( 'NONE',  ( -0.06162841671618448508, -0.9961946980917499861, -0.06162841671618445039 ) ) ;
#30952 = CARTESIAN_POINT ( 'NONE',  ( -0.1193023033433100039, 1508.062965917820065, 180.6164617310760150 ) ) ;
#30953 = CARTESIAN_POINT ( 'NONE',  ( 2.587404269808366575, 1516.541469363555507, 216.8310653096392571 ) ) ;
#30954 = CARTESIAN_POINT ( 'NONE',  ( -7.323034312095000331, 1516.609912606490070, 212.5765947784269940 ) ) ;
#30955 = CARTESIAN_POINT ( 'NONE',  ( 2.329920892869609794, 1515.492270357739926, 213.2601720494629944 ) ) ;
#30956 = CARTESIAN_POINT ( 'NONE',  ( -11.60004869885203682, 1426.461377484368768, 139.0976633225263015 ) ) ;
#30958 = EDGE_LOOP ( 'NONE', ( #9344, #48826, #68030, #91635 ) ) ;
#30957 = CARTESIAN_POINT ( 'NONE',  ( -11.60674135321730027, 1507.508082919659955, 207.5537295141489835 ) ) ;
#30959 = CARTESIAN_POINT ( 'NONE',  ( -16.66231036550680500, 1523.604703353109926, 237.7554842931448036 ) ) ;
#30960 = CARTESIAN_POINT ( 'NONE',  ( 20.61309283089999767, 1451.396441790530162, 213.2979450416279974 ) ) ;
#30961 = CARTESIAN_POINT ( 'NONE',  ( -11.75672898480000050, 1431.354866972360014, 150.7379580337980087 ) ) ;
#30962 = CARTESIAN_POINT ( 'NONE',  ( -2.351149531359999489, 1431.454776817389984, 214.3229504429189944 ) ) ;
#30963 = CARTESIAN_POINT ( 'NONE',  ( -8.138947185354830083, 1440.565483764919918, 204.7812048973189860 ) ) ;
#30964 = CARTESIAN_POINT ( 'NONE',  ( -18.84390534926900074, 1444.419481533549970, 208.3496837893860061 ) ) ;
#30965 = CARTESIAN_POINT ( 'NONE',  ( -14.45258105951289807, 1415.677402202029953, 212.7925583759839867 ) ) ;
#30966 = CARTESIAN_POINT ( 'NONE',  ( -0.3646785447090010179, 1445.165625506690048, 215.3775911874990072 ) ) ;
#30968 = CARTESIAN_POINT ( 'NONE',  ( -10.08936239315010042, 1480.949542027630059, 206.0194718485379894 ) ) ;
#30967 = CARTESIAN_POINT ( 'NONE',  ( -18.47369489899999806, 1444.809210807949967, 226.6829861377979967 ) ) ;
#30969 = CARTESIAN_POINT ( 'NONE',  ( -1.902213919270000053, 1485.189568804029932, 182.6864153717980059 ) ) ;
#30970 = ORIENTED_EDGE ( 'NONE', *, *, #3181, .F. ) ;
#30971 = CARTESIAN_POINT ( 'NONE',  ( 4.997573787194999895, 1516.742629295279812, 205.6633194342169872 ) ) ;
#30972 = CARTESIAN_POINT ( 'NONE',  ( 9.927171082400001012, 1406.526425255430013, 267.4967810687980432 ) ) ;
#30973 = CARTESIAN_POINT ( 'NONE',  ( 0.5133736986269999969, 1410.311097483629965, 185.0719951505979850 ) ) ;
#30974 = CARTESIAN_POINT ( 'NONE',  ( 18.35208442190000255, 1410.878106859430090, 194.0788163582980133 ) ) ;
#30975 = EDGE_CURVE ( 'NONE', #32282, #108592, #77103, .T. ) ;
#30976 = CARTESIAN_POINT ( 'NONE',  ( 24.54210601322609975, 1438.972376264970535, 212.5794209063584219 ) ) ;
#30977 = EDGE_CURVE ( 'NONE', #81044, #19696, #18816, .T. ) ;
#30978 = DIRECTION ( 'NONE',  ( 0.09060005235378243427, 0.000000000000000000, 0.9958873583460591261 ) ) ;
#30979 = CARTESIAN_POINT ( 'NONE',  ( 11.60004869885203682, 1425.463724408334429, 136.9266941120787919 ) ) ;
#30980 = CARTESIAN_POINT ( 'NONE',  ( -6.580058596648179936, 1439.972221953270719, 203.3337447694734408 ) ) ;
#30981 = CARTESIAN_POINT ( 'NONE',  ( -2.425481787957049828, 1449.557072802999983, 154.2478782243809974 ) ) ;
#30982 = CARTESIAN_POINT ( 'NONE',  ( -12.60275825409999939, 1445.063511714940205, 186.1741640718979909 ) ) ;
#30983 = CARTESIAN_POINT ( 'NONE',  ( 0.8755637861606549999, 1450.882485026169888, 155.3353120183400051 ) ) ;
#30984 = CARTESIAN_POINT ( 'NONE',  ( -106.1577607520000015, 1391.913060387289988, 304.2026179676581705 ) ) ;
#30985 = CARTESIAN_POINT ( 'NONE',  ( -11.39360664199999995, 1501.071473187889978, 211.1722694393789936 ) ) ;
#30986 = CARTESIAN_POINT ( 'NONE',  ( -12.48077398309999886, 1422.454772915230024, 243.9198229428980085 ) ) ;
#30987 = ADVANCED_FACE ( 'NONE', ( #44048 ), #67912, .F. ) ;
#30988 = CARTESIAN_POINT ( 'NONE',  ( -27.43355922089999765, 1507.980920696029898, 210.8261541407979962 ) ) ;
#30989 = CARTESIAN_POINT ( 'NONE',  ( 4.261975124720000174, 1441.226018928259919, 159.2131618765980079 ) ) ;
#30990 = CARTESIAN_POINT ( 'NONE',  ( -3.713685391600000330, 1474.937103713529950, 269.6455928562979807 ) ) ;
#30991 = CARTESIAN_POINT ( 'NONE',  ( -11.04285492396053314, 1425.185071086764538, 139.1363384239375023 ) ) ;
#30992 = CARTESIAN_POINT ( 'NONE',  ( -20.20959865099510111, 1522.382868172863937, 182.0120230947222524 ) ) ;
#30993 = CARTESIAN_POINT ( 'NONE',  ( -11.81076840317520649, 1486.509818544849622, 184.2931069832207243 ) ) ;
#30994 = CARTESIAN_POINT ( 'NONE',  ( -25.09809013212120377, 1384.845757878930044, 223.7730809620549906 ) ) ;
#30995 = CARTESIAN_POINT ( 'NONE',  ( -106.4810267374109998, 1391.913060387289988, 303.2786322724959973 ) ) ;
#30996 = CARTESIAN_POINT ( 'NONE',  ( 11.60004869885206880, 1428.983126981192754, 137.0999999980979851 ) ) ;
#30997 = FACE_OUTER_BOUND ( 'NONE', #86417, .T. ) ;
#30998 = FACE_OUTER_BOUND ( 'NONE', #91249, .T. ) ;
#30999 = CARTESIAN_POINT ( 'NONE',  ( 7.932497417486165325, 1511.860489184832204, 205.9801110084320896 ) ) ;
#31000 = CARTESIAN_POINT ( 'NONE',  ( -21.08955099079999940, 1409.649523736130050, 203.6792363195980045 ) ) ;
#31001 = CARTESIAN_POINT ( 'NONE',  ( -15.03709947301200067, 1422.462674465683904, 228.7610913021540000 ) ) ;
#31002 = ADVANCED_FACE ( 'NONE', ( #61420 ), #18264, .F. ) ;
#31003 = CARTESIAN_POINT ( 'NONE',  ( 19.27715895977949145, 1456.031238095710933, 225.1558865330630397 ) ) ;
#31004 = VERTEX_POINT ( 'NONE', #59750 ) ;
#31005 = CARTESIAN_POINT ( 'NONE',  ( -3.749717822977947979, 1410.420720693452722, 232.2953181525738842 ) ) ;
#31006 = CARTESIAN_POINT ( 'NONE',  ( -7.522201478567969168, 1510.631883387999551, 215.0340703743040081 ) ) ;
#31007 = CARTESIAN_POINT ( 'NONE',  ( -18.65942492963539934, 1468.219830252329984, 201.0822089472089829 ) ) ;
#31009 = CARTESIAN_POINT ( 'NONE',  ( -12.38551416666500060, 1511.900571936589813, 193.4278863644669855 ) ) ;
#31008 = CARTESIAN_POINT ( 'NONE',  ( -5.940539704407487243, 1517.051704408389924, 229.2045057395878871 ) ) ;
#31010 = CARTESIAN_POINT ( 'NONE',  ( -15.91560388664723824, 1409.468828761781651, 225.2517153350140688 ) ) ;
#31011 = EDGE_CURVE ( 'NONE', #59795, #5604, #70576, .T. ) ;
#31012 = CARTESIAN_POINT ( 'NONE',  ( 39.35235217899570159, 1449.784370637009943, 136.1661491917279818 ) ) ;
#31013 = CARTESIAN_POINT ( 'NONE',  ( 7.716252052974999387, 1516.810037859429940, 202.1795012402670011 ) ) ;
#31014 = CARTESIAN_POINT ( 'NONE',  ( 7.739519778090000024, 1427.631386558690110, 212.7537242539289934 ) ) ;
#31015 = CARTESIAN_POINT ( 'NONE',  ( 0.000000000000000000, 1402.913060387289988, 209.1218459616989946 ) ) ;
#31016 = CARTESIAN_POINT ( 'NONE',  ( 16.00554743903499855, 1513.636261293280086, 194.3802644824669983 ) ) ;
#31017 = FACE_BOUND ( 'NONE', #57793, .T. ) ;
#31018 = CARTESIAN_POINT ( 'NONE',  ( -39.84051976466280109, 1379.672107560330005, 228.6815457374439973 ) ) ;
#31019 = CARTESIAN_POINT ( 'NONE',  ( 7.331153383319085393, 1366.861207034019344, 207.6218459616988241 ) ) ;
#31021 = ORIENTED_EDGE ( 'NONE', *, *, #38481, .F. ) ;
#31020 = CARTESIAN_POINT ( 'NONE',  ( -19.27348165808830061, 1379.660826776269914, 212.5863292630419892 ) ) ;
#31022 = ORIENTED_EDGE ( 'NONE', *, *, #28403, .T. ) ;
#31023 = CARTESIAN_POINT ( 'NONE',  ( -7.332112344980000529, 1396.169103392430088, 200.5548326435979902 ) ) ;
#31024 = CARTESIAN_POINT ( 'NONE',  ( -22.12171058789999734, 1410.179612746230077, 213.4701572216380043 ) ) ;
#31025 = CARTESIAN_POINT ( 'NONE',  ( -13.14575342714752360, 1444.761353586959785, 169.3990435656776015 ) ) ;
#31026 = EDGE_CURVE ( 'NONE', #107294, #27091, #16573, .T. ) ;
#31027 = CARTESIAN_POINT ( 'NONE',  ( 21.38883640680690945, 1509.706499414715836, 229.8114585089465152 ) ) ;
#31028 = CARTESIAN_POINT ( 'NONE',  ( 2.329957323386949941, 1515.551704201149960, 205.2926810894529979 ) ) ;
#31030 = CARTESIAN_POINT ( 'NONE',  ( -21.50621374580559930, 1505.483499709200032, 209.5478608782210301 ) ) ;
#31029 = CARTESIAN_POINT ( 'NONE',  ( -8.580669785929998739, 1384.878224714389944, 218.6695462856589813 ) ) ;
#31031 = EDGE_CURVE ( 'NONE', #106344, #80080, #47353, .T. ) ;
#31032 = CARTESIAN_POINT ( 'NONE',  ( -10.03977927579999907, 1416.217772597929979, 193.5333243407980035 ) ) ;
#31033 = CARTESIAN_POINT ( 'NONE',  ( -40.51897750172089729, 1445.566678767979965, 136.8537167310219900 ) ) ;
#31034 = CARTESIAN_POINT ( 'NONE',  ( 10.46340173671210039, 1396.278450429100076, 205.5098926540979960 ) ) ;
#31035 = CARTESIAN_POINT ( 'NONE',  ( 1.121465867070000177, 1416.819756528530206, 190.1591350936980120 ) ) ;
#31036 = CARTESIAN_POINT ( 'NONE',  ( 11.17161729519999902, 1425.146288952430041, 145.5104394328979822 ) ) ;
#31037 = CARTESIAN_POINT ( 'NONE',  ( 2.911036452777519212, 1509.035170506769646, 179.6587957555915125 ) ) ;
#31038 = ORIENTED_EDGE ( 'NONE', *, *, #33035, .F. ) ;
#31039 = CARTESIAN_POINT ( 'NONE',  ( -16.73628186595857059, 1526.382868172864164, 184.0591879540917546 ) ) ;
#31040 = CARTESIAN_POINT ( 'NONE',  ( 22.07691437628581710, 1523.843263703803586, 233.7988804623609269 ) ) ;
#31041 = VERTEX_POINT ( 'NONE', #45723 ) ;
#31042 = EDGE_LOOP ( 'NONE', ( #9845, #97683, #60558, #56239 ) ) ;
#31043 = EDGE_CURVE ( 'NONE', #2720, #63057, #92763, .T. ) ;
#31044 = DIRECTION ( 'NONE',  ( 5.980589973904019347E-17, -1.000000000000000000, 1.736889445713099699E-16 ) ) ;
#31045 = FACE_OUTER_BOUND ( 'NONE', #11905, .T. ) ;
#31046 = CARTESIAN_POINT ( 'NONE',  ( -13.41813859969999889, 1434.820761659759910, 195.8250830286980033 ) ) ;
#31047 = CARTESIAN_POINT ( 'NONE',  ( -9.862951377749247683, 1519.551704408389924, 228.3939896778649654 ) ) ;
#31048 = CARTESIAN_POINT ( 'NONE',  ( 2.873958851594999864, 1516.588006113850042, 216.0563744999969913 ) ) ;
#31049 = CARTESIAN_POINT ( 'NONE',  ( -13.80262683337540075, 1380.210689512640101, 209.0012437275910315 ) ) ;
#31050 = EDGE_CURVE ( 'NONE', #21147, #43726, #88802, .T. ) ;
#31051 = EDGE_CURVE ( 'NONE', #17819, #73768, #11561, .T. ) ;
#31052 = ORIENTED_EDGE ( 'NONE', *, *, #65845, .F. ) ;
#31053 = CARTESIAN_POINT ( 'NONE',  ( -4.145978979534980458E-15, 1375.413060387289988, 209.1218459572589836 ) ) ;
#31054 = CARTESIAN_POINT ( 'NONE',  ( -8.884906359809958687, 1509.278151300639820, 180.4749538926859884 ) ) ;
#31055 = CARTESIAN_POINT ( 'NONE',  ( -45.66666430340000460, 1379.776249196590243, 231.3493056156590058 ) ) ;
#31056 = CARTESIAN_POINT ( 'NONE',  ( 5.191738023060000096, 1415.425433635630043, 225.9364502213980188 ) ) ;
#31057 = CARTESIAN_POINT ( 'NONE',  ( 6.547556931335000385, 1516.633288330999903, 205.8595812817970057 ) ) ;
#31058 = ORIENTED_EDGE ( 'NONE', *, *, #108252, .T. ) ;
#31059 = CARTESIAN_POINT ( 'NONE',  ( 1.133653140995000141, 1516.978425811520083, 209.8592968530090275 ) ) ;
#31060 = CARTESIAN_POINT ( 'NONE',  ( -21.19481754039999899, 1509.644157119530064, 229.6418610316979994 ) ) ;
#31061 = CARTESIAN_POINT ( 'NONE',  ( -16.18783066347087285, 1412.761876852201794, 269.3698687316306177 ) ) ;
#31062 = FACE_OUTER_BOUND ( 'NONE', #50306, .T. ) ;
#31064 = ORIENTED_EDGE ( 'NONE', *, *, #35168, .F. ) ;
#31063 = CARTESIAN_POINT ( 'NONE',  ( -31.26701299884003404, 1523.919943579690425, 196.3491295910356769 ) ) ;
#31065 = EDGE_CURVE ( 'NONE', #40736, #59940, #1975, .T. ) ;
#31066 = CARTESIAN_POINT ( 'NONE',  ( -0.01304429014381880067, 1452.995120068570031, 183.2387050828319843 ) ) ;
#31067 = CARTESIAN_POINT ( 'NONE',  ( -29.54320591851210409, 1440.913060386779989, 236.8530523014009930 ) ) ;
#31068 = CARTESIAN_POINT ( 'NONE',  ( -38.64161925439999834, 1383.830331748989920, 239.2263113910589993 ) ) ;
#31069 = CARTESIAN_POINT ( 'NONE',  ( -0.4854401037883160352, 1465.014776865540171, 237.7376948412489810 ) ) ;
#31070 = CARTESIAN_POINT ( 'NONE',  ( 7.395434848029290187, 1409.662563599529904, 270.3697498994749822 ) ) ;
#31071 = EDGE_CURVE ( 'NONE', #8871, #33676, #21941, .T. ) ;
#31072 = CARTESIAN_POINT ( 'NONE',  ( -5.773668852974999766, 1516.734985836460055, 213.1604834329569940 ) ) ;
#31073 = CARTESIAN_POINT ( 'NONE',  ( -58.09331443159999964, 1379.714558625850032, 257.1750531167589884 ) ) ;
#31074 = CARTESIAN_POINT ( 'NONE',  ( 24.04079115580000092, 1410.979580360030013, 208.5492527449709996 ) ) ;
#31075 = CARTESIAN_POINT ( 'NONE',  ( 28.82451532742483735, 1526.348417187219184, 198.1911182592214402 ) ) ;
#31076 = CARTESIAN_POINT ( 'NONE',  ( -9.911041288964989704, 1424.405074346095262, 139.1388764670732598 ) ) ;
#31077 = CARTESIAN_POINT ( 'NONE',  ( -7.713124426543250145, 1516.690597168669910, 209.9915660461619780 ) ) ;
#31078 = CARTESIAN_POINT ( 'NONE',  ( -2.282301616165000269, 1516.836638729160086, 210.8392784184970026 ) ) ;
#31079 = CARTESIAN_POINT ( 'NONE',  ( -107.4307047400000101, 1391.913060387289988, 300.8770155100590387 ) ) ;
#31080 = CARTESIAN_POINT ( 'NONE',  ( 19.37374569213945463, 1526.382868172863937, 234.3668155954418637 ) ) ;
#31081 =( BOUNDED_CURVE ( )  B_SPLINE_CURVE ( 3, ( #54865, #13919, #99031, #88988 ),
 .UNSPECIFIED., .F., .T. ) 
 B_SPLINE_CURVE_WITH_KNOTS ( ( 4, 4 ),
 ( 6.278255371134338070, 6.312181817398001549 ),
 .UNSPECIFIED. ) 
 CURVE ( )  GEOMETRIC_REPRESENTATION_ITEM ( )  RATIONAL_B_SPLINE_CURVE ( ( 1.000000000000000000, 0.9999040853203211565, 0.9999040853203211565, 1.000000000000000000 ) ) 
 REPRESENTATION_ITEM ( '' )  );
#31082 = CARTESIAN_POINT ( 'NONE',  ( -113.4000000000000057, 1384.687144183860028, 311.2164849012590366 ) ) ;
#31084 = ORIENTED_EDGE ( 'NONE', *, *, #57599, .F. ) ;
#31083 = CARTESIAN_POINT ( 'NONE',  ( -46.06193801929999410, 1386.649016502250106, 219.0505733356889948 ) ) ;
#31085 = CARTESIAN_POINT ( 'NONE',  ( -48.62444006980110345, 1385.130390675030185, 258.8912542385650113 ) ) ;
#31086 = DIRECTION ( 'NONE',  ( 1.755985294532469921E-16, -1.000000000000000000, 1.338183447452831989E-16 ) ) ;
#31087 = DIRECTION ( 'NONE',  ( -0.000000000000000000, 1.836970198721029688E-16, 1.000000000000000000 ) ) ;
#31088 = DIRECTION ( 'NONE',  ( -0.002120872317203444275, 0.9999913661844078705, 0.003573437736364524098 ) ) ;
#31089 = CARTESIAN_POINT ( 'NONE',  ( 9.726491193908251375E-12, 1408.913060387299993, 194.1220083575990145 ) ) ;
#31090 = CARTESIAN_POINT ( 'NONE',  ( 11.36300084380000008, 1422.238049685370015, 206.7577474052189928 ) ) ;
#31091 = DIRECTION ( 'NONE',  ( -0.6736849260863841948, 0.000000000000000000, 0.7390186874254148774 ) ) ;
#31092 = CONICAL_SURFACE ( 'NONE', #34615, 1.000000000000007327, 0.7853981633970000820 ) ;
#31094 = LINE ( 'NONE', #66933, #88881 ) ;
#31093 = CARTESIAN_POINT ( 'NONE',  ( -6.554151464375000735, 1516.906641539930206, 216.4536580562070185 ) ) ;
#31095 = CARTESIAN_POINT ( 'NONE',  ( -2.926343479570000294, 1461.299900799990155, 228.5762336084989954 ) ) ;
#31096 = CARTESIAN_POINT ( 'NONE',  ( -0.3106507924581433655, 1515.598599846415254, 205.0832686031015157 ) ) ;
#31097 = ORIENTED_EDGE ( 'NONE', *, *, #65232, .T. ) ;
#31098 = CARTESIAN_POINT ( 'NONE',  ( 6.941100277744999936, 1516.858069504249897, 202.1782432786469883 ) ) ;
#31099 = CARTESIAN_POINT ( 'NONE',  ( -14.92003716616500064, 1512.136030808819896, 221.5058330632670049 ) ) ;
#31100 = ORIENTED_EDGE ( 'NONE', *, *, #101405, .T. ) ;
#31101 = CARTESIAN_POINT ( 'NONE',  ( 1.472772998086409935, 1415.954755710899917, 191.9874378180679741 ) ) ;
#31102 = B_SPLINE_CURVE_WITH_KNOTS ( 'NONE', 3,
 ( #58329, #108166, #39316, #90256, #14096, #92454, #81305, #4621, #38756, #22477, #31456, #107623, #72931, #13540, #47724, #23043, #5158, #30906, #65084, #99199, #82429, #76224, #636, #60548, #67841, #94110, #50487, #9555, #68952, #17381, #59442, #34765, #34213, #33106, #68399, #103626, #35317, #84063, #103054, #26924, #7361, #110368, #43725, #93553, #51580, #102503, #25793, #43182, #61113, #69504, #95228, #24682, #16825, #51026, #85712, #75684, #59992, #93010, #109825, #94670, #67295, #9008, #52137, #17941, #33647, #26352, #86269, #85161, #77878, #101952, #1186, #101387, #77334, #8447, #49926, #41526 ),
 .UNSPECIFIED., .F., .F.,
 ( 4, 3, 3, 3, 3, 3, 3, 3, 3, 3, 3, 3, 3, 3, 3, 3, 3, 3, 3, 3, 3, 3, 3, 3, 3, 4 ),
 ( 14.42287683710000046, 15.38027101718479983, 16.28803242362360137, 17.17436300713509922, 18.03299319179360083, 18.25245355743909670, 18.88350267378229930, 19.53205862555210004, 20.18761089655719942, 20.84551208257209964, 21.50053011586949836, 22.14300480878290145, 22.77552979124989818, 23.39142327888709971, 23.76042384637030125, 24.22815370064810025, 24.70787457184220060, 25.19935369834729855, 25.70478207845420116, 26.21374533000209794, 26.72094108690890124, 27.22151789532390254, 27.70638377802430341, 28.18141454126959999, 28.64088071977139904, 29.04792982929999923 ),
 .UNSPECIFIED. ) ;
#31103 = CIRCLE ( 'NONE', #91927, 1.000000000000000888 ) ;
#31104 = B_SPLINE_CURVE_WITH_KNOTS ( 'NONE', 5,
 ( #32096, #107145, #65163, #66283, #31537, #40491, #82506, #83051, #6344 ),
 .UNSPECIFIED., .F., .F.,
 ( 6, 3, 6 ),
 ( 0.000000000000000000, 0.4236215395309710918, 1.000000000000000000 ),
 .UNSPECIFIED. ) ;
#31105 = CARTESIAN_POINT ( 'NONE',  ( 22.87505597199999841, 1449.859370063780034, 219.3153813166979944 ) ) ;
#31106 = CARTESIAN_POINT ( 'NONE',  ( 7.981679316644171074, 1438.119269022099388, 153.6915228190263178 ) ) ;
#31107 = CARTESIAN_POINT ( 'NONE',  ( 9.343973014947424716, 1425.273178258202051, 195.5824969410661538 ) ) ;
#31108 = CARTESIAN_POINT ( 'NONE',  ( 2.620959656609999744, 1442.441462711689837, 217.7270133417389957 ) ) ;
#31109 = CARTESIAN_POINT ( 'NONE',  ( 15.95000232293457643, 1421.267744195325577, 227.4487368220951282 ) ) ;
#31110 = CARTESIAN_POINT ( 'NONE',  ( -3.655438681029999692, 1446.309375400119961, 170.5481836841979941 ) ) ;
#31111 = CARTESIAN_POINT ( 'NONE',  ( -18.76864046240000050, 1424.623155651629986, 224.6048661548979908 ) ) ;
#31112 = CARTESIAN_POINT ( 'NONE',  ( 8.342125760907268983, 1487.569189912864431, 202.1972327929222502 ) ) ;
#31113 = CARTESIAN_POINT ( 'NONE',  ( -107.7385742300000118, 1388.132002054980148, 298.3363211298590159 ) ) ;
#31114 = CARTESIAN_POINT ( 'NONE',  ( 19.07205183430000162, 1488.300534546829795, 189.3974363681980151 ) ) ;
#31115 = CARTESIAN_POINT ( 'NONE',  ( 0.5840752967518939576, 1410.310972847609946, 233.1572170071730170 ) ) ;
#31116 = CARTESIAN_POINT ( 'NONE',  ( -34.65398121300953704, 1458.146139331663790, 269.5268082531298433 ) ) ;
#31117 = ORIENTED_EDGE ( 'NONE', *, *, #52290, .T. ) ;
#31118 = LINE ( 'NONE', #56337, #82070 ) ;
#31119 = CARTESIAN_POINT ( 'NONE',  ( -3.994937574034520100, 1430.106198372560129, 201.8091617894969829 ) ) ;
#31120 = CARTESIAN_POINT ( 'NONE',  ( 32.52419458002820107, 1524.600389084707103, 201.1675047309180968 ) ) ;
#31121 = CARTESIAN_POINT ( 'NONE',  ( -4.159508860199999880, 1408.913060387329779, 226.9541261483979895 ) ) ;
#31122 = CARTESIAN_POINT ( 'NONE',  ( -1.443308773824269364, 1409.130619237754445, 186.4549414979184689 ) ) ;
#31123 = CARTESIAN_POINT ( 'NONE',  ( -12.69557643223229881, 1442.808827016684518, 186.1671471355434448 ) ) ;
#31124 = AXIS2_PLACEMENT_3D ( 'NONE', #75417, #50215, #1892 ) ;
#31125 = CARTESIAN_POINT ( 'NONE',  ( -13.82860589446197075, 1517.051704408389924, 226.2317424102079144 ) ) ;
#31126 = FACE_OUTER_BOUND ( 'NONE', #87821, .T. ) ;
#31127 = CARTESIAN_POINT ( 'NONE',  ( -14.62022782577733082, 1410.806204324935607, 226.7253561846267758 ) ) ;
#31128 = CARTESIAN_POINT ( 'NONE',  ( -14.09290554161880138, 1415.677402202029953, 204.2440491414689916 ) ) ;
#31129 = CARTESIAN_POINT ( 'NONE',  ( 23.79680546489999671, 1435.328500499490019, 137.0919807913980151 ) ) ;
#31130 = CARTESIAN_POINT ( 'NONE',  ( -13.13810362587316050, 1443.057752665512453, 169.4001936047692425 ) ) ;
#31132 = VERTEX_POINT ( 'NONE', #38386 ) ;
#31131 = CARTESIAN_POINT ( 'NONE',  ( -13.85929582179999997, 1410.325638522630015, 227.0940391209979907 ) ) ;
#31133 = CARTESIAN_POINT ( 'NONE',  ( -102.7832239250000015, 1382.339223999440037, 310.5717497612590137 ) ) ;
#31134 = CARTESIAN_POINT ( 'NONE',  ( 13.83393986337329906, 1512.951873711600001, 224.4212087918060092 ) ) ;
#31135 = ORIENTED_EDGE ( 'NONE', *, *, #81481, .F. ) ;
#31136 = ORIENTED_EDGE ( 'NONE', *, *, #28127, .T. ) ;
#31137 = CARTESIAN_POINT ( 'NONE',  ( 16.40028066370599902, 1414.913057860449953, 209.2777006334819987 ) ) ;
#31138 = CARTESIAN_POINT ( 'NONE',  ( 12.96261739959999915, 1509.136740573229872, 234.0631307178979910 ) ) ;
#31140 = CARTESIAN_POINT ( 'NONE',  ( -31.20802388950000150, 1451.456139917630026, 248.1710554650979930 ) ) ;
#31139 = CARTESIAN_POINT ( 'NONE',  ( 4.461864229229999701, 1454.855724705989815, 217.5673509250489985 ) ) ;
#31141 = CARTESIAN_POINT ( 'NONE',  ( -19.90008872329999789, 1491.252934255230002, 189.9399603158979914 ) ) ;
#31142 = CARTESIAN_POINT ( 'NONE',  ( -11.33778558790000091, 1433.696525961220004, 151.4746538488979866 ) ) ;
#31143 = CARTESIAN_POINT ( 'NONE',  ( 11.78824854703250047, 1517.051704408389924, 211.4132493584619965 ) ) ;
#31144 = CARTESIAN_POINT ( 'NONE',  ( 11.69617228600709957, 1426.722709022770005, 141.2463821871190248 ) ) ;
#31145 = CARTESIAN_POINT ( 'NONE',  ( 26.78593482470590104, 1474.097921906449983, 209.4579982356089829 ) ) ;
#31146 = CARTESIAN_POINT ( 'NONE',  ( -26.26372997560000044, 1440.614374483860047, 137.6218707767980334 ) ) ;
#31147 = CARTESIAN_POINT ( 'NONE',  ( 0.8282867551300300279, 1515.122054816080208, 213.4497952811889832 ) ) ;
#31148 = FACE_BOUND ( 'NONE', #64850, .T. ) ;
#31149 = CARTESIAN_POINT ( 'NONE',  ( -6.355761515339399814, 1477.685937564089954, 218.7950034472659979 ) ) ;
#31150 = CARTESIAN_POINT ( 'NONE',  ( 1.602682243905599213, 1362.313628982924683, 208.3718459617061285 ) ) ;
#31151 = CARTESIAN_POINT ( 'NONE',  ( -11.71000892829403206, 1509.446600626986992, 236.7426052959320089 ) ) ;
#31153 = VERTEX_POINT ( 'NONE', #106690 ) ;
#31152 = CARTESIAN_POINT ( 'NONE',  ( 1.255340816988079985E-08, 1408.894734928509934, 261.0927290538760417 ) ) ;
#31154 = ORIENTED_EDGE ( 'NONE', *, *, #105176, .F. ) ;
#31155 = DIRECTION ( 'NONE',  ( 5.980589973904019347E-17, -1.000000000000000000, 1.736889445713099699E-16 ) ) ;
#31156 = CARTESIAN_POINT ( 'NONE',  ( -18.77469242039999742, 1505.713855622889923, 222.6051356488989938 ) ) ;
#31157 = CARTESIAN_POINT ( 'NONE',  ( -5.207740107420000264, 1471.814797097629935, 270.0726242057979789 ) ) ;
#31158 = DIRECTION ( 'NONE',  ( 0.000000000000000000, 1.000000000000000000, 0.000000000000000000 ) ) ;
#31159 = CARTESIAN_POINT ( 'NONE',  ( -5.013321581124261961, 1375.421791045822374, 214.7179703222298883 ) ) ;
#31160 = CARTESIAN_POINT ( 'NONE',  ( 0.2051679708434860083, 1452.385543061679982, 183.1882097260399860 ) ) ;
#31161 = ADVANCED_FACE ( 'NONE', ( #46280 ), #80407, .T. ) ;
#31162 = CARTESIAN_POINT ( 'NONE',  ( -9.096737447160000656, 1384.691502115709909, 199.9504659608490158 ) ) ;
#31163 = CARTESIAN_POINT ( 'NONE',  ( 18.22204802156040060, 1431.452345132420078, 207.6392317545619903 ) ) ;
#31164 = CARTESIAN_POINT ( 'NONE',  ( -3.957900269260000048, 1458.284989000489986, 219.0746905126889885 ) ) ;
#31165 = CARTESIAN_POINT ( 'NONE',  ( 9.671060821790000261, 1366.060403940050037, 207.6218459616989946 ) ) ;
#31166 = CARTESIAN_POINT ( 'NONE',  ( -33.71036013506279971, 1416.517407414779882, 268.0042259019550102 ) ) ;
#31167 = EDGE_CURVE ( 'NONE', #25915, #77692, #87434, .T. ) ;
#31168 = ORIENTED_EDGE ( 'NONE', *, *, #22650, .F. ) ;
#31169 = CARTESIAN_POINT ( 'NONE',  ( -3.548560001899690342, 1506.246208310000156, 181.0144377455499978 ) ) ;
#31170 = AXIS2_PLACEMENT_3D ( 'NONE', #79281, #95516, #107087 ) ;
#31171 = VERTEX_POINT ( 'NONE', #63631 ) ;
#31172 = EDGE_LOOP ( 'NONE', ( #5844, #69635, #10686, #52855 ) ) ;
#31173 = CARTESIAN_POINT ( 'NONE',  ( -3.445407572115000150, 1516.764084769670262, 211.4198948937369948 ) ) ;
#31174 = EDGE_CURVE ( 'NONE', #61114, #99409, #110108, .T. ) ;
#31175 = DIRECTION ( 'NONE',  ( 0.000000000000000000, 0.000000000000000000, -1.000000000000000000 ) ) ;
#31176 = DIRECTION ( 'NONE',  ( -1.000000000000000000, 0.000000000000000000, 0.000000000000000000 ) ) ;
#31178 = CARTESIAN_POINT ( 'NONE',  ( -17.62371441874761047, 1419.748654031750903, 206.8646141850265963 ) ) ;
#31177 = CARTESIAN_POINT ( 'NONE',  ( 0.7572979362240020995, 1516.829948096479939, 212.5714934102470011 ) ) ;
#31179 = CARTESIAN_POINT ( 'NONE',  ( -15.95246779919999902, 1455.452439780930035, 189.1034377625979914 ) ) ;
#31180 = CIRCLE ( 'NONE', #104478, 5.499916801759985319 ) ;
#31181 = EDGE_CURVE ( 'NONE', #41312, #58330, #99939, .T. ) ;
#31182 = CARTESIAN_POINT ( 'NONE',  ( -2.211711111070695068, 1449.929476652820540, 182.9238327313504442 ) ) ;
#31183 = B_SPLINE_SURFACE_WITH_KNOTS ( 'NONE', 5, 5, ( 
 ( #93753, #14855, #85361, #27544, #300, #104253 ),
 ( #41176, #49045, #32224, #66404, #75350, #100523 ),
 ( #23802, #83724, #57994, #25449, #92127, #109490 ),
 ( #101060, #92669, #50147, #84274, #87464, #46021 ),
 ( #10755, #61726, #28649, #29197, #96965, #2925 ),
 ( #12928, #72321, #20230, #88564, #105358, #11848 ) ),
 .UNSPECIFIED., .F., .F., .F.,
 ( 6, 6 ),
 ( 6, 6 ),
 ( 9.285377752849999666, 26.18270615990000039 ),
 ( 0.000000000000000000, 2.000000000000000000 ),
 .UNSPECIFIED. ) ;
#31184 = ORIENTED_EDGE ( 'NONE', *, *, #73400, .F. ) ;
#31185 = DIRECTION ( 'NONE',  ( 0.000000000000000000, 0.000000000000000000, -1.000000000000000000 ) ) ;
#31186 = CARTESIAN_POINT ( 'NONE',  ( -0.01171164408179850049, 1516.939568781210028, 202.5649949355269825 ) ) ;
#31187 = B_SPLINE_SURFACE_WITH_KNOTS ( 'NONE', 5, 5, ( 
 ( #98142, #32045, #20880, #72963, #107101, #48319 ),
 ( #30390, #98699, #74068, #13569, #47754, #81889 ),
 ( #55077, #5192, #39347, #107656, #30942, #99229 ),
 ( #22507, #56709, #90844, #14129, #82460, #108198 ),
 ( #14688, #65667, #23076, #57283, #48877, #83002 ),
 ( #8481, #49414, #7939, #57823, #58913, #51064 ) ),
 .UNSPECIFIED., .F., .F., .F.,
 ( 6, 6 ),
 ( 6, 6 ),
 ( 3.432284486139999924, 15.04427212800000113 ),
 ( 0.000000000000000000, 2.000000000000000000 ),
 .UNSPECIFIED. ) ;
#31188 = CARTESIAN_POINT ( 'NONE',  ( -41.47274544121170692, 1445.558652941947912, 135.4389022873576778 ) ) ;
#31189 = CARTESIAN_POINT ( 'NONE',  ( 1.343905436027461819, 1508.993419142904713, 238.7384818784190941 ) ) ;
#31190 = CARTESIAN_POINT ( 'NONE',  ( -42.54898663771669476, 1436.084673314200018, 270.0692056436710118 ) ) ;
#31191 = LINE ( 'NONE', #91652, #56150 ) ;
#31192 = CARTESIAN_POINT ( 'NONE',  ( -5.776215019550000385, 1396.296062261430052, 198.6637670179979693 ) ) ;
#31194 = ORIENTED_EDGE ( 'NONE', *, *, #103543, .F. ) ;
#31193 = CARTESIAN_POINT ( 'NONE',  ( -8.121968579123178600, 1364.865207952712808, 208.3718459617061285 ) ) ;
#31195 = EDGE_LOOP ( 'NONE', ( #81969, #47057, #2468, #5911 ) ) ;
#31196 = DIRECTION ( 'NONE',  ( -1.000000000000000000, 0.000000000000000000, 0.000000000000000000 ) ) ;
#31197 = CARTESIAN_POINT ( 'NONE',  ( 3.874528905232604625, 1425.932572816098173, 185.2903555449227326 ) ) ;
#31198 = CARTESIAN_POINT ( 'NONE',  ( -11.95631299936500014, 1516.551704408390151, 216.1284114631369846 ) ) ;
#31199 = CARTESIAN_POINT ( 'NONE',  ( -20.69303424980000372, 1486.764600954290017, 209.1218459616989946 ) ) ;
#31200 = CARTESIAN_POINT ( 'NONE',  ( -2.062285449869999621, 1486.118212117930170, 181.8549132572979943 ) ) ;
#31201 = B_SPLINE_CURVE_WITH_KNOTS ( 'NONE', 3,
 ( #79602, #2906, #37025, #54954 ),
 .UNSPECIFIED., .F., .F.,
 ( 4, 4 ),
 ( -49.62857964555200141, -30.36953107781529937 ),
 .UNSPECIFIED. ) ;
#31203 = EDGE_CURVE ( 'NONE', #106581, #6621, #72410, .T. ) ;
#31202 = EDGE_CURVE ( 'NONE', #33799, #21086, #65820, .T. ) ;
#31204 = CARTESIAN_POINT ( 'NONE',  ( 7.726684687535000151, 1517.208444099459939, 210.2479840788170122 ) ) ;
#31205 = CARTESIAN_POINT ( 'NONE',  ( -68.75925446219999060, 1379.747924465840015, 280.1317017307590049 ) ) ;
#31206 = CARTESIAN_POINT ( 'NONE',  ( -2.177011892179100183, 1484.252254114900097, 183.0856693271300060 ) ) ;
#31207 = CARTESIAN_POINT ( 'NONE',  ( -14.21330248699999999, 1430.152305291330094, 222.3202484490980169 ) ) ;
#31208 = CARTESIAN_POINT ( 'NONE',  ( 0.000000000000000000, 1445.052233488290085, 126.8032249175980155 ) ) ;
#31209 = CARTESIAN_POINT ( 'NONE',  ( 11.76669761379999990, 1446.210547856740050, 187.6280415629979927 ) ) ;
#31210 = CARTESIAN_POINT ( 'NONE',  ( 4.610079833424999940, 1516.713079096360161, 207.9883289669969884 ) ) ;
#31211 = EDGE_CURVE ( 'NONE', #107129, #54363, #5914, .T. ) ;
#31212 = ORIENTED_EDGE ( 'NONE', *, *, #51476, .T. ) ;
#31213 = CARTESIAN_POINT ( 'NONE',  ( -29.40443212115400939, 1512.187213306747481, 196.1539082851718661 ) ) ;
#31214 = CARTESIAN_POINT ( 'NONE',  ( -11.30499956576250042, 1428.976642403380083, 112.4490109703959888 ) ) ;
#31215 = AXIS2_PLACEMENT_3D ( 'NONE', #38245, #64032, #98146 ) ;
#31216 = CARTESIAN_POINT ( 'NONE',  ( -23.83335724643239573, 1446.583467845320911, 213.8372151209257481 ) ) ;
#31217 = VERTEX_POINT ( 'NONE', #33288 ) ;
#31218 = DIRECTION ( 'NONE',  ( 0.02616798426500965835, -0.9993150019883683122, 0.02616798426500970692 ) ) ;
#31219 = CARTESIAN_POINT ( 'NONE',  ( 25.23107375087169757, 1451.155107251089930, 137.3931022878719830 ) ) ;
#31220 = CARTESIAN_POINT ( 'NONE',  ( 13.28956057169999916, 1415.163755984130148, 197.3206489009980089 ) ) ;
#31221 = CARTESIAN_POINT ( 'NONE',  ( -9.097854467734780570, 1384.691521587119723, 199.9510732930289976 ) ) ;
#31222 = CARTESIAN_POINT ( 'NONE',  ( 19.78689921630000015, 1409.768476627529935, 198.2512349542980132 ) ) ;
#31223 = CARTESIAN_POINT ( 'NONE',  ( 29.99620953741488449, 1526.382868172863937, 198.4974435154498735 ) ) ;
#31224 = CARTESIAN_POINT ( 'NONE',  ( 12.03449221500000199, 1491.353386477190043, 206.6667661068590292 ) ) ;
#31225 = CARTESIAN_POINT ( 'NONE',  ( -0.1622545728502209350, 1506.474306126712690, 187.1056287556957045 ) ) ;
#31226 = CARTESIAN_POINT ( 'NONE',  ( 4.245220697766579399, 1441.395571263719830, 161.9150406115920191 ) ) ;
#31227 = DIRECTION ( 'NONE',  ( -1.755985294532469921E-16, 1.000000000000000000, -1.338183447452831989E-16 ) ) ;
#31228 = CARTESIAN_POINT ( 'NONE',  ( 17.99277867620000038, 1432.534352819589913, 212.7098897757189775 ) ) ;
#31229 = CARTESIAN_POINT ( 'NONE',  ( 4.617490466775000080, 1516.685667699390024, 216.4467608883869900 ) ) ;
#31230 = ORIENTED_EDGE ( 'NONE', *, *, #24172, .F. ) ;
#31231 = CARTESIAN_POINT ( 'NONE',  ( 7.709251280239639570, 1516.542689134859984, 207.3693600638700048 ) ) ;
#31232 = CARTESIAN_POINT ( 'NONE',  ( 8.486023334060119439, 1517.151704408390060, 207.2139745301958271 ) ) ;
#31233 = CARTESIAN_POINT ( 'NONE',  ( -0.2459700386814729911, 1408.921650059179910, 231.8163769252240058 ) ) ;
#31234 = CARTESIAN_POINT ( 'NONE',  ( -2.755131347899999916, 1422.216165794629887, 90.98709265669789659 ) ) ;
#31235 = CARTESIAN_POINT ( 'NONE',  ( 1.146125081599999929, 1474.496542508589982, 219.7253671311989933 ) ) ;
#31236 = CARTESIAN_POINT ( 'NONE',  ( 30.24726669678259938, 1509.969318215629983, 207.3401543782560168 ) ) ;
#31237 = CARTESIAN_POINT ( 'NONE',  ( 11.60004869885391443, 1426.112340653894762, 139.0390921710123564 ) ) ;
#31238 = CARTESIAN_POINT ( 'NONE',  ( -0.4151546846821904668, 1524.726013923371283, 173.3106345060153330 ) ) ;
#31239 = CARTESIAN_POINT ( 'NONE',  ( -2.500000000000000000, 1432.110435327849927, 157.4891270399980101 ) ) ;
#31240 = CARTESIAN_POINT ( 'NONE',  ( -12.31949146158819985, 1378.253793448930082, 209.5105130821430066 ) ) ;
#31241 = CARTESIAN_POINT ( 'NONE',  ( -1.776356839399999804E-15, 1414.661898229710005, 209.1218459616989946 ) ) ;
#31242 = CARTESIAN_POINT ( 'NONE',  ( 28.69268220582149809, 1440.913060387340010, 233.8417140319789951 ) ) ;
#31244 = CARTESIAN_POINT ( 'NONE',  ( 9.907316696420009450, 1469.648968762289996, 210.8737231108960088 ) ) ;
#31243 = CARTESIAN_POINT ( 'NONE',  ( -9.772455935529970716, 1472.076110283059961, 211.9302343523150114 ) ) ;
#31245 = CARTESIAN_POINT ( 'NONE',  ( 10.81518794224679958, 1424.921099295370141, 144.1705737284439977 ) ) ;
#31246 = EDGE_LOOP ( 'NONE', ( #65772, #27707, #36471, #2664 ) ) ;
#31247 = ORIENTED_EDGE ( 'NONE', *, *, #109623, .T. ) ;
#31248 = AXIS2_PLACEMENT_3D ( 'NONE', #42934, #15492, #77092 ) ;
#31249 = CARTESIAN_POINT ( 'NONE',  ( 12.53380498098208840, 1442.773887284840384, 206.9039879563480326 ) ) ;
#31250 = FACE_OUTER_BOUND ( 'NONE', #44309, .T. ) ;
#31251 = CARTESIAN_POINT ( 'NONE',  ( -1.843107666119999877, 1444.183210091189949, 199.2363500995090249 ) ) ;
#31252 = CARTESIAN_POINT ( 'NONE',  ( 8.270286460330000367, 1424.455427991309989, 195.9054154081989907 ) ) ;
#31253 = CARTESIAN_POINT ( 'NONE',  ( -14.47255314515679991, 1379.648765529259890, 208.1785496007449865 ) ) ;
#31254 = AXIS2_PLACEMENT_3D ( 'NONE', #20748, #12359, #98566 ) ;
#31255 = CARTESIAN_POINT ( 'NONE',  ( 23.68614698517409067, 1509.855248197463879, 227.6068541032486223 ) ) ;
#31256 = CIRCLE ( 'NONE', #22272, 4.014133627551895067 ) ;
#31257 = CARTESIAN_POINT ( 'NONE',  ( -17.38483621660000011, 1410.884422118429939, 225.7833436061980024 ) ) ;
#31258 = CARTESIAN_POINT ( 'NONE',  ( -0.4832821051016459868, 1508.551704408389924, 220.0496842192639804 ) ) ;
#31259 = CARTESIAN_POINT ( 'NONE',  ( -40.54665132019379570, 1383.827310385500141, 242.7435723248869976 ) ) ;
#31260 = CARTESIAN_POINT ( 'NONE',  ( -5.121512578775000435, 1511.279956263560052, 201.1879310057669841 ) ) ;
#31261 = CARTESIAN_POINT ( 'NONE',  ( -13.02791578709999953, 1434.994518313060098, 194.2036555078979632 ) ) ;
#31262 = CARTESIAN_POINT ( 'NONE',  ( -12.56112213346830053, 1502.620980619200054, 209.0016574251579868 ) ) ;
#31263 = CARTESIAN_POINT ( 'NONE',  ( 1.604557024660000053, 1465.957280275429866, 234.9244852315979699 ) ) ;
#31265 = ORIENTED_EDGE ( 'NONE', *, *, #26905, .T. ) ;
#31264 = CARTESIAN_POINT ( 'NONE',  ( -3.163820906539999811, 1456.764302747290003, 218.0770706517390067 ) ) ;
#31266 = CARTESIAN_POINT ( 'NONE',  ( -0.8347645832880000727, 1451.405209460129981, 182.9461533385980090 ) ) ;
#31267 = CARTESIAN_POINT ( 'NONE',  ( -17.67357672280000003, 1382.321958893279771, 219.3032393030590015 ) ) ;
#31268 = CARTESIAN_POINT ( 'NONE',  ( 4.554659021567319499, 1508.551704408389924, 205.2297450218139829 ) ) ;
#31270 = EDGE_LOOP ( 'NONE', ( #71727, #80658, #10135, #8865, #92187, #45344 ) ) ;
#31269 = LINE ( 'NONE', #4433, #7216 ) ;
#31271 = ORIENTED_EDGE ( 'NONE', *, *, #77821, .T. ) ;
#31272 = PRODUCT ( 'Crank Arm', 'Crank Arm', '', ( #5156 ) ) ;
#31273 = CARTESIAN_POINT ( 'NONE',  ( -3.665756888920000289, 1509.051704408389924, 204.1347675262390169 ) ) ;
#31274 = CARTESIAN_POINT ( 'NONE',  ( 34.88060122484030501, 1437.118155287319951, 136.5398807287430145 ) ) ;
#31275 = CARTESIAN_POINT ( 'NONE',  ( 11.90000415720300175, 1434.913060496859998, 147.6452464505769910 ) ) ;
#31276 = DIRECTION ( 'NONE',  ( -5.980589973904019347E-17, 1.000000000000000000, -1.736889445713099699E-16 ) ) ;
#31277 = CARTESIAN_POINT ( 'NONE',  ( -106.9415904979999965, 1381.793463357829978, 298.5192869564590410 ) ) ;
#31278 = CYLINDRICAL_SURFACE ( 'NONE', #91094, 4.000000000000000000 ) ;
#31279 = CARTESIAN_POINT ( 'NONE',  ( -3.321447364419999548, 1484.261043626330093, 183.3707343507980170 ) ) ;
#31280 = CARTESIAN_POINT ( 'NONE',  ( 13.45932853639649984, 1409.383070496670143, 202.6355491842259937 ) ) ;
#31281 = CARTESIAN_POINT ( 'NONE',  ( 18.80464664967999866, 1425.799544216437880, 225.6097399491019928 ) ) ;
#31282 = CARTESIAN_POINT ( 'NONE',  ( 156.6846457583332892, 1524.382868172863937, 77.25240589481998654 ) ) ;
#31283 = CARTESIAN_POINT ( 'NONE',  ( -18.59366407810000155, 1470.691086342629887, 190.0416152128979945 ) ) ;
#31284 = CARTESIAN_POINT ( 'NONE',  ( 10.96867220289999878, 1432.296152391259739, 151.7700998162980000 ) ) ;
#31285 = CARTESIAN_POINT ( 'NONE',  ( -2.402297588538860218, 1450.020914723239912, 183.8092250355219903 ) ) ;
#31286 = ORIENTED_EDGE ( 'NONE', *, *, #61646, .F. ) ;
#31287 = AXIS2_PLACEMENT_3D ( 'NONE', #67, #8433, #10101 ) ;
#31288 = CARTESIAN_POINT ( 'NONE',  ( 20.71343476517798621, 1522.906561336852974, 238.3377464195744722 ) ) ;
#31289 = DIRECTION ( 'NONE',  ( 0.000000000000000000, 0.000000000000000000, 1.000000000000000000 ) ) ;
#31290 = CARTESIAN_POINT ( 'NONE',  ( -12.30110944409999973, 1435.657202184449943, 151.0470392402980053 ) ) ;
#31291 = CARTESIAN_POINT ( 'NONE',  ( 3.347731885920769895E-10, 1465.323236593859974, 238.9305512232619719 ) ) ;
#31292 = CARTESIAN_POINT ( 'NONE',  ( -20.35676096567760140, 1499.986133293800094, 190.6179917588589774 ) ) ;
#31293 = CARTESIAN_POINT ( 'NONE',  ( -15.31114377250000125, 1420.272718699760162, 211.9351904690790036 ) ) ;
#31294 = CARTESIAN_POINT ( 'NONE',  ( -109.1721745879999901, 1385.500491102209935, 311.2318004082590051 ) ) ;
#31295 = CARTESIAN_POINT ( 'NONE',  ( -8.454424074398959377, 1511.603884447429891, 214.9855816549980148 ) ) ;
#31296 = CARTESIAN_POINT ( 'NONE',  ( -9.569455633217616608, 1362.104322562968264, 207.6218459616987673 ) ) ;
#31297 = CARTESIAN_POINT ( 'NONE',  ( -46.27186622794469884, 1440.245173416720036, 267.5896806125069816 ) ) ;
#31298 = CYLINDRICAL_SURFACE ( 'NONE', #15808, 1.000000000000000888 ) ;
#31299 = CARTESIAN_POINT ( 'NONE',  ( 3.316380893998936763, 1524.425415513988810, 176.3365459558180817 ) ) ;
#31300 = CARTESIAN_POINT ( 'NONE',  ( -6.951517170504999399, 1517.194816588360027, 207.9969518818670053 ) ) ;
#31301 = CARTESIAN_POINT ( 'NONE',  ( -26.35475552313950232, 1507.985742420310089, 201.5462045797129917 ) ) ;
#31302 = B_SPLINE_SURFACE_WITH_KNOTS ( 'NONE', 5, 5, ( 
 ( #91868, #90765, #49332, #84568, #30856, #108112 ),
 ( #7317, #22427, #66697, #108672, #24633, #58829 ),
 ( #6753, #92407, #57198, #41481, #83458, #75642 ),
 ( #31406, #14604, #65588, #48794, #92967, #31962 ),
 ( #66155, #7858, #107569, #56629, #14045, #6208 ),
 ( #39821, #74540, #48235, #57748, #82376, #101903 ) ),
 .UNSPECIFIED., .F., .F., .F.,
 ( 6, 6 ),
 ( 6, 6 ),
 ( 123.8981301339999987, 143.2822930469999960 ),
 ( 0.000000000000000000, 2.000000000000000000 ),
 .UNSPECIFIED. ) ;
#31303 = CARTESIAN_POINT ( 'NONE',  ( 6.942384827123182056, 1508.551704408389924, 200.9625026564361292 ) ) ;
#31304 = CARTESIAN_POINT ( 'NONE',  ( 7.275136103057380232, 1425.000205421479905, 212.7055067982740013 ) ) ;
#31305 = ORIENTED_EDGE ( 'NONE', *, *, #4667, .F. ) ;
#31306 = EDGE_CURVE ( 'NONE', #100091, #32688, #35799, .T. ) ;
#31307 = CARTESIAN_POINT ( 'NONE',  ( 39.71667995010000141, 1438.440173428300113, 259.0958843804980347 ) ) ;
#31308 = DIRECTION ( 'NONE',  ( -1.000000000000000000, 0.000000000000000000, 0.000000000000000000 ) ) ;
#31310 = CARTESIAN_POINT ( 'NONE',  ( -17.60627563539999940, 1410.895669414830081, 194.0661810347980065 ) ) ;
#31309 = CARTESIAN_POINT ( 'NONE',  ( -1.490778394210000135, 1464.110353063229923, 182.6238274118979916 ) ) ;
#31311 = CARTESIAN_POINT ( 'NONE',  ( -1.255439442925828430, 1407.658910741955879, 270.1375224078223596 ) ) ;
#31312 = CARTESIAN_POINT ( 'NONE',  ( -25.89722382409999923, 1435.736014097309862, 225.2448095317979835 ) ) ;
#31313 = CARTESIAN_POINT ( 'NONE',  ( -28.93366682225746089, 1509.926821294354568, 203.5275689439237965 ) ) ;
#31314 = EDGE_CURVE ( 'NONE', #103948, #46147, #79421, .T. ) ;
#31315 = CARTESIAN_POINT ( 'NONE',  ( -10.29290297689570011, 1452.553624295069994, 150.4708687035819992 ) ) ;
#31316 = CARTESIAN_POINT ( 'NONE',  ( 18.12896501882653411, 1435.130582088436313, 143.3945274339172329 ) ) ;
#31317 = ORIENTED_EDGE ( 'NONE', *, *, #104403, .T. ) ;
#31318 = CARTESIAN_POINT ( 'NONE',  ( -107.6093135319519973, 1378.913060387369796, 300.4165847144340091 ) ) ;
#31319 = CARTESIAN_POINT ( 'NONE',  ( 3.718673206215620104E-05, 1408.561116146350059, 270.4290838584209951 ) ) ;
#31320 = DIRECTION ( 'NONE',  ( 0.000000000000000000, -1.836970198721029688E-16, -1.000000000000000000 ) ) ;
#31321 = CARTESIAN_POINT ( 'NONE',  ( 10.36617021350000023, 1462.084514122090013, 211.0499682573590121 ) ) ;
#31322 = EDGE_LOOP ( 'NONE', ( #31997, #72376, #27320, #11649, #96887 ) ) ;
#31323 = ORIENTED_EDGE ( 'NONE', *, *, #19892, .F. ) ;
#31324 = CARTESIAN_POINT ( 'NONE',  ( -9.851472566700000044, 1384.510545767029953, 199.8981574268189831 ) ) ;
#31325 = CARTESIAN_POINT ( 'NONE',  ( -24.13064078950060320, 1411.115359567930000, 208.8754834058540268 ) ) ;
#31326 = ORIENTED_EDGE ( 'NONE', *, *, #33065, .T. ) ;
#31327 = CARTESIAN_POINT ( 'NONE',  ( 3.910153960660829764, 1508.551704408439946, 204.2884083744090162 ) ) ;
#31328 = CARTESIAN_POINT ( 'NONE',  ( -13.93783161230000012, 1507.632723584029918, 232.3716436017979845 ) ) ;
#31329 = CARTESIAN_POINT ( 'NONE',  ( 2.487923749338929902, 1508.731372610989865, 213.6767948862569995 ) ) ;
#31330 = CARTESIAN_POINT ( 'NONE',  ( 45.57954469825010335, 1446.130764200959902, 268.5106337247650004 ) ) ;
#31331 = AXIS2_PLACEMENT_3D ( 'NONE', #84302, #82659, #108964 ) ;
#31332 = CARTESIAN_POINT ( 'NONE',  ( -12.61823209568500026, 1416.826860677879949, 222.0544590270410197 ) ) ;
#31333 = CARTESIAN_POINT ( 'NONE',  ( 0.2417153426969999852, 1418.558758520830224, 184.6769579382979884 ) ) ;
#31334 = CARTESIAN_POINT ( 'NONE',  ( -2.296124889065000119, 1516.677239312369920, 204.5136991508470032 ) ) ;
#31335 = ADVANCED_FACE ( 'NONE', ( #90992 ), #93794, .F. ) ;
#31336 = VERTEX_POINT ( 'NONE', #22475 ) ;
#31337 = CARTESIAN_POINT ( 'NONE',  ( 11.48584737056929939, 1480.327931592909863, 211.7937108438270002 ) ) ;
#31339 = B_SPLINE_CURVE_WITH_KNOTS ( 'NONE', 5,
 ( #25219, #68934, #1168, #95211, #9538, #86804, #103607, #59423, #42599, #101932, #17921, #34195, #93535, #26332, #19024, #76755, #95759, #86247 ),
 .UNSPECIFIED., .F., .F.,
 ( 6, 3, 3, 3, 3, 6 ),
 ( 15.88432520349999955, 16.90079360149999843, 18.14364336469999728, 21.12354018079999918, 24.53920724549999832, 25.22570695429999788 ),
 .UNSPECIFIED. ) ;
#31338 = CARTESIAN_POINT ( 'NONE',  ( 22.12673968580000050, 1409.685743163530105, 208.3470067452770138 ) ) ;
#31340 = CARTESIAN_POINT ( 'NONE',  ( 12.98890325061326756, 1442.943211643413406, 187.1799295177850695 ) ) ;
#31341 = EDGE_LOOP ( 'NONE', ( #14382, #54359, #52125, #108902, #62336 ) ) ;
#31342 = VERTEX_POINT ( 'NONE', #56675 ) ;
#31343 = CARTESIAN_POINT ( 'NONE',  ( 2.038847259681869861, 1522.861859112239244, 173.3106345060298565 ) ) ;
#31344 = DIRECTION ( 'NONE',  ( 0.000000000000000000, 1.000000000000000000, 0.000000000000000000 ) ) ;
#31345 = CARTESIAN_POINT ( 'NONE',  ( -13.96132456265650035, 1513.058738973280015, 193.8412935603610094 ) ) ;
#31346 = CARTESIAN_POINT ( 'NONE',  ( 8.841553233067839912, 1503.647460366240011, 218.3045275839649833 ) ) ;
#31347 = CARTESIAN_POINT ( 'NONE',  ( 9.568810912189999129, 1420.789473812500091, 197.0881969165990029 ) ) ;
#31348 = CARTESIAN_POINT ( 'NONE',  ( -4.140517654259704194, 1426.000593950702523, 186.1118291128992155 ) ) ;
#31350 = B_SPLINE_CURVE_WITH_KNOTS ( 'NONE', 3,
 ( #36265, #1578, #38321, #87224, #26756, #17771, #62051, #4723, #104575, #18890, #10514, #29918, #60378, #47288, #18339, #96176, #19451, #53650, #35712, #69341, #72500, #106629, #52530, #86116, #38867, #86663, #87794, #2144, #9957, #11078, #70454, #45245, #26190, #60944, #44129, #95073, #78264, #13105, #61492, #51974 ),
 .UNSPECIFIED., .F., .F.,
 ( 4, 3, 3, 3, 3, 3, 3, 3, 3, 3, 3, 3, 3, 4 ),
 ( -1.449276807229999964, -1.377900617911430148, -1.266157031164990121, -1.152673605843979932, -1.038158481000059918, -0.9221425583362260481, -0.8054446481160930649, -0.6883773969095410283, -0.5712841841444460389, -0.4548595335433320841, -0.3393020229786609665, -0.2248662951613220606, -0.1117297126499861015, 0.000000000000000000 ),
 .UNSPECIFIED. ) ;
#31349 = CARTESIAN_POINT ( 'NONE',  ( -108.5358826105733812, 1381.246854040435437, 297.9911112566219344 ) ) ;
#31351 = CARTESIAN_POINT ( 'NONE',  ( -5.264762213780000089, 1496.215614374990082, 199.2138355340389921 ) ) ;
#31352 = CARTESIAN_POINT ( 'NONE',  ( 33.91369120209999721, 1435.681798817170147, 134.0999999980979851 ) ) ;
#31354 = CARTESIAN_POINT ( 'NONE',  ( -105.5686611308969987, 1391.210113098429929, 305.6570713065560199 ) ) ;
#31353 = CARTESIAN_POINT ( 'NONE',  ( 30.57821243133773947, 1525.253972588462602, 196.6735172117064110 ) ) ;
#31355 = CARTESIAN_POINT ( 'NONE',  ( 11.18609796984200067, 1425.994771849919971, 206.4955550758209881 ) ) ;
#31356 = CARTESIAN_POINT ( 'NONE',  ( -24.20611828920600317, 1508.692521244279988, 222.4038325357350061 ) ) ;
#31357 = CARTESIAN_POINT ( 'NONE',  ( -7.651189275224999697, 1514.325389163589989, 203.4154480846970046 ) ) ;
#31358 = ORIENTED_EDGE ( 'NONE', *, *, #65951, .T. ) ;
#31359 = CARTESIAN_POINT ( 'NONE',  ( 12.58190538649999901, 1415.948532225030021, 222.2791103911980031 ) ) ;
#31360 = CARTESIAN_POINT ( 'NONE',  ( -17.18283320249707913, 1417.508594224242870, 206.5901238511499400 ) ) ;
#31361 = CARTESIAN_POINT ( 'NONE',  ( -83.32062985459390347, 1384.985472285010019, 305.8467810391779835 ) ) ;
#31362 = CIRCLE ( 'NONE', #8100, 1.999999999999999556 ) ;
#31363 = CARTESIAN_POINT ( 'NONE',  ( -8.264565553860000691, 1386.032785243389981, 199.7638704706089925 ) ) ;
#31364 = CARTESIAN_POINT ( 'NONE',  ( -15.74296179209999913, 1415.733199231679919, 209.6832678893589730 ) ) ;
#31366 = EDGE_LOOP ( 'NONE', ( #74837, #32664, #104506, #103877, #95505 ) ) ;
#31365 = CARTESIAN_POINT ( 'NONE',  ( 11.26951302955830059, 1422.439921091280212, 203.3658004337269745 ) ) ;
#31367 = CARTESIAN_POINT ( 'NONE',  ( 11.60004869885206880, 1428.983126981192754, 137.0999999980979851 ) ) ;
#31368 = CARTESIAN_POINT ( 'NONE',  ( 16.62350534370850141, 1524.082740465118604, 237.7032228575765771 ) ) ;
#31369 = CARTESIAN_POINT ( 'NONE',  ( -16.33362175549999762, 1416.748655660220038, 208.2080258544030187 ) ) ;
#31370 = CARTESIAN_POINT ( 'NONE',  ( 11.21036242749999978, 1433.950538822089811, 151.6031954420979844 ) ) ;
#31371 = CARTESIAN_POINT ( 'NONE',  ( 1.776356839399999804E-15, 1469.463552837929910, 265.6112251771979800 ) ) ;
#31372 = CARTESIAN_POINT ( 'NONE',  ( 3.149414619133680482, 1370.221588481574372, 210.2153961732977905 ) ) ;
#31373 = CIRCLE ( 'NONE', #2799, 1.999999999999998668 ) ;
#31374 = CARTESIAN_POINT ( 'NONE',  ( 2.921131820879320440, 1415.930151663460038, 231.8786077272699799 ) ) ;
#31375 = CARTESIAN_POINT ( 'NONE',  ( -108.2947392991006978, 1388.907026348439786, 298.1986017272994900 ) ) ;
#31376 = CARTESIAN_POINT ( 'NONE',  ( 11.12931921225938225, 1512.151624459632103, 224.9062103328911633 ) ) ;
#31377 = CARTESIAN_POINT ( 'NONE',  ( -21.86721050905262587, 1523.611961620354123, 235.0400593884483840 ) ) ;
#31378 = CARTESIAN_POINT ( 'NONE',  ( -113.4000000000000057, 1384.926148861439970, 304.2218459572590064 ) ) ;
#31379 = CARTESIAN_POINT ( 'NONE',  ( -17.19048262749999978, 1409.513365268830057, 224.2117643060980186 ) ) ;
#31380 = CARTESIAN_POINT ( 'NONE',  ( 28.35863496383795379, 1526.382868172863937, 219.7167431890427451 ) ) ;
#31381 = CARTESIAN_POINT ( 'NONE',  ( -1.339831530989999964, 1424.180425965929999, 228.4049732387980214 ) ) ;
#31382 = CARTESIAN_POINT ( 'NONE',  ( 4.649753459270000278, 1460.482125307190017, 203.9966562023689676 ) ) ;
#31383 = CARTESIAN_POINT ( 'NONE',  ( 5.451195050909999503E-14, 1410.389826760030019, 269.3346704430979912 ) ) ;
#31384 = CARTESIAN_POINT ( 'NONE',  ( 3.810920848475609887E-07, 1407.244912221920004, 196.0950346751619691 ) ) ;
#31385 = CARTESIAN_POINT ( 'NONE',  ( 21.60894078433416610, 1517.051704408389924, 218.5714488934191309 ) ) ;
#31386 =( BOUNDED_CURVE ( )  B_SPLINE_CURVE ( 3, ( #31279, #57062, #16651, #50317 ),
 .UNSPECIFIED., .F., .F. ) 
 B_SPLINE_CURVE_WITH_KNOTS ( ( 4, 4 ),
 ( 4.159034560815309867, 5.265743431342809977 ),
 .UNSPECIFIED. ) 
 CURVE ( )  GEOMETRIC_REPRESENTATION_ITEM ( )  RATIONAL_B_SPLINE_CURVE ( ( 1.000000000000000000, 0.9005109389839739409, 0.9005109389839739409, 1.000000000000000000 ) ) 
 REPRESENTATION_ITEM ( '' )  );
#31387 = CARTESIAN_POINT ( 'NONE',  ( -17.65532977206540011, 1419.497220819440145, 207.2321560918570071 ) ) ;
#31388 = CARTESIAN_POINT ( 'NONE',  ( -8.218607532720000108, 1415.425433635630043, 224.6826798189979968 ) ) ;
#31389 = DIRECTION ( 'NONE',  ( 0.000000000000000000, 0.000000000000000000, -1.000000000000000000 ) ) ;
#31391 = VERTEX_POINT ( 'NONE', #98106 ) ;
#31390 = CARTESIAN_POINT ( 'NONE',  ( -13.40477891429999957, 1409.381165581829919, 216.6964573264080229 ) ) ;
#31392 = CARTESIAN_POINT ( 'NONE',  ( -14.64149002350000117, 1416.824060884929850, 198.5247578393980064 ) ) ;
#31393 = B_SPLINE_CURVE_WITH_KNOTS ( 'NONE', 3,
 ( #94696, #45427, #69533, #35908, #28599, #62800 ),
 .UNSPECIFIED., .F., .F.,
 ( 4, 2, 4 ),
 ( -1.285435071100343021E-05, 0.001079388306740753593, 0.002171630964192510903 ),
 .UNSPECIFIED. ) ;
#31394 = CARTESIAN_POINT ( 'NONE',  ( 17.71193101166619854, 1519.551704408389924, 196.6727161458730109 ) ) ;
#31395 = CARTESIAN_POINT ( 'NONE',  ( 12.91318184880000075, 1434.774345493619876, 147.9456464303979715 ) ) ;
#31396 = CARTESIAN_POINT ( 'NONE',  ( -26.79413161609999960, 1436.761919078669962, 136.7821860783980128 ) ) ;
#31397 = CARTESIAN_POINT ( 'NONE',  ( 5.767944999630000069, 1441.815290517450194, 183.8476023479979915 ) ) ;
#31398 = ORIENTED_EDGE ( 'NONE', *, *, #4863, .F. ) ;
#31399 = CARTESIAN_POINT ( 'NONE',  ( -17.59770716511913591, 1524.659802833170716, 180.6838038464929639 ) ) ;
#31400 = CARTESIAN_POINT ( 'NONE',  ( 4.114426077449999219, 1478.089653320190109, 199.4391987246589792 ) ) ;
#31401 = CARTESIAN_POINT ( 'NONE',  ( -104.7665161994586072, 1380.738255385528419, 308.0305743392281101 ) ) ;
#31402 = CARTESIAN_POINT ( 'NONE',  ( -11.05734857760000089, 1492.520961800689975, 208.6928883350419994 ) ) ;
#31403 = CARTESIAN_POINT ( 'NONE',  ( 0.8634109271070009584, 1463.906666237789977, 202.1056695248490200 ) ) ;
#31404 = CARTESIAN_POINT ( 'NONE',  ( 33.97073229624528778, 1418.068708379463715, 269.2736084937218379 ) ) ;
#31405 = CARTESIAN_POINT ( 'NONE',  ( -13.04097860699999956, 1380.055736578640108, 210.2016245823089946 ) ) ;
#31406 = CARTESIAN_POINT ( 'NONE',  ( 2.500000000000000000, 1431.405490208399897, 183.1416673773980222 ) ) ;
#31407 = CARTESIAN_POINT ( 'NONE',  ( -60.86887317925939556, 1385.065624857220200, 245.8709774141379967 ) ) ;
#31408 = CARTESIAN_POINT ( 'NONE',  ( -12.24666832539229944, 1490.299283743809838, 209.4193319484280096 ) ) ;
#31409 = CARTESIAN_POINT ( 'NONE',  ( -26.81185740190621303, 1435.935043934885243, 136.4231258368600663 ) ) ;
#31410 = VERTEX_POINT ( 'NONE', #4617 ) ;
#31411 = CARTESIAN_POINT ( 'NONE',  ( -27.78835038220000087, 1451.943064120830059, 135.3296735906980075 ) ) ;
#31412 = CARTESIAN_POINT ( 'NONE',  ( -16.33802103553490070, 1410.720457927129928, 226.6282205582409972 ) ) ;
#31414 = ORIENTED_EDGE ( 'NONE', *, *, #85617, .T. ) ;
#31413 = CARTESIAN_POINT ( 'NONE',  ( 0.4918970380822089705, 1416.941427595080086, 184.7882001716829734 ) ) ;
#31415 = CARTESIAN_POINT ( 'NONE',  ( -109.1321491280000089, 1384.869787261709916, 311.2644938432590038 ) ) ;
#31417 = CARTESIAN_POINT ( 'NONE',  ( 9.985337640048900454, 1470.806041673749860, 211.4815898445349944 ) ) ;
#31416 = AXIS2_PLACEMENT_3D ( 'NONE', #39494, #3714, #13157 ) ;
#31418 = CARTESIAN_POINT ( 'NONE',  ( 17.89866715925209917, 1430.472632720380034, 212.6087062095869840 ) ) ;
#31419 = CARTESIAN_POINT ( 'NONE',  ( -109.9878849640000027, 1384.810441490199992, 311.4547210892589533 ) ) ;
#31420 = CARTESIAN_POINT ( 'NONE',  ( -0.1687673399551990194, 1419.486623560560020, 184.4224968243179887 ) ) ;
#31421 = CARTESIAN_POINT ( 'NONE',  ( 1.172684541229999988, 1466.870711192130102, 235.2669543350980064 ) ) ;
#31422 = CARTESIAN_POINT ( 'NONE',  ( 19.25129681859999664, 1409.750010412430129, 220.2447021582979971 ) ) ;
#31423 = B_SPLINE_SURFACE_WITH_KNOTS ( 'NONE', 5, 5, ( 
 ( #88573, #77953, #19694, #53897, #37049, #36503 ),
 ( #61193, #28658, #70147, #62288, #43803, #52220 ),
 ( #88032, #104810, #19124, #96416, #53324, #1825 ),
 ( #86347, #11316, #45486, #11856, #70699, #35398 ),
 ( #18570, #87472, #2386, #79628, #34840, #78514 ),
 ( #46029, #1259, #69031, #2932, #54440, #103132 ),
 ( #71245, #9631, #105368, #62863, #69586, #103704 ),
 ( #27004, #35960, #52765, #86904, #104260, #27551 ),
 ( #61733, #99137, #89651, #12394, #90752, #56617 ),
 ( #98600, #64485, #37606, #81791, #22414, #30843 ),
 ( #107004, #21864, #13474, #73969, #56063, #20781 ),
 ( #80157, #65576, #91309, #14031, #38151, #31396 ) ),
 .UNSPECIFIED., .F., .F., .F.,
 ( 6, 3, 3, 6 ),
 ( 6, 6 ),
 ( 13.64477700820000017, 16.39774826220000037, 20.55756172009999716, 23.69575850009999840 ),
 ( 0.000000000000000000, 1.506046440610000037 ),
 .UNSPECIFIED. ) ;
#31424 = CARTESIAN_POINT ( 'NONE',  ( -1.981971470188760298, 1412.641733730590204, 186.1285722913719951 ) ) ;
#31425 = CARTESIAN_POINT ( 'NONE',  ( -9.746793100592970660, 1463.060628619970203, 228.0587242826289867 ) ) ;
#31426 = CARTESIAN_POINT ( 'NONE',  ( -17.42096267240000174, 1423.098173955330140, 226.5666896228979965 ) ) ;
#31428 = DIRECTION ( 'NONE',  ( 0.8775825618903727587, 9.629649721936177897E-33, 0.4794255386042027833 ) ) ;
#31427 = CARTESIAN_POINT ( 'NONE',  ( -4.607530503061391336, 1511.399179795973851, 200.7291179019183005 ) ) ;
#31429 = CARTESIAN_POINT ( 'NONE',  ( 6.906779328069999835, 1480.511272950890088, 206.6585084482690036 ) ) ;
#31430 = CARTESIAN_POINT ( 'NONE',  ( -107.1941519259529230, 1348.229899472571105, 305.8064591614598839 ) ) ;
#31431 = CARTESIAN_POINT ( 'NONE',  ( -3.145663868875199221, 1370.195136005008180, 207.6218459616987673 ) ) ;
#31432 = CARTESIAN_POINT ( 'NONE',  ( -13.31089767776890120, 1503.456584347970193, 208.6977459380580058 ) ) ;
#31433 = CARTESIAN_POINT ( 'NONE',  ( -5.512208796550649659, 1374.913060387289988, 203.3071194642340345 ) ) ;
#31434 = B_SPLINE_CURVE_WITH_KNOTS ( 'NONE', 3,
 ( #9749, #278, #93729, #17008, #77520, #43915, #51207, #49149, #820, #60742, #40728, #85336, #18139, #52882, #52335, #86458 ),
 .UNSPECIFIED., .F., .F.,
 ( 4, 3, 3, 3, 3, 4 ),
 ( -7.874164595100000774, -7.551475176867179506, -6.470576537018629892, -5.390579508517740592, -4.310775221818579972, -3.231130238939999622 ),
 .UNSPECIFIED. ) ;
#31435 = CARTESIAN_POINT ( 'NONE',  ( 6.935457925184999262, 1516.627618683580067, 205.6664679548470076 ) ) ;
#31436 = CARTESIAN_POINT ( 'NONE',  ( -3.481831347839449808, 1485.997118152289886, 182.2030801867670107 ) ) ;
#31437 = CARTESIAN_POINT ( 'NONE',  ( -4.221414803702270291, 1441.605272108680083, 169.3185911052280233 ) ) ;
#31439 = ORIENTED_EDGE ( 'NONE', *, *, #9351, .F. ) ;
#31438 = CARTESIAN_POINT ( 'NONE',  ( -68.69955443098810122, 1379.747795958880261, 280.2901399885819842 ) ) ;
#31440 = ORIENTED_EDGE ( 'NONE', *, *, #55688, .T. ) ;
#31441 = DIRECTION ( 'NONE',  ( 0.03173147633655607619, -0.9969860201949453105, -0.07079540200709832920 ) ) ;
#31442 = ORIENTED_EDGE ( 'NONE', *, *, #105511, .T. ) ;
#31443 = CARTESIAN_POINT ( 'NONE',  ( -0.5979661643004559046, 1486.030882971970186, 221.0048940962329880 ) ) ;
#31444 = AXIS2_PLACEMENT_3D ( 'NONE', #53347, #38172, #106484 ) ;
#31445 = CARTESIAN_POINT ( 'NONE',  ( 11.39601957930000076, 1501.670084141789857, 207.8884637162790057 ) ) ;
#31447 = CARTESIAN_POINT ( 'NONE',  ( 16.15586037378450257, 1410.120038459840089, 191.7753741660440028 ) ) ;
#31446 = CARTESIAN_POINT ( 'NONE',  ( -11.74292464122704160, 1426.692342792548061, 144.5930205200747025 ) ) ;
#31448 = CARTESIAN_POINT ( 'NONE',  ( -4.610079871555000430, 1516.713079096360161, 210.2553629353369899 ) ) ;
#31449 = CARTESIAN_POINT ( 'NONE',  ( -11.43737779389999965, 1425.481201409729920, 144.1652972830979991 ) ) ;
#31450 = FACE_OUTER_BOUND ( 'NONE', #110584, .T. ) ;
#31451 = CARTESIAN_POINT ( 'NONE',  ( 12.45552494207550076, 1501.256435928469955, 211.6864728236859889 ) ) ;
#31452 =( NAMED_UNIT ( * ) SI_UNIT ( $, .STERADIAN. ) SOLID_ANGLE_UNIT ( ) );
#31454 = AXIS2_PLACEMENT_3D ( 'NONE', #83410, #58776, #92914 ) ;
#31453 = CARTESIAN_POINT ( 'NONE',  ( 4.968825510885260144, 1508.551704408389924, 211.9229860405860109 ) ) ;
#31455 = B_SPLINE_CURVE_WITH_KNOTS ( 'NONE', 5,
 ( #83775, #73746, #107870, #13791, #99456, #39002, #73179, #107323, #47975 ),
 .UNSPECIFIED., .F., .F.,
 ( 6, 3, 6 ),
 ( 0.000000000000000000, 0.5000000000000000000, 1.000000000000000000 ),
 .UNSPECIFIED. ) ;
#31456 = CARTESIAN_POINT ( 'NONE',  ( -40.01879385046350279, 1441.795747474259997, 136.9110126192350094 ) ) ;
#31457 = ORIENTED_EDGE ( 'NONE', *, *, #47425, .F. ) ;
#31458 = CARTESIAN_POINT ( 'NONE',  ( 18.32583792955789903, 1473.764139442630039, 194.8973871065419985 ) ) ;
#31459 = CARTESIAN_POINT ( 'NONE',  ( 1.396945595908719806, 1473.097535771269804, 219.2356281669150064 ) ) ;
#31460 = ORIENTED_EDGE ( 'NONE', *, *, #50753, .F. ) ;
#31461 = VERTEX_POINT ( 'NONE', #5720 ) ;
#31462 = CARTESIAN_POINT ( 'NONE',  ( 9.609922565670512284, 1410.623556455364223, 229.9593671579381464 ) ) ;
#31463 = CARTESIAN_POINT ( 'NONE',  ( 10.48842339441639915, 1452.980979821939854, 210.6446836343209839 ) ) ;
#31464 = CARTESIAN_POINT ( 'NONE',  ( 0.1257759720830000094, 1452.989722137430135, 183.2438651275979851 ) ) ;
#31465 = CARTESIAN_POINT ( 'NONE',  ( -15.31790971930000111, 1507.704306114589826, 209.3792549816630242 ) ) ;
#31466 = CARTESIAN_POINT ( 'NONE',  ( -2.836810703500213027, 1368.016923498806364, 210.6218459617142003 ) ) ;
#31467 = CARTESIAN_POINT ( 'NONE',  ( -28.25086642335310216, 1508.135711581739997, 208.8579954535609886 ) ) ;
#31468 = CARTESIAN_POINT ( 'NONE',  ( 38.81202642569470385, 1436.797832264049930, 135.0591075470150031 ) ) ;
#31469 = CARTESIAN_POINT ( 'NONE',  ( 6.942384827123173174, 1507.551704408389924, 200.9625026564361292 ) ) ;
#31470 = CARTESIAN_POINT ( 'NONE',  ( 30.15585515321759758, 1524.425415513990174, 222.4071264889503254 ) ) ;
#31471 = DIRECTION ( 'NONE',  ( 0.2054769195713296581, 0.000000000000000000, -0.9786619618251632957 ) ) ;
#31472 = CARTESIAN_POINT ( 'NONE',  ( -84.62715972491490390, 1384.816154433129896, 288.3829489245200079 ) ) ;
#31473 = EDGE_LOOP ( 'NONE', ( #28780, #91404, #94951, #24964 ) ) ;
#31474 = CARTESIAN_POINT ( 'NONE',  ( -2.291676311554999845, 1516.534976163889951, 201.8006522243570089 ) ) ;
#31475 = CARTESIAN_POINT ( 'NONE',  ( 6.938478784765000462, 1516.719999691880048, 208.3679751968140010 ) ) ;
#31476 = VERTEX_POINT ( 'NONE', #54499 ) ;
#31477 = CARTESIAN_POINT ( 'NONE',  ( 41.10790882195649942, 1440.913060387330006, 268.6213595677239709 ) ) ;
#31478 = CARTESIAN_POINT ( 'NONE',  ( -0.002351591770409689267, 1451.792435456469320, 154.0463020581492515 ) ) ;
#31479 = ORIENTED_EDGE ( 'NONE', *, *, #36006, .T. ) ;
#31480 = LINE ( 'NONE', #99778, #17707 ) ;
#31481 = CARTESIAN_POINT ( 'NONE',  ( -16.40416249119999748, 1409.987717225529877, 191.8167551617980280 ) ) ;
#31482 = DIRECTION ( 'NONE',  ( 0.000000000000000000, 0.000000000000000000, 1.000000000000000000 ) ) ;
#31483 = CARTESIAN_POINT ( 'NONE',  ( 23.55087631299999984, 1411.110694763729953, 207.7642880164279973 ) ) ;
#31484 = CARTESIAN_POINT ( 'NONE',  ( -4.363122395629999595, 1421.971318393930005, 184.5104903241980026 ) ) ;
#31485 = LINE ( 'NONE', #99783, #40578 ) ;
#31486 = CARTESIAN_POINT ( 'NONE',  ( 31.50789225850000008, 1415.566663160229837, 266.5723572024979831 ) ) ;
#31487 = CARTESIAN_POINT ( 'NONE',  ( -12.40455451760000116, 1434.419853495040115, 146.4343135272980021 ) ) ;
#31489 = EDGE_CURVE ( 'NONE', #42444, #63875, #38751, .T. ) ;
#31488 = CARTESIAN_POINT ( 'NONE',  ( -4.987078454525000204, 1509.051704408389924, 209.1727295022979831 ) ) ;
#31491 = CARTESIAN_POINT ( 'NONE',  ( -11.60004869886986789, 1424.304888195492822, 137.2804668087435118 ) ) ;
#31490 = CARTESIAN_POINT ( 'NONE',  ( 16.26126431490000002, 1459.229823316930151, 230.3673621847979973 ) ) ;
#31492 = CARTESIAN_POINT ( 'NONE',  ( -4.363122561674769528, 1421.971318449149976, 184.5104913919989826 ) ) ;
#31493 = CARTESIAN_POINT ( 'NONE',  ( -5.004475612664999851, 1517.026025493960105, 216.8437538584669824 ) ) ;
#31494 = ORIENTED_EDGE ( 'NONE', *, *, #87635, .F. ) ;
#31495 = CARTESIAN_POINT ( 'NONE',  ( -9.972208786350000409, 1449.536236232390138, 205.8362451147190200 ) ) ;
#31496 = CARTESIAN_POINT ( 'NONE',  ( -10.13268345264436476, 1480.912692742363561, 206.1544537871127432 ) ) ;
#31497 = AXIS2_PLACEMENT_3D ( 'NONE', #90971, #38905, #57410 ) ;
#31498 = CARTESIAN_POINT ( 'NONE',  ( 18.29465319566073234, 1446.505244253307637, 215.9117699586604999 ) ) ;
#31499 = CARTESIAN_POINT ( 'NONE',  ( 5.785582913545000316, 1516.981965530290154, 213.1542438721070027 ) ) ;
#31500 = CARTESIAN_POINT ( 'NONE',  ( 18.59438456350000024, 1507.626747898329995, 188.5297968183980117 ) ) ;
#31501 = CARTESIAN_POINT ( 'NONE',  ( -11.44980511867515993, 1425.806253551034388, 139.0985862314396684 ) ) ;
#31503 = EDGE_LOOP ( 'NONE', ( #23588, #76729 ) ) ;
#31502 = CARTESIAN_POINT ( 'NONE',  ( -11.36293846883789804, 1500.786239116730030, 211.0742332070699945 ) ) ;
#31504 = CARTESIAN_POINT ( 'NONE',  ( -19.59880086690000311, 1507.802454088529885, 229.4381582326980151 ) ) ;
#31505 = CARTESIAN_POINT ( 'NONE',  ( 3.410547590470000223, 1507.830663321090015, 220.3411986762989727 ) ) ;
#31506 = CARTESIAN_POINT ( 'NONE',  ( -10.95785036490000053, 1431.503689836019930, 151.7245498010980214 ) ) ;
#31507 = CARTESIAN_POINT ( 'NONE',  ( 19.02764298761669792, 1456.917174445179853, 225.6166628802600087 ) ) ;
#31508 = CARTESIAN_POINT ( 'NONE',  ( -109.6125588903939985, 1383.187010251420133, 311.2171431170959863 ) ) ;
#31509 = CARTESIAN_POINT ( 'NONE',  ( 11.78818150890059968, 1426.417842412089840, 148.5075604377779825 ) ) ;
#31510 = CARTESIAN_POINT ( 'NONE',  ( -21.97938480444670262, 1506.433683733529961, 209.5040264213440082 ) ) ;
#31511 = FACE_OUTER_BOUND ( 'NONE', #52943, .T. ) ;
#31513 = CARTESIAN_POINT ( 'NONE',  ( -2.685939447044066952, 1419.763153556473526, 137.0999999980978430 ) ) ;
#31512 = CARTESIAN_POINT ( 'NONE',  ( -23.96120601207324796, 1411.110625406946610, 208.0854022759841655 ) ) ;
#31514 = CARTESIAN_POINT ( 'NONE',  ( -3.002432322850000279, 1486.001776092530008, 182.1376723879980091 ) ) ;
#31515 = ORIENTED_EDGE ( 'NONE', *, *, #100121, .T. ) ;
#31516 = CARTESIAN_POINT ( 'NONE',  ( -2.879642191334999879, 1516.812046502680005, 205.6755161564470313 ) ) ;
#31517 = CARTESIAN_POINT ( 'NONE',  ( 12.72718513819999941, 1407.064594780429843, 267.4694263162979837 ) ) ;
#31518 = FACE_OUTER_BOUND ( 'NONE', #60292, .T. ) ;
#31520 = B_SPLINE_CURVE_WITH_KNOTS ( 'NONE', 3,
 ( #5082, #56605, #39233, #30833, #82893, #99125, #100252, #99675, #22404, #90741 ),
 .UNSPECIFIED., .F., .F.,
 ( 4, 2, 2, 2, 4 ),
 ( 1.734723475976807094E-17, 0.0007406479101619456874, 0.001481295820323874027, 0.002221943730485802584, 0.002962591640647730708 ),
 .UNSPECIFIED. ) ;
#31519 = CARTESIAN_POINT ( 'NONE',  ( 17.57165883560000097, 1410.882996087329957, 192.7623837702980154 ) ) ;
#31521 = COLOUR_RGB ( '', 0.66274510, 0.83137255, 0.94901961) ;
#31522 = EDGE_CURVE ( 'NONE', #43603, #4789, #86152, .T. ) ;
#31523 = CARTESIAN_POINT ( 'NONE',  ( 23.14416256224673063, 1432.663507748254688, 215.7929284277614954 ) ) ;
#31524 = EDGE_CURVE ( 'NONE', #14678, #105869, #35385, .T. ) ;
#31525 = CARTESIAN_POINT ( 'NONE',  ( -24.86308739729999928, 1452.044818012130236, 135.5986755553979890 ) ) ;
#31526 = CARTESIAN_POINT ( 'NONE',  ( 27.93978865640000109, 1508.083000434530049, 211.1815961025180286 ) ) ;
#31527 = EDGE_CURVE ( 'NONE', #82581, #37235, #52685, .T. ) ;
#31528 = DIRECTION ( 'NONE',  ( 0.000000000000000000, -1.000000000000000000, 1.836970198721029688E-16 ) ) ;
#31529 = FACE_BOUND ( 'NONE', #61079, .T. ) ;
#31530 = CARTESIAN_POINT ( 'NONE',  ( -12.19576017219999997, 1445.284187945309895, 186.5171125204979887 ) ) ;
#31531 = EDGE_CURVE ( 'NONE', #39742, #106739, #109585, .T. ) ;
#31532 = CARTESIAN_POINT ( 'NONE',  ( -19.74181951150670500, 1486.027887478371213, 190.1836019666429820 ) ) ;
#31533 = EDGE_CURVE ( 'NONE', #37815, #54528, #99416, .T. ) ;
#31534 = CARTESIAN_POINT ( 'NONE',  ( -105.9134739529999933, 1391.838461175369957, 304.2044424958581885 ) ) ;
#31535 = CARTESIAN_POINT ( 'NONE',  ( -11.17096468969999812, 1500.478073591689963, 215.5530715242690007 ) ) ;
#31536 = CARTESIAN_POINT ( 'NONE',  ( -7.121584071090000023, 1409.161751583130126, 195.9581075130980139 ) ) ;
#31537 = CARTESIAN_POINT ( 'NONE',  ( 20.31245888920532394, 1507.850143714011892, 228.7302838063898207 ) ) ;
#31538 = CARTESIAN_POINT ( 'NONE',  ( 4.219804471239999799, 1441.618635230429845, 168.7222761371980084 ) ) ;
#31539 = CARTESIAN_POINT ( 'NONE',  ( -3.776688141959999800, 1475.993142067930194, 267.8478539070980560 ) ) ;
#31540 = FACE_OUTER_BOUND ( 'NONE', #101953, .T. ) ;
#31541 = CARTESIAN_POINT ( 'NONE',  ( -9.096596473720000020, 1440.282624608189963, 206.1069770705490214 ) ) ;
#31542 = CARTESIAN_POINT ( 'NONE',  ( -9.324653930165572646, 1486.515044582724386, 183.2464455839941593 ) ) ;
#31543 = CARTESIAN_POINT ( 'NONE',  ( -59.96123856990180201, 1384.695927338900219, 280.8926189855779967 ) ) ;
#31544 = CARTESIAN_POINT ( 'NONE',  ( 1.457628745286551286, 1507.679360684215908, 236.7889182220722546 ) ) ;
#31545 = CARTESIAN_POINT ( 'NONE',  ( -4.277761497305760940, 1517.051704409989952, 216.4479871024050226 ) ) ;
#31546 = CARTESIAN_POINT ( 'NONE',  ( -45.67177343128329881, 1440.913044206929953, 266.1885934837860077 ) ) ;
#31547 = CARTESIAN_POINT ( 'NONE',  ( 32.21030510514599143, 1524.412455883367329, 216.0988835363537817 ) ) ;
#31548 = CARTESIAN_POINT ( 'NONE',  ( 8.501597980927209974, 1511.397677006128788, 204.1858220046408974 ) ) ;
#31549 = FACE_OUTER_BOUND ( 'NONE', #9325, .T. ) ;
#31550 = EDGE_CURVE ( 'NONE', #59085, #98070, #46136, .T. ) ;
#31551 = CARTESIAN_POINT ( 'NONE',  ( 12.69964242394170029, 1421.449485046359996, 206.4738677144460155 ) ) ;
#31552 = CARTESIAN_POINT ( 'NONE',  ( -25.70445440479999988, 1412.495827564830051, 269.4333631909979658 ) ) ;
#31553 = ORIENTED_EDGE ( 'NONE', *, *, #37734, .T. ) ;
#31554 = CARTESIAN_POINT ( 'NONE',  ( -7.554020802055777750, 1410.549877764319717, 230.8257970151002780 ) ) ;
#31556 = ADVANCED_FACE ( 'NONE', ( #33144 ), #34830, .T. ) ;
#31555 = CARTESIAN_POINT ( 'NONE',  ( -13.59314176670009999, 1508.069786739810070, 209.4864804417960329 ) ) ;
#31557 = CARTESIAN_POINT ( 'NONE',  ( -19.86622908376359931, 1443.388396254009876, 213.1207183147250248 ) ) ;
#31559 = CARTESIAN_POINT ( 'NONE',  ( -14.01565498306790047, 1379.590400379700213, 211.9190739246080284 ) ) ;
#31558 = CARTESIAN_POINT ( 'NONE',  ( -16.56054082451800014, 1417.106265379630031, 208.4979211302300257 ) ) ;
#31560 = CARTESIAN_POINT ( 'NONE',  ( 16.55384015339962289, 1524.739915903632209, 237.4556660764005471 ) ) ;
#31561 = CARTESIAN_POINT ( 'NONE',  ( 1.204096590079999967E-15, 1406.443991414029824, 146.1721969590979882 ) ) ;
#31562 = B_SPLINE_CURVE_WITH_KNOTS ( 'NONE', 3,
 ( #42709, #100931, #109371, #77413, #17464, #32649, #58413, #75761, #66826, #94758 ),
 .UNSPECIFIED., .F., .F.,
 ( 4, 2, 2, 2, 4 ),
 ( 3.469446951953614189E-18, 0.0007403986298595326620, 0.001480797259719061855, 0.002221195889578590939, 0.002961594519438120240 ),
 .UNSPECIFIED. ) ;
#31563 = EDGE_CURVE ( 'NONE', #52385, #94751, #17894, .T. ) ;
#31564 = CARTESIAN_POINT ( 'NONE',  ( -4.222077288720000432, 1454.203574068490298, 200.3246332720389944 ) ) ;
#31565 = CARTESIAN_POINT ( 'NONE',  ( 6.940473334145000450, 1516.833525648419936, 202.5658237375970145 ) ) ;
#31566 = CARTESIAN_POINT ( 'NONE',  ( 8.413970532630001387, 1428.089005924990033, 212.8939830477889927 ) ) ;
#31567 = CARTESIAN_POINT ( 'NONE',  ( -2.416798835000000256, 1426.601114010129777, 146.0361887655980127 ) ) ;
#31568 = CARTESIAN_POINT ( 'NONE',  ( 16.44381310503499805, 1512.620989416239809, 195.6052243943669851 ) ) ;
#31569 = CARTESIAN_POINT ( 'NONE',  ( -21.78529113934020245, 1417.868803632889922, 208.5446529662619923 ) ) ;
#31570 = CARTESIAN_POINT ( 'NONE',  ( 8.335345713666398798E-14, 1380.413060386289999, 209.1217751689949864 ) ) ;
#31571 = CARTESIAN_POINT ( 'NONE',  ( 22.22116651786569719, 1509.699978059410114, 228.6323576840410112 ) ) ;
#31573 = VERTEX_POINT ( 'NONE', #74624 ) ;
#31572 = CARTESIAN_POINT ( 'NONE',  ( -17.14950101167192642, 1517.051704408390151, 195.3930630967549007 ) ) ;
#31574 = VERTEX_POINT ( 'NONE', #108203 ) ;
#31575 = CARTESIAN_POINT ( 'NONE',  ( -10.84028228440000063, 1397.329407496930116, 216.7606694918979713 ) ) ;
#31576 = CARTESIAN_POINT ( 'NONE',  ( -21.06868771289999742, 1409.648795181130026, 214.7337414265580264 ) ) ;
#31577 = ORIENTED_EDGE ( 'NONE', *, *, #28913, .T. ) ;
#31578 = CARTESIAN_POINT ( 'NONE',  ( -7.075873090581220301E-12, 1395.913060387330006, 220.1216245177919859 ) ) ;
#31579 = DIRECTION ( 'NONE',  ( 0.9076061524720596685, 1.962993793439040551E-32, -0.4198226673190293412 ) ) ;
#31580 = CARTESIAN_POINT ( 'NONE',  ( -7.691516692145000000, 1512.326491219019999, 211.8199587616570057 ) ) ;
#31582 = CARTESIAN_POINT ( 'NONE',  ( -13.77385084366710011, 1508.394378971780043, 184.0922798201980299 ) ) ;
#31581 = CARTESIAN_POINT ( 'NONE',  ( 0.7910245917146940808, 1426.918876941764893, 137.0999999980980135 ) ) ;
#31583 = CARTESIAN_POINT ( 'NONE',  ( 3.798153425019999752, 1449.235780910159974, 184.2153987367980221 ) ) ;
#31584 = CARTESIAN_POINT ( 'NONE',  ( -4.776356492423380118, 1463.978274100160206, 200.0897609657779981 ) ) ;
#31585 = CARTESIAN_POINT ( 'NONE',  ( 4.576312612474012553, 1517.051704408389924, 195.8593501239998318 ) ) ;
#31586 =( LENGTH_UNIT ( ) NAMED_UNIT ( * ) SI_UNIT ( .MILLI., .METRE. ) );
#31587 = CARTESIAN_POINT ( 'NONE',  ( 8.082860218267720498, 1396.195320171349977, 201.5809466256010012 ) ) ;
#31588 = CARTESIAN_POINT ( 'NONE',  ( 1.309033247469999717, 1415.245980412430072, 191.0747513254979992 ) ) ;
#31589 = CARTESIAN_POINT ( 'NONE',  ( 11.66762902670000024, 1426.112960980830167, 146.5933604607980101 ) ) ;
#31590 = CARTESIAN_POINT ( 'NONE',  ( 8.111736945090072481, 1509.196641154956069, 180.9310382456955608 ) ) ;
#31591 = VERTEX_POINT ( 'NONE', #5197 ) ;
#31592 = CARTESIAN_POINT ( 'NONE',  ( 12.84231544366310018, 1435.935755016759913, 150.8115345589289973 ) ) ;
#31593 = CARTESIAN_POINT ( 'NONE',  ( 1.525930004160000131, 1471.299568758030091, 187.8082942405980020 ) ) ;
#31594 = ORIENTED_EDGE ( 'NONE', *, *, #2736, .T. ) ;
#31595 = EDGE_LOOP ( 'NONE', ( #12315, #102117, #56238, #26889, #101646, #72515, #58033 ) ) ;
#31596 = CARTESIAN_POINT ( 'NONE',  ( -18.72409591074379875, 1458.246134293049863, 227.3156199550079748 ) ) ;
#31597 = CARTESIAN_POINT ( 'NONE',  ( 21.05586012649999716, 1495.072013869990087, 210.1549089269589956 ) ) ;
#31598 = CARTESIAN_POINT ( 'NONE',  ( -109.5723520410060843, 1386.720847671712136, 311.1928145605723444 ) ) ;
#31599 = CARTESIAN_POINT ( 'NONE',  ( 6.942973629204999497, 1516.833844030519913, 216.4505221401170161 ) ) ;
#31600 = CARTESIAN_POINT ( 'NONE',  ( -13.20215179197749933, 1379.610106626019842, 208.3537467556710112 ) ) ;
#31601 = PRODUCT_DEFINITION ( 'UNKNOWN', '', #86976, #96107 ) ;
#31602 = VERTEX_POINT ( 'NONE', #91954 ) ;
#31603 = CARTESIAN_POINT ( 'NONE',  ( -11.32042714269999983, 1502.674858046290183, 207.0911706105389953 ) ) ;
#31604 = CARTESIAN_POINT ( 'NONE',  ( -1.799807112810000165, 1414.009329215630032, 185.8866739651980140 ) ) ;
#31605 = CARTESIAN_POINT ( 'NONE',  ( -60.40574806380000439, 1377.395658627419834, 258.0520616922589738 ) ) ;
#31606 = ORIENTED_EDGE ( 'NONE', *, *, #110417, .T. ) ;
#31607 = CARTESIAN_POINT ( 'NONE',  ( -2.492443689034999910, 1516.793978928989873, 205.8699571027569846 ) ) ;
#31608 = ORIENTED_EDGE ( 'NONE', *, *, #35189, .F. ) ;
#31609 = CARTESIAN_POINT ( 'NONE',  ( 6.556850996575000146, 1516.939568781210028, 209.1101343261499892 ) ) ;
#31610 = B_SPLINE_CURVE_WITH_KNOTS ( 'NONE', 5,
 ( #21783, #22335, #13946, #65495, #99604, #22887, #45933, #71722, #105839 ),
 .UNSPECIFIED., .F., .F.,
 ( 6, 3, 6 ),
 ( 0.000000000000000000, 0.5000000000000000000, 1.000000000000000000 ),
 .UNSPECIFIED. ) ;
#31611 = CARTESIAN_POINT ( 'NONE',  ( -7.721313575298860421, 1452.995439927550024, 203.8751428730399766 ) ) ;
#31612 = CARTESIAN_POINT ( 'NONE',  ( -33.74130636077602929, 1422.741317463423002, 269.5146518279480006 ) ) ;
#31613 = CARTESIAN_POINT ( 'NONE',  ( 6.580362910585000336, 1511.382498894339733, 216.4385679756969978 ) ) ;
#31615 = VERTEX_POINT ( 'NONE', #5763 ) ;
#31614 = CARTESIAN_POINT ( 'NONE',  ( -0.2612772523530000335, 1416.851343897030119, 227.4677504995979973 ) ) ;
#31616 = CARTESIAN_POINT ( 'NONE',  ( -0.01306239367006429945, 1452.951700076570205, 183.2402720810920016 ) ) ;
#31617 = CARTESIAN_POINT ( 'NONE',  ( -33.94015795350929920, 1440.913060389670136, 248.7268766980600105 ) ) ;
#31618 = CARTESIAN_POINT ( 'NONE',  ( -27.62991514189999975, 1384.504118323729926, 225.6271822822590138 ) ) ;
#31620 = ADVANCED_FACE ( 'NONE', ( #56714 ), #101431, .F. ) ;
#31619 = CARTESIAN_POINT ( 'NONE',  ( -0.2432179624465790058, 1465.024700022039951, 237.7670363050069682 ) ) ;
#31621 = EDGE_CURVE ( 'NONE', #30027, #76210, #14134, .T. ) ;
#31622 = CARTESIAN_POINT ( 'NONE',  ( 4.986174232479999802, 1408.440924972429912, 270.3887730021980360 ) ) ;
#31623 = CARTESIAN_POINT ( 'NONE',  ( -1.121383629864999953, 1517.104192383289956, 213.7476359466970166 ) ) ;
#31624 = CARTESIAN_POINT ( 'NONE',  ( 23.98088334710000069, 1410.978996304829934, 208.3903162892720218 ) ) ;
#31625 = LINE ( 'NONE', #40583, #69686 ) ;
#31626 = CARTESIAN_POINT ( 'NONE',  ( 12.19154428201109930, 1492.561849750740066, 211.0960655454310029 ) ) ;
#31627 = CARTESIAN_POINT ( 'NONE',  ( -7.708942735038510463, 1516.530904812869949, 211.0733318003030092 ) ) ;
#31628 = CARTESIAN_POINT ( 'NONE',  ( -1.701850495234999983, 1516.908147884120126, 210.2591426210370003 ) ) ;
#31629 = DIRECTION ( 'NONE',  ( -1.755985294532469921E-16, 1.000000000000000000, -1.338183447452831989E-16 ) ) ;
#31630 = CARTESIAN_POINT ( 'NONE',  ( 0.09078858057499999967, 1420.445484879229980, 183.3263106172979917 ) ) ;
#31631 = CARTESIAN_POINT ( 'NONE',  ( -2.640434834157888933, 1526.748660780343471, 176.9315852594522482 ) ) ;
#31633 = ORIENTED_EDGE ( 'NONE', *, *, #34980, .T. ) ;
#31632 = CARTESIAN_POINT ( 'NONE',  ( -27.63867464639999838, 1385.244481134689977, 225.6178332698589770 ) ) ;
#31634 = CARTESIAN_POINT ( 'NONE',  ( -54.74390983765479746, 1385.094081698930040, 271.3100142828129719 ) ) ;
#31635 = ADVANCED_FACE ( 'NONE', ( #93050 ), #15763, .F. ) ;
#31636 = CARTESIAN_POINT ( 'NONE',  ( 31.34137657907978891, 1523.481610118013123, 196.3411265156827596 ) ) ;
#31637 = DIRECTION ( 'NONE',  ( 1.755985294532464991E-16, -1.000000000000000000, 1.338183447452830017E-16 ) ) ;
#31638 = VECTOR ( 'NONE', #39637, 1000.000000000000000 ) ;
#31639 = CARTESIAN_POINT ( 'NONE',  ( -8.991795041622840046, 1509.227063482730046, 237.0095535837990326 ) ) ;
#31640 = CARTESIAN_POINT ( 'NONE',  ( 7.243833416339904296, 1473.411017056090031, 218.0151120354588556 ) ) ;
#31641 = CARTESIAN_POINT ( 'NONE',  ( 11.97204719289999986, 1426.674835027849895, 205.8341005045690224 ) ) ;
#31642 = CARTESIAN_POINT ( 'NONE',  ( -3.617573937782270210, 1497.333809982809953, 198.4503636364750037 ) ) ;
#31644 = DIRECTION ( 'NONE',  ( -0.9993779842017727066, -0.0009463033499147846571, -0.03525264816679202218 ) ) ;
#31643 = CARTESIAN_POINT ( 'NONE',  ( 2.291676273424999799, 1516.534976163889951, 216.4430396779769978 ) ) ;
#31645 = CARTESIAN_POINT ( 'NONE',  ( -2.664535259099999805E-15, 1422.937291763169924, 209.1218459616989946 ) ) ;
#31646 = CARTESIAN_POINT ( 'NONE',  ( 30.51126001304326252, 1526.382868172863937, 219.8557927178086970 ) ) ;
#31647 = ORIENTED_EDGE ( 'NONE', *, *, #3941, .F. ) ;
#31648 = CARTESIAN_POINT ( 'NONE',  ( 3.452917022905000355, 1517.089216728169959, 202.1725802860869976 ) ) ;
#31649 = CARTESIAN_POINT ( 'NONE',  ( 28.32265147467229838, 1509.673549449270013, 207.2611521541350044 ) ) ;
#31650 = CARTESIAN_POINT ( 'NONE',  ( 0.3785491535969999766, 1487.217178801030059, 230.2600272812980222 ) ) ;
#31651 = VECTOR ( 'NONE', #18580, 1000.000000000000000 ) ;
#31652 = EDGE_CURVE ( 'NONE', #76248, #40736, #106348, .T. ) ;
#31653 = CARTESIAN_POINT ( 'NONE',  ( -17.17241001986523941, 1512.187213306747481, 179.6185504016045797 ) ) ;
#31654 = CARTESIAN_POINT ( 'NONE',  ( 10.83576136632169984, 1461.764785210480113, 210.8453021311209739 ) ) ;
#31655 = CARTESIAN_POINT ( 'NONE',  ( 9.169705329756888901, 1425.158430046457852, 195.6334031360315748 ) ) ;
#31656 = CARTESIAN_POINT ( 'NONE',  ( 4.438328147020000003, 1466.438991376089916, 218.4230750687189868 ) ) ;
#31657 = CARTESIAN_POINT ( 'NONE',  ( 14.16828006819016395, 1420.021719220239902, 228.3966679742590031 ) ) ;
#31658 = EDGE_CURVE ( 'NONE', #21410, #101374, #24180, .T. ) ;
#31659 = CARTESIAN_POINT ( 'NONE',  ( 38.88267750156879998, 1447.890902847689858, 136.5100495134630023 ) ) ;
#31660 = CARTESIAN_POINT ( 'NONE',  ( -18.93172946400000356, 1424.841178919430149, 224.3420561942980100 ) ) ;
#31661 = CARTESIAN_POINT ( 'NONE',  ( 8.305536275772812616, 1487.549204498889594, 202.1547115178333058 ) ) ;
#31662 = CARTESIAN_POINT ( 'NONE',  ( -108.9824555929999974, 1388.007023282849786, 297.6230262977589973 ) ) ;
#31663 = CARTESIAN_POINT ( 'NONE',  ( 7.889195814119081440, 1372.293237941190000, 213.4317332778174716 ) ) ;
#31664 = CARTESIAN_POINT ( 'NONE',  ( -106.3970662050000016, 1391.913060387289988, 303.5338388646590033 ) ) ;
#31665 = CARTESIAN_POINT ( 'NONE',  ( -15.60993031491385707, 1469.237360295198414, 269.3672923534541042 ) ) ;
#31666 = ORIENTED_EDGE ( 'NONE', *, *, #54207, .F. ) ;
#31667 = CARTESIAN_POINT ( 'NONE',  ( -8.039518803556870097, 1439.999387722500160, 205.2469398296260010 ) ) ;
#31668 = CARTESIAN_POINT ( 'NONE',  ( 11.11083760155161748, 1506.426094404281002, 190.1501388411886637 ) ) ;
#31669 = EDGE_CURVE ( 'NONE', #17250, #43307, #103375, .T. ) ;
#31670 = CARTESIAN_POINT ( 'NONE',  ( 11.21799561054379879, 1470.401428587849978, 207.2916120790159766 ) ) ;
#31671 = CARTESIAN_POINT ( 'NONE',  ( -9.202936508599998788, 1519.913060387329779, 230.3262217860979888 ) ) ;
#31672 = CARTESIAN_POINT ( 'NONE',  ( 1.317811661047101346, 1522.051704408389924, 223.5300434977941677 ) ) ;
#31673 = CARTESIAN_POINT ( 'NONE',  ( -12.99496264364580256, 1442.946651945849453, 186.5341436481298274 ) ) ;
#31674 = CARTESIAN_POINT ( 'NONE',  ( -16.66936639845670598, 1523.382868172864164, 180.4828114240741854 ) ) ;
#31675 = CARTESIAN_POINT ( 'NONE',  ( -3.586360116007019982, 1515.071395204220153, 213.2046256369000048 ) ) ;
#31676 = EDGE_CURVE ( 'NONE', #76166, #86228, #26035, .T. ) ;
#31677 = DIRECTION ( 'NONE',  ( 0.000000000000000000, 0.000000000000000000, -1.000000000000000000 ) ) ;
#31678 = CARTESIAN_POINT ( 'NONE',  ( -14.69797768358330003, 1415.677402203350084, 206.1947793185709941 ) ) ;
#31679 = CARTESIAN_POINT ( 'NONE',  ( -7.105427357599999217E-15, 1405.913060387330006, 137.0999999980979851 ) ) ;
#31680 = CARTESIAN_POINT ( 'NONE',  ( -13.06317481566171068, 1442.994605609547762, 169.4117022543989890 ) ) ;
#31682 = ORIENTED_EDGE ( 'NONE', *, *, #86900, .T. ) ;
#31681 = CARTESIAN_POINT ( 'NONE',  ( 31.44837959398592986, 1511.187213306747708, 220.9083067115976462 ) ) ;
#31683 = CARTESIAN_POINT ( 'NONE',  ( 0.2112786387551819911, 1416.230844595159851, 190.9402219459099967 ) ) ;
#31684 = CARTESIAN_POINT ( 'NONE',  ( 21.83810631170608474, 1509.467311289125064, 226.7543823560263547 ) ) ;
#31685 = ORIENTED_EDGE ( 'NONE', *, *, #107727, .F. ) ;
#31686 = ORIENTED_EDGE ( 'NONE', *, *, #67288, .T. ) ;
#31687 = CARTESIAN_POINT ( 'NONE',  ( 18.02416168173120070, 1416.221314539589912, 209.0673659498179973 ) ) ;
#31688 = CARTESIAN_POINT ( 'NONE',  ( 9.717824533310780666, 1463.678478211699939, 210.3770741684630252 ) ) ;
#31690 = CARTESIAN_POINT ( 'NONE',  ( -25.95416491200000308, 1449.827894582669842, 231.7292227871980117 ) ) ;
#31689 = CARTESIAN_POINT ( 'NONE',  ( 3.845501273690000055, 1455.043435614390091, 217.8764266887590111 ) ) ;
#31691 = CARTESIAN_POINT ( 'NONE',  ( -2.540028566810000221, 1444.571278203389966, 217.8835225073589754 ) ) ;
#31692 = EDGE_CURVE ( 'NONE', #49707, #29992, #33690, .T. ) ;
#31693 = CARTESIAN_POINT ( 'NONE',  ( -11.29872328070000087, 1433.512132546310113, 151.5043843572979938 ) ) ;
#31694 = CARTESIAN_POINT ( 'NONE',  ( 15.20279577643499991, 1516.814170398969964, 225.0317485278669949 ) ) ;
#31695 = AXIS2_PLACEMENT_3D ( 'NONE', #36886, #62685, #17849 ) ;
#31696 = CARTESIAN_POINT ( 'NONE',  ( 16.63506016420000222, 1409.493969489730034, 224.1775087685979884 ) ) ;
#31697 = CARTESIAN_POINT ( 'NONE',  ( -26.28587293000000003, 1436.455679608809987, 136.7639433163979845 ) ) ;
#31699 = EDGE_CURVE ( 'NONE', #82014, #106524, #94065, .T. ) ;
#31698 = CARTESIAN_POINT ( 'NONE',  ( -12.00387303569999986, 1415.296882282229944, 195.7718046162979704 ) ) ;
#31700 = FACE_BOUND ( 'NONE', #72519, .T. ) ;
#31701 = CARTESIAN_POINT ( 'NONE',  ( 2.389941574139999858, 1450.533795919260001, 183.3353223396979956 ) ) ;
#31702 = CARTESIAN_POINT ( 'NONE',  ( 8.396902068309636036, 1363.743897584764454, 207.6218459616988241 ) ) ;
#31703 = CARTESIAN_POINT ( 'NONE',  ( -29.02628104977890189, 1509.926680457060002, 211.9910930732060024 ) ) ;
#31705 = VERTEX_POINT ( 'NONE', #53286 ) ;
#31704 = CARTESIAN_POINT ( 'NONE',  ( -4.244249385787189894E-10, 1412.540523501239932, 252.0669699321499877 ) ) ;
#31706 = ORIENTED_EDGE ( 'NONE', *, *, #63184, .F. ) ;
#31707 = CARTESIAN_POINT ( 'NONE',  ( -11.78952479729490044, 1427.771338190059851, 147.6174756818780054 ) ) ;
#31708 = CARTESIAN_POINT ( 'NONE',  ( 16.43010731360000065, 1495.465599852389914, 192.8750426889990024 ) ) ;
#31709 = CARTESIAN_POINT ( 'NONE',  ( -3.549205704360000269, 1473.795584311630137, 270.2903253923980174 ) ) ;
#31710 = CYLINDRICAL_SURFACE ( 'NONE', #10467, 29.99999999999999645 ) ;
#31711 = FACE_OUTER_BOUND ( 'NONE', #80783, .T. ) ;
#31712 = CARTESIAN_POINT ( 'NONE',  ( -13.60685608969999905, 1452.409494112630000, 223.2534408495980074 ) ) ;
#31713 = CARTESIAN_POINT ( 'NONE',  ( -7.075873090581220301E-12, 1395.913060387330006, 220.1216245177919859 ) ) ;
#31714 = CARTESIAN_POINT ( 'NONE',  ( 18.72022026493218405, 1457.160368941672687, 229.5334714930285713 ) ) ;
#31715 = DIRECTION ( 'NONE',  ( -0.04471266514373050532, 0.9989992949979481507, -0.001089114019438660068 ) ) ;
#31716 = CARTESIAN_POINT ( 'NONE',  ( -4.394233624539999994, 1456.808182323690062, 217.5515244654889955 ) ) ;
#31717 = CARTESIAN_POINT ( 'NONE',  ( 11.34530601785825965, 1366.910327255101038, 208.3718459617010978 ) ) ;
#31718 = CARTESIAN_POINT ( 'NONE',  ( -37.07982229246980665, 1420.640666704749947, 269.2047045636169855 ) ) ;
#31719 = ORIENTED_EDGE ( 'NONE', *, *, #36631, .F. ) ;
#31720 = CARTESIAN_POINT ( 'NONE',  ( -4.328845283827259749, 1515.087839320550074, 210.3999710242079857 ) ) ;
#31721 = EDGE_LOOP ( 'NONE', ( #96687, #56856, #40829, #5448 ) ) ;
#31722 = AXIS2_PLACEMENT_3D ( 'NONE', #109887, #25854, #102015 ) ;
#31723 = ORIENTED_EDGE ( 'NONE', *, *, #78146, .T. ) ;
#31724 = CARTESIAN_POINT ( 'NONE',  ( -5.771149113014999443, 1516.616791731099966, 211.6102065995370083 ) ) ;
#31725 = CARTESIAN_POINT ( 'NONE',  ( -8.650355960269319411, 1448.128899224820088, 212.2110593161760050 ) ) ;
#31726 = CARTESIAN_POINT ( 'NONE',  ( 41.16307904399219808, 1444.157581002339839, 136.7448092931550150 ) ) ;
#31728 = CARTESIAN_POINT ( 'NONE',  ( -17.64855902048280356, 1419.508594242146955, 207.1654737734966147 ) ) ;
#31727 = CARTESIAN_POINT ( 'NONE',  ( 1.714334247185000049, 1516.699825673279975, 213.1484604498870112 ) ) ;
#31729 = CARTESIAN_POINT ( 'NONE',  ( -15.85109824379999921, 1440.436905774210118, 189.7893843040980073 ) ) ;
#31730 = CIRCLE ( 'NONE', #53172, 8.500000000000000000 ) ;
#31731 = B_SPLINE_CURVE_WITH_KNOTS ( 'NONE', 3,
 ( #94865, #36075, #77521, #821, #27664, #51208 ),
 .UNSPECIFIED., .F., .F.,
 ( 4, 2, 4 ),
 ( -1.131363979550832737E-05, 0.001067788114096722158, 0.002146889867988952330 ),
 .UNSPECIFIED. ) ;
#31732 = FACE_OUTER_BOUND ( 'NONE', #94231, .T. ) ;
#31733 = EDGE_LOOP ( 'NONE', ( #23668, #12327 ) ) ;
#31734 = CARTESIAN_POINT ( 'NONE',  ( -26.47025460449999912, 1435.961592063199760, 136.4857856691980089 ) ) ;
#31735 =( BOUNDED_CURVE ( )  B_SPLINE_CURVE ( 3, ( #74446, #81699, #98511, #99052 ),
 .UNSPECIFIED., .F., .T. ) 
 B_SPLINE_CURVE_WITH_KNOTS ( ( 4, 4 ),
 ( 1.036306151091926031, 2.105316129261890268 ),
 .UNSPECIFIED. ) 
 CURVE ( )  GEOMETRIC_REPRESENTATION_ITEM ( )  RATIONAL_B_SPLINE_CURVE ( ( 1.000000000000000000, 0.9070139338303890852, 0.9070139338303890852, 1.000000000000000000 ) ) 
 REPRESENTATION_ITEM ( '' )  );
#31736 = CARTESIAN_POINT ( 'NONE',  ( 0.7391219670640019057, 1517.130100026000036, 202.1721425974470208 ) ) ;
#31737 = CARTESIAN_POINT ( 'NONE',  ( -41.65674268029999894, 1443.992461967939789, 135.6790812281979868 ) ) ;
#31738 = CARTESIAN_POINT ( 'NONE',  ( -9.638891686394590153, 1503.623617614200384, 228.8110675621960013 ) ) ;
#31739 = CARTESIAN_POINT ( 'NONE',  ( -40.40952010682039486, 1425.380211256870098, 269.9834891395850036 ) ) ;
#31740 = CARTESIAN_POINT ( 'NONE',  ( -18.66351252432520269, 1486.318487979379825, 199.8022941382239992 ) ) ;
#31741 = CARTESIAN_POINT ( 'NONE',  ( -3.851962676559999910, 1397.715880058830180, 196.6003271923979980 ) ) ;
#31743 = ORIENTED_EDGE ( 'NONE', *, *, #8213, .F. ) ;
#31742 = CARTESIAN_POINT ( 'NONE',  ( -8.001072242696793069, 1364.926390148715655, 209.6218459617148824 ) ) ;
#31744 = ORIENTED_EDGE ( 'NONE', *, *, #74348, .F. ) ;
#31745 = CARTESIAN_POINT ( 'NONE',  ( -11.86930535227000050, 1432.575968667860025, 149.9818528069360184 ) ) ;
#31746 = DIRECTION ( 'NONE',  ( 1.755985294532464991E-16, -1.000000000000000000, 1.338183447452830017E-16 ) ) ;
#31747 = CARTESIAN_POINT ( 'NONE',  ( 10.78618902296759963, 1460.496538158609837, 207.3635337098189950 ) ) ;
#31748 = ADVANCED_FACE ( 'NONE', ( #11278 ), #37007, .F. ) ;
#31749 = CARTESIAN_POINT ( 'NONE',  ( -14.53429262354389984, 1436.249209451070101, 149.9090136612170170 ) ) ;
#31750 = CARTESIAN_POINT ( 'NONE',  ( -1.202963480870000046, 1486.064486177629988, 181.8233092472979990 ) ) ;
#31751 = AXIS2_PLACEMENT_3D ( 'NONE', #10411, #2595, #45702 ) ;
#31752 = CARTESIAN_POINT ( 'NONE',  ( -0.7351098092479989576, 1516.977504706749869, 211.6135016956469883 ) ) ;
#31753 = CARTESIAN_POINT ( 'NONE',  ( -68.76896737129999337, 1379.747921602020142, 280.1883489107589753 ) ) ;
#31754 = FACE_OUTER_BOUND ( 'NONE', #88575, .T. ) ;
#31755 = CARTESIAN_POINT ( 'NONE',  ( 8.475509682807949474, 1437.831708687899891, 211.6527867693390306 ) ) ;
#31756 = CARTESIAN_POINT ( 'NONE',  ( -13.36059443979999983, 1414.988015881329829, 220.3623400978979987 ) ) ;
#31757 = CARTESIAN_POINT ( 'NONE',  ( 7.933914926335000395, 1511.279956263560052, 204.0003333914669952 ) ) ;
#31758 = CARTESIAN_POINT ( 'NONE',  ( -7.338753868364999988, 1517.184383877180153, 206.8309596656170015 ) ) ;
#31759 = EDGE_LOOP ( 'NONE', ( #38394, #64573, #89517, #14361, #17251 ) ) ;
#31760 = CARTESIAN_POINT ( 'NONE',  ( -36.37832874669039995, 1451.642701154630004, 134.4203408178500183 ) ) ;
#31761 = CARTESIAN_POINT ( 'NONE',  ( -11.31317986880000070, 1471.144533718689900, 207.5705785899590126 ) ) ;
#31762 = CARTESIAN_POINT ( 'NONE',  ( -20.19776133349999014, 1456.164861684272637, 224.8266744640568504 ) ) ;
#31763 = ORIENTED_EDGE ( 'NONE', *, *, #77661, .T. ) ;
#31764 = CARTESIAN_POINT ( 'NONE',  ( -3.350338079455601026, 1523.604703353109699, 242.0808062845893289 ) ) ;
#31765 = EDGE_CURVE ( 'NONE', #93538, #44452, #44728, .T. ) ;
#31766 = CARTESIAN_POINT ( 'NONE',  ( 12.79711581523170061, 1435.583474523099994, 150.7184249802959926 ) ) ;
#31767 = CARTESIAN_POINT ( 'NONE',  ( 13.73564804769999981, 1415.163755998629995, 197.5875405738979964 ) ) ;
#31768 = CARTESIAN_POINT ( 'NONE',  ( -9.643453033020000120, 1414.681692383400105, 208.0622029686790029 ) ) ;
#31769 = CARTESIAN_POINT ( 'NONE',  ( 11.36018337630000019, 1414.996442546230128, 222.2791104318980047 ) ) ;
#31770 = CARTESIAN_POINT ( 'NONE',  ( 2.762616382466477560, 1451.876908917511173, 183.8170818175215970 ) ) ;
#31771 = CARTESIAN_POINT ( 'NONE',  ( 6.914811870799999483, 1487.329785955590069, 200.7563842756789825 ) ) ;
#31772 = B_SPLINE_CURVE_WITH_KNOTS ( 'NONE', 5,
 ( #52673, #17926, #26910, #34199, #44274, #86251 ),
 .UNSPECIFIED., .F., .F.,
 ( 6, 6 ),
 ( 0.000000000000000000, 1.000000000000000000 ),
 .UNSPECIFIED. ) ;
#31773 = CARTESIAN_POINT ( 'NONE',  ( -0.2545641238315171084, 1506.446781340913049, 187.1295352870444901 ) ) ;
#31774 = CARTESIAN_POINT ( 'NONE',  ( 24.34257435393226032, 1445.451185733568082, 214.1610445365998032 ) ) ;
#31775 = TOROIDAL_SURFACE ( 'NONE', #53225, 1.000000000000000000, 1.000000000000000000 ) ;
#31776 = CARTESIAN_POINT ( 'NONE',  ( -11.97724519069999971, 1441.600846913620217, 147.6096801420980000 ) ) ;
#31777 = FACE_OUTER_BOUND ( 'NONE', #72978, .T. ) ;
#31778 = CARTESIAN_POINT ( 'NONE',  ( 2.873958851594999864, 1516.588006113850042, 216.0563744999969913 ) ) ;
#31779 = VERTEX_POINT ( 'NONE', #39769 ) ;
#31780 = CARTESIAN_POINT ( 'NONE',  ( 7.715537193931590210, 1516.782738493960096, 208.5984514415330011 ) ) ;
#31781 = CARTESIAN_POINT ( 'NONE',  ( -15.45910334130000052, 1472.202164814229945, 270.0849031532980007 ) ) ;
#31782 = CARTESIAN_POINT ( 'NONE',  ( -16.93017999142119834, 1508.551704408389924, 212.6742212789120003 ) ) ;
#31783 = CARTESIAN_POINT ( 'NONE',  ( -16.54713268119330039, 1508.454488439769875, 213.8523356813170153 ) ) ;
#31784 = CARTESIAN_POINT ( 'NONE',  ( -2.620218387640000035, 1476.166204755790204, 220.2952108551989738 ) ) ;
#31785 = CARTESIAN_POINT ( 'NONE',  ( 30.25602947823919919, 1509.982583641990004, 213.6645168607980168 ) ) ;
#31786 = CARTESIAN_POINT ( 'NONE',  ( -11.39965473667389873, 1470.700470268689969, 209.4027647874690103 ) ) ;
#31787 = CARTESIAN_POINT ( 'NONE',  ( -6.423569254462077716, 1508.337306375136222, 219.9732112918911753 ) ) ;
#31788 = CARTESIAN_POINT ( 'NONE',  ( 17.97140328465984638, 1424.060494694068439, 225.5988178466726595 ) ) ;
#31790 = EDGE_CURVE ( 'NONE', #62931, #83528, #66153, .T. ) ;
#31789 = CARTESIAN_POINT ( 'NONE',  ( 1.085795944719189832, 1456.124699793469972, 198.6100061673760138 ) ) ;
#31791 = DIRECTION ( 'NONE',  ( -1.000000000000000000, 0.000000000000000000, 0.000000000000000000 ) ) ;
#31792 = CARTESIAN_POINT ( 'NONE',  ( 29.45229671441789776, 1440.913060386809775, 236.5454254465630015 ) ) ;
#31794 = CARTESIAN_POINT ( 'NONE',  ( -22.11554775090000291, 1489.452917662329810, 207.6017475386279898 ) ) ;
#31793 = CARTESIAN_POINT ( 'NONE',  ( -10.57951331165799935, 1470.368418028770066, 211.8757554959190088 ) ) ;
#31795 = CARTESIAN_POINT ( 'NONE',  ( 13.19072720129999965, 1429.093818030529974, 222.3773134601979962 ) ) ;
#31796 = ORIENTED_EDGE ( 'NONE', *, *, #80295, .F. ) ;
#31797 = ADVANCED_FACE ( 'NONE', ( #16726 ), #95159, .T. ) ;
#31798 = ORIENTED_EDGE ( 'NONE', *, *, #76199, .F. ) ;
#31799 = CARTESIAN_POINT ( 'NONE',  ( 7.491611919662470420, 1440.071325087319565, 213.7318617617365248 ) ) ;
#31800 = AXIS2_PLACEMENT_3D ( 'NONE', #26, #34159, #16229 ) ;
#31801 = EDGE_CURVE ( 'NONE', #79144, #11721, #55425, .T. ) ;
#31802 = CARTESIAN_POINT ( 'NONE',  ( 17.34616664546187081, 1410.519557093256935, 192.4923973019862729 ) ) ;
#31803 = CARTESIAN_POINT ( 'NONE',  ( 14.71230246817723142, 1414.913060387329779, 201.6306905010262369 ) ) ;
#31804 = CARTESIAN_POINT ( 'NONE',  ( 8.250335230039999246, 1424.462285376320096, 195.8663749243990253 ) ) ;
#31805 = CARTESIAN_POINT ( 'NONE',  ( -17.83486663330464950, 1523.678648413191695, 237.8759530894961074 ) ) ;
#31806 = CARTESIAN_POINT ( 'NONE',  ( 11.09879666485499961, 1422.175572497959820, 210.6094381644089992 ) ) ;
#31807 = EDGE_CURVE ( 'NONE', #52731, #63621, #50930, .T. ) ;
#31808 = CARTESIAN_POINT ( 'NONE',  ( -16.69297358003335674, 1526.382868172864164, 234.5473741529612255 ) ) ;
#31809 = CARTESIAN_POINT ( 'NONE',  ( -2.044097970649489948, 1508.551704408389924, 220.0684391793160160 ) ) ;
#31810 = CARTESIAN_POINT ( 'NONE',  ( -40.79815830855969949, 1383.826919031519992, 243.1918157079990124 ) ) ;
#31811 = AXIS2_PLACEMENT_3D ( 'NONE', #88066, #2422, #95894 ) ;
#31812 = CARTESIAN_POINT ( 'NONE',  ( -3.927225904784999777, 1511.005930286190051, 201.4860115694070259 ) ) ;
#31813 = CARTESIAN_POINT ( 'NONE',  ( -14.16616822539999987, 1471.309244717429920, 193.0783035305979922 ) ) ;
#31814 = CARTESIAN_POINT ( 'NONE',  ( -11.87563350447849864, 1433.006677213540115, 147.6591432354780125 ) ) ;
#31815 = CARTESIAN_POINT ( 'NONE',  ( 11.63699242075930051, 1492.551924726440120, 211.6216904535779975 ) ) ;
#31817 = ORIENTED_EDGE ( 'NONE', *, *, #100654, .T. ) ;
#31816 = CARTESIAN_POINT ( 'NONE',  ( -2.764335539890000248, 1457.844979587290027, 219.4374305647990013 ) ) ;
#31818 = CARTESIAN_POINT ( 'NONE',  ( 34.09079054514135976, 1524.667648926078527, 217.9059385276705143 ) ) ;
#31819 = CARTESIAN_POINT ( 'NONE',  ( -9.333610200140000757, 1378.889285013490280, 208.6192618550260249 ) ) ;
#31820 = CARTESIAN_POINT ( 'NONE',  ( 4.771130221510349934, 1508.551704408389924, 205.6145743722929922 ) ) ;
#31821 = ORIENTED_EDGE ( 'NONE', *, *, #27539, .T. ) ;
#31822 = EDGE_LOOP ( 'NONE', ( #32576, #62828, #58494, #110730, #76949, #99731, #92612, #21813 ) ) ;
#31823 = CARTESIAN_POINT ( 'NONE',  ( -9.071346014019580295, 1385.910705005249838, 218.5589227285099980 ) ) ;
#31824 = CARTESIAN_POINT ( 'NONE',  ( -2.329906356571839865, 1515.372228416479857, 204.8601837680460278 ) ) ;
#31826 = DIRECTION ( 'NONE',  ( -1.836970198721029688E-16, -1.000000000000000000, 0.000000000000000000 ) ) ;
#31825 = CARTESIAN_POINT ( 'NONE',  ( -17.17241001986523941, 1512.187213306747481, 179.6185504016045797 ) ) ;
#31827 = DIRECTION ( 'NONE',  ( -0.000000000000000000, -1.000000000000000000, -0.000000000000000000 ) ) ;
#31828 = CARTESIAN_POINT ( 'NONE',  ( -106.0162444670000070, 1379.399730046070090, 300.9954964968589479 ) ) ;
#31829 = FACE_OUTER_BOUND ( 'NONE', #12975, .T. ) ;
#31830 = CARTESIAN_POINT ( 'NONE',  ( -13.28196447587500018, 1508.551704408389924, 216.3748897397299800 ) ) ;
#31831 = AXIS2_PLACEMENT_3D ( 'NONE', #45502, #88046, #10208 ) ;
#31832 = CARTESIAN_POINT ( 'NONE',  ( 11.91057031607170025, 1409.328986667859908, 200.0892353780850215 ) ) ;
#31833 = CARTESIAN_POINT ( 'NONE',  ( -3.899071993169999590E-16, 1420.943991414029824, 172.2701767054979882 ) ) ;
#31834 = DIRECTION ( 'NONE',  ( 0.7414773880254614813, 0.000000000000000000, -0.6709778558543786353 ) ) ;
#31835 = EDGE_CURVE ( 'NONE', #26950, #7882, #37948, .T. ) ;
#31836 = CARTESIAN_POINT ( 'NONE',  ( 7.743638678103569539, 1435.911626056160003, 205.3099362470069877 ) ) ;
#31837 = CARTESIAN_POINT ( 'NONE',  ( -2.500000000000000000, 1439.615672362369878, 170.5246407198980023 ) ) ;
#31838 = CARTESIAN_POINT ( 'NONE',  ( -3.724487131215511670, 1424.082886414761788, 184.7380720752485956 ) ) ;
#31839 = VERTEX_POINT ( 'NONE', #84517 ) ;
#31840 = EDGE_CURVE ( 'NONE', #49915, #25603, #83357, .T. ) ;
#31841 = CARTESIAN_POINT ( 'NONE',  ( -2.431412526649999961, 1428.647745098929818, 149.4227846719979880 ) ) ;
#31842 = CARTESIAN_POINT ( 'NONE',  ( 18.31156613494090024, 1457.716607816860005, 228.0465888042749896 ) ) ;
#31843 = CARTESIAN_POINT ( 'NONE',  ( -12.64307430949999933, 1435.023293913380030, 150.5876313343979973 ) ) ;
#31844 = DIRECTION ( 'NONE',  ( -1.040834085586083310E-14, 0.000000000000000000, 1.000000000000000000 ) ) ;
#31845 = CARTESIAN_POINT ( 'NONE',  ( -17.05938549526129577, 1517.051704405600049, 195.1949804090679947 ) ) ;
#31846 = CARTESIAN_POINT ( 'NONE',  ( -25.00976051679999657, 1436.598010167069788, 137.9330532114979917 ) ) ;
#31847 = CARTESIAN_POINT ( 'NONE',  ( -109.0826469409999930, 1385.476187853860210, 311.2341188642590168 ) ) ;
#31848 = CARTESIAN_POINT ( 'NONE',  ( -8.797412869267919433, 1511.644547967860035, 215.2508032624510008 ) ) ;
#31849 = CARTESIAN_POINT ( 'NONE',  ( -10.22852398056611278, 1361.350133274729160, 209.6218459617033432 ) ) ;
#31850 = CARTESIAN_POINT ( 'NONE',  ( -45.67170290102849606, 1440.913066807300083, 266.1885079402800329 ) ) ;
#31851 = CARTESIAN_POINT ( 'NONE',  ( -23.20318578650891794, 1433.765053652970209, 215.6666533212324168 ) ) ;
#31852 = CARTESIAN_POINT ( 'NONE',  ( 13.89991610216109841, 1452.702855433150035, 223.2766279111739891 ) ) ;
#31853 = CARTESIAN_POINT ( 'NONE',  ( -5.781585816274999345, 1516.939646076049939, 209.1342929058909874 ) ) ;
#31854 = VECTOR ( 'NONE', #104005, 1000.000000000000000 ) ;
#31855 = LINE ( 'NONE', #58179, #37730 ) ;
#31856 = FILL_AREA_STYLE_COLOUR ( '', #28373 ) ;
#31857 = CARTESIAN_POINT ( 'NONE',  ( 2.809892388859999812, 1422.122748426330190, 101.6305461396979979 ) ) ;
#31858 = CARTESIAN_POINT ( 'NONE',  ( 7.261033881273809776, 1424.990117404329794, 212.7330084483390067 ) ) ;
#31859 = ORIENTED_EDGE ( 'NONE', *, *, #19031, .F. ) ;
#31860 = CARTESIAN_POINT ( 'NONE',  ( 26.00754374119999923, 1427.792721087130076, 240.2274372948979817 ) ) ;
#31861 = CARTESIAN_POINT ( 'NONE',  ( 22.08622291482350519, 1523.382868172864164, 233.8253038720783366 ) ) ;
#31863 = DIRECTION ( 'NONE',  ( -5.980589973904019347E-17, 1.000000000000000000, -1.736889445713099699E-16 ) ) ;
#31862 = CARTESIAN_POINT ( 'NONE',  ( -0.4526181979879999595, 1452.693343343929882, 183.1469136533980020 ) ) ;
#31864 = CARTESIAN_POINT ( 'NONE',  ( 15.74021840907683512, 1521.951704408389787, 196.3375305114159062 ) ) ;
#31865 = CARTESIAN_POINT ( 'NONE',  ( -23.79286722360000184, 1428.843115172530133, 231.7321643605979773 ) ) ;
#31866 = CARTESIAN_POINT ( 'NONE',  ( -29.04414693871334308, 1509.932335316460922, 204.0080394800089039 ) ) ;
#31867 = CARTESIAN_POINT ( 'NONE',  ( -8.876970405461879210, 1452.603069750020040, 151.0241627572419816 ) ) ;
#31868 = CARTESIAN_POINT ( 'NONE',  ( 27.02655593769999953, 1451.108952154630060, 136.3738421987980018 ) ) ;
#31869 = ORIENTED_EDGE ( 'NONE', *, *, #13707, .T. ) ;
#31870 = CARTESIAN_POINT ( 'NONE',  ( -2.500000000000000000, 1424.046630307830128, 154.4234530583979961 ) ) ;
#31871 = CARTESIAN_POINT ( 'NONE',  ( 6.691728662302649767E-05, 1410.389828169050134, 269.3346513474109543 ) ) ;
#31872 = CARTESIAN_POINT ( 'NONE',  ( 15.59164432048419968, 1421.661620995860176, 227.7520908980149841 ) ) ;
#31873 = CARTESIAN_POINT ( 'NONE',  ( 9.717822231039999537, 1463.678487757089897, 210.3770952454989924 ) ) ;
#31874 = ORIENTED_EDGE ( 'NONE', *, *, #66459, .F. ) ;
#31875 = ORIENTED_EDGE ( 'NONE', *, *, #102104, .T. ) ;
#31876 = VECTOR ( 'NONE', #24874, 1000.000000000000000 ) ;
#31877 = CARTESIAN_POINT ( 'NONE',  ( -46.08898162120000563, 1384.736188145109963, 219.0284454471089646 ) ) ;
#31878 = CARTESIAN_POINT ( 'NONE',  ( -23.73958735709999956, 1410.154131308830074, 209.3402010283099912 ) ) ;
#31879 = ORIENTED_EDGE ( 'NONE', *, *, #56752, .F. ) ;
#31880 = CARTESIAN_POINT ( 'NONE',  ( 3.803002571174680213, 1508.880967335730247, 204.6292016602320132 ) ) ;
#31881 = DIRECTION ( 'NONE',  ( 0.000000000000000000, -1.000000000000000000, 0.000000000000000000 ) ) ;
#31882 = CIRCLE ( 'NONE', #35492, 2.000000000000001776 ) ;
#31883 = AXIS2_PLACEMENT_3D ( 'NONE', #91460, #5242, #66828 ) ;
#31884 = CARTESIAN_POINT ( 'NONE',  ( -2.900078654861840022, 1473.495617646690107, 183.7954459137889955 ) ) ;
#31885 = CARTESIAN_POINT ( 'NONE',  ( -21.24403838879999995, 1415.846602379829847, 218.4048111434979944 ) ) ;
#31886 = CIRCLE ( 'NONE', #17561, 33.13701971169416538 ) ;
#31887 = CARTESIAN_POINT ( 'NONE',  ( 45.98765409508450830, 1442.794819212339917, 268.4974154456440374 ) ) ;
#31888 = CARTESIAN_POINT ( 'NONE',  ( -4.487358483189090030, 1509.034524749680031, 205.3201112091969947 ) ) ;
#31889 = CARTESIAN_POINT ( 'NONE',  ( -5.881379503709999845, 1428.766218426890191, 203.1321793329989873 ) ) ;
#31890 = CARTESIAN_POINT ( 'NONE',  ( 2.479246847704999812, 1516.983612918759945, 205.0778556245070092 ) ) ;
#31891 = ORIENTED_EDGE ( 'NONE', *, *, #105901, .F. ) ;
#31892 = CARTESIAN_POINT ( 'NONE',  ( 3.034964868304999897, 1517.051704408389924, 200.9398869892670234 ) ) ;
#31893 = AXIS2_PLACEMENT_3D ( 'NONE', #30192, #36945, #62187 ) ;
#31894 = CARTESIAN_POINT ( 'NONE',  ( 15.02944345243210122, 1512.205851781539877, 196.5435174618820042 ) ) ;
#31895 = CARTESIAN_POINT ( 'NONE',  ( 9.293666974126480795, 1480.089863132871187, 204.1131580292703802 ) ) ;
#31896 = ORIENTED_EDGE ( 'NONE', *, *, #4958, .T. ) ;
#31897 = CARTESIAN_POINT ( 'NONE',  ( -10.63047325564510004, 1480.584009184299930, 210.2203730784849824 ) ) ;
#31898 = CARTESIAN_POINT ( 'NONE',  ( 26.56840054362369585, 1451.979948467160057, 135.1038962431699986 ) ) ;
#31899 = CARTESIAN_POINT ( 'NONE',  ( -12.62550847681250055, 1512.222316757829958, 194.0651229827790019 ) ) ;
#31900 = CARTESIAN_POINT ( 'NONE',  ( 7.461990519024649160, 1504.220424024579870, 219.4654900686530254 ) ) ;
#31901 = CARTESIAN_POINT ( 'NONE',  ( 7.782527000790000038, 1421.790398246840141, 195.8641137985989928 ) ) ;
#31902 = CARTESIAN_POINT ( 'NONE',  ( 21.63150929049999860, 1409.668449337029870, 213.1599398232280009 ) ) ;
#31903 = CARTESIAN_POINT ( 'NONE',  ( -9.819355888608599869, 1492.974921486040103, 201.7186537263710022 ) ) ;
#31904 = CARTESIAN_POINT ( 'NONE',  ( -4.321803588699999921, 1496.124825247590024, 198.6279956811989962 ) ) ;
#31905 = DIRECTION ( 'NONE',  ( 1.000000000000000000, 0.000000000000000000, 0.000000000000000000 ) ) ;
#31907 = CARTESIAN_POINT ( 'NONE',  ( -18.22449011683852760, 1423.927591919610677, 225.4533452331210412 ) ) ;
#31906 = CARTESIAN_POINT ( 'NONE',  ( -13.80541478530910027, 1434.979604282769969, 148.5370187744020143 ) ) ;
#31908 = CARTESIAN_POINT ( 'NONE',  ( 10.66776494214329851, 1424.286285492139996, 206.6302606398689932 ) ) ;
#31909 = CARTESIAN_POINT ( 'NONE',  ( -13.59371612979999888, 1379.659895191500027, 212.3998098368589922 ) ) ;
#31910 = CARTESIAN_POINT ( 'NONE',  ( -7.636446066375000008, 1514.050458741980037, 203.1354708283169828 ) ) ;
#31911 = ORIENTED_EDGE ( 'NONE', *, *, #100195, .T. ) ;
#31912 = CARTESIAN_POINT ( 'NONE',  ( 3.268607741949999923, 1425.981674191930097, 219.6133831120980062 ) ) ;
#31913 = DIRECTION ( 'NONE',  ( 0.02616798426500960631, -0.9993150019883683122, -0.02616798426500955774 ) ) ;
#31914 = DIRECTION ( 'NONE',  ( 1.000000000000000000, 5.309750374689999822E-19, 2.343158368729999945E-19 ) ) ;
#31915 = CARTESIAN_POINT ( 'NONE',  ( -9.082734998440001206, 1385.203252519110038, 199.9450228470490174 ) ) ;
#31916 = CARTESIAN_POINT ( 'NONE',  ( 9.802591111456759876, 1422.649162510939959, 211.3555123156029936 ) ) ;
#31917 = CARTESIAN_POINT ( 'NONE',  ( 11.58812742166940168, 1425.640754144680159, 202.9099269016940070 ) ) ;
#31918 = B_SPLINE_CURVE_WITH_KNOTS ( 'NONE', 3,
 ( #33824, #26529, #60725, #60156, #69119, #51191 ),
 .UNSPECIFIED., .F., .F.,
 ( 4, 2, 4 ),
 ( 0.000000000000000000, 0.5000000000000000000, 1.000000000000000000 ),
 .UNSPECIFIED. ) ;
#31919 = CARTESIAN_POINT ( 'NONE',  ( 16.81223226430000039, 1414.913060387329779, 210.6693098017280192 ) ) ;
#31920 = CARTESIAN_POINT ( 'NONE',  ( 16.49514911236786219, 1525.343710797494396, 237.0302821690905546 ) ) ;
#31921 = CARTESIAN_POINT ( 'NONE',  ( -7.795091205023656933, 1476.960015112429573, 215.9744489608353319 ) ) ;
#31923 = EDGE_CURVE ( 'NONE', #67251, #16145, #3990, .T. ) ;
#31922 = CARTESIAN_POINT ( 'NONE',  ( -12.63252536770000134, 1420.772946692730102, 222.2681001552979865 ) ) ;
#31924 = CARTESIAN_POINT ( 'NONE',  ( 39.47393889809999479, 1455.502555575530096, 271.1218459616979999 ) ) ;
#31925 = CARTESIAN_POINT ( 'NONE',  ( 0.9233357834264179775, 1450.850097690670054, 181.4078119359379855 ) ) ;
#31926 = CARTESIAN_POINT ( 'NONE',  ( -16.77179453697938527, 1420.486811422051233, 203.1613059882370180 ) ) ;
#31927 = CARTESIAN_POINT ( 'NONE',  ( 0.4435022289555869968, 1418.672171135500093, 184.7048927309859891 ) ) ;
#31928 = CARTESIAN_POINT ( 'NONE',  ( 11.35225316950000085, 1419.758531043530184, 229.7208292713979745 ) ) ;
#31929 = CARTESIAN_POINT ( 'NONE',  ( 0.8775825618903729808, 1398.755125754900064, 208.6424204230947907 ) ) ;
#31930 = CARTESIAN_POINT ( 'NONE',  ( 4.223612416888080645, 1474.237109173149975, 219.7333844760279931 ) ) ;
#31931 = CARTESIAN_POINT ( 'NONE',  ( -18.01164195190000328, 1410.466195698429829, 224.7175291131979975 ) ) ;
#31932 = FACE_OUTER_BOUND ( 'NONE', #6071, .T. ) ;
#31933 = B_SPLINE_CURVE_WITH_KNOTS ( 'NONE', 5,
 ( #88551, #106983, #81224, #29184, #106442, #48201 ),
 .UNSPECIFIED., .F., .F.,
 ( 6, 6 ),
 ( 0.000000000000000000, 1.000000000000000000 ),
 .UNSPECIFIED. ) ;
#31934 = CARTESIAN_POINT ( 'NONE',  ( -25.55912388069999963, 1449.022877353309923, 137.9013602817979915 ) ) ;
#31935 = CARTESIAN_POINT ( 'NONE',  ( -17.58999536348959936, 1410.451648346190041, 193.0352298804580187 ) ) ;
#31936 = EDGE_CURVE ( 'NONE', #21237, #57810, #48742, .T. ) ;
#31937 = CARTESIAN_POINT ( 'NONE',  ( 1.346199663083729914E-06, 1408.510422093800116, 195.3530119415600268 ) ) ;
#31938 = DIRECTION ( 'NONE',  ( -1.000000000000000000, 0.000000000000000000, 0.000000000000000000 ) ) ;
#31939 = CARTESIAN_POINT ( 'NONE',  ( -17.51440549372729905, 1442.103934404829943, 219.2287673605049747 ) ) ;
#31940 = CARTESIAN_POINT ( 'NONE',  ( -3.560380890149999811, 1415.087974640030097, 226.2956427098980043 ) ) ;
#31941 = CARTESIAN_POINT ( 'NONE',  ( 0.1872740515456740029, 1470.279753032280041, 182.5118344780429709 ) ) ;
#31943 = ORIENTED_EDGE ( 'NONE', *, *, #19428, .T. ) ;
#31942 = CARTESIAN_POINT ( 'NONE',  ( 8.293154156760014217, 1466.896286154528752, 203.5718718306909523 ) ) ;
#31944 = CARTESIAN_POINT ( 'NONE',  ( -20.17294526779999941, 1444.994950788469851, 161.5349527656980229 ) ) ;
#31945 = ADVANCED_FACE ( 'NONE', ( #76124 ), #71612, .T. ) ;
#31946 = CARTESIAN_POINT ( 'NONE',  ( -0.8748704360600072505, 1484.083060082853308, 198.4676730996152969 ) ) ;
#31947 = CARTESIAN_POINT ( 'NONE',  ( 11.94112614929999872, 1433.615419815239875, 149.4776156485979755 ) ) ;
#31948 = CARTESIAN_POINT ( 'NONE',  ( -40.33550002387350020, 1439.280879845010077, 134.0999999981289932 ) ) ;
#31949 = CARTESIAN_POINT ( 'NONE',  ( -3.628052555810424629, 1430.352677179689636, 201.5964689278353035 ) ) ;
#31950 = ORIENTED_EDGE ( 'NONE', *, *, #99420, .T. ) ;
#31951 = B_SPLINE_SURFACE_WITH_KNOTS ( 'NONE', 5, 5, ( 
 ( #109063, #67066, #65970, #93884, #50799, #49159 ),
 ( #25017, #6035, #50267, #23914, #48610, #7141 ),
 ( #16064, #84396, #110145, #109604, #32877, #32347 ),
 ( #76543, #7684, #59218, #33419, #57567, #41296 ),
 ( #40739, #58656, #92791, #93337, #59763, #110695 ),
 ( #49710, #33988, #74369, #82743, #101172, #24467 ),
 ( #74914, #66526, #58109, #92240, #15512, #103380 ),
 ( #102827, #11007, #77655, #1512, #95009, #968 ),
 ( #422, #62550, #96104, #60311, #18276, #104507 ),
 ( #18827, #69275, #17150, #86599, #94430, #95555 ),
 ( #10446, #78199, #44059, #35092, #87157, #19378 ),
 ( #44619, #68724, #26684, #17708, #28354, #35642 ) ),
 .UNSPECIFIED., .F., .F., .F.,
 ( 6, 3, 3, 6 ),
 ( 6, 6 ),
 ( 4.119532581660000581, 6.664003371819999799, 7.493366175190000256, 9.981901822019999315 ),
 ( 0.000000000000000000, 2.000000000000000000 ),
 .UNSPECIFIED. ) ;
#31952 = FACE_OUTER_BOUND ( 'NONE', #18348, .T. ) ;
#31953 = CARTESIAN_POINT ( 'NONE',  ( 2.620401159549908598, 1523.382868172863937, 176.0805060893157190 ) ) ;
#31954 = CARTESIAN_POINT ( 'NONE',  ( -104.2957601855958814, 1380.406565240221653, 307.1919735274812524 ) ) ;
#31955 = DIRECTION ( 'NONE',  ( -1.755985294532469921E-16, 1.000000000000000000, -1.338183447452831989E-16 ) ) ;
#31956 = CARTESIAN_POINT ( 'NONE',  ( 2.516232255349999836, 1464.674062122390069, 202.5523636628589941 ) ) ;
#31957 = CARTESIAN_POINT ( 'NONE',  ( -46.02997362520000735, 1440.913038198389813, 268.4959101188979957 ) ) ;
#31958 = B_SPLINE_CURVE_WITH_KNOTS ( 'NONE', 3,
 ( #107561, #3481, #63936, #99141 ),
 .UNSPECIFIED., .F., .F.,
 ( 4, 4 ),
 ( 0.000000000000000000, 1.000000000000000000 ),
 .UNSPECIFIED. ) ;
#31959 = AXIS2_PLACEMENT_3D ( 'NONE', #84322, #24938, #68106 ) ;
#31960 = DIRECTION ( 'NONE',  ( 0.000000000000000000, 0.000000000000000000, 1.000000000000000000 ) ) ;
#31961 = CARTESIAN_POINT ( 'NONE',  ( -12.31607806409999917, 1378.979632277839983, 209.9715911835569955 ) ) ;
#31962 = CARTESIAN_POINT ( 'NONE',  ( 3.910028042040000429, 1431.491579035269979, 185.0507363215979808 ) ) ;
#31963 = CARTESIAN_POINT ( 'NONE',  ( -50.69150226891620292, 1385.021539566839920, 226.3387534530459959 ) ) ;
#31964 = CARTESIAN_POINT ( 'NONE',  ( -11.18264923832449931, 1391.913060387289988, 212.0534155766569882 ) ) ;
#31965 = CARTESIAN_POINT ( 'NONE',  ( -26.79413167943010166, 1436.761919080860025, 136.7821860765010058 ) ) ;
#31966 = EDGE_LOOP ( 'NONE', ( #28865, #6070, #84763, #8606 ) ) ;
#31967 = CONICAL_SURFACE ( 'NONE', #89209, 7.500000000000000000, 0.02617993877989872875 ) ;
#31968 = CARTESIAN_POINT ( 'NONE',  ( -27.26775404520000023, 1451.960960096730105, 134.9110166487979825 ) ) ;
#31969 = CARTESIAN_POINT ( 'NONE',  ( -17.00746236582520154, 1410.591278265990013, 226.2082703236820009 ) ) ;
#31971 = ORIENTED_EDGE ( 'NONE', *, *, #44604, .T. ) ;
#31970 = CARTESIAN_POINT ( 'NONE',  ( -18.74729292449999818, 1442.199705176290081, 209.1218459616989946 ) ) ;
#31972 = CARTESIAN_POINT ( 'NONE',  ( 5.826428076080000906, 1473.811884028689974, 218.9454251420289950 ) ) ;
#31973 = AXIS2_PLACEMENT_3D ( 'NONE', #49287, #15095, #74497 ) ;
#31974 = CARTESIAN_POINT ( 'NONE',  ( 10.18019783711949877, 1471.338426166499858, 211.9712393461159934 ) ) ;
#31975 = EDGE_CURVE ( 'NONE', #75650, #108306, #34416, .T. ) ;
#31976 = CARTESIAN_POINT ( 'NONE',  ( 22.97508917209999879, 1509.490924000130008, 224.8302120705980087 ) ) ;
#31977 = CARTESIAN_POINT ( 'NONE',  ( -109.1258763339999973, 1384.668900320659986, 311.2567808922589734 ) ) ;
#31978 = CARTESIAN_POINT ( 'NONE',  ( -0.1548877673338640015, 1419.548927902510059, 184.3830762897939906 ) ) ;
#31979 = CARTESIAN_POINT ( 'NONE',  ( 0.9551731419629999609, 1466.226277197029958, 235.4680291051979850 ) ) ;
#31980 = CARTESIAN_POINT ( 'NONE',  ( 17.22539861130000105, 1409.514584562929940, 222.3763154799979986 ) ) ;
#31981 = CARTESIAN_POINT ( 'NONE',  ( -2.666035071639449860, 1419.521156420629950, 186.1676433668029915 ) ) ;
#31982 = CARTESIAN_POINT ( 'NONE',  ( -17.71700096680000058, 1424.354672622029966, 228.0407626086980031 ) ) ;
#31983 = CARTESIAN_POINT ( 'NONE',  ( -3.806637153123912043, 1511.520884442064244, 200.9879143131876162 ) ) ;
#31984 = CARTESIAN_POINT ( 'NONE',  ( 7.244363788860000319, 1481.023503507690066, 208.0198210207190073 ) ) ;
#31985 = CARTESIAN_POINT ( 'NONE',  ( -113.4000000000000057, 1311.832804576489934, 294.9031044600990299 ) ) ;
#31986 = CARTESIAN_POINT ( 'NONE',  ( -3.173741429363529321, 1370.393155323753945, 210.6218459617030021 ) ) ;
#31987 = B_SPLINE_CURVE_WITH_KNOTS ( 'NONE', 5,
 ( #11719, #36914, #36362, #53185, #61589, #53760, #97370, #87327, #95174 ),
 .UNSPECIFIED., .F., .F.,
 ( 6, 3, 6 ),
 ( 0.000000000000000000, 0.6021179571096993977, 1.000000000000000000 ),
 .UNSPECIFIED. ) ;
#31988 = CARTESIAN_POINT ( 'NONE',  ( 8.796059898599999372, 1362.759824263850078, 210.6218459616991936 ) ) ;
#31989 = CARTESIAN_POINT ( 'NONE',  ( 6.547556931335000385, 1516.633288330999903, 205.8595812817970057 ) ) ;
#31990 = CIRCLE ( 'NONE', #46338, 0.9999999999999685807 ) ;
#31991 = CARTESIAN_POINT ( 'NONE',  ( -10.49533061896650032, 1485.816092626590034, 184.3926849958960190 ) ) ;
#31992 = VERTEX_POINT ( 'NONE', #10579 ) ;
#31993 = CARTESIAN_POINT ( 'NONE',  ( 2.890489020090289962, 1507.108937781499890, 235.9439513786750240 ) ) ;
#31994 = CARTESIAN_POINT ( 'NONE',  ( -0.9080294960061148224, 1420.737356635930155, 182.9235011294603055 ) ) ;
#31996 = ORIENTED_EDGE ( 'NONE', *, *, #57059, .F. ) ;
#31995 = CARTESIAN_POINT ( 'NONE',  ( -68.62638760068000465, 1379.747582755300073, 280.2329060256320190 ) ) ;
#31997 = ORIENTED_EDGE ( 'NONE', *, *, #11077, .F. ) ;
#31998 = CARTESIAN_POINT ( 'NONE',  ( -7.896115406091596789, 1382.897682410418156, 218.7445328676782594 ) ) ;
#31999 = ORIENTED_EDGE ( 'NONE', *, *, #50256, .F. ) ;
#32000 = CARTESIAN_POINT ( 'NONE',  ( 2.396857868302820105, 1485.113936978040101, 220.7346362247920126 ) ) ;
#32001 = CARTESIAN_POINT ( 'NONE',  ( -22.35979953749999893, 1410.906900737730211, 203.0403674361979824 ) ) ;
#32003 = CARTESIAN_POINT ( 'NONE',  ( 15.93913202865929968, 1410.714489637869974, 191.5350724760020285 ) ) ;
#32002 = CARTESIAN_POINT ( 'NONE',  ( -9.939393947103138061, 1441.236512651819794, 153.4167241843420300 ) ) ;
#32004 = CARTESIAN_POINT ( 'NONE',  ( 5.789394662204999875, 1517.164987839469859, 210.8286437561770299 ) ) ;
#32005 = CARTESIAN_POINT ( 'NONE',  ( 41.61584690620330207, 1442.586878941469877, 136.0036615449459987 ) ) ;
#32006 = CARTESIAN_POINT ( 'NONE',  ( -10.81515773970000005, 1424.921120067930133, 144.1684135307980057 ) ) ;
#32007 = LINE ( 'NONE', #66741, #5338 ) ;
#32008 = CARTESIAN_POINT ( 'NONE',  ( 12.70100719244910081, 1500.608200984970154, 209.4159698383299997 ) ) ;
#32009 = APPLICATION_PROTOCOL_DEFINITION ( 'draft international standard', 'automotive_design', 1998, #45628 ) ;
#32010 = CARTESIAN_POINT ( 'NONE',  ( -5.864566082395460178, 1522.051704408389924, 192.0899093523580063 ) ) ;
#32011 = CARTESIAN_POINT ( 'NONE',  ( -14.88313348660000024, 1507.431571772529878, 231.7094224802980023 ) ) ;
#32012 = ORIENTED_EDGE ( 'NONE', *, *, #68131, .F. ) ;
#32013 = CARTESIAN_POINT ( 'NONE',  ( -21.44637752539939868, 1506.412652546340269, 216.0243762360449864 ) ) ;
#32014 = CARTESIAN_POINT ( 'NONE',  ( -18.21986176780000122, 1458.468391452929836, 227.9546142145979957 ) ) ;
#32015 = ORIENTED_EDGE ( 'NONE', *, *, #40642, .T. ) ;
#32016 = ORIENTED_EDGE ( 'NONE', *, *, #69304, .F. ) ;
#32017 = CARTESIAN_POINT ( 'NONE',  ( 15.83309290234510414, 1410.837657475366996, 227.0154553047771913 ) ) ;
#32018 = CARTESIAN_POINT ( 'NONE',  ( 10.28174319281220050, 1453.348041341110047, 211.7471195966300002 ) ) ;
#32019 = APPLICATION_CONTEXT ( 'automotive_design' ) ;
#32020 = CARTESIAN_POINT ( 'NONE',  ( 0.000000000000000000, 1518.913060387330006, 209.1218459616979999 ) ) ;
#32021 = CARTESIAN_POINT ( 'NONE',  ( -20.35947145212350051, 1508.252440922349933, 209.6500315394189897 ) ) ;
#32022 = CARTESIAN_POINT ( 'NONE',  ( -3.428961876718509050, 1367.251209528720665, 208.3718459617061285 ) ) ;
#32023 = CARTESIAN_POINT ( 'NONE',  ( 2.330134126767420266, 1515.064792882699976, 204.7923971855439902 ) ) ;
#32024 = VECTOR ( 'NONE', #92314, 1000.000000000000114 ) ;
#32025 = CARTESIAN_POINT ( 'NONE',  ( -12.31752013540000057, 1377.944433778000075, 209.1218459012849848 ) ) ;
#32026 = CARTESIAN_POINT ( 'NONE',  ( 33.91369120209999721, 1451.728768194229815, 134.0999999980979851 ) ) ;
#32027 = CARTESIAN_POINT ( 'NONE',  ( 2.606069733071630257, 1421.343799577720119, 183.3146730432610241 ) ) ;
#32028 = FACE_OUTER_BOUND ( 'NONE', #36980, .T. ) ;
#32029 = CARTESIAN_POINT ( 'NONE',  ( -10.67458293690000026, 1390.939237263959967, 215.3172610932390114 ) ) ;
#32030 = CARTESIAN_POINT ( 'NONE',  ( -83.57387407986560390, 1384.811398240090057, 287.3271726340860255 ) ) ;
#32031 = ORIENTED_EDGE ( 'NONE', *, *, #26512, .F. ) ;
#32032 = CARTESIAN_POINT ( 'NONE',  ( 2.290256263724999908, 1517.170721208160103, 202.1706708033170230 ) ) ;
#32033 = CARTESIAN_POINT ( 'NONE',  ( -6.952166420425000659, 1517.213554313520035, 207.4130983078469797 ) ) ;
#32034 = ORIENTED_EDGE ( 'NONE', *, *, #22923, .F. ) ;
#32035 = CARTESIAN_POINT ( 'NONE',  ( 37.85189106831440142, 1440.913060387330006, 264.7684821643020427 ) ) ;
#32036 = CARTESIAN_POINT ( 'NONE',  ( 18.48154349909999539, 1467.192605361630058, 228.1015105461979999 ) ) ;
#32037 = VERTEX_POINT ( 'NONE', #12216 ) ;
#32038 = TOROIDAL_SURFACE ( 'NONE', #99959, 1.000000000000000000, 1.000000000000000000 ) ;
#32039 = DIRECTION ( 'NONE',  ( -7.436362843295819681E-17, 1.000000000000000000, -1.457576885956999882E-16 ) ) ;
#32040 = CARTESIAN_POINT ( 'NONE',  ( 8.454790733525280544, 1428.363638633589972, 213.4109935021670026 ) ) ;
#32041 = CARTESIAN_POINT ( 'NONE',  ( -17.02817110700241443, 1508.455360531000224, 213.2597695858250404 ) ) ;
#32042 = CARTESIAN_POINT ( 'NONE',  ( -10.69637384178539996, 1462.945480530389887, 206.3136169826919968 ) ) ;
#32043 = FACE_OUTER_BOUND ( 'NONE', #68972, .T. ) ;
#32044 = CARTESIAN_POINT ( 'NONE',  ( 10.63889126261920026, 1470.011729377750044, 207.0794648040029813 ) ) ;
#32045 = CARTESIAN_POINT ( 'NONE',  ( -3.611923964340000293, 1508.978187008830218, 180.0004836359980231 ) ) ;
#32046 = CARTESIAN_POINT ( 'NONE',  ( -12.06145328200000044, 1433.903212736319801, 146.4342169817980164 ) ) ;
#32047 = CARTESIAN_POINT ( 'NONE',  ( 26.49460307026359729, 1499.744025783769985, 206.2293708431749906 ) ) ;
#32049 = CARTESIAN_POINT ( 'NONE',  ( -10.57448040964888492, 1423.877913334070627, 137.4727699158958956 ) ) ;
#32048 = CARTESIAN_POINT ( 'NONE',  ( 12.60568905610000101, 1462.740100782129957, 231.3171901606980043 ) ) ;
#32050 = CARTESIAN_POINT ( 'NONE',  ( -4.603585632142040751, 1422.096080299584173, 184.6430019781807346 ) ) ;
#32051 = CARTESIAN_POINT ( 'NONE',  ( -2.291514335905000088, 1517.194972660189933, 216.8481778957070105 ) ) ;
#32052 = ORIENTED_EDGE ( 'NONE', *, *, #80306, .T. ) ;
#32053 = VECTOR ( 'NONE', #40864, 1000.000000000000227 ) ;
#32054 = CARTESIAN_POINT ( 'NONE',  ( -1.098784916811339940, 1486.285180436948394, 181.7858322622153935 ) ) ;
#32055 = CARTESIAN_POINT ( 'NONE',  ( -0.03770439129968750080, 1508.815788562569878, 179.7994759633430135 ) ) ;
#32056 = AXIS2_PLACEMENT_3D ( 'NONE', #52918, #37209, #63007 ) ;
#32057 = CARTESIAN_POINT ( 'NONE',  ( -21.83164632205553346, 1524.739915903632664, 233.6211154403027024 ) ) ;
#32058 = CARTESIAN_POINT ( 'NONE',  ( 1.714334247185000049, 1516.699825673279975, 213.1484604498870112 ) ) ;
#32059 = CARTESIAN_POINT ( 'NONE',  ( 18.56428471230000099, 1507.623776012629833, 188.5292884487979848 ) ) ;
#32060 =( BOUNDED_SURFACE ( )  B_SPLINE_SURFACE ( 3, 2, ( 
 ( #54869, #52657, #105821 ),
 ( #97399, #70036, #1159 ),
 ( #96304, #87923, #70580 ),
 ( #69475, #11744, #78401 ),
 ( #104148, #27434, #11210 ),
 ( #26895, #61084, #20134 ),
 ( #88457, #61617, #95749 ),
 ( #87355, #10651, #78973 ),
 ( #14482, #22868, #56515 ),
 ( #107445, #82798, #66031 ) ),
 .UNSPECIFIED., .F., .F., .F. ) 
 B_SPLINE_SURFACE_WITH_KNOTS ( ( 4, 2, 2, 2, 4 ),
 ( 3, 3 ),
 ( 1.570796326794896558, 1.963495408493620697, 2.356194490192344837, 2.748893571891068976, 3.141592653589793116 ),
 ( 0.000000000000000000, 1.000000000000000000 ),
 .UNSPECIFIED. ) 
 GEOMETRIC_REPRESENTATION_ITEM ( )  RATIONAL_B_SPLINE_SURFACE ( (
 ( 1.000000000000000000, 0.7071067811865870967, 1.000000000000000000),
 ( 1.000000000000000000, 0.7166207884813499129, 1.000000000000000000),
 ( 1.000000000000000000, 0.7259222650918575326, 1.000000000000000000),
 ( 1.000000000000000000, 0.7428408967918733730, 1.000000000000000000),
 ( 1.000000000000000000, 0.7504512394537499187, 1.000000000000000000),
 ( 1.000000000000000000, 0.7630177051937450106, 1.000000000000000000),
 ( 1.000000000000000000, 0.7679730451964706939, 1.000000000000000000),
 ( 1.000000000000000000, 0.7746454561805765637, 1.000000000000000000),
 ( 1.000000000000000000, 0.7763684247028794783, 1.000000000000000000),
 ( 1.000000000000000000, 0.7763623250684325017, 1.000000000000000000) ) ) 
 REPRESENTATION_ITEM ( '' )  SURFACE ( )  );
#32061 = DIRECTION ( 'NONE',  ( 0.000000000000000000, 1.000000000000000000, 0.000000000000000000 ) ) ;
#32063 = EDGE_LOOP ( 'NONE', ( #88828, #48844, #58074, #46830 ) ) ;
#32062 = CARTESIAN_POINT ( 'NONE',  ( -12.48995958582669985, 1501.883328869510024, 211.6213070116990025 ) ) ;
#32064 = CARTESIAN_POINT ( 'NONE',  ( -17.83486663330463173, 1523.678648413191922, 237.8759530894961358 ) ) ;
#32065 = CARTESIAN_POINT ( 'NONE',  ( 2.810679194570000039, 1508.430220233089813, 220.1167136484990010 ) ) ;
#32066 = CARTESIAN_POINT ( 'NONE',  ( -11.86301030670000145, 1432.114658971819836, 150.3940075513980048 ) ) ;
#32067 = CARTESIAN_POINT ( 'NONE',  ( 19.02704169900689735, 1456.915441405320053, 225.6706379604710264 ) ) ;
#32068 = CARTESIAN_POINT ( 'NONE',  ( -55.15130194409999831, 1379.936376805820146, 253.2598301361589961 ) ) ;
#32069 = CARTESIAN_POINT ( 'NONE',  ( 3.149355032655189568, 1421.363409079380062, 147.6430073452349916 ) ) ;
#32070 = CARTESIAN_POINT ( 'NONE',  ( 16.73628186595820466, 1526.382868172864164, 184.0591879540915841 ) ) ;
#32071 = CARTESIAN_POINT ( 'NONE',  ( 11.74267738989999899, 1446.506701540040012, 187.7371936343980110 ) ) ;
#32073 = CARTESIAN_POINT ( 'NONE',  ( -8.160972540127728436, 1423.396019259317200, 139.1420364792214457 ) ) ;
#32072 = CARTESIAN_POINT ( 'NONE',  ( -20.43674167330000202, 1495.372756435230258, 227.5904186109980003 ) ) ;
#32074 = CARTESIAN_POINT ( 'NONE',  ( 6.575517168109999311, 1463.094441317690098, 208.8281860452259764 ) ) ;
#32075 = CIRCLE ( 'NONE', #94647, 24.94174191160003318 ) ;
#32076 = EDGE_LOOP ( 'NONE', ( #68817, #999 ) ) ;
#32077 = CARTESIAN_POINT ( 'NONE',  ( 4.997250153905000047, 1516.727068157269969, 205.8570671527170077 ) ) ;
#32078 = CARTESIAN_POINT ( 'NONE',  ( 6.132762384200000305, 1406.804540994629861, 269.4856206602979682 ) ) ;
#32079 = CARTESIAN_POINT ( 'NONE',  ( 0.2331116816730000041, 1408.921200826630184, 186.4825379344979694 ) ) ;
#32080 = B_SPLINE_CURVE_WITH_KNOTS ( 'NONE', 3,
 ( #37842, #82600, #108897, #92092, #99928, #23772, #14824, #58508, #108347, #109459, #101574, #15911, #49011, #32188 ),
 .UNSPECIFIED., .F., .F.,
 ( 4, 2, 2, 2, 2, 2, 4 ),
 ( 0.000000000000000000, 0.2500000000000011657, 0.3750000000000017764, 0.5000000000000023315, 0.6250000000000028866, 0.7500000000000035527, 1.000000000000000000 ),
 .UNSPECIFIED. ) ;
#32081 = CARTESIAN_POINT ( 'NONE',  ( 22.08950919660000167, 1410.866032929729954, 203.5800407805880070 ) ) ;
#32082 = EDGE_CURVE ( 'NONE', #57781, #19417, #109478, .T. ) ;
#32083 = CARTESIAN_POINT ( 'NONE',  ( 23.87292829602066391, 1435.060528072440775, 214.1385913967735917 ) ) ;
#32084 = CARTESIAN_POINT ( 'NONE',  ( -9.179967000164252156, 1389.194332180375795, 217.4405442298740354 ) ) ;
#32085 = DIRECTION ( 'NONE',  ( -1.000000000000000000, 1.110223024625156540E-13, 0.000000000000000000 ) ) ;
#32086 = CARTESIAN_POINT ( 'NONE',  ( 15.80576098240000071, 1459.642315333929901, 231.7528682457979983 ) ) ;
#32087 = CARTESIAN_POINT ( 'NONE',  ( -3.440623305239999929, 1458.093607836889760, 219.2469823057990084 ) ) ;
#32088 = AXIS2_PLACEMENT_3D ( 'NONE', #41870, #33447, #25044 ) ;
#32089 = CARTESIAN_POINT ( 'NONE',  ( -1.835536242490369840, 1450.383119622699951, 182.7750508701979868 ) ) ;
#32090 = ADVANCED_FACE ( 'NONE', ( #20598 ), #100512, .T. ) ;
#32091 = CARTESIAN_POINT ( 'NONE',  ( 1.976367954473379873, 1450.328871374169921, 155.3359367358600309 ) ) ;
#32092 = CARTESIAN_POINT ( 'NONE',  ( -5.445054425793269814, 1494.866999379700246, 198.0707246423999948 ) ) ;
#32093 = CARTESIAN_POINT ( 'NONE',  ( -12.31987546767580000, 1378.182896808870055, 209.4394671972719948 ) ) ;
#32094 = CARTESIAN_POINT ( 'NONE',  ( -10.37541004874250028, 1409.275377690029927, 198.3562446834129958 ) ) ;
#32095 = B_SPLINE_SURFACE_WITH_KNOTS ( 'NONE', 5, 5, ( 
 ( #23058, #82443, #29280, #48303, #81874, #81320, #82986, #80795, #38225 ),
 ( #4634, #29828, #37684, #106539, #4101, #91395, #72408, #56136, #57268 ),
 ( #47194, #48860, #14672, #71889, #89187, #55610, #106004, #98681, #63475 ),
 ( #99768, #72948, #13008, #97594, #38772, #64563, #55060, #12479, #13553 ),
 ( #107084, #89734, #46662, #5741, #64014, #98125, #30373, #21943, #90271 ),
 ( #47739, #73505, #5176, #39332, #39884, #107640, #30923, #65102, #99214 ) ),
 .UNSPECIFIED., .F., .F., .F.,
 ( 6, 6 ),
 ( 6, 3, 6 ),
 ( 39.30566959800000149, 56.26181209559999985 ),
 ( 0.000000000000000000, 1.000000000000000000, 2.000000000000000000 ),
 .UNSPECIFIED. ) ;
#32096 = CARTESIAN_POINT ( 'NONE',  ( 19.77969251879999746, 1507.818093401829856, 229.2755605921979907 ) ) ;
#32097 = CARTESIAN_POINT ( 'NONE',  ( 2.499999995770000094, 1440.150490393029941, 165.1395456438979750 ) ) ;
#32098 = CARTESIAN_POINT ( 'NONE',  ( -6.179141267909999513, 1475.525926640629905, 266.9460417852980072 ) ) ;
#32099 = CARTESIAN_POINT ( 'NONE',  ( -4.234073038696310576, 1446.327642199189995, 164.0207583150770176 ) ) ;
#32100 = CARTESIAN_POINT ( 'NONE',  ( -20.99468044909999875, 1509.712668440929974, 187.9191382749980050 ) ) ;
#32101 = CARTESIAN_POINT ( 'NONE',  ( -11.21638122688047368, 1414.413060387330006, 208.4170904300009113 ) ) ;
#32102 = CARTESIAN_POINT ( 'NONE',  ( -46.75536493990070142, 1384.755724536759772, 255.0759030878719784 ) ) ;
#32103 = CARTESIAN_POINT ( 'NONE',  ( -106.5401037502859936, 1391.913060387289988, 302.9983041365559870 ) ) ;
#32104 = AXIS2_PLACEMENT_3D ( 'NONE', #74359, #95969, #46150 ) ;
#32105 = CARTESIAN_POINT ( 'NONE',  ( 12.21876415499199986, 1416.384967872819971, 223.5297635905479865 ) ) ;
#32106 = B_SPLINE_SURFACE_WITH_KNOTS ( 'NONE', 5, 1, ( 
 ( #100670, #41881 ),
 ( #109641, #92279 ),
 ( #15548, #7181 ),
 ( #76040, #41338 ),
 ( #67658, #101766 ),
 ( #53061, #60351 ) ),
 .UNSPECIFIED., .F., .F., .F.,
 ( 6, 6 ),
 ( 2, 2 ),
 ( 0.000000000000000000, 4.002909968980000066 ),
 ( 8.881784197000000007E-16, 14.00000000000000000 ),
 .UNSPECIFIED. ) ;
#32107 = CARTESIAN_POINT ( 'NONE',  ( -24.04648193933079980, 1444.796109374620073, 212.0322675289330050 ) ) ;
#32108 = CARTESIAN_POINT ( 'NONE',  ( 31.12456774391174008, 1525.960063244516959, 217.0912716842395582 ) ) ;
#32109 = CARTESIAN_POINT ( 'NONE',  ( 7.894434426187861398, 1512.053483454368461, 206.1275301515672709 ) ) ;
#32110 = CARTESIAN_POINT ( 'NONE',  ( 4.229167303610000594, 1436.983388288790138, 227.1518914930990150 ) ) ;
#32111 = CARTESIAN_POINT ( 'NONE',  ( -15.03580570476699840, 1422.460868293147996, 229.1221787420450084 ) ) ;
#32112 = AXIS2_PLACEMENT_3D ( 'NONE', #107996, #74979, #40247 ) ;
#32113 = CARTESIAN_POINT ( 'NONE',  ( 9.786977753351113307, 1519.551704408389924, 226.9642986349141722 ) ) ;
#32114 = EDGE_LOOP ( 'NONE', ( #78237, #79145 ) ) ;
#32115 = B_SPLINE_SURFACE_WITH_KNOTS ( 'NONE', 5, 5, ( 
 ( #48894, #31505, #74636, #40461, #81907, #5212 ),
 ( #39366, #49435, #108771, #32065, #66254, #100373 ),
 ( #23658, #82477, #83557, #107675, #65135, #38257 ),
 ( #99248, #22525, #56727, #8500, #60601, #24734 ),
 ( #84114, #58931, #102005, #33702, #84659, #76830 ),
 ( #85210, #16336, #49977, #16879, #41578, #50535 ),
 ( #60044, #92508, #144, #66798, #7959, #42126 ),
 ( #76274, #6850, #75734, #109878, #33157, #7413 ),
 ( #110423, #41011, #67897, #94722, #93601, #9067 ) ),
 .UNSPECIFIED., .F., .F., .F.,
 ( 6, 3, 6 ),
 ( 6, 6 ),
 ( 0.000000000000000000, 4.751561961960000247, 10.41361588720000064 ),
 ( 0.000000000000000000, 1.000000000000000000 ),
 .UNSPECIFIED. ) ;
#32116 = LINE ( 'NONE', #14753, #7014 ) ;
#32117 = CARTESIAN_POINT ( 'NONE',  ( -13.59471078833350077, 1507.829393183870025, 209.3810580891559994 ) ) ;
#32118 = CARTESIAN_POINT ( 'NONE',  ( -2.775555821678710178, 1468.867611629940257, 187.4507004058289965 ) ) ;
#32120 = CARTESIAN_POINT ( 'NONE',  ( -12.81053755176069942, 1379.345370588119977, 211.6929659203159986 ) ) ;
#32119 = CARTESIAN_POINT ( 'NONE',  ( 11.33800672749999983, 1425.544273751829905, 137.4271120788979772 ) ) ;
#32121 = CARTESIAN_POINT ( 'NONE',  ( 16.50400130224765149, 1525.907212628473644, 236.2546788475581252 ) ) ;
#32122 = CIRCLE ( 'NONE', #91101, 1.000000000000085043 ) ;
#32123 = CARTESIAN_POINT ( 'NONE',  ( -119.0092909768300018, 1350.849221539110204, 301.1574763303589748 ) ) ;
#32124 = CARTESIAN_POINT ( 'NONE',  ( -5.349442052910000633, 1454.859441816789968, 201.3532327490590035 ) ) ;
#32125 = CARTESIAN_POINT ( 'NONE',  ( -4.036748876935000396, 1516.667393516340098, 202.1854475764570225 ) ) ;
#32126 = CARTESIAN_POINT ( 'NONE',  ( 10.96966286673369950, 1432.359740019160199, 151.7701370213850112 ) ) ;
#32127 = CARTESIAN_POINT ( 'NONE',  ( -11.86359345204703786, 1398.264825172677774, 203.8060210069523350 ) ) ;
#32128 = CARTESIAN_POINT ( 'NONE',  ( 15.40521415373500069, 1513.907445464720013, 194.0960529043670135 ) ) ;
#32129 = CARTESIAN_POINT ( 'NONE',  ( -17.02234413428539739, 1420.211165650439852, 204.6962164606919998 ) ) ;
#32130 = FACE_OUTER_BOUND ( 'NONE', #98541, .T. ) ;
#32131 = CARTESIAN_POINT ( 'NONE',  ( 20.57820410168999814, 1507.771244142579917, 228.0150965724730270 ) ) ;
#32133 = ORIENTED_EDGE ( 'NONE', *, *, #67238, .F. ) ;
#32132 = CARTESIAN_POINT ( 'NONE',  ( -47.95030196609049966, 1379.684879134860012, 241.5716482886410006 ) ) ;
#32134 = ORIENTED_EDGE ( 'NONE', *, *, #77, .T. ) ;
#32135 = CARTESIAN_POINT ( 'NONE',  ( 12.00222499182989999, 1433.736528012170083, 150.1432766994780081 ) ) ;
#32136 = CARTESIAN_POINT ( 'NONE',  ( -13.13104840879999990, 1397.401700877830081, 207.3834689486880052 ) ) ;
#32137 = CARTESIAN_POINT ( 'NONE',  ( -20.09807828239999949, 1410.109999577329745, 220.1458087410979942 ) ) ;
#32138 = ORIENTED_EDGE ( 'NONE', *, *, #13231, .T. ) ;
#32139 = CARTESIAN_POINT ( 'NONE',  ( -13.45615543559949145, 1444.281848265668714, 169.3621925482611346 ) ) ;
#32140 = DIRECTION ( 'NONE',  ( -5.980589973904019347E-17, 1.000000000000000000, -1.736889445713099699E-16 ) ) ;
#32142 = CARTESIAN_POINT ( 'NONE',  ( -13.70995644358860055, 1507.826637856930120, 184.2436392040419832 ) ) ;
#32141 = CARTESIAN_POINT ( 'NONE',  ( 2.919790884400000230, 1445.755750970590043, 200.1990502211790215 ) ) ;
#32143 = CARTESIAN_POINT ( 'NONE',  ( 3.809409616780000007, 1468.703253529829908, 183.3440034161980066 ) ) ;
#32144 = CARTESIAN_POINT ( 'NONE',  ( -4.591854502347329614, 1463.586371817870031, 200.3131754724250015 ) ) ;
#32145 = CARTESIAN_POINT ( 'NONE',  ( -17.50950631050429962, 1417.908328417909843, 206.9179188249679839 ) ) ;
#32146 = CARTESIAN_POINT ( 'NONE',  ( 8.906967729100440323, 1396.224098604110168, 202.5685376797749768 ) ) ;
#32147 = CARTESIAN_POINT ( 'NONE',  ( 1.549353400650000046, 1416.067629296030191, 190.3885695989980036 ) ) ;
#32148 = CARTESIAN_POINT ( 'NONE',  ( 11.18838110630000138, 1425.436776285730048, 146.8505530396979850 ) ) ;
#32149 = CARTESIAN_POINT ( 'NONE',  ( 16.68463225901000158, 1442.773887286389936, 162.0935120915889911 ) ) ;
#32150 = ORIENTED_EDGE ( 'NONE', *, *, #4208, .T. ) ;
#32151 = CARTESIAN_POINT ( 'NONE',  ( 13.27152677196249897, 1435.087436992850144, 149.8492268114800368 ) ) ;
#32152 = VERTEX_POINT ( 'NONE', #63754 ) ;
#32153 = EDGE_LOOP ( 'NONE', ( #83326, #88193, #10059, #105435, #48482 ) ) ;
#32154 = CARTESIAN_POINT ( 'NONE',  ( 13.51610093809999924, 1443.913060387330006, 169.3501091259980171 ) ) ;
#32155 = CARTESIAN_POINT ( 'NONE',  ( -6.996308864409999551, 1463.880774057229928, 235.8431045883980062 ) ) ;
#32156 = CIRCLE ( 'NONE', #94734, 477.3522486052488034 ) ;
#32157 = CARTESIAN_POINT ( 'NONE',  ( -106.9654571391928641, 1390.307193624053525, 308.7685348267781933 ) ) ;
#32158 = CARTESIAN_POINT ( 'NONE',  ( -7.715625241105000143, 1516.786099423779888, 215.6766101314970001 ) ) ;
#32159 = CARTESIAN_POINT ( 'NONE',  ( -8.353227804513524646, 1511.405761256387450, 213.6090188832756667 ) ) ;
#32160 = ORIENTED_EDGE ( 'NONE', *, *, #58849, .T. ) ;
#32161 = CARTESIAN_POINT ( 'NONE',  ( -11.68017202480000094, 1503.190160464489963, 208.0141257398589971 ) ) ;
#32162 = CARTESIAN_POINT ( 'NONE',  ( 2.500000000000000000, 1448.206572385129903, 168.0224266773309978 ) ) ;
#32163 = CARTESIAN_POINT ( 'NONE',  ( -58.56722970770000103, 1379.895658628519868, 258.8926058799589782 ) ) ;
#32164 = EDGE_CURVE ( 'NONE', #106220, #3217, #105887, .T. ) ;
#32165 = VERTEX_POINT ( 'NONE', #105191 ) ;
#32166 = CARTESIAN_POINT ( 'NONE',  ( 0.7355686427760019797, 1517.012231669750008, 205.8548062402470009 ) ) ;
#32167 = ORIENTED_EDGE ( 'NONE', *, *, #107501, .F. ) ;
#32168 = CARTESIAN_POINT ( 'NONE',  ( -5.786847777804999815, 1517.104497701820037, 208.3841784293060186 ) ) ;
#32169 = DIRECTION ( 'NONE',  ( -6.123233995736769734E-17, -1.000000000000000000, -1.124819836996399911E-32 ) ) ;
#32170 = EDGE_CURVE ( 'NONE', #38319, #69349, #64768, .T. ) ;
#32172 = EDGE_CURVE ( 'NONE', #4923, #45986, #71952, .T. ) ;
#32171 = CARTESIAN_POINT ( 'NONE',  ( -35.06679765450265052, 1424.124224229928814, 269.5324321545449493 ) ) ;
#32173 = CARTESIAN_POINT ( 'NONE',  ( 6.610870897525000345, 1511.929989569699956, 216.5045975180869959 ) ) ;
#32175 = VERTEX_POINT ( 'NONE', #100622 ) ;
#32174 = CARTESIAN_POINT ( 'NONE',  ( -1.674829163958580169, 1414.913060387399810, 226.0541986821700107 ) ) ;
#32176 = CARTESIAN_POINT ( 'NONE',  ( -9.822264486677861081E-06, 1450.913060148159957, 181.2410907034809782 ) ) ;
#32177 = CARTESIAN_POINT ( 'NONE',  ( -31.17697957079580107, 1440.913060388259964, 241.8836480397630169 ) ) ;
#32178 = CARTESIAN_POINT ( 'NONE',  ( -38.54974011449999693, 1384.147589378169869, 239.2788492578590080 ) ) ;
#32179 = CARTESIAN_POINT ( 'NONE',  ( 21.03867822700000190, 1494.819670719790111, 208.4793431422329775 ) ) ;
#32180 = B_SPLINE_CURVE_WITH_KNOTS ( 'NONE', 5,
 ( #87028, #44492, #1952, #70274, #34420, #80297, #81928, #64062, #3612 ),
 .UNSPECIFIED., .F., .F.,
 ( 6, 3, 6 ),
 ( 429.4216791289999833, 432.6128460950000090, 434.5419185690000177 ),
 .UNSPECIFIED. ) ;
#32181 = CARTESIAN_POINT ( 'NONE',  ( 6.501109236959999649, 1407.992916451829842, 270.1283629016979830 ) ) ;
#32182 = CARTESIAN_POINT ( 'NONE',  ( -4.998515195425000002, 1516.787536375099990, 213.1617432482970003 ) ) ;
#32183 = CARTESIAN_POINT ( 'NONE',  ( 23.57777505329999812, 1409.993680146930046, 209.2866710572280056 ) ) ;
#32184 = CARTESIAN_POINT ( 'NONE',  ( -20.87372870449999951, 1509.581281395429869, 188.4712523506979949 ) ) ;
#32185 = CARTESIAN_POINT ( 'NONE',  ( 11.90847486998620042, 1492.860655245649923, 212.4217341398910150 ) ) ;
#32186 = CARTESIAN_POINT ( 'NONE',  ( 7.508704985436030377, 1508.884117426709963, 214.6350462372689947 ) ) ;
#32187 = CARTESIAN_POINT ( 'NONE',  ( 5.789394662204999875, 1517.164987839469859, 210.8286437561770299 ) ) ;
#32188 = CARTESIAN_POINT ( 'NONE',  ( -2.500574544111449971, 1448.942056179399970, 154.5733147259969940 ) ) ;
#32189 = CARTESIAN_POINT ( 'NONE',  ( 0.4756500442839999843, 1418.694808079630093, 184.7107058538980198 ) ) ;
#32190 = CARTESIAN_POINT ( 'NONE',  ( 3.515215440921866552, 1419.856978125559863, 137.0999999980978430 ) ) ;
#32192 = ORIENTED_EDGE ( 'NONE', *, *, #96276, .T. ) ;
#32191 = CARTESIAN_POINT ( 'NONE',  ( -47.38272174249999580, 1385.138016709929843, 256.2741787814589998 ) ) ;
#32193 = CARTESIAN_POINT ( 'NONE',  ( -50.04085626606729420, 1385.121777519389980, 261.8108732571790256 ) ) ;
#32194 = CIRCLE ( 'NONE', #73279, 1.000060826959960236 ) ;
#32195 = B_SPLINE_SURFACE_WITH_KNOTS ( 'NONE', 5, 5, ( 
 ( #38447, #31697, #40102, #5401, #81010, #98356 ),
 ( #82103, #21628, #14887, #57485, #98902, #6502 ),
 ( #74284, #108414, #40656, #74828, #4843, #65880 ),
 ( #14337, #73734, #107857, #55834, #81542, #56921 ),
 ( #100001, #23289, #89413, #31146, #91051, #89955 ),
 ( #48526, #107311, #91610, #49078, #55283, #13229 ) ),
 .UNSPECIFIED., .F., .F., .F.,
 ( 6, 6 ),
 ( 6, 6 ),
 ( 5.133465978379999406, 14.11476443669999981 ),
 ( 0.000000000000000000, 2.000000000000000000 ),
 .UNSPECIFIED. ) ;
#32196 = CARTESIAN_POINT ( 'NONE',  ( 17.60616633871843106, 1410.892144412839798, 225.1414472891892729 ) ) ;
#32197 = CARTESIAN_POINT ( 'NONE',  ( -3.870244853708171284, 1370.348070663988892, 209.9344813661604974 ) ) ;
#32198 = EDGE_CURVE ( 'NONE', #39621, #83528, #33982, .T. ) ;
#32199 =( BOUNDED_CURVE ( )  B_SPLINE_CURVE ( 3, ( #107077, #64553, #11924, #46104 ),
 .UNSPECIFIED., .F., .F. ) 
 B_SPLINE_CURVE_WITH_KNOTS ( ( 4, 4 ),
 ( 0.9985734095396142651, 2.143019256287069574 ),
 .UNSPECIFIED. ) 
 CURVE ( )  GEOMETRIC_REPRESENTATION_ITEM ( )  RATIONAL_B_SPLINE_CURVE ( ( 1.000000000000000000, 0.8937995569179151278, 0.8937995569179151278, 1.000000000000000000 ) ) 
 REPRESENTATION_ITEM ( '' )  );
#32200 = CARTESIAN_POINT ( 'NONE',  ( -6.733539913119999554, 1418.366792801529982, 233.9669031324980040 ) ) ;
#32201 = CARTESIAN_POINT ( 'NONE',  ( 5.027849746001829878, 1485.388521802679861, 218.6205834690780136 ) ) ;
#32202 = CARTESIAN_POINT ( 'NONE',  ( -24.03284404440000088, 1444.467324254849927, 212.3598065616679946 ) ) ;
#32203 = CARTESIAN_POINT ( 'NONE',  ( 1.513089995879569383, 1498.833490213426558, 197.8872906115371109 ) ) ;
#32204 = B_SPLINE_CURVE_WITH_KNOTS ( 'NONE', 5,
 ( #95967, #54551, #62399, #97081, #63508, #68169 ),
 .UNSPECIFIED., .F., .F.,
 ( 6, 6 ),
 ( 0.000000000000000000, 1.000000000000000000 ),
 .UNSPECIFIED. ) ;
#32206 = DIRECTION ( 'NONE',  ( 1.387778780781444413E-14, 0.000000000000000000, 1.000000000000000000 ) ) ;
#32205 = CARTESIAN_POINT ( 'NONE',  ( 3.454119916704999849, 1516.594591938570147, 216.8324563732270178 ) ) ;
#32207 = PLANE ( 'NONE',  #22746 ) ;
#32208 = CARTESIAN_POINT ( 'NONE',  ( 32.41382812665953139, 1525.581535527370988, 220.2604433702309734 ) ) ;
#32209 = ORIENTED_EDGE ( 'NONE', *, *, #99232, .T. ) ;
#32210 = CARTESIAN_POINT ( 'NONE',  ( -0.7538707734179979081, 1516.719999691880048, 202.1833671473370089 ) ) ;
#32211 = CARTESIAN_POINT ( 'NONE',  ( -16.85261136226499801, 1513.023086264660151, 222.3204897471670165 ) ) ;
#32212 = CIRCLE ( 'NONE', #7198, 28.99999999999999645 ) ;
#32213 = CARTESIAN_POINT ( 'NONE',  ( 14.46822985410000051, 1463.223607397130081, 223.0618228778980097 ) ) ;
#32214 = CARTESIAN_POINT ( 'NONE',  ( 19.24972504899999848, 1455.799292141330170, 225.3448411794979904 ) ) ;
#32215 = CARTESIAN_POINT ( 'NONE',  ( 10.84428623605119846, 1461.742173074219863, 210.7892283924740013 ) ) ;
#32216 = LINE ( 'NONE', #50138, #71756 ) ;
#32217 = CARTESIAN_POINT ( 'NONE',  ( 4.575325728500000189, 1466.769487727290198, 218.0849816997290134 ) ) ;
#32218 = DIRECTION ( 'NONE',  ( 0.03489949670250328678, -0.9993908270190956511, 0.000000000000000000 ) ) ;
#32219 = CARTESIAN_POINT ( 'NONE',  ( 40.25496866969060505, 1444.330520920399977, 137.0766690124500258 ) ) ;
#32220 = CARTESIAN_POINT ( 'NONE',  ( -20.26396079519999915, 1427.262199077629930, 222.0222826655979702 ) ) ;
#32221 = CARTESIAN_POINT ( 'NONE',  ( 8.033473906835755685, 1487.403589905162789, 201.8500708422530749 ) ) ;
#32222 = CARTESIAN_POINT ( 'NONE',  ( -107.0237318669999951, 1390.464738565959806, 299.4840498548589949 ) ) ;
#32223 = EDGE_CURVE ( 'NONE', #95777, #74589, #69264, .T. ) ;
#32224 = CARTESIAN_POINT ( 'NONE',  ( -16.93636994520000272, 1413.292055451130182, 226.4943808309979829 ) ) ;
#32225 = B_SPLINE_CURVE_WITH_KNOTS ( 'NONE', 5,
 ( #97474, #105327, #62822, #20203, #54402, #88534, #105889, #3439, #29168 ),
 .UNSPECIFIED., .F., .F.,
 ( 6, 3, 6 ),
 ( 0.000000000000000000, 0.5000000000000000000, 1.000000000000000000 ),
 .UNSPECIFIED. ) ;
#32226 = CARTESIAN_POINT ( 'NONE',  ( 20.21716934225348439, 1526.104292489126465, 184.5497256588712105 ) ) ;
#32227 = CARTESIAN_POINT ( 'NONE',  ( -24.21249802766532255, 1465.849153120822621, 269.4183097923577179 ) ) ;
#32228 = ORIENTED_EDGE ( 'NONE', *, *, #43333, .F. ) ;
#32229 = CARTESIAN_POINT ( 'NONE',  ( 1.628202555219999903, 1430.465083930730088, 150.2970716576980124 ) ) ;
#32230 = CARTESIAN_POINT ( 'NONE',  ( -42.57897977376345011, 1428.602532329936821, 269.0600478115077294 ) ) ;
#32231 = CARTESIAN_POINT ( 'NONE',  ( 3.439855069772169809E-11, 1452.913060387330006, 150.8032249182200246 ) ) ;
#32232 = CARTESIAN_POINT ( 'NONE',  ( -5.668006973570000717, 1484.831902833290087, 198.6468248041990137 ) ) ;
#32233 = CIRCLE ( 'NONE', #64467, 29.84605316859531143 ) ;
#32234 = CARTESIAN_POINT ( 'NONE',  ( -0.1142305270560000086, 1416.107866688329977, 233.5491553016980220 ) ) ;
#32235 = CARTESIAN_POINT ( 'NONE',  ( -13.33531041039106668, 1443.287836672654976, 186.9550018447848743 ) ) ;
#32236 = B_SPLINE_SURFACE_WITH_KNOTS ( 'NONE', 5, 5, ( 
 ( #4736, #97153, #12043, #38334, #96608, #79263 ),
 ( #70889, #72514, #88760, #107202, #106105, #13118 ),
 ( #37251, #47301, #38879, #63047, #30490, #46226 ),
 ( #96045, #87660, #19316, #2573, #36695, #37803 ),
 ( #105004, #28292, #54084, #55175, #88209, #11503 ),
 ( #63583, #89301, #73624, #57924, #107754, #58468 ) ),
 .UNSPECIFIED., .F., .F., .F.,
 ( 6, 6 ),
 ( 6, 6 ),
 ( 6.379889989409999629, 6.971779114740000338 ),
 ( 0.000000000000000000, 1.455840041380000116 ),
 .UNSPECIFIED. ) ;
#32237 = CARTESIAN_POINT ( 'NONE',  ( -8.671125672311569943, 1437.958062009570085, 208.7129840011259887 ) ) ;
#32238 = CARTESIAN_POINT ( 'NONE',  ( 5.257080573758897479, 1522.051704408389924, 218.9984329930441618 ) ) ;
#32239 = PLANE ( 'NONE',  #100362 ) ;
#32240 = CARTESIAN_POINT ( 'NONE',  ( -37.79051013476979648, 1445.035584066110005, 137.0421779799580122 ) ) ;
#32241 = CARTESIAN_POINT ( 'NONE',  ( 23.61230407060000047, 1435.322065071379939, 137.2857908826979951 ) ) ;
#32242 = CARTESIAN_POINT ( 'NONE',  ( -13.14246787946174422, 1443.061742832075879, 169.3995334515947491 ) ) ;
#32244 = ORIENTED_EDGE ( 'NONE', *, *, #78050, .T. ) ;
#32243 = CARTESIAN_POINT ( 'NONE',  ( -14.66467552210000136, 1409.425162140929842, 225.2836404500980052 ) ) ;
#32245 = AXIS2_PLACEMENT_3D ( 'NONE', #26057, #8164, #94370 ) ;
#32246 = CARTESIAN_POINT ( 'NONE',  ( 0.6362176846909819439, 1414.913060387399810, 192.9136500303789887 ) ) ;
#32247 = CARTESIAN_POINT ( 'NONE',  ( 21.95659374958953691, 1509.539900942172380, 226.8505570154440534 ) ) ;
#32248 = ORIENTED_EDGE ( 'NONE', *, *, #11107, .T. ) ;
#32249 = EDGE_LOOP ( 'NONE', ( #37422, #25394, #23950, #39271, #88684, #7719, #54305, #16826, #64403 ) ) ;
#32250 = CARTESIAN_POINT ( 'NONE',  ( 16.70118312301820040, 1414.971390223319986, 209.2094541707220117 ) ) ;
#32251 = CARTESIAN_POINT ( 'NONE',  ( -8.862056518773441027, 1384.892951007370129, 218.6851137863439760 ) ) ;
#32253 = CARTESIAN_POINT ( 'NONE',  ( -19.28618930569999890, 1452.501336721830057, 211.9649570637480167 ) ) ;
#32252 = CARTESIAN_POINT ( 'NONE',  ( -11.68426330212614417, 1428.980873612041023, 140.1562216286908154 ) ) ;
#32254 = CARTESIAN_POINT ( 'NONE',  ( -2.975911813860000255, 1445.219193664589966, 217.6412520525290120 ) ) ;
#32255 = CARTESIAN_POINT ( 'NONE',  ( -11.03393269049999859, 1433.573953115969971, 151.7352805125980240 ) ) ;
#32256 = EDGE_CURVE ( 'NONE', #32684, #43726, #64825, .T. ) ;
#32257 = CARTESIAN_POINT ( 'NONE',  ( 2.220446049249999755E-16, 1516.051704408390151, 209.1218459616989946 ) ) ;
#32258 = EDGE_CURVE ( 'NONE', #67278, #43673, #78022, .T. ) ;
#32259 = CARTESIAN_POINT ( 'NONE',  ( 13.58235846979999906, 1416.828040475229955, 196.3349388281980055 ) ) ;
#32260 = CARTESIAN_POINT ( 'NONE',  ( -11.80119706069999985, 1415.163755984130148, 195.8322853899979918 ) ) ;
#32261 = CARTESIAN_POINT ( 'NONE',  ( -3.782764153885679992, 1454.025518203000047, 199.3518729501290068 ) ) ;
#32262 = CARTESIAN_POINT ( 'NONE',  ( -11.47171006529080017, 1480.905530949450167, 211.9467558702930035 ) ) ;
#32263 = CARTESIAN_POINT ( 'NONE',  ( 9.454737631249999552, 1363.431170718789872, 207.6218459616989946 ) ) ;
#32264 = CARTESIAN_POINT ( 'NONE',  ( -14.43289921072090110, 1509.539432542180066, 182.8218189571549885 ) ) ;
#32266 = ORIENTED_EDGE ( 'NONE', *, *, #3648, .F. ) ;
#32265 = CARTESIAN_POINT ( 'NONE',  ( -1.875238357586299756E-09, 1416.153069931509890, 240.2634071211490152 ) ) ;
#32267 = VERTEX_POINT ( 'NONE', #67605 ) ;
#32268 = CARTESIAN_POINT ( 'NONE',  ( -11.81434188762340121, 1428.975514852789956, 148.8502864864200035 ) ) ;
#32269 = CARTESIAN_POINT ( 'NONE',  ( 0.03745370349719699676, 1502.433616705189934, 233.2734988771990174 ) ) ;
#32270 = CARTESIAN_POINT ( 'NONE',  ( -4.801572058700000589, 1471.236463740830231, 269.3376025177980182 ) ) ;
#32271 = CARTESIAN_POINT ( 'NONE',  ( -110.0632822187059929, 1384.922692771400079, 296.9512106417570294 ) ) ;
#32272 = CARTESIAN_POINT ( 'NONE',  ( -126.6653580271998862, 1320.102705746891161, 300.8346439529095164 ) ) ;
#32273 = CARTESIAN_POINT ( 'NONE',  ( -9.902323404119773187, 1422.657237248887441, 210.6700027881538233 ) ) ;
#32274 = AXIS2_PLACEMENT_3D ( 'NONE', #48119, #13932, #82258 ) ;
#32275 = CARTESIAN_POINT ( 'NONE',  ( -13.97867491850210087, 1429.402194067919709, 222.2970902837259928 ) ) ;
#32276 = CARTESIAN_POINT ( 'NONE',  ( -20.53044877720000372, 1484.405134138590029, 211.1019867995989898 ) ) ;
#32277 = B_SPLINE_SURFACE_WITH_KNOTS ( 'NONE', 5, 5, ( 
 ( #37810, #73631, #30497, #13669, #64686, #90391, #40004, #13125, #108313 ),
 ( #106112, #82571, #56815, #47309, #80914, #98804, #47858, #72520, #90953 ),
 ( #14239, #63590, #48429, #65775, #20429, #88767, #20979, #55183, #4210 ),
 ( #12605, #23190, #84208, #15876, #24293, #33801, #51171, #6409, #109430 ),
 ( #15335, #92062, #83115, #6949, #33251, #240, #41666, #75284, #16972 ),
 ( #101540, #92602, #110519, #74728, #66343, #108862, #76369, #75823, #7504 ),
 ( #100997, #57390, #48982, #57930, #24829, #100459, #50078, #109974, #8050 ),
 ( #14796, #58475, #67995, #102107, #32707, #85299, #59034, #32155, #23742 ),
 ( #93158, #49530, #83655, #67441, #50620, #8598, #91516, #16428, #41106 ),
 ( #40555, #25386, #42770, #66888, #84753, #42218, #59579, #93692, #76931 ),
 ( #34368, #99892, #10261, #43877, #96484, #44438, #70224, #61266, #79147 ),
 ( #17530, #34913, #60137, #78581, #3004, #27082, #1897, #18100, #11386 ),
 ( #95382, #78020, #51733, #783, #85868, #35468, #69098, #45558, #2458 ),
 ( #36034, #103199, #104328, #19764, #94256, #18646, #53966, #27622, #61808 ),
 ( #88099, #102641, #95930, #77483, #79698, #9170, #19190, #43335, #70772 ) ),
 .UNSPECIFIED., .F., .F., .F.,
 ( 6, 3, 3, 3, 6 ),
 ( 6, 3, 6 ),
 ( 76.61796729980000009, 89.38050170190000188, 98.82656461499999523, 108.2726275280000010, 112.1339374929999906 ),
 ( 0.000000000000000000, 1.000000000000000000, 2.000000000000000000 ),
 .UNSPECIFIED. ) ;
#32278 = CARTESIAN_POINT ( 'NONE',  ( -24.08426305480000451, 1411.115211393229856, 208.6111285346999864 ) ) ;
#32279 = LINE ( 'NONE', #12724, #28960 ) ;
#32280 = CARTESIAN_POINT ( 'NONE',  ( 11.88647226875623986, 1365.999781939073273, 209.6218459617033432 ) ) ;
#32281 = CARTESIAN_POINT ( 'NONE',  ( -37.60268983529039843, 1420.124584829160085, 267.2573160899880236 ) ) ;
#32282 = VERTEX_POINT ( 'NONE', #93874 ) ;
#32283 = CARTESIAN_POINT ( 'NONE',  ( 10.41177662488709998, 1460.024663752159995, 205.9063130872220029 ) ) ;
#32284 = EDGE_LOOP ( 'NONE', ( #45211, #57939, #106109 ) ) ;
#32285 = VERTEX_POINT ( 'NONE', #26112 ) ;
#32286 = CARTESIAN_POINT ( 'NONE',  ( 0.7576635334400020350, 1516.855632454399938, 211.9899581013969794 ) ) ;
#32287 = CARTESIAN_POINT ( 'NONE',  ( 38.71370889343818078, 1444.324653571829003, 136.9324510732293732 ) ) ;
#32288 = CARTESIAN_POINT ( 'NONE',  ( -2.470168521978398424, 1523.382868172864164, 175.3649660270905315 ) ) ;
#32289 = EDGE_CURVE ( 'NONE', #108583, #82581, #98752, .T. ) ;
#32291 = CARTESIAN_POINT ( 'NONE',  ( -17.63831374727218915, 1419.677598567774794, 207.0084533942130349 ) ) ;
#32290 = CARTESIAN_POINT ( 'NONE',  ( -3.253462098795000035, 1516.874084700499907, 212.5832060635069922 ) ) ;
#32292 = CARTESIAN_POINT ( 'NONE',  ( -14.71271264950000024, 1455.450119958330106, 188.4035724979979989 ) ) ;
#32293 = DIRECTION ( 'NONE',  ( 0.9455185755993178454, 0.000000000000000000, -0.3255681544571537578 ) ) ;
#32294 = ORIENTED_EDGE ( 'NONE', *, *, #63283, .T. ) ;
#32295 = CARTESIAN_POINT ( 'NONE',  ( -26.56630858009999940, 1435.444835103639889, 135.5553490494979769 ) ) ;
#32296 = EDGE_CURVE ( 'NONE', #40624, #35166, #26673, .T. ) ;
#32297 = ADVANCED_FACE ( 'NONE', ( #93328 ), #24458, .F. ) ;
#32298 = CARTESIAN_POINT ( 'NONE',  ( -4.618749106614999711, 1516.729202374750002, 202.5720834851169911 ) ) ;
#32299 = CARTESIAN_POINT ( 'NONE',  ( 10.95098223739999987, 1471.837422851889869, 212.3987393883689947 ) ) ;
#32300 = EDGE_CURVE ( 'NONE', #32175, #33852, #39774, .T. ) ;
#32301 = CARTESIAN_POINT ( 'NONE',  ( -34.79440155389130496, 1384.568141483509862, 208.5850534773520053 ) ) ;
#32302 = DIRECTION ( 'NONE',  ( 9.341989762165448955E-47, -1.000000000000000000, 1.836970198721029688E-16 ) ) ;
#32303 = AXIS2_PLACEMENT_3D ( 'NONE', #36536, #46619, #62324 ) ;
#32304 = CARTESIAN_POINT ( 'NONE',  ( 45.97228714287020068, 1578.884309444509881, 188.3086953514500124 ) ) ;
#32305 = CARTESIAN_POINT ( 'NONE',  ( 0.04898334450229999831, 1396.985963204730069, 196.3070572679980046 ) ) ;
#32307 = EDGE_LOOP ( 'NONE', ( #16789, #9686, #24084, #84049 ) ) ;
#32306 = CARTESIAN_POINT ( 'NONE',  ( 0.000000000000000000, 1502.413060387330006, 209.1218459616979999 ) ) ;
#32308 = ORIENTED_EDGE ( 'NONE', *, *, #94079, .F. ) ;
#32309 = CARTESIAN_POINT ( 'NONE',  ( 0.2178156354970000319, 1452.982786352329867, 183.2541304307979999 ) ) ;
#32310 = CARTESIAN_POINT ( 'NONE',  ( -28.72841836130151805, 1526.333389947941441, 220.1290250959031596 ) ) ;
#32311 = EDGE_CURVE ( 'NONE', #25245, #14800, #94420, .T. ) ;
#32312 = CARTESIAN_POINT ( 'NONE',  ( 4.138599669886909638, 1426.481420035549945, 191.5413917934459960 ) ) ;
#32313 = CARTESIAN_POINT ( 'NONE',  ( -23.85691843449999894, 1435.349182908609919, 137.3960071424980072 ) ) ;
#32314 = CARTESIAN_POINT ( 'NONE',  ( -24.67190123920000033, 1441.699982178919981, 210.7126285418079874 ) ) ;
#32315 = CARTESIAN_POINT ( 'NONE',  ( 2.299983577604999940, 1516.861367446839949, 211.4044688825970013 ) ) ;
#32316 = EDGE_CURVE ( 'NONE', #43735, #37252, #6031, .T. ) ;
#32317 = CARTESIAN_POINT ( 'NONE',  ( -0.1681681984989999989, 1416.866694505930127, 168.0175527136979667 ) ) ;
#32318 = CARTESIAN_POINT ( 'NONE',  ( -2.832196849119999804, 1497.533045831589789, 201.1364434386690050 ) ) ;
#32319 = CARTESIAN_POINT ( 'NONE',  ( 8.993477303732159811, 1437.143916695869848, 212.0776306990970284 ) ) ;
#32320 = CARTESIAN_POINT ( 'NONE',  ( -13.17906415938499975, 1414.913527275050001, 220.1406906569499995 ) ) ;
#32321 = B_SPLINE_CURVE_WITH_KNOTS ( 'NONE', 3,
 ( #30444, #12000, #97657, #37758, #29886, #54040, #96000, #71950, #19270, #53473, #87617, #10905, #45078, #46182, #80311, #104957, #72471, #3627, #62437, #28247, #96563, #21469, #12549, #46728, #2528, #63541, #106062, #19835, #70848, #80861, #4162, #38289, #88169, #55679, #64078, #11457, #45633, #79773, #22010 ),
 .UNSPECIFIED., .F., .F.,
 ( 4, 2, 2, 1, 1, 2, 2, 2, 2, 1, 1, 2, 2, 2, 2, 2, 1, 1, 1, 2, 2, 2, 4 ),
 ( 0.000000000000000000, 0.06250000000013596069, 0.09375000000020394797, 0.1093750000002379347, 0.1171875000002547407, 0.1210937500002617073, 0.1250000000002686462, 0.1875000000003115841, 0.2187500000003269607, 0.2343750000003285150, 0.2421875000003315404, 0.2460937500003291256, 0.2500000000003266831, 0.3750000000005528356, 0.4375000000006535328, 0.4687500000006948331, 0.4843750000007214784, 0.4921875000007256973, 0.4960937500007246426, 0.4980468750007239764, 0.5000000000007233103, 0.7500000000003617107, 1.000000000000000000 ),
 .UNSPECIFIED. ) ;
#32322 = CARTESIAN_POINT ( 'NONE',  ( -0.01265822594359850006, 1516.959716008189844, 207.4120794380770292 ) ) ;
#32323 = EDGE_LOOP ( 'NONE', ( #9633, #80343, #101392 ) ) ;
#32324 = FACE_OUTER_BOUND ( 'NONE', #73470, .T. ) ;
#32326 = ADVANCED_FACE ( 'NONE', ( #77105 ), #92780, .T. ) ;
#32325 = CARTESIAN_POINT ( 'NONE',  ( -8.628995479883890596, 1437.624223205020144, 208.3388049724410109 ) ) ;
#32327 = CARTESIAN_POINT ( 'NONE',  ( -13.36039414200000230, 1385.021583142659892, 218.9683482914990122 ) ) ;
#32328 = ORIENTED_EDGE ( 'NONE', *, *, #35703, .T. ) ;
#32330 = CIRCLE ( 'NONE', #60888, 1.999999999999999556 ) ;
#32329 = CARTESIAN_POINT ( 'NONE',  ( -8.178500771994089646, 1441.152429774469965, 153.9860759686779943 ) ) ;
#32331 = CARTESIAN_POINT ( 'NONE',  ( 13.04561791671889992, 1435.047968860360015, 150.0615661932069997 ) ) ;
#32332 = CARTESIAN_POINT ( 'NONE',  ( 14.00211218169999938, 1416.535385209229844, 196.4050012923980262 ) ) ;
#32333 = EDGE_CURVE ( 'NONE', #69866, #28257, #27223, .T. ) ;
#32334 = CARTESIAN_POINT ( 'NONE',  ( -9.306860583259998876, 1415.471543658610017, 206.2851672951890123 ) ) ;
#32335 = CARTESIAN_POINT ( 'NONE',  ( -11.32634609552117411, 1425.525426998061675, 138.7434885827603637 ) ) ;
#32336 = CARTESIAN_POINT ( 'NONE',  ( 2.817354810100396456, 1451.820641374121124, 183.8336154107607854 ) ) ;
#32337 = CARTESIAN_POINT ( 'NONE',  ( 5.247705765879999262, 1487.053368902190186, 199.5049302458390059 ) ) ;
#32338 = EDGE_CURVE ( 'NONE', #64407, #71213, #90274, .T. ) ;
#32339 = CARTESIAN_POINT ( 'NONE',  ( 2.393268998928310687, 1426.806556743500096, 139.9374969045731518 ) ) ;
#32340 = CARTESIAN_POINT ( 'NONE',  ( 24.66473933617894687, 1441.732816492871962, 212.5822908973776180 ) ) ;
#32341 = CARTESIAN_POINT ( 'NONE',  ( -13.74003952106156135, 1447.587101742432196, 195.3179347002435122 ) ) ;
#32342 = CARTESIAN_POINT ( 'NONE',  ( 7.718134629434999283, 1516.881930554049859, 216.4517759834270123 ) ) ;
#32343 = ORIENTED_EDGE ( 'NONE', *, *, #52925, .T. ) ;
#32344 = CARTESIAN_POINT ( 'NONE',  ( -12.70951029399999932, 1416.237488680629895, 195.9645815363980148 ) ) ;
#32345 = CARTESIAN_POINT ( 'NONE',  ( -16.50397793950000036, 1420.609998909190153, 203.2697724632589882 ) ) ;
#32346 = EDGE_CURVE ( 'NONE', #90692, #94444, #96660, .T. ) ;
#32347 = CARTESIAN_POINT ( 'NONE',  ( 1.166167165090000069, 1418.953384179930026, 184.8577940441979877 ) ) ;
#32348 = CARTESIAN_POINT ( 'NONE',  ( 10.11243515225062772, 1384.899971913130003, 216.4689601570715638 ) ) ;
#32349 = CARTESIAN_POINT ( 'NONE',  ( -17.15830831501837039, 1512.187213306747481, 209.3391145445735333 ) ) ;
#32350 = CARTESIAN_POINT ( 'NONE',  ( -11.26841194160630089, 1471.218450017450095, 207.2998296250100054 ) ) ;
#32351 = CARTESIAN_POINT ( 'NONE',  ( -5.004574234055505499, 1508.230405643570293, 220.4208381782240735 ) ) ;
#32352 = CARTESIAN_POINT ( 'NONE',  ( 18.58720762869999987, 1416.311719779230089, 209.7162280979700029 ) ) ;
#32353 = CARTESIAN_POINT ( 'NONE',  ( -2.690862365372829856, 1454.581388717919936, 198.9826033966560033 ) ) ;
#32354 = CARTESIAN_POINT ( 'NONE',  ( -6.278986562220500571E-07, 1407.561930675709846, 222.2258005058740196 ) ) ;
#32355 = CARTESIAN_POINT ( 'NONE',  ( -17.17241001986523941, 1512.187213306747481, 180.6185504016045797 ) ) ;
#32357 = CARTESIAN_POINT ( 'NONE',  ( 26.35471571933159751, 1507.985750330240080, 216.6976075425179999 ) ) ;
#32356 = CARTESIAN_POINT ( 'NONE',  ( -110.0636328970000051, 1384.926148861439970, 296.9511395936589793 ) ) ;
#32358 = CARTESIAN_POINT ( 'NONE',  ( -1.200707496499999971, 1481.436145357489977, 229.6922108031990035 ) ) ;
#32359 = ORIENTED_EDGE ( 'NONE', *, *, #97392, .T. ) ;
#32360 = VERTEX_POINT ( 'NONE', #53012 ) ;
#32361 = CARTESIAN_POINT ( 'NONE',  ( 3.628818056492709943, 1505.602008419380127, 221.3635114792730292 ) ) ;
#32362 = CARTESIAN_POINT ( 'NONE',  ( -8.861637179848576906, 1506.578945819425144, 229.3724288155509043 ) ) ;
#32363 = CARTESIAN_POINT ( 'NONE',  ( -2.048534905309999932, 1444.110401950890036, 199.2775038477390126 ) ) ;
#32364 = CARTESIAN_POINT ( 'NONE',  ( 11.56811101928649954, 1502.082184429209974, 211.3526444203309893 ) ) ;
#32365 = CARTESIAN_POINT ( 'NONE',  ( -295.4396879434189600, -8387.357407334295203, -1814.563882277197763 ) ) ;
#32366 = AXIS2_PLACEMENT_3D ( 'NONE', #6019, #109047, #15497 ) ;
#32367 = EDGE_CURVE ( 'NONE', #27144, #38088, #28643, .T. ) ;
#32368 = CARTESIAN_POINT ( 'NONE',  ( -0.1127505383448819953, 1508.551704408389924, 220.0210036674560001 ) ) ;
#32369 = CARTESIAN_POINT ( 'NONE',  ( -4.138543391159999807, 1515.492058413689847, 207.2788837304390199 ) ) ;
#32370 = CARTESIAN_POINT ( 'NONE',  ( -45.33985951152630633, 1383.819616475409930, 251.8326084204159940 ) ) ;
#32371 = CARTESIAN_POINT ( 'NONE',  ( -4.522891097415000061, 1511.193640125469983, 201.2736662571170143 ) ) ;
#32372 = CARTESIAN_POINT ( 'NONE',  ( -14.31281836590000012, 1471.309462467430194, 193.2293590363979945 ) ) ;
#32373 = EDGE_CURVE ( 'NONE', #105990, #90799, #21831, .T. ) ;
#32374 = LINE ( 'NONE', #17179, #19604 ) ;
#32375 = CARTESIAN_POINT ( 'NONE',  ( 11.16165179841680022, 1492.334248400359911, 211.8614833883839879 ) ) ;
#32377 = VERTEX_POINT ( 'NONE', #28344 ) ;
#32376 = CARTESIAN_POINT ( 'NONE',  ( 0.02062240259779879806, 1456.497060068189967, 219.0045627830490105 ) ) ;
#32378 = CARTESIAN_POINT ( 'NONE',  ( 32.36284091029084209, 1525.878013734320120, 218.9814869512333075 ) ) ;
#32379 = CARTESIAN_POINT ( 'NONE',  ( -39.71502537339999606, 1379.912275921419905, 233.1978909833590023 ) ) ;
#32380 = CARTESIAN_POINT ( 'NONE',  ( 4.980141907642230414, 1508.551704408389924, 206.4478324081339906 ) ) ;
#32381 = ORIENTED_EDGE ( 'NONE', *, *, #46825, .T. ) ;
#32382 = ORIENTED_EDGE ( 'NONE', *, *, #36587, .T. ) ;
#32383 = CARTESIAN_POINT ( 'NONE',  ( 1.546943247107299912, 1416.828039266790029, 190.2227890105679933 ) ) ;
#32384 = CARTESIAN_POINT ( 'NONE',  ( 35.37723571902410669, 1437.232678306320167, 136.5359279969920010 ) ) ;
#32386 = DIRECTION ( 'NONE',  ( -0.8383970168982891602, -0.5450600352768949497, 0.000000000000000000 ) ) ;
#32385 = DIRECTION ( 'NONE',  ( -0.6736849260863837507, 0.000000000000000000, 0.7390186874254154326 ) ) ;
#32387 = CARTESIAN_POINT ( 'NONE',  ( -7.935787006710000036, 1461.796959919690153, 203.3733083132490265 ) ) ;
#32388 = CARTESIAN_POINT ( 'NONE',  ( -105.9513423759999995, 1381.041490069900192, 299.4116665826589951 ) ) ;
#32389 = EDGE_CURVE ( 'NONE', #42621, #39431, #97194, .T. ) ;
#32390 = CARTESIAN_POINT ( 'NONE',  ( -21.53712143570537663, 1523.621879633028584, 234.3036048850999578 ) ) ;
#32391 = VECTOR ( 'NONE', #106601, 1000.000000000000000 ) ;
#32392 = CARTESIAN_POINT ( 'NONE',  ( -9.648630365757211891, 1508.551704408389924, 218.4115283752189782 ) ) ;
#32393 = CARTESIAN_POINT ( 'NONE',  ( 7.656439366225840537, 1409.180429141550121, 196.2649065922109912 ) ) ;
#32394 = CARTESIAN_POINT ( 'NONE',  ( 18.12088407619999941, 1425.009777113730024, 225.3844322571980001 ) ) ;
#32395 = CARTESIAN_POINT ( 'NONE',  ( 16.09101509135354036, 1459.755789917567654, 220.7358767599917542 ) ) ;
#32396 = CARTESIAN_POINT ( 'NONE',  ( 1.914129829356669976, 1431.087911108530079, 199.8421603670449826 ) ) ;
#32397 = CARTESIAN_POINT ( 'NONE',  ( -2.500000000000000000, 1439.577074560980009, 165.1593652794979903 ) ) ;
#32398 = CARTESIAN_POINT ( 'NONE',  ( -21.05488988819999818, 1452.177807430829944, 142.3440031108980008 ) ) ;
#32399 = EDGE_LOOP ( 'NONE', ( #102778, #48958, #83221, #23841 ) ) ;
#32400 = CARTESIAN_POINT ( 'NONE',  ( -21.59396340175319651, 1525.159196711359755, 184.7447238809834857 ) ) ;
#32401 = CARTESIAN_POINT ( 'NONE',  ( 0.000000000000000000, 1420.584111001019892, 209.1218459616989946 ) ) ;
#32402 =( BOUNDED_CURVE ( )  B_SPLINE_CURVE ( 3, ( #12009, #80870, #107719, #99294 ),
 .UNSPECIFIED., .F., .F. ) 
 B_SPLINE_CURVE_WITH_KNOTS ( ( 4, 4 ),
 ( 2.436781329611983793, 3.141592653589793116 ),
 .UNSPECIFIED. ) 
 CURVE ( )  GEOMETRIC_REPRESENTATION_ITEM ( )  RATIONAL_B_SPLINE_CURVE ( ( 1.000000000000000000, 0.9590300661663088144, 0.9590300661663088144, 1.000000000000000000 ) ) 
 REPRESENTATION_ITEM ( '' )  );
#32403 = CARTESIAN_POINT ( 'NONE',  ( -12.89608628189999884, 1434.724840674140069, 149.2206162816979997 ) ) ;
#32404 = CIRCLE ( 'NONE', #75270, 2.000011244141678635 ) ;
#32405 = EDGE_CURVE ( 'NONE', #56464, #65089, #60798, .T. ) ;
#32406 = CARTESIAN_POINT ( 'NONE',  ( -4.921730754668429691E-10, 1470.815717837130023, 256.1342986906989836 ) ) ;
#32407 = CARTESIAN_POINT ( 'NONE',  ( 1.550613581710394095, 1515.551704304084751, 213.0145121093438547 ) ) ;
#32408 = CARTESIAN_POINT ( 'NONE',  ( -15.05020751920000066, 1420.512178086570202, 211.8108503490890087 ) ) ;
#32409 = CARTESIAN_POINT ( 'NONE',  ( -109.3221271740000020, 1385.236114835410035, 311.2661557522589533 ) ) ;
#32410 = AXIS2_PLACEMENT_3D ( 'NONE', #39798, #105500, #30832 ) ;
#32411 = CARTESIAN_POINT ( 'NONE',  ( -8.290649527490709048, 1511.656200769810084, 215.0711531565719952 ) ) ;
#32412 = CARTESIAN_POINT ( 'NONE',  ( -9.725849732204427056, 1360.959007460116936, 209.6218459617033432 ) ) ;
#32413 = CARTESIAN_POINT ( 'NONE',  ( 32.02808312589922224, 1511.187213306747708, 220.9649204700462235 ) ) ;
#32414 = CARTESIAN_POINT ( 'NONE',  ( 13.54178722023820036, 1508.727572038920016, 233.5140146356369826 ) ) ;
#32415 = EDGE_CURVE ( 'NONE', #100609, #17148, #79119, .T. ) ;
#32416 = CARTESIAN_POINT ( 'NONE',  ( -7.807919481659999938, 1426.371178030289911, 206.6874965076690103 ) ) ;
#32417 = B_SPLINE_CURVE_WITH_KNOTS ( 'NONE', 3,
 ( #93042, #41559, #7394, #75714, #123, #102532, #91948, #34247, #109860, #32044, #85747, #43216, #32603, #92486, #67876, #100879, #66233, #16316, #58912, #67326, #50517, #25272, #75170, #100352, #8480, #23640, #68430, #16859, #15756, #33137, #109320, #6831, #40991, #24714 ),
 .UNSPECIFIED., .F., .F.,
 ( 4, 3, 3, 3, 3, 3, 3, 3, 3, 3, 3, 4 ),
 ( -1.999999957325899969, -1.874565698771090139, -1.690129705517909864, -1.503459105586989919, -1.315598157701630022, -1.126271480114729995, -0.9365167983017219644, -0.7468004907161611694, -0.5575843769484218893, -0.3700485060396170311, -0.1840983994498410770, 0.000000000000000000 ),
 .UNSPECIFIED. ) ;
#32418 = CARTESIAN_POINT ( 'NONE',  ( -0.007128875282218469743, 1517.006509894990131, 208.3750284165899984 ) ) ;
#32419 = CARTESIAN_POINT ( 'NONE',  ( 3.862639946661079904, 1407.379789369289938, 221.6375632500230211 ) ) ;
#32420 = CARTESIAN_POINT ( 'NONE',  ( -14.36584259495580085, 1379.600156427309912, 208.0333617596500062 ) ) ;
#32421 = CARTESIAN_POINT ( 'NONE',  ( 7.246758094710430420, 1424.980848950539894, 212.7605380421140069 ) ) ;
#32422 = VECTOR ( 'NONE', #69170, 1000.000000000000000 ) ;
#32423 = ORIENTED_EDGE ( 'NONE', *, *, #9653, .F. ) ;
#32424 = CARTESIAN_POINT ( 'NONE',  ( 26.44959072580000026, 1437.431546973660033, 225.6828644691980230 ) ) ;
#32426 = CARTESIAN_POINT ( 'NONE',  ( -15.10840968467219980, 1512.260118274579781, 221.8456817057260082 ) ) ;
#32425 = CARTESIAN_POINT ( 'NONE',  ( -3.530374461310000100, 1489.044399826630070, 181.7468199677979896 ) ) ;
#32427 = ADVANCED_FACE ( 'NONE', ( #38930 ), #56309, .T. ) ;
#32428 = CARTESIAN_POINT ( 'NONE',  ( -2.781364391544570047, 1419.521710623789886, 186.1806238305539978 ) ) ;
#32429 = CARTESIAN_POINT ( 'NONE',  ( -10.70017680549999994, 1423.864995475129945, 211.7704828164379762 ) ) ;
#32430 = CARTESIAN_POINT ( 'NONE',  ( -13.82378397995019981, 1379.696997726179916, 208.1617145838290241 ) ) ;
#32431 = EDGE_CURVE ( 'NONE', #62788, #75187, #63078, .T. ) ;
#32432 = CARTESIAN_POINT ( 'NONE',  ( -3.469412232211699809, 1452.791905842489996, 152.3220070113180213 ) ) ;
#32433 = B_SPLINE_CURVE_WITH_KNOTS ( 'NONE', 5,
 ( #7374, #41538, #75152, #23054, #91928, #57804, #90266, #30369, #14668 ),
 .UNSPECIFIED., .F., .F.,
 ( 6, 3, 6 ),
 ( 0.000000000000000000, 0.5000000000000000000, 1.000000000000000000 ),
 .UNSPECIFIED. ) ;
#32434 = CARTESIAN_POINT ( 'NONE',  ( -18.79707643829999952, 1416.837309283529976, 208.4087471548650115 ) ) ;
#32435 = EDGE_LOOP ( 'NONE', ( #107917, #106221, #91154, #44519 ) ) ;
#32436 = CARTESIAN_POINT ( 'NONE',  ( -5.360342550372870107, 1422.242822755830048, 144.1527768786770025 ) ) ;
#32437 = CARTESIAN_POINT ( 'NONE',  ( 5.764621990845120029E-05, 1409.781064299669879, 270.0713832058750086 ) ) ;
#32438 = CARTESIAN_POINT ( 'NONE',  ( 16.28387335898309729, 1423.071578876830017, 229.4312782304039899 ) ) ;
#32439 = CARTESIAN_POINT ( 'NONE',  ( 2.038646110889678287, 1525.960063244516959, 177.0579350083066004 ) ) ;
#32440 = ORIENTED_EDGE ( 'NONE', *, *, #84635, .T. ) ;
#32441 = ORIENTED_EDGE ( 'NONE', *, *, #53536, .T. ) ;
#32442 = CARTESIAN_POINT ( 'NONE',  ( -39.76804797110000322, 1384.988983489909742, 212.4493689816489734 ) ) ;
#32443 = CARTESIAN_POINT ( 'NONE',  ( -22.71969927661109878, 1409.706431297170184, 209.0865112504420154 ) ) ;
#32444 = EDGE_CURVE ( 'NONE', #69935, #108962, #32582, .T. ) ;
#32445 = ORIENTED_EDGE ( 'NONE', *, *, #63343, .F. ) ;
#32446 = CARTESIAN_POINT ( 'NONE',  ( -11.60015079993175036, 1437.619279042158723, 151.8496192710196340 ) ) ;
#32447 = CARTESIAN_POINT ( 'NONE',  ( 0.000000000000000000, 1508.913060387330006, 209.1218459616979999 ) ) ;
#32448 = EDGE_CURVE ( 'NONE', #73065, #82244, #25832, .T. ) ;
#32449 = CARTESIAN_POINT ( 'NONE',  ( -3.191653983950000217, 1507.639293120730144, 236.7936837086979835 ) ) ;
#32450 = CARTESIAN_POINT ( 'NONE',  ( -22.33198887150000189, 1410.866712961029862, 213.4112846406879953 ) ) ;
#32451 = ORIENTED_EDGE ( 'NONE', *, *, #105777, .F. ) ;
#32452 = CARTESIAN_POINT ( 'NONE',  ( 41.83092555681560043, 1455.428899374940102, 266.5381060907129722 ) ) ;
#32453 = CARTESIAN_POINT ( 'NONE',  ( -0.6346444654042239231, 1424.181128449899916, 228.1611430178420221 ) ) ;
#32454 = CARTESIAN_POINT ( 'NONE',  ( -0.3212355716730000421, 1418.619114157530021, 184.6997714626980098 ) ) ;
#32455 = CARTESIAN_POINT ( 'NONE',  ( 3.447264348965000558, 1516.858765657450249, 205.6607986404769974 ) ) ;
#32456 = VECTOR ( 'NONE', #20865, 1000.000000000000000 ) ;
#32457 = ORIENTED_EDGE ( 'NONE', *, *, #44853, .T. ) ;
#32458 = CARTESIAN_POINT ( 'NONE',  ( 18.96133265953471181, 1457.509259180501431, 226.7471396993940687 ) ) ;
#32459 = CARTESIAN_POINT ( 'NONE',  ( 14.94819994016220122, 1513.870294662249989, 194.3661611336529802 ) ) ;
#32460 = CARTESIAN_POINT ( 'NONE',  ( 4.541133981099999772, 1426.446980476019917, 211.3175313703289930 ) ) ;
#32461 = ORIENTED_EDGE ( 'NONE', *, *, #62348, .T. ) ;
#32462 = CARTESIAN_POINT ( 'NONE',  ( 2.500000000000000000, 1448.552414630679777, 182.3688072228979991 ) ) ;
#32463 = CARTESIAN_POINT ( 'NONE',  ( 26.91229608229999926, 1451.721307008429903, 135.7917609875980247 ) ) ;
#32464 = CARTESIAN_POINT ( 'NONE',  ( -13.27508839399100005, 1512.548660307890032, 193.8371749040339864 ) ) ;
#32465 = CARTESIAN_POINT ( 'NONE',  ( 9.120907800999310311, 1452.594551268460009, 150.9409900070750155 ) ) ;
#32466 = CARTESIAN_POINT ( 'NONE',  ( 7.966089429799998456, 1421.435344681000061, 195.9328034231990046 ) ) ;
#32467 = EDGE_CURVE ( 'NONE', #35207, #105161, #70194, .T. ) ;
#32468 = CARTESIAN_POINT ( 'NONE',  ( 0.3404198581328219952, 1431.708939325159918, 218.6080673264870029 ) ) ;
#32469 = CARTESIAN_POINT ( 'NONE',  ( -4.329448776040000446, 1515.064792882589927, 209.0973262533439936 ) ) ;
#32470 = CARTESIAN_POINT ( 'NONE',  ( 1.806552148200949892, 1408.976146578469979, 186.8750707912049904 ) ) ;
#32472 = CARTESIAN_POINT ( 'NONE',  ( 4.038582000521929061, 1515.598601297060441, 209.4325486173436843 ) ) ;
#32471 = CARTESIAN_POINT ( 'NONE',  ( -13.39822223261879941, 1434.924425846410031, 148.8729776175770212 ) ) ;
#32473 = CARTESIAN_POINT ( 'NONE',  ( 10.66776494060489888, 1424.286284153560018, 206.6302608488180113 ) ) ;
#32474 = VECTOR ( 'NONE', #97523, 1000.000000000000000 ) ;
#32475 = CARTESIAN_POINT ( 'NONE',  ( -10.76003433109999996, 1379.099935777159772, 215.2151889901689970 ) ) ;
#32476 = EDGE_CURVE ( 'NONE', #69390, #64966, #40600, .T. ) ;
#32477 = CARTESIAN_POINT ( 'NONE',  ( -8.126234285584999384, 1514.923664147150021, 202.9950997886369635 ) ) ;
#32478 = EDGE_LOOP ( 'NONE', ( #87827, #39854, #33602, #69708 ) ) ;
#32479 = CARTESIAN_POINT ( 'NONE',  ( 2.340571794239999726, 1472.604797962090061, 216.2450463976489914 ) ) ;
#32480 = DIRECTION ( 'NONE',  ( 0.1403901532130676921, 0.9900962604114871279, 1.240732444514164729E-15 ) ) ;
#32481 = CARTESIAN_POINT ( 'NONE',  ( -0.1681681984989999989, 1432.413060387330006, 146.1721969590979882 ) ) ;
#32482 = CARTESIAN_POINT ( 'NONE',  ( -9.868952737369999895, 1387.120338798609964, 200.7479674930190185 ) ) ;
#32483 = CARTESIAN_POINT ( 'NONE',  ( 9.799993285045120572, 1423.431501241479964, 209.4821564460780223 ) ) ;
#32484 = CARTESIAN_POINT ( 'NONE',  ( 10.94471713272500146, 1423.681646166069868, 203.2258399444270083 ) ) ;
#32485 = CARTESIAN_POINT ( 'NONE',  ( 1.727284872639999858, 1431.232427857390121, 218.4620812309590008 ) ) ;
#32486 = VECTOR ( 'NONE', #67101, 1000.000000000000000 ) ;
#32487 = FACE_OUTER_BOUND ( 'NONE', #23893, .T. ) ;
#32488 = CARTESIAN_POINT ( 'NONE',  ( -9.128811013672018859, 1383.865584117230128, 218.5284686629279918 ) ) ;
#32489 = CARTESIAN_POINT ( 'NONE',  ( 17.83486663330486621, 1523.678648413191695, 180.3677388339000061 ) ) ;
#32490 = CARTESIAN_POINT ( 'NONE',  ( 1.914156610164409855, 1431.087920293139859, 199.8421651263110164 ) ) ;
#32491 = CARTESIAN_POINT ( 'NONE',  ( 13.15726442299999910, 1416.543503932829935, 196.3435872999980063 ) ) ;
#32492 = CARTESIAN_POINT ( 'NONE',  ( 0.6916575409457245138, 1467.050682359807524, 235.5170429814173474 ) ) ;
#32493 = CARTESIAN_POINT ( 'NONE',  ( -109.4272857735724358, 1387.208746469848847, 297.3473037064583764 ) ) ;
#32494 = CARTESIAN_POINT ( 'NONE',  ( 8.536750983910001978, 1465.433596956489964, 214.1723092710689968 ) ) ;
#32495 = CARTESIAN_POINT ( 'NONE',  ( -4.487249792034999629, 1509.038615934239942, 209.1218459511669892 ) ) ;
#32496 = CARTESIAN_POINT ( 'NONE',  ( 2.234923043937409926, 1512.341036938790012, 216.7210731156089878 ) ) ;
#32497 = CARTESIAN_POINT ( 'NONE',  ( 18.50064172359999759, 1416.067629290630066, 209.7633006632509876 ) ) ;
#32498 = CIRCLE ( 'NONE', #50416, 2.000000000000000000 ) ;
#32500 = B_SPLINE_CURVE_WITH_KNOTS ( 'NONE', 3,
 ( #27440, #70042, #6374, #33765, #61623, #40520, #57896, #95755 ),
 .UNSPECIFIED., .F., .F.,
 ( 4, 2, 2, 4 ),
 ( 0.000000000000000000, 0.2500000000000000000, 0.5000000000000000000, 1.000000000000000000 ),
 .UNSPECIFIED. ) ;
#32499 = CARTESIAN_POINT ( 'NONE',  ( -8.117665312093365060, 1425.422482083973136, 208.7068306292352986 ) ) ;
#32501 = B_SPLINE_CURVE_WITH_KNOTS ( 'NONE', 5,
 ( #83454, #17331, #92402, #84564, #59946, #6748, #94062, #101337, #32521 ),
 .UNSPECIFIED., .F., .F.,
 ( 6, 3, 6 ),
 ( 0.000000000000000000, 0.5111911274250463544, 1.000000000000000000 ),
 .UNSPECIFIED. ) ;
#32502 = CARTESIAN_POINT ( 'NONE',  ( -1.808747093880000101, 1474.298755092390138, 216.4373183392189617 ) ) ;
#32503 = CARTESIAN_POINT ( 'NONE',  ( -17.59271046137119754, 1410.455526649410103, 193.4350316739960078 ) ) ;
#32504 = CARTESIAN_POINT ( 'NONE',  ( 0.7420515760630009838, 1515.368784161290250, 204.8340560411189699 ) ) ;
#32505 = CARTESIAN_POINT ( 'NONE',  ( -0.4151546846839010985, 1522.906561336850928, 173.3106345060153046 ) ) ;
#32506 = CARTESIAN_POINT ( 'NONE',  ( -13.97985289466289949, 1420.196174639120045, 195.9955836006969889 ) ) ;
#32507 = CARTESIAN_POINT ( 'NONE',  ( -7.646910556199999931, 1414.913060387329779, 223.7159594430980007 ) ) ;
#32508 = CARTESIAN_POINT ( 'NONE',  ( 0.2051560345590330015, 1460.078046002440033, 182.9497274072810171 ) ) ;
#32510 = EDGE_LOOP ( 'NONE', ( #67730, #90368, #96241, #99430 ) ) ;
#32509 = CARTESIAN_POINT ( 'NONE',  ( -5.636364295891119980, 1407.760601417009866, 221.4271416552059861 ) ) ;
#32511 = CARTESIAN_POINT ( 'NONE',  ( -17.22592482065197927, 1443.913060387330233, 162.9227486220069920 ) ) ;
#32512 = CARTESIAN_POINT ( 'NONE',  ( -7.956327371650409042, 1385.264409114995033, 199.4928816929445077 ) ) ;
#32513 = DIRECTION ( 'NONE',  ( -0.9455185755993178454, 0.000000000000000000, 0.3255681544571537578 ) ) ;
#32514 = CARTESIAN_POINT ( 'NONE',  ( -41.14836836638649942, 1446.538313981779993, 134.0999999985649822 ) ) ;
#32515 = CARTESIAN_POINT ( 'NONE',  ( -109.3497582309999814, 1384.888520030000109, 297.1386468897590021 ) ) ;
#32516 = ORIENTED_EDGE ( 'NONE', *, *, #68672, .T. ) ;
#32517 = CARTESIAN_POINT ( 'NONE',  ( -17.50735355147196515, 1524.972613296805548, 180.8654324079905393 ) ) ;
#32518 = CARTESIAN_POINT ( 'NONE',  ( -11.99447448239999936, 1410.787978745530154, 198.2808973881980137 ) ) ;
#32519 = CARTESIAN_POINT ( 'NONE',  ( -103.6745750688534429, 1379.960313182111804, 305.2256231368813246 ) ) ;
#32520 = CARTESIAN_POINT ( 'NONE',  ( 20.54545170502450446, 1497.714248496870141, 214.2325552634220003 ) ) ;
#32521 = CARTESIAN_POINT ( 'NONE',  ( 3.628818056492709943, 1505.602008419380127, 221.3635114792730292 ) ) ;
#32522 = CARTESIAN_POINT ( 'NONE',  ( 40.82574024660451784, 1425.625456410858988, 269.1071013978336168 ) ) ;
#32523 = CARTESIAN_POINT ( 'NONE',  ( -14.91281678549999867, 1416.540137034410009, 213.0067496813389880 ) ) ;
#32524 = CARTESIAN_POINT ( 'NONE',  ( -13.57778968770000105, 1380.131028916370269, 210.8119687010990049 ) ) ;
#32525 = DIRECTION ( 'NONE',  ( -0.000000000000000000, -1.000000000000000000, -0.000000000000000000 ) ) ;
#32526 = CARTESIAN_POINT ( 'NONE',  ( -64.59939480701859793, 1385.084584694940077, 254.1492228190850255 ) ) ;
#32527 = CARTESIAN_POINT ( 'NONE',  ( -17.44374831407654725, 1524.130440953581001, 237.5220222273293302 ) ) ;
#32528 = CARTESIAN_POINT ( 'NONE',  ( 11.82645876916039995, 1426.795760154579966, 206.5338053568990233 ) ) ;
#32529 = VERTEX_POINT ( 'NONE', #22662 ) ;
#32530 = CARTESIAN_POINT ( 'NONE',  ( -29.29916080650000154, 1450.601733552070073, 136.3811420100980172 ) ) ;
#32531 = CARTESIAN_POINT ( 'NONE',  ( -15.92198785269019901, 1410.714326797879949, 226.7129421669140186 ) ) ;
#32533 = ORIENTED_EDGE ( 'NONE', *, *, #50627, .F. ) ;
#32532 = CARTESIAN_POINT ( 'NONE',  ( 3.947090874974254149, 1427.113278099589934, 134.0999999980980704 ) ) ;
#32534 = CARTESIAN_POINT ( 'NONE',  ( 2.484906683780000236, 1472.794382616990106, 219.0213525527389891 ) ) ;
#32535 = CARTESIAN_POINT ( 'NONE',  ( 10.20292507491700107, 1470.367289678880070, 209.9988428381880112 ) ) ;
#32536 = CARTESIAN_POINT ( 'NONE',  ( -18.24877744519994138, 1410.913188608474002, 224.3502044276641527 ) ) ;
#32538 = B_SPLINE_CURVE_WITH_KNOTS ( 'NONE', 3,
 ( #13542, #29268, #63460, #97579, #55046, #89174 ),
 .UNSPECIFIED., .F., .F.,
 ( 4, 2, 4 ),
 ( 0.000000000000000000, 0.5000000000000000000, 1.000000000000000000 ),
 .UNSPECIFIED. ) ;
#32537 = CARTESIAN_POINT ( 'NONE',  ( -109.8283088200000037, 1384.770372820250032, 311.3782655042589909 ) ) ;
#32539 = CARTESIAN_POINT ( 'NONE',  ( -11.09323634000895353, 1492.391963403851150, 209.0647905715161698 ) ) ;
#32540 = CARTESIAN_POINT ( 'NONE',  ( 20.29357770150000206, 1410.117248657430082, 219.1572836432980012 ) ) ;
#32541 = CARTESIAN_POINT ( 'NONE',  ( -22.52609270576707701, 1509.699688878261213, 190.3721629464874638 ) ) ;
#32542 = CARTESIAN_POINT ( 'NONE',  ( -17.44047523940000133, 1423.641482825129970, 226.7779220472980057 ) ) ;
#32543 = CARTESIAN_POINT ( 'NONE',  ( -2.942030012410809636, 1512.314860016870171, 201.2300683927209946 ) ) ;
#32544 = CARTESIAN_POINT ( 'NONE',  ( -13.88938230474218294, 1379.665440102101456, 212.4764176185094868 ) ) ;
#32545 = CARTESIAN_POINT ( 'NONE',  ( -98.31848851494262931, 1331.448250124730066, 312.4609134345859047 ) ) ;
#32546 = CARTESIAN_POINT ( 'NONE',  ( -3.286051671319225598, 1371.185232598742687, 209.6218459617033432 ) ) ;
#32547 = FACE_OUTER_BOUND ( 'NONE', #65637, .T. ) ;
#32548 = AXIS2_PLACEMENT_3D ( 'NONE', #51690, #743, #51138 ) ;
#32549 = CARTESIAN_POINT ( 'NONE',  ( -3.267603553834999897, 1516.858171774179937, 205.8687047948669999 ) ) ;
#32550 = CARTESIAN_POINT ( 'NONE',  ( 2.499999987259999834, 1447.625363422479950, 167.4763715502979835 ) ) ;
#32551 = VERTEX_POINT ( 'NONE', #73110 ) ;
#32552 = CARTESIAN_POINT ( 'NONE',  ( -3.052975934615000053, 1516.551704408390151, 201.1191225673069880 ) ) ;
#32553 = CARTESIAN_POINT ( 'NONE',  ( -4.224734712525329172, 1441.578183378099993, 166.5712083107650017 ) ) ;
#32555 = VERTEX_POINT ( 'NONE', #56864 ) ;
#32554 = CARTESIAN_POINT ( 'NONE',  ( -68.69823031144730408, 1379.747764229889981, 280.2920408481639925 ) ) ;
#32556 = CARTESIAN_POINT ( 'NONE',  ( -17.54118812318929699, 1417.910349704349983, 206.8634943573240150 ) ) ;
#32557 = ORIENTED_EDGE ( 'NONE', *, *, #51072, .T. ) ;
#32558 = CARTESIAN_POINT ( 'NONE',  ( -16.78435733967954846, 1513.560745840784421, 222.3626190331726491 ) ) ;
#32559 = CARTESIAN_POINT ( 'NONE',  ( 11.36069158549999969, 1501.598968272789989, 207.6205322127590023 ) ) ;
#32561 = CARTESIAN_POINT ( 'NONE',  ( 15.97496008288169733, 1409.470830777089986, 192.9108099150550117 ) ) ;
#32560 = CARTESIAN_POINT ( 'NONE',  ( -20.59678673803600546, 1507.763197061015035, 190.3721465278125606 ) ) ;
#32562 = CARTESIAN_POINT ( 'NONE',  ( -7.708770045145000083, 1516.524310051880093, 211.4128934593470035 ) ) ;
#32563 = CARTESIAN_POINT ( 'NONE',  ( 40.57510725528580053, 1442.092273678310221, 136.9264308840439810 ) ) ;
#32564 = VECTOR ( 'NONE', #67221, 1000.000000000000000 ) ;
#32565 = ADVANCED_FACE ( 'NONE', ( #30544 ), #74771, .F. ) ;
#32566 = CARTESIAN_POINT ( 'NONE',  ( -11.63661014589999887, 1425.864895317229866, 144.1626081073980004 ) ) ;
#32567 = DIRECTION ( 'NONE',  ( -0.02616795315378250830, -0.9993150033772694174, -0.02616796233621986045 ) ) ;
#32569 = EDGE_CURVE ( 'NONE', #66425, #94251, #19083, .T. ) ;
#32568 = CARTESIAN_POINT ( 'NONE',  ( 15.40019697367809570, 1461.678762082152616, 229.7684540114784966 ) ) ;
#32570 = CARTESIAN_POINT ( 'NONE',  ( 14.45783227242900004, 1416.839692127189892, 196.8516148535319985 ) ) ;
#32571 = CARTESIAN_POINT ( 'NONE',  ( -7.075873090581220301E-12, 1395.913060387330006, 220.1216245177919859 ) ) ;
#32572 = ORIENTED_EDGE ( 'NONE', *, *, #41136, .T. ) ;
#32573 = CARTESIAN_POINT ( 'NONE',  ( 18.46110511450000047, 1471.786120934990095, 195.2229451476989937 ) ) ;
#32574 = DIRECTION ( 'NONE',  ( -5.980589973904019347E-17, 1.000000000000000000, -1.736889445713099699E-16 ) ) ;
#32575 = VERTEX_POINT ( 'NONE', #99941 ) ;
#32576 = ORIENTED_EDGE ( 'NONE', *, *, #82224, .T. ) ;
#32577 = CARTESIAN_POINT ( 'NONE',  ( -29.76861393075075668, 1509.997849702723215, 209.5183840890453837 ) ) ;
#32578 = CARTESIAN_POINT ( 'NONE',  ( 10.42032938315659862, 1453.131236670619955, 211.0854769158530360 ) ) ;
#32579 = CARTESIAN_POINT ( 'NONE',  ( 0.1923572142570000032, 1452.340214348429754, 183.2784190975980039 ) ) ;
#32580 = CARTESIAN_POINT ( 'NONE',  ( -20.34501938112269670, 1508.551704408389924, 210.4487953478319753 ) ) ;
#32581 = CARTESIAN_POINT ( 'NONE',  ( -19.06723915664710134, 1485.490521620860136, 189.6150037022410118 ) ) ;
#32583 = CARTESIAN_POINT ( 'NONE',  ( 4.329448776040000446, 1515.064792882589927, 210.9648081929590262 ) ) ;
#32582 = CIRCLE ( 'NONE', #41536, 7.500000000000000000 ) ;
#32584 = CARTESIAN_POINT ( 'NONE',  ( -13.82378400310000011, 1379.696997732550017, 208.1617145800939852 ) ) ;
#32585 = EDGE_CURVE ( 'NONE', #57683, #52165, #33766, .T. ) ;
#32586 = CARTESIAN_POINT ( 'NONE',  ( 42.60628464680300453, 1443.705283352369861, 135.6938352391079832 ) ) ;
#32587 = CARTESIAN_POINT ( 'NONE',  ( 2.598899143124699940, 1421.341238652740003, 183.3127735487479981 ) ) ;
#32588 = CARTESIAN_POINT ( 'NONE',  ( 29.74902317390491646, 1525.343710797494623, 222.0046397572924377 ) ) ;
#32589 = CARTESIAN_POINT ( 'NONE',  ( -11.84252628229999971, 1391.501155191750058, 212.7918940593590094 ) ) ;
#32590 = CARTESIAN_POINT ( 'NONE',  ( -84.89198071708958082, 1384.817327810709912, 288.6329308340300486 ) ) ;
#32591 = ORIENTED_EDGE ( 'NONE', *, *, #48911, .F. ) ;
#32592 = CARTESIAN_POINT ( 'NONE',  ( 3.453544825624999870, 1517.106845464700200, 201.7850012896870169 ) ) ;
#32593 = CARTESIAN_POINT ( 'NONE',  ( -3.269025173884999802, 1517.026534522949987, 208.0024068424170025 ) ) ;
#32594 = ORIENTED_EDGE ( 'NONE', *, *, #110303, .T. ) ;
#32595 = CARTESIAN_POINT ( 'NONE',  ( 11.27186228809999946, 1414.983771850430003, 222.4323528540979851 ) ) ;
#32596 = CARTESIAN_POINT ( 'NONE',  ( 4.613666293552466158, 1511.398924905619651, 217.5165917695272242 ) ) ;
#32597 = ORIENTED_EDGE ( 'NONE', *, *, #93088, .T. ) ;
#32598 = CARTESIAN_POINT ( 'NONE',  ( -13.40958059889999987, 1414.996444526030018, 220.3303867755979866 ) ) ;
#32599 = CARTESIAN_POINT ( 'NONE',  ( 6.884066909838960413, 1429.271425755099926, 215.6498002703089867 ) ) ;
#32600 = CARTESIAN_POINT ( 'NONE',  ( -15.69795926999090163, 1522.051704408389924, 195.4758181584410011 ) ) ;
#32601 = CARTESIAN_POINT ( 'NONE',  ( -10.24974442935089947, 1462.794995015260156, 206.4145582120489735 ) ) ;
#32602 = CARTESIAN_POINT ( 'NONE',  ( -13.44341642900000089, 1426.042751063429932, 222.1933743934980043 ) ) ;
#32603 = CARTESIAN_POINT ( 'NONE',  ( 10.47538074031769995, 1469.876780579760180, 207.1493381432659930 ) ) ;
#32604 = CARTESIAN_POINT ( 'NONE',  ( 7.613968465965000654, 1512.903985260039917, 203.5071921160869977 ) ) ;
#32605 = CARTESIAN_POINT ( 'NONE',  ( -17.05938549526129577, 1517.051704405600049, 195.1949804090679947 ) ) ;
#32606 = CARTESIAN_POINT ( 'NONE',  ( -15.52964665090000018, 1451.324133669029834, 222.4830580725980269 ) ) ;
#32608 = CARTESIAN_POINT ( 'NONE',  ( -1.729960644012338955, 1451.871857846600051, 184.1618444272322108 ) ) ;
#32607 = CARTESIAN_POINT ( 'NONE',  ( 12.47197601159999891, 1461.938359065629811, 231.9335636622980132 ) ) ;
#32609 = CARTESIAN_POINT ( 'NONE',  ( -4.550835815579397092, 1422.060929357180612, 184.6135640397586712 ) ) ;
#32610 = EDGE_CURVE ( 'NONE', #48164, #51456, #20095, .T. ) ;
#32611 = CARTESIAN_POINT ( 'NONE',  ( -6.942354311545000378, 1516.905946377369901, 216.8406094761369900 ) ) ;
#32612 = VERTEX_POINT ( 'NONE', #2362 ) ;
#32613 = CARTESIAN_POINT ( 'NONE',  ( 7.734617087614999775, 1516.863303996349941, 201.3001138717470155 ) ) ;
#32614 = PLANE ( 'NONE',  #60729 ) ;
#32615 = CARTESIAN_POINT ( 'NONE',  ( -21.55808852496470962, 1523.844789899204443, 234.2610814835831547 ) ) ;
#32616 = CARTESIAN_POINT ( 'NONE',  ( -3.255967424474999650, 1516.989560013210166, 214.1335248082570217 ) ) ;
#32617 = CARTESIAN_POINT ( 'NONE',  ( 2.956827888069309740, 1515.222544093250008, 213.4459675459839900 ) ) ;
#32618 = EDGE_CURVE ( 'NONE', #40693, #88887, #92680, .T. ) ;
#32619 = CARTESIAN_POINT ( 'NONE',  ( -11.60004869885203682, 1426.175846117266929, 138.0317712997469073 ) ) ;
#32621 = EDGE_LOOP ( 'NONE', ( #44036, #67706 ) ) ;
#32620 = CARTESIAN_POINT ( 'NONE',  ( -11.98797817168060043, 1501.622048148490194, 211.4516665317300124 ) ) ;
#32622 = CARTESIAN_POINT ( 'NONE',  ( -15.55913749090388087, 1415.687746563815381, 209.6140629208140922 ) ) ;
#32623 = CARTESIAN_POINT ( 'NONE',  ( -15.41004399704489991, 1507.593738162499903, 192.1064836414840045 ) ) ;
#32624 = CARTESIAN_POINT ( 'NONE',  ( -11.75996506569999944, 1431.602545802069926, 150.7723106216979829 ) ) ;
#32625 = CARTESIAN_POINT ( 'NONE',  ( -6.095125402108049428, 1441.837371024610093, 202.1071835498420057 ) ) ;
#32626 = CARTESIAN_POINT ( 'NONE',  ( 27.01381218759999925, 1450.681579806120226, 136.4483250053980044 ) ) ;
#32627 = CARTESIAN_POINT ( 'NONE',  ( -7.602521990106799521, 1425.809942238630128, 203.7442148849289936 ) ) ;
#32628 = CARTESIAN_POINT ( 'NONE',  ( 6.906779373730000060, 1480.511273071390178, 206.6585084174489850 ) ) ;
#32630 = CARTESIAN_POINT ( 'NONE',  ( -3.194520716545333094, 1421.833028466792484, 139.1411856592992820 ) ) ;
#32629 = CARTESIAN_POINT ( 'NONE',  ( -21.13276769859999860, 1482.727891398330030, 225.4958365253980048 ) ) ;
#32631 = DIRECTION ( 'NONE',  ( -1.755985294532469921E-16, 1.000000000000000000, -1.338183447452831989E-16 ) ) ;
#32632 = ORIENTED_EDGE ( 'NONE', *, *, #13224, .F. ) ;
#32633 = CARTESIAN_POINT ( 'NONE',  ( 6.546951682585000043, 1516.606339319019980, 206.2472570094369928 ) ) ;
#32634 = CARTESIAN_POINT ( 'NONE',  ( 9.813457517070000691, 1407.253461234630095, 269.4661102456980188 ) ) ;
#32635 = CARTESIAN_POINT ( 'NONE',  ( -32.86802468386279941, 1523.382868172864164, 217.2040256693919957 ) ) ;
#32636 = CARTESIAN_POINT ( 'NONE',  ( 18.81101837559999979, 1410.875859629429897, 194.9135330840980203 ) ) ;
#32637 = CARTESIAN_POINT ( 'NONE',  ( -0.3240745752627050003, 1508.859753704990226, 238.3613378923800212 ) ) ;
#32638 = CARTESIAN_POINT ( 'NONE',  ( 2.003572920832760396, 1454.623075833809935, 218.3091034149879874 ) ) ;
#32639 = CARTESIAN_POINT ( 'NONE',  ( 2.500000000000000000, 1448.894380902750072, 155.6080914261119972 ) ) ;
#32640 = CARTESIAN_POINT ( 'NONE',  ( 10.27415084429999936, 1462.789161984029761, 234.7156815036980220 ) ) ;
#32641 = CARTESIAN_POINT ( 'NONE',  ( -15.22265112240000029, 1415.931502849980234, 206.6367959904590066 ) ) ;
#32642 = CARTESIAN_POINT ( 'NONE',  ( -13.94141741770000031, 1444.723632129780071, 188.4161808736979822 ) ) ;
#32643 = CARTESIAN_POINT ( 'NONE',  ( -15.55054316549999882, 1408.913060387329779, 218.7899552842880269 ) ) ;
#32644 = CARTESIAN_POINT ( 'NONE',  ( 9.181100887863649973, 1450.964097471789955, 210.1935140534000084 ) ) ;
#32645 = CARTESIAN_POINT ( 'NONE',  ( 5.402393448019999767, 1407.889686284330082, 270.1311850753980366 ) ) ;
#32646 = CARTESIAN_POINT ( 'NONE',  ( 1.449741897432649917, 1506.060387600080048, 181.1592481886430051 ) ) ;
#32647 = CYLINDRICAL_SURFACE ( 'NONE', #69482, 1.999999999999999556 ) ;
#32648 = CARTESIAN_POINT ( 'NONE',  ( -12.90006350071139885, 1507.961479924099876, 209.2725772594830005 ) ) ;
#32649 = CARTESIAN_POINT ( 'NONE',  ( 21.32683180188249139, 1525.211477436245787, 234.3841140920684722 ) ) ;
#32650 = CARTESIAN_POINT ( 'NONE',  ( -3.441813313009999487, 1475.979926173929925, 267.5320898906979892 ) ) ;
#32651 = CARTESIAN_POINT ( 'NONE',  ( -4.221566735949540572, 1446.221982441119962, 169.5773968837689836 ) ) ;
#32652 = CARTESIAN_POINT ( 'NONE',  ( -14.63125512773061665, 1514.438041836527418, 192.7641272998755824 ) ) ;
#32653 = CARTESIAN_POINT ( 'NONE',  ( -10.65998469088088285, 1486.512546998173775, 183.7751546670934886 ) ) ;
#32654 = CARTESIAN_POINT ( 'NONE',  ( -48.91894787223070296, 1384.745253908090035, 259.5132730780889574 ) ) ;
#32655 = CARTESIAN_POINT ( 'NONE',  ( -106.8704702527970056, 1391.913060387289988, 302.0021170729179971 ) ) ;
#32656 = CARTESIAN_POINT ( 'NONE',  ( -4.884981308350000102E-15, 1441.600846913620217, 155.7224805731980268 ) ) ;
#32657 = CARTESIAN_POINT ( 'NONE',  ( -24.99371936868969968, 1457.420242470830090, 211.0583525782739969 ) ) ;
#32658 = CARTESIAN_POINT ( 'NONE',  ( -16.62351968733423391, 1524.082582765195411, 237.7032314130105703 ) ) ;
#32659 = CARTESIAN_POINT ( 'NONE',  ( 11.99447453070000158, 1410.787978747230227, 198.2808974363979928 ) ) ;
#32660 = CARTESIAN_POINT ( 'NONE',  ( -1.270643054695779872, 1395.957432220560122, 220.0592832377249977 ) ) ;
#32661 = CARTESIAN_POINT ( 'NONE',  ( -9.574034133352039788, 1380.787723534742099, 201.2514544285035640 ) ) ;
#32662 = CARTESIAN_POINT ( 'NONE',  ( -15.06702969580600104, 1422.390513282080065, 229.4662855426749672 ) ) ;
#32663 = CARTESIAN_POINT ( 'NONE',  ( 10.32403803707900103, 1479.706866225239992, 206.5120394917040301 ) ) ;
#32664 = ORIENTED_EDGE ( 'NONE', *, *, #35867, .F. ) ;
#32665 = CARTESIAN_POINT ( 'NONE',  ( -4.069377925904865023, 1410.431552160933734, 232.1899145600301324 ) ) ;
#32666 = CARTESIAN_POINT ( 'NONE',  ( -19.16799087484339736, 1444.936066881249872, 199.7607002489500019 ) ) ;
#32667 = CARTESIAN_POINT ( 'NONE',  ( -7.535878286259929837, 1510.580107401401165, 214.9399003442833305 ) ) ;
#32668 = CARTESIAN_POINT ( 'NONE',  ( 20.10528729596699904, 1430.878053334959986, 215.1856554786780009 ) ) ;
#32670 = CARTESIAN_POINT ( 'NONE',  ( -15.09659340796500082, 1514.030803186779849, 193.4062324905669925 ) ) ;
#32669 = DIRECTION ( 'NONE',  ( 0.000000000000000000, 0.000000000000000000, -1.000000000000000000 ) ) ;
#32671 = CARTESIAN_POINT ( 'NONE',  ( 17.22627284987205698, 1525.856065479249082, 236.4663881609581892 ) ) ;
#32672 = CYLINDRICAL_SURFACE ( 'NONE', #63439, 0.5000000000000026645 ) ;
#32673 = CARTESIAN_POINT ( 'NONE',  ( 27.87287880629999748, 1445.634712509609926, 137.2901166997980056 ) ) ;
#32674 = CARTESIAN_POINT ( 'NONE',  ( 32.38114538885250226, 1523.604703353109699, 202.1233279672528624 ) ) ;
#32675 = CARTESIAN_POINT ( 'NONE',  ( 2.483322453895000059, 1517.139039350860003, 202.5585910412470128 ) ) ;
#32676 = CARTESIAN_POINT ( 'NONE',  ( 20.83094015040000002, 1452.185627928030044, 134.0999999980979851 ) ) ;
#32677 = CARTESIAN_POINT ( 'NONE',  ( -11.91237982683207441, 1398.266268150713813, 203.9165306044730244 ) ) ;
#32678 = CARTESIAN_POINT ( 'NONE',  ( 15.78855998223499846, 1512.525301340730039, 195.5242935507669984 ) ) ;
#32679 = CARTESIAN_POINT ( 'NONE',  ( -21.92444879442203742, 1509.678679009930875, 190.3921826424486312 ) ) ;
#32680 = CARTESIAN_POINT ( 'NONE',  ( -7.543042896288979726, 1380.366160256679905, 209.1217757912289983 ) ) ;
#32681 = CARTESIAN_POINT ( 'NONE',  ( 20.59987047751410216, 1509.677367640170132, 230.5839189361119850 ) ) ;
#32683 = ORIENTED_EDGE ( 'NONE', *, *, #3458, .F. ) ;
#32682 = CARTESIAN_POINT ( 'NONE',  ( -43.42514567895799615, 1379.701639055019996, 233.3025972862479875 ) ) ;
#32684 = VERTEX_POINT ( 'NONE', #49572 ) ;
#32685 = CARTESIAN_POINT ( 'NONE',  ( 11.30148062330549941, 1434.205170771390158, 151.5393079379209951 ) ) ;
#32686 = CARTESIAN_POINT ( 'NONE',  ( -10.99057042539999962, 1396.296859563830139, 212.4415749538880220 ) ) ;
#32687 = CARTESIAN_POINT ( 'NONE',  ( -20.10955669739999863, 1409.615301589730052, 218.0117348428780133 ) ) ;
#32688 = VERTEX_POINT ( 'NONE', #23783 ) ;
#32689 = CARTESIAN_POINT ( 'NONE',  ( -106.0972438490000087, 1378.969065180200005, 306.6607963967590536 ) ) ;
#32690 = CARTESIAN_POINT ( 'NONE',  ( -27.59578993569999739, 1509.876726607029923, 201.0523566146180201 ) ) ;
#32691 = CARTESIAN_POINT ( 'NONE',  ( 3.829164871872719811, 1515.551704201149960, 206.7918886313289875 ) ) ;
#32693 = CARTESIAN_POINT ( 'NONE',  ( -14.07629452796359892, 1509.199332581739782, 183.4924235105400214 ) ) ;
#32692 = DIRECTION ( 'NONE',  ( -0.9993779840209170429, 0.0009463042317009280006, 0.03525265327019704714 ) ) ;
#32694 = CARTESIAN_POINT ( 'NONE',  ( 5.445834981259999985, 1449.233209377699950, 184.7342386783979862 ) ) ;
#32695 = CARTESIAN_POINT ( 'NONE',  ( -4.990022623493119980, 1464.266792026490066, 199.7730999070479925 ) ) ;
#32696 = CARTESIAN_POINT ( 'NONE',  ( 1.690753242990000071, 1418.551567007509902, 204.1881961068189923 ) ) ;
#32697 =( NAMED_UNIT ( * ) PLANE_ANGLE_UNIT ( ) SI_UNIT ( $, .RADIAN. ) );
#32698 = CARTESIAN_POINT ( 'NONE',  ( 7.500488151212729271, 1396.174983287849955, 201.0066138490270191 ) ) ;
#32699 = CARTESIAN_POINT ( 'NONE',  ( 0.5943821362729999613, 1416.311719779230089, 190.5346383329979858 ) ) ;
#32700 = CARTESIAN_POINT ( 'NONE',  ( 11.76831692830000087, 1432.246165101169936, 150.8114755703979881 ) ) ;
#32701 = CARTESIAN_POINT ( 'NONE',  ( 5.561506164031474242, 1509.113139076760490, 180.2055687771843679 ) ) ;
#32702 = ORIENTED_EDGE ( 'NONE', *, *, #56884, .F. ) ;
#32703 = CARTESIAN_POINT ( 'NONE',  ( 13.15418294748539907, 1434.930549361600015, 149.6534202118089922 ) ) ;
#32704 = ORIENTED_EDGE ( 'NONE', *, *, #86501, .F. ) ;
#32705 = ORIENTED_EDGE ( 'NONE', *, *, #55628, .T. ) ;
#32706 = CARTESIAN_POINT ( 'NONE',  ( 13.44021863898581159, 1444.325653863644675, 169.3641315964260343 ) ) ;
#32707 = CARTESIAN_POINT ( 'NONE',  ( -6.622597241890000319, 1464.346823720030216, 234.5437523557980057 ) ) ;
#32708 = CARTESIAN_POINT ( 'NONE',  ( -12.81144342830000049, 1416.820969729830040, 196.2462494151980081 ) ) ;
#32709 = CARTESIAN_POINT ( 'NONE',  ( -1.124894088365000044, 1517.194816588360027, 216.0733631026070043 ) ) ;
#32710 = CARTESIAN_POINT ( 'NONE',  ( -8.412838876992196901, 1511.396718925154573, 213.7904301685088342 ) ) ;
#32711 = EDGE_LOOP ( 'NONE', ( #18769, #21114, #39176, #30064 ) ) ;
#32712 = CARTESIAN_POINT ( 'NONE',  ( -12.75671326420000007, 1503.496710435090108, 208.6968438420659879 ) ) ;
#32713 = DIRECTION ( 'NONE',  ( 0.000000000000000000, 1.000000000000000000, 0.000000000000000000 ) ) ;
#32714 = CARTESIAN_POINT ( 'NONE',  ( -26.93900968170000354, 1377.750345454750004, 210.6882938058390096 ) ) ;
#32715 = EDGE_CURVE ( 'NONE', #59085, #59795, #50125, .T. ) ;
#32716 =( BOUNDED_SURFACE ( )  B_SPLINE_SURFACE ( 1, 2, ( 
 ( #78205, #104514, #35650, #103958, #27255, #78766, #2082 ),
 ( #102834, #96110, #70955, #19384, #105070, #28359, #26128 ) ),
 .UNSPECIFIED., .F., .F., .F. ) 
 B_SPLINE_SURFACE_WITH_KNOTS ( ( 2, 2 ),
 ( 3, 2, 2, 3 ),
 ( -10000.00000000000000, 10000.00000000000000 ),
 ( 2.628620570831615044, 3.141592653589790007, 4.712388980384689674, 5.770213224422409581 ),
 .UNSPECIFIED. ) 
 GEOMETRIC_REPRESENTATION_ITEM ( )  RATIONAL_B_SPLINE_SURFACE ( (
 ( 0.8711730262221800691, 0.9043503973637049276, 1.000000000000000000, 0.7071067811865480168, 1.000000000000000000, 0.8027563838226560167, 0.8711730262223089660),
 ( 0.8711730262221800691, 0.9043503973637049276, 1.000000000000000000, 0.7071067811865480168, 1.000000000000000000, 0.8027563838226560167, 0.8711730262223089660) ) ) 
 REPRESENTATION_ITEM ( '' )  SURFACE ( )  );
#32717 = ORIENTED_EDGE ( 'NONE', *, *, #76082, .F. ) ;
#32718 = CARTESIAN_POINT ( 'NONE',  ( -5.786837717054999608, 1517.040132827679827, 205.8646253294070050 ) ) ;
#32719 = ORIENTED_EDGE ( 'NONE', *, *, #11821, .F. ) ;
#32720 = CARTESIAN_POINT ( 'NONE',  ( -2.292217048824999992, 1516.941178807709775, 209.1350424789999920 ) ) ;
#32721 = CARTESIAN_POINT ( 'NONE',  ( -20.06869840700000296, 1507.849569109330105, 229.0200580499979992 ) ) ;
#32722 = EDGE_CURVE ( 'NONE', #90510, #84504, #59622, .T. ) ;
#32723 = CARTESIAN_POINT ( 'NONE',  ( -11.06559390560000011, 1410.233130097329877, 188.8575565919979908 ) ) ;
#32724 = CARTESIAN_POINT ( 'NONE',  ( -1.261572150459999930, 1410.336495002929951, 232.9947536822979828 ) ) ;
#32726 = ORIENTED_EDGE ( 'NONE', *, *, #21547, .F. ) ;
#32725 = CARTESIAN_POINT ( 'NONE',  ( 0.05448001190707260633, 1416.221314539489867, 227.1460076434290158 ) ) ;
#32727 = CARTESIAN_POINT ( 'NONE',  ( 18.24053064509999800, 1425.259887461229937, 223.9475156350980285 ) ) ;
#32728 = CARTESIAN_POINT ( 'NONE',  ( -14.95528230852240092, 1508.551704408389924, 210.3622119209300081 ) ) ;
#32729 = CARTESIAN_POINT ( 'NONE',  ( -73.61402272690000359, 1384.068034839990105, 298.8931160141590340 ) ) ;
#32730 = CARTESIAN_POINT ( 'NONE',  ( -0.2608622107377010502, 1466.756006659810055, 235.6083744819270009 ) ) ;
#32731 = CARTESIAN_POINT ( 'NONE',  ( 10.68754207573829973, 1410.138259118899896, 270.3681159542280170 ) ) ;
#32732 = CARTESIAN_POINT ( 'NONE',  ( -4.999456428534999830, 1516.830644417779922, 213.7431138541670066 ) ) ;
#32733 = CARTESIAN_POINT ( 'NONE',  ( 24.06407462299999978, 1410.713862210129946, 208.8709579670279766 ) ) ;
#32734 = CARTESIAN_POINT ( 'NONE',  ( 11.71533056565333197, 1414.421228241719973, 209.8579518281819674 ) ) ;
#32735 = CARTESIAN_POINT ( 'NONE',  ( 1.542378980109999853, 1442.042834985789796, 218.9497927206290058 ) ) ;
#32736 = CARTESIAN_POINT ( 'NONE',  ( 6.648352156676600622, 1508.610125823030103, 216.2179235647060125 ) ) ;
#32737 = CARTESIAN_POINT ( 'NONE',  ( 1.137296650804999976, 1516.908147884120126, 210.8236964273370120 ) ) ;
#32738 = CARTESIAN_POINT ( 'NONE',  ( 6.832964021560000489, 1409.413060387330006, 271.1218459616979999 ) ) ;
#32739 = CARTESIAN_POINT ( 'NONE',  ( 17.61566626013499004, 1524.599984580802129, 180.6473472415456456 ) ) ;
#32740 = CARTESIAN_POINT ( 'NONE',  ( 3.194497190068566361, 1421.833025343917370, 139.1411856790333843 ) ) ;
#32742 = VERTEX_POINT ( 'NONE', #102146 ) ;
#32741 = CARTESIAN_POINT ( 'NONE',  ( -43.21308294339999634, 1386.785232113230222, 247.4412949693590065 ) ) ;
#32743 = CARTESIAN_POINT ( 'NONE',  ( -46.76181045157920124, 1385.141772473130004, 255.0711131765360165 ) ) ;
#32744 = CARTESIAN_POINT ( 'NONE',  ( -2.831258933819999884E-09, 1475.995240999430052, 267.2559760609979662 ) ) ;
#32745 = CARTESIAN_POINT ( 'NONE',  ( 32.97913964219439720, 1511.187213306747708, 220.2739374644211807 ) ) ;
#32746 = DIRECTION ( 'NONE',  ( -1.755985294532469921E-16, 1.000000000000000000, -1.338183447452831989E-16 ) ) ;
#32747 = CARTESIAN_POINT ( 'NONE',  ( 10.70463268489986142, 1472.030523703590006, 213.2176825260488613 ) ) ;
#32748 = CARTESIAN_POINT ( 'NONE',  ( 11.92256370189999792, 1421.800997465520140, 206.9479557017089917 ) ) ;
#32749 = CARTESIAN_POINT ( 'NONE',  ( 12.13495036573499952, 1511.961073825299991, 225.2306057305669924 ) ) ;
#32751 = PLANE ( 'NONE',  #3069 ) ;
#32750 = DIRECTION ( 'NONE',  ( 5.980589973904019347E-17, -1.000000000000000000, 1.736889445713099699E-16 ) ) ;
#32752 = CARTESIAN_POINT ( 'NONE',  ( 3.272667022753707577, 1519.551704408389924, 229.2073556998901438 ) ) ;
#32753 = DIRECTION ( 'NONE',  ( 0.4763271851929161138, 0.000000000000000000, 0.8792681119238848764 ) ) ;
#32754 = ORIENTED_EDGE ( 'NONE', *, *, #48262, .T. ) ;
#32755 = CARTESIAN_POINT ( 'NONE',  ( 6.552897366944999469, 1516.858146885269889, 202.5651945608169910 ) ) ;
#32756 = CARTESIAN_POINT ( 'NONE',  ( -0.2697921844439999939, 1467.610413176630118, 229.6924542576979889 ) ) ;
#32757 = CARTESIAN_POINT ( 'NONE',  ( 19.88034263189999962, 1455.027112605630009, 224.4525163018979868 ) ) ;
#32758 = CARTESIAN_POINT ( 'NONE',  ( 8.660742842291162091, 1437.358295876703323, 153.3239294377561635 ) ) ;
#32759 = FACE_OUTER_BOUND ( 'NONE', #18400, .T. ) ;
#32760 = CARTESIAN_POINT ( 'NONE',  ( -0.4215884677550009729, 1444.753357002690109, 218.0930000387590155 ) ) ;
#32761 = CARTESIAN_POINT ( 'NONE',  ( 7.489142240313679366, 1416.917596226978048, 230.9382929016721562 ) ) ;
#32762 = CARTESIAN_POINT ( 'NONE',  ( 30.86131930287799818, 1436.470231434929929, 136.6051523533310217 ) ) ;
#32763 = CARTESIAN_POINT ( 'NONE',  ( 40.09012144279480339, 1445.376175965129960, 136.9018312957269927 ) ) ;
#32764 = CARTESIAN_POINT ( 'NONE',  ( -23.28544946739999943, 1434.322615792679926, 214.3287644136879919 ) ) ;
#32765 = CARTESIAN_POINT ( 'NONE',  ( -11.75704297446499957, 1511.932705841380084, 218.3428388715770154 ) ) ;
#32766 = CARTESIAN_POINT ( 'NONE',  ( -108.8461099330000081, 1385.969494106900129, 297.2525754554590094 ) ) ;
#32767 = CARTESIAN_POINT ( 'NONE',  ( 12.05022103600000172, 1508.335016562029978, 184.5151076142980173 ) ) ;
#32768 = CARTESIAN_POINT ( 'NONE',  ( 18.66420869458043441, 1526.382868172864164, 185.4599087859680537 ) ) ;
#32769 = CARTESIAN_POINT ( 'NONE',  ( -34.27281677136750915, 1458.542448025342537, 269.5216919828922073 ) ) ;
#32770 = ORIENTED_EDGE ( 'NONE', *, *, #33158, .F. ) ;
#32771 = CARTESIAN_POINT ( 'NONE',  ( -8.178306764501339643, 1439.185977283359989, 206.0664987394139871 ) ) ;
#32772 = CARTESIAN_POINT ( 'NONE',  ( 15.27152964737910068, 1506.433683733550197, 193.3098315259690025 ) ) ;
#32773 = CARTESIAN_POINT ( 'NONE',  ( -1.925297170580940076, 1519.551704408389924, 187.5582988486569889 ) ) ;
#32774 = CARTESIAN_POINT ( 'NONE',  ( -8.805428988939999257, 1497.713060387329961, 229.3821491682979854 ) ) ;
#32775 = CARTESIAN_POINT ( 'NONE',  ( -0.02518341440730000394, 1415.404722957129934, 233.4400562564979964 ) ) ;
#32776 = CARTESIAN_POINT ( 'NONE',  ( -12.76951649852674286, 1444.992622299949517, 185.9723966557366737 ) ) ;
#32777 = CARTESIAN_POINT ( 'NONE',  ( -9.062501693986670048, 1438.222286192869888, 210.0833190316829757 ) ) ;
#32778 = CARTESIAN_POINT ( 'NONE',  ( -2.898098007869549964, 1515.492902828930028, 213.2585957736860109 ) ) ;
#32779 = CARTESIAN_POINT ( 'NONE',  ( -6.910691058390185937, 1416.743833086882205, 231.4108548000287726 ) ) ;
#32780 = CARTESIAN_POINT ( 'NONE',  ( -18.84855559419433391, 1451.021439095374490, 146.7293775064046599 ) ) ;
#32781 = CARTESIAN_POINT ( 'NONE',  ( 25.74428607489999976, 1435.913748434279796, 136.6865143993979927 ) ) ;
#32782 = CARTESIAN_POINT ( 'NONE',  ( -4.532544388959999893, 1433.779930133089920, 212.7417843401189828 ) ) ;
#32784 = ORIENTED_EDGE ( 'NONE', *, *, #35850, .F. ) ;
#32783 = CARTESIAN_POINT ( 'NONE',  ( -14.55268370649999987, 1410.361136006629977, 226.7453334963979898 ) ) ;
#32785 = CARTESIAN_POINT ( 'NONE',  ( 0.3106767230383539746, 1415.088506334920112, 192.0574112331409822 ) ) ;
#32786 = CARTESIAN_POINT ( 'NONE',  ( -12.11621817362850351, 1378.266527857301298, 211.6883570102415035 ) ) ;
#32787 = VERTEX_POINT ( 'NONE', #33290 ) ;
#32788 = VERTEX_POINT ( 'NONE', #25427 ) ;
#32789 = FACE_OUTER_BOUND ( 'NONE', #40150, .T. ) ;
#32790 = CARTESIAN_POINT ( 'NONE',  ( -18.66420869458028520, 1526.382868172864164, 232.7837831374281166 ) ) ;
#32792 = CARTESIAN_POINT ( 'NONE',  ( -16.58880512860000067, 1456.884093369330003, 220.8293426371980104 ) ) ;
#32791 = CARTESIAN_POINT ( 'NONE',  ( 1.660254716250000095, 1454.717553612689926, 218.3876423414490091 ) ) ;
#32793 = CARTESIAN_POINT ( 'NONE',  ( -20.53924275249999809, 1507.908979316930072, 189.7573387548980008 ) ) ;
#32794 = CARTESIAN_POINT ( 'NONE',  ( -11.71913435010000093, 1433.163605237980164, 150.8449725526980103 ) ) ;
#32795 = CARTESIAN_POINT ( 'NONE',  ( -15.23481017189999953, 1380.318026959200097, 210.0536512759839809 ) ) ;
#32796 = CARTESIAN_POINT ( 'NONE',  ( 9.624923068494529943, 1463.973964823269853, 211.0293340011560019 ) ) ;
#32797 = CARTESIAN_POINT ( 'NONE',  ( 7.368463984539999956, 1423.734805372980190, 213.0570616533089776 ) ) ;
#32798 = CARTESIAN_POINT ( 'NONE',  ( -24.34803299149999845, 1439.482366230929983, 212.0309832708680062 ) ) ;
#32799 = CARTESIAN_POINT ( 'NONE',  ( -3.345456442099850047, 1454.253772392629799, 199.1892521207759899 ) ) ;
#32800 = CARTESIAN_POINT ( 'NONE',  ( -0.1155235852791031970, 1467.141897078556440, 235.6414018107566335 ) ) ;
#32801 = CARTESIAN_POINT ( 'NONE',  ( 6.474683829332638751, 1363.643362496321288, 209.6218459617148824 ) ) ;
#32802 = CARTESIAN_POINT ( 'NONE',  ( -20.18749645201030063, 1509.735829383545934, 186.8627948558383878 ) ) ;
#32804 = VERTEX_POINT ( 'NONE', #85341 ) ;
#32803 = CARTESIAN_POINT ( 'NONE',  ( -9.833393186232900263, 1517.151704408390060, 212.5077547680540135 ) ) ;
#32805 = ORIENTED_EDGE ( 'NONE', *, *, #35047, .F. ) ;
#32806 = CARTESIAN_POINT ( 'NONE',  ( -11.77540867291269855, 1427.269330905989818, 146.7706912077400148 ) ) ;
#32807 = CARTESIAN_POINT ( 'NONE',  ( -18.90194474967839966, 1503.740679335620143, 222.2659978651250015 ) ) ;
#32808 = CARTESIAN_POINT ( 'NONE',  ( -5.260636025280000183, 1472.387947547730164, 270.3705385644980197 ) ) ;
#32809 = CARTESIAN_POINT ( 'NONE',  ( 0.4943681453122752423, 1473.359364695990507, 219.3321834821998664 ) ) ;
#32810 = CARTESIAN_POINT ( 'NONE',  ( -122.8636594665494499, 1366.350733876287677, 299.0518252276506814 ) ) ;
#32811 = CARTESIAN_POINT ( 'NONE',  ( -14.61959290290118041, 1420.357143390019928, 213.8552925859152367 ) ) ;
#32812 = CARTESIAN_POINT ( 'NONE',  ( 21.45452449210000267, 1497.713060387329961, 205.0582954851479940 ) ) ;
#32813 = CARTESIAN_POINT ( 'NONE',  ( -8.154724234939999761, 1384.732207671340120, 199.6512008194690111 ) ) ;
#32814 = CARTESIAN_POINT ( 'NONE',  ( 18.29188182340000068, 1431.768652859389704, 209.1218459616989946 ) ) ;
#32815 = CARTESIAN_POINT ( 'NONE',  ( -6.833118095721640195, 1429.964654908410012, 222.3013511789650067 ) ) ;
#32816 = CARTESIAN_POINT ( 'NONE',  ( 11.57989268124586424, 1366.469131039695867, 208.3718459617010978 ) ) ;
#32817 = CARTESIAN_POINT ( 'NONE',  ( -9.152553986288870291, 1448.325309252199986, 210.6317879819130212 ) ) ;
#32818 = CARTESIAN_POINT ( 'NONE',  ( -15.41942199670529945, 1408.188993866129977, 269.2062666358880278 ) ) ;
#32819 = CARTESIAN_POINT ( 'NONE',  ( -13.21521023968930031, 1435.711572018790093, 150.5102260760120032 ) ) ;
#32820 = VERTEX_POINT ( 'NONE', #15383 ) ;
#32821 = CARTESIAN_POINT ( 'NONE',  ( -4.329089011153670619, 1515.078531749479907, 210.5455323891260093 ) ) ;
#32822 = VERTEX_POINT ( 'NONE', #110561 ) ;
#32823 = ORIENTED_EDGE ( 'NONE', *, *, #44729, .T. ) ;
#32824 = CARTESIAN_POINT ( 'NONE',  ( 4.882230504881198030, 1422.395003669154676, 184.3285600118643117 ) ) ;
#32825 = CARTESIAN_POINT ( 'NONE',  ( 7.596893798666170206, 1424.854153163179944, 194.2789038821860288 ) ) ;
#32826 = CARTESIAN_POINT ( 'NONE',  ( -5.772727946874999461, 1516.691414181030041, 212.5791125756269935 ) ) ;
#32827 = CARTESIAN_POINT ( 'NONE',  ( -16.72315470559999895, 1470.469491759329912, 188.8178631691980058 ) ) ;
#32828 = CARTESIAN_POINT ( 'NONE',  ( -16.93883337398300171, 1507.634953145470035, 230.1482688801679899 ) ) ;
#32829 = ORIENTED_EDGE ( 'NONE', *, *, #26542, .F. ) ;
#32830 = CARTESIAN_POINT ( 'NONE',  ( -102.0335792520000098, 1376.985289779790037, 301.2067031052590664 ) ) ;
#32831 = CARTESIAN_POINT ( 'NONE',  ( 1.124289655455000148, 1517.184063036290127, 202.5579304082170040 ) ) ;
#32832 = CARTESIAN_POINT ( 'NONE',  ( -109.6086345746109885, 1383.178240054900016, 311.2147542219479988 ) ) ;
#32833 = CARTESIAN_POINT ( 'NONE',  ( -28.80308794735720213, 1384.553337952709853, 204.9648910289260186 ) ) ;
#32835 = B_SPLINE_CURVE_WITH_KNOTS ( 'NONE', 3,
 ( #21069, #46874, #81002, #38436, #27289, #70432 ),
 .UNSPECIFIED., .F., .F.,
 ( 4, 2, 4 ),
 ( 0.000000000000000000, 0.4821770457261087550, 0.9643540914522175100 ),
 .UNSPECIFIED. ) ;
#32834 = FACE_OUTER_BOUND ( 'NONE', #88302, .T. ) ;
#32836 = DIRECTION ( 'NONE',  ( 0.9455185755993178454, 0.000000000000000000, -0.3255681544571539243 ) ) ;
#32838 = VERTEX_POINT ( 'NONE', #33847 ) ;
#32837 = CARTESIAN_POINT ( 'NONE',  ( -38.59236949370799863, 1443.548215515760148, 137.1678974980329997 ) ) ;
#32839 = CARTESIAN_POINT ( 'NONE',  ( 11.27867428310018560, 1425.794442006550980, 197.9026106389715380 ) ) ;
#32840 = CARTESIAN_POINT ( 'NONE',  ( 26.14369035709999878, 1488.683671327730053, 214.7624555471579981 ) ) ;
#32841 = AXIS2_PLACEMENT_3D ( 'NONE', #46499, #96331, #88483 ) ;
#32842 = CARTESIAN_POINT ( 'NONE',  ( 5.808733308747313195, 1474.842457401947740, 269.6417025878172353 ) ) ;
#32843 = LINE ( 'NONE', #31198, #59248 ) ;
#32844 = CARTESIAN_POINT ( 'NONE',  ( -10.96015512746500065, 1516.551704408390151, 193.2119433744669834 ) ) ;
#32845 = CARTESIAN_POINT ( 'NONE',  ( -24.46154330250000086, 1442.364448987709920, 211.0683006204080243 ) ) ;
#32846 = CARTESIAN_POINT ( 'NONE',  ( 7.338753830235000386, 1517.184383877180153, 211.4127322367170052 ) ) ;
#32847 = CARTESIAN_POINT ( 'NONE',  ( -68.78553819374839406, 1379.747969107289919, 280.2964879544919654 ) ) ;
#32848 = CIRCLE ( 'NONE', #755, 1.500000000000001332 ) ;
#32849 = CARTESIAN_POINT ( 'NONE',  ( -0.3328314641405109575, 1452.976685807730291, 183.2631399573310205 ) ) ;
#32850 = DIRECTION ( 'NONE',  ( -0.03508471684983520411, 0.9993076967569471947, -0.01237698856314710383 ) ) ;
#32851 = CARTESIAN_POINT ( 'NONE',  ( -13.08238251380000072, 1414.913528139129994, 220.2039091924980028 ) ) ;
#32852 = CARTESIAN_POINT ( 'NONE',  ( 1.117840086735000016, 1516.949031626070109, 207.4047068479870006 ) ) ;
#32853 = ORIENTED_EDGE ( 'NONE', *, *, #65808, .F. ) ;
#32854 = FACE_OUTER_BOUND ( 'NONE', #107207, .T. ) ;
#32855 = CARTESIAN_POINT ( 'NONE',  ( -10.24275455859999973, 1472.071912135389994, 207.8889228267089777 ) ) ;
#32856 = CARTESIAN_POINT ( 'NONE',  ( -19.59641516460481725, 1457.071779919169330, 225.8968562730828467 ) ) ;
#32857 = ORIENTED_EDGE ( 'NONE', *, *, #78858, .T. ) ;
#32858 = CARTESIAN_POINT ( 'NONE',  ( -3.351013500467394213, 1524.082740465118604, 242.0157168755361852 ) ) ;
#32859 = CARTESIAN_POINT ( 'NONE',  ( 12.85396610232849923, 1434.713524430809912, 149.4748486273309993 ) ) ;
#32860 = B_SPLINE_SURFACE_WITH_KNOTS ( 'NONE', 5, 5, ( 
 ( #39514, #3184, #73688, #19942, #88265, #63106 ),
 ( #20477, #72049, #29443, #63642, #67490, #101595 ),
 ( #50668, #91569, #58530, #5912, #40609, #31650 ),
 ( #83711, #56874, #109479, #14844, #15391, #23245 ),
 ( #32756, #110570, #42267, #65832, #24879, #84800 ),
 ( #101046, #83169, #41164, #91003, #40059, #108920 ) ),
 .UNSPECIFIED., .F., .F., .F.,
 ( 6, 6 ),
 ( 6, 6 ),
 ( 19.55448171529999968, 88.89713672540000289 ),
 ( -2.775557561569999727E-17, 1.000000000000000000 ),
 .UNSPECIFIED. ) ;
#32861 = CARTESIAN_POINT ( 'NONE',  ( -4.074500880610250064, 1440.601538448055862, 185.2207594585182164 ) ) ;
#32862 = CARTESIAN_POINT ( 'NONE',  ( -9.467443545490001000, 1415.183427459279983, 206.9475390216489927 ) ) ;
#32863 = AXIS2_PLACEMENT_3D ( 'NONE', #105847, #54896, #72254 ) ;
#32864 = CARTESIAN_POINT ( 'NONE',  ( -11.44902708475428987, 1425.804265263478555, 139.1023607573540630 ) ) ;
#32865 = CARTESIAN_POINT ( 'NONE',  ( 6.435066429969999113, 1488.114327637990073, 199.4146561316890143 ) ) ;
#32866 = LINE ( 'NONE', #92779, #50169 ) ;
#32867 = CARTESIAN_POINT ( 'NONE',  ( -15.06903107870000191, 1410.389868148830146, 226.7125060204980116 ) ) ;
#32868 = ADVANCED_FACE ( 'NONE', ( #87443 ), #10405, .T. ) ;
#32870 = CARTESIAN_POINT ( 'NONE',  ( 0.000000000000000000, 1523.051704408389696, 185.4225825198192013 ) ) ;
#32869 = CARTESIAN_POINT ( 'NONE',  ( -0.7369042090349989804, 1517.080322339569875, 214.1333973382469935 ) ) ;
#32871 = CARTESIAN_POINT ( 'NONE',  ( -8.860943469877430090, 1385.062452151980096, 218.6812855941350051 ) ) ;
#32872 = CARTESIAN_POINT ( 'NONE',  ( 4.036119644515000715, 1516.647924054489977, 216.4458205765370167 ) ) ;
#32873 = ORIENTED_EDGE ( 'NONE', *, *, #110454, .F. ) ;
#32874 = DIRECTION ( 'NONE',  ( 0.000000000000000000, -1.000000000000000000, 0.000000000000000000 ) ) ;
#32875 = B_SPLINE_SURFACE_WITH_KNOTS ( 'NONE', 5, 3, ( 
 ( #45823, #45273, #88901, #79411 ),
 ( #54769, #71037, #96205, #97299 ),
 ( #2723, #21669, #3829, #37403 ),
 ( #38489, #36845, #62079, #37957 ),
 ( #63728, #28450, #62644, #72666 ),
 ( #72137, #97838, #106792, #79956 ) ),
 .UNSPECIFIED., .F., .F., .F.,
 ( 6, 6 ),
 ( 4, 4 ),
 ( 0.000000000000000000, 52.98902693510000006 ),
 ( 37.69911184309999896, 40.20365518519999881 ),
 .UNSPECIFIED. ) ;
#32876 = CARTESIAN_POINT ( 'NONE',  ( -17.16826720739999956, 1420.250473903940019, 203.6854009021189995 ) ) ;
#32877 = CARTESIAN_POINT ( 'NONE',  ( 0.9849188036980001115, 1419.502007416729839, 184.7914211646979936 ) ) ;
#32878 = B_SPLINE_CURVE_WITH_KNOTS ( 'NONE', 3,
 ( #1899, #104884, #45559, #62361, #52846, #36035, #96485, #79700, #19766, #53967, #97585, #3005, #104330, #11387, #71326, #61809, #70225, #106532, #27623, #105440, #46105, #80235, #2459, #4094, #55053, #28729, #88649, #62934, #37678, #20857, #3555, #86972, #97046, #71882, #20309, #89180, #54512, #95931, #29274, #19191, #63466, #12472, #64007, #53395, #46656, #38219, #98119, #72401 ),
 .UNSPECIFIED., .F., .F.,
 ( 4, 2, 2, 1, 1, 1, 1, 2, 2, 2, 2, 2, 1, 1, 1, 1, 2, 2, 2, 2, 2, 1, 1, 1, 1, 1, 1, 2, 2, 2, 4 ),
 ( 0.000000000000000000, 0.1249999999999676648, 0.1874999999999503175, 0.2187499999999427680, 0.2343749999999387990, 0.2421874999999371336, 0.2460937499999352185, 0.2480468749999343858, 0.2499999999999335532, 0.3749999999998849809, 0.4374999999998616662, 0.4687499999998501754, 0.4843749999998440137, 0.4921874999998419598, 0.4960937499998416267, 0.4980468749998407385, 0.4990234374998410161, 0.4999999999998412381, 0.6249999999996845856, 0.6874999999996069810, 0.7187499999995685673, 0.7343749999995491384, 0.7421874999995393685, 0.7460937499995340394, 0.7480468749995313749, 0.7490234374995307087, 0.7495117187495299316, 0.7497558593745294875, 0.7499999999995291544, 0.8749999999997645217, 1.000000000000000000 ),
 .UNSPECIFIED. ) ;
#32879 = CARTESIAN_POINT ( 'NONE',  ( -2.829326390389999890, 1474.515727672689991, 219.0106651408090102 ) ) ;
#32880 = CARTESIAN_POINT ( 'NONE',  ( 2.038646110889595242, 1525.960063244516959, 177.0579350083065435 ) ) ;
#32881 = CARTESIAN_POINT ( 'NONE',  ( -21.47567121439999838, 1505.309716411789850, 210.5476439721289807 ) ) ;
#32882 = CARTESIAN_POINT ( 'NONE',  ( -11.28893270251630021, 1471.181900745179746, 207.4356590764699888 ) ) ;
#32883 = CARTESIAN_POINT ( 'NONE',  ( -5.592450460805372003, 1508.275704380422212, 220.2479065938019573 ) ) ;
#32884 = CARTESIAN_POINT ( 'NONE',  ( 17.25473568693964665, 1422.487072245637364, 226.6732862807842821 ) ) ;
#32885 = CARTESIAN_POINT ( 'NONE',  ( -2.409034624560000282, 1512.051704408390151, 204.7134966871890072 ) ) ;
#32886 = CARTESIAN_POINT ( 'NONE',  ( 39.91818200059610433, 1440.913060366189939, 259.1711454722760095 ) ) ;
#32888 = CARTESIAN_POINT ( 'NONE',  ( 3.206304093069999972, 1492.460538144390057, 188.3278363003989853 ) ) ;
#32887 = CARTESIAN_POINT ( 'NONE',  ( -14.20981681145070041, 1419.004817284329874, 200.1611811227300279 ) ) ;
#32889 = CARTESIAN_POINT ( 'NONE',  ( 4.709520687179999499, 1480.407452823689937, 228.9869292435990076 ) ) ;
#32890 = VERTEX_POINT ( 'NONE', #45461 ) ;
#32891 = EDGE_LOOP ( 'NONE', ( #31100, #76346, #2455, #81173 ) ) ;
#32892 = DIRECTION ( 'NONE',  ( 2.148885482424154438E-07, 0.03085800255252074339, 0.9995237784457268182 ) ) ;
#32893 = CARTESIAN_POINT ( 'NONE',  ( -15.31790971930000111, 1507.704306114589826, 209.3792549816630242 ) ) ;
#32894 = CARTESIAN_POINT ( 'NONE',  ( 7.854266064069999942, 1423.715025901959962, 195.8676021965990230 ) ) ;
#32895 = CARTESIAN_POINT ( 'NONE',  ( -1966.210325831229966, 11216.44053380570040, -21.67665461820280015 ) ) ;
#32896 = DIRECTION ( 'NONE',  ( -0.7835778918569903384, -0.02736314294039966441, -0.6206907005919922726 ) ) ;
#32897 = B_SPLINE_CURVE_WITH_KNOTS ( 'NONE', 3,
 ( #3872, #37999, #63769, #28496, #96812, #19526, #97885, #21159, #12791, #88401, #53161, #35795, #18966, #87302, #10595, #78917, #30690, #82752, #31240 ),
 .UNSPECIFIED., .F., .F.,
 ( 4, 3, 3, 3, 3, 3, 4 ),
 ( -136.9023999274239998, -136.8784091759999910, -136.4141923412300059, -135.9934039197389950, -135.7136470572270071, -135.3701148500000215, -135.0843709324570057 ),
 .UNSPECIFIED. ) ;
#32898 = CARTESIAN_POINT ( 'NONE',  ( -31.32995031131184760, 1523.678648413191695, 221.9013357025048663 ) ) ;
#32899 = CARTESIAN_POINT ( 'NONE',  ( -4.217997304759999899, 1515.470303964289997, 208.3798484374839859 ) ) ;
#32900 = CARTESIAN_POINT ( 'NONE',  ( -59.78493395224469964, 1383.796987562569939, 280.2502008579959920 ) ) ;
#32901 = EDGE_CURVE ( 'NONE', #39470, #80762, #31201, .T. ) ;
#32902 = EDGE_CURVE ( 'NONE', #48553, #88847, #94520, .T. ) ;
#32903 = CARTESIAN_POINT ( 'NONE',  ( -12.27023095390000051, 1416.839692139930094, 194.6640140145979956 ) ) ;
#32904 = LINE ( 'NONE', #8251, #42886 ) ;
#32905 = CARTESIAN_POINT ( 'NONE',  ( 10.89683788740839887, 1490.584122941180112, 210.4541128349080168 ) ) ;
#32906 = EDGE_CURVE ( 'NONE', #15707, #21322, #84533, .T. ) ;
#32908 = ORIENTED_EDGE ( 'NONE', *, *, #66546, .F. ) ;
#32907 = CARTESIAN_POINT ( 'NONE',  ( 1.538502245710000160, 1455.675329834489958, 218.5739180266590154 ) ) ;
#32909 = CARTESIAN_POINT ( 'NONE',  ( -1.906501312376459942E-08, 1515.051704408389924, 213.4516374609670208 ) ) ;
#32910 = CARTESIAN_POINT ( 'NONE',  ( -73.11457663749999369, 1384.756954744069844, 272.3426209276589702 ) ) ;
#32911 = EDGE_CURVE ( 'NONE', #76707, #29958, #35170, .T. ) ;
#32912 = CARTESIAN_POINT ( 'NONE',  ( 4.987078442593329441, 1508.551704408389924, 206.6339108768089829 ) ) ;
#32913 = ORIENTED_EDGE ( 'NONE', *, *, #61460, .T. ) ;
#32914 = VERTEX_POINT ( 'NONE', #99115 ) ;
#32915 = ADVANCED_FACE ( 'NONE', ( #75609 ), #104289, .F. ) ;
#32916 = FACE_OUTER_BOUND ( 'NONE', #6822, .T. ) ;
#32917 = CARTESIAN_POINT ( 'NONE',  ( -4.082779675200169933, 1515.071395204220153, 205.5354858456919942 ) ) ;
#32919 = CARTESIAN_POINT ( 'NONE',  ( 3.092979971720000165, 1469.622821628089923, 189.3242126552989930 ) ) ;
#32918 = DIRECTION ( 'NONE',  ( -0.9455185755993178454, 0.000000000000000000, 0.3255681544571537578 ) ) ;
#32920 = AXIS2_PLACEMENT_3D ( 'NONE', #54132, #45730, #38393 ) ;
#32921 = CARTESIAN_POINT ( 'NONE',  ( -8.728835042969999236, 1462.533594714489936, 204.2920097199789780 ) ) ;
#32922 = CARTESIAN_POINT ( 'NONE',  ( -105.0999857459999873, 1379.412654380750155, 302.9955102991589797 ) ) ;
#32923 = CARTESIAN_POINT ( 'NONE',  ( -32.38845791999490586, 1523.456872492435195, 216.1254071228449902 ) ) ;
#32924 = B_SPLINE_CURVE_WITH_KNOTS ( 'NONE', 3,
 ( #14318, #31128, #6484, #107839, #64210, #23271, #74265, #30019, #21056, #38967, #13209, #31678, #14868, #55815, #39540, #40636, #47942, #82647, #74808, #89393, #99978, #48509, #90483, #4822, #40085, #91031, #5939, #65859, #30583, #56351, #83196, #13758, #108952, #63666, #55261, #97780, #46862, #80992, #4298, #38425, #72601, #106729, #98333 ),
 .UNSPECIFIED., .F., .F.,
 ( 4, 3, 3, 3, 3, 3, 3, 3, 3, 3, 3, 3, 3, 3, 4 ),
 ( 3.966820340228049968, 5.122032127245899957, 6.221263424738429748, 7.257200153960000399, 8.081244681909998562, 8.905289209860001165, 9.318356587769999422, 10.01723044449550137, 10.55754830240000075, 11.31812075668910111, 12.00342336190689885, 12.22175150850000058, 12.83982335616149939, 13.41885480076430071, 13.57487840009213897 ),
 .UNSPECIFIED. ) ;
#32925 = CARTESIAN_POINT ( 'NONE',  ( -29.73374635647653008, 1526.349689584397083, 201.0212862843677613 ) ) ;
#32926 = CARTESIAN_POINT ( 'NONE',  ( -16.05960259768179910, 1508.551704408389924, 213.7616175704369823 ) ) ;
#32927 = CARTESIAN_POINT ( 'NONE',  ( -33.36586802512168504, 1512.187213306747481, 216.3367586934473366 ) ) ;
#32928 = CARTESIAN_POINT ( 'NONE',  ( 18.03146720619200138, 1424.667981931974055, 225.2975763146619954 ) ) ;
#32929 = CARTESIAN_POINT ( 'NONE',  ( 4.408868868459999923, 1425.824683875729988, 185.4670087524980033 ) ) ;
#32930 = CARTESIAN_POINT ( 'NONE',  ( -10.96966273854589957, 1432.359729197300112, 151.7701366752919796 ) ) ;
#32931 = CARTESIAN_POINT ( 'NONE',  ( -2.705839759132969924, 1440.724342078179916, 165.1197109057160048 ) ) ;
#32932 = CARTESIAN_POINT ( 'NONE',  ( 5.563540928143850373, 1516.551188145990182, 199.3082484782189852 ) ) ;
#32933 = ORIENTED_EDGE ( 'NONE', *, *, #46780, .F. ) ;
#32935 = EDGE_CURVE ( 'NONE', #18384, #35589, #14743, .T. ) ;
#32934 = CARTESIAN_POINT ( 'NONE',  ( 4.196074440480000121E-15, 1430.453334911130241, 150.3332009510979788 ) ) ;
#32936 = CARTESIAN_POINT ( 'NONE',  ( 18.74257907359240249, 1456.927692655689953, 228.0561368610119928 ) ) ;
#32937 = CARTESIAN_POINT ( 'NONE',  ( -4.552706710259999845, 1475.816573717389929, 203.2240324946190242 ) ) ;
#32938 = CARTESIAN_POINT ( 'NONE',  ( 29.40443212115394189, 1512.187213306747481, 222.0897836382243042 ) ) ;
#32939 = CARTESIAN_POINT ( 'NONE',  ( 20.19452632973207784, 1436.434739331579522, 145.2312131346681667 ) ) ;
#32940 = CARTESIAN_POINT ( 'NONE',  ( -1.342110557989999897, 1416.822690122629865, 228.0800073794979994 ) ) ;
#32941 = CARTESIAN_POINT ( 'NONE',  ( -3.072927222099999689, 1475.870007387389933, 199.1238673863090014 ) ) ;
#32942 = CARTESIAN_POINT ( 'NONE',  ( -105.0227953419999949, 1390.444196973850012, 305.3128289140589686 ) ) ;
#32943 = ADVANCED_FACE ( 'NONE', ( #20615 ), #36341, .F. ) ;
#32944 = CARTESIAN_POINT ( 'NONE',  ( -7.899414352548780549, 1511.275771545139833, 214.6924451503199975 ) ) ;
#32945 = CARTESIAN_POINT ( 'NONE',  ( -8.538839991155660059, 1362.569232148552146, 210.6218459616991936 ) ) ;
#32946 = CARTESIAN_POINT ( 'NONE',  ( -45.63704539349389933, 1440.913071918759897, 268.9748468665420091 ) ) ;
#32947 = CARTESIAN_POINT ( 'NONE',  ( 2.907323806750489847, 1428.844561383579958, 216.8721538760840133 ) ) ;
#32948 = CARTESIAN_POINT ( 'NONE',  ( -1.843107666119999877, 1444.183210091189949, 199.2363500995090249 ) ) ;
#32949 = EDGE_CURVE ( 'NONE', #89343, #69095, #45151, .T. ) ;
#32950 = CARTESIAN_POINT ( 'NONE',  ( -6.562094107424999656, 1517.122674412569950, 208.3832410274270046 ) ) ;
#32951 = CARTESIAN_POINT ( 'NONE',  ( -2.478936252380000038, 1432.480737126569920, 157.5199335589979910 ) ) ;
#32952 = CARTESIAN_POINT ( 'NONE',  ( 4.082703447780033024, 1515.071394417502688, 205.5355069181578358 ) ) ;
#32953 = CARTESIAN_POINT ( 'NONE',  ( 7.430468893321169332, 1426.189551463749922, 212.4985856753800135 ) ) ;
#32954 = EDGE_CURVE ( 'NONE', #32988, #61245, #80557, .T. ) ;
#32955 = CARTESIAN_POINT ( 'NONE',  ( -26.51713393923600037, 1451.737905241030148, 135.8255081778609963 ) ) ;
#32956 = EDGE_LOOP ( 'NONE', ( #73074, #13175, #20956, #10272 ) ) ;
#32957 = CARTESIAN_POINT ( 'NONE',  ( 4.123065267750000373, 1419.629243940029937, 225.6556823394980142 ) ) ;
#32959 = CARTESIAN_POINT ( 'NONE',  ( -14.72576942166499947, 1512.123542805230272, 221.3115653187670091 ) ) ;
#32958 = CARTESIAN_POINT ( 'NONE',  ( -11.30037463203350079, 1491.719108927019988, 206.9447153815449951 ) ) ;
#32960 = CARTESIAN_POINT ( 'NONE',  ( -19.75595483460000068, 1465.302321228290111, 208.1554333590609929 ) ) ;
#32961 = CARTESIAN_POINT ( 'NONE',  ( -21.38445639499393636, 1453.349625645140804, 224.4824140893579170 ) ) ;
#32962 = CARTESIAN_POINT ( 'NONE',  ( -14.47191459792289869, 1379.648775954749908, 208.1784578746709826 ) ) ;
#32963 = DIRECTION ( 'NONE',  ( -0.9455185755993178454, 0.000000000000000000, 0.3255681544571539243 ) ) ;
#32964 = CARTESIAN_POINT ( 'NONE',  ( -5399.190776299624304, 2837.541834147241843, -8134.792049093260175 ) ) ;
#32965 = ORIENTED_EDGE ( 'NONE', *, *, #95240, .F. ) ;
#32966 = FACE_OUTER_BOUND ( 'NONE', #32307, .T. ) ;
#32967 = CARTESIAN_POINT ( 'NONE',  ( 13.16549422024820082, 1421.079389199930120, 230.1572586433449885 ) ) ;
#32968 = CARTESIAN_POINT ( 'NONE',  ( 33.28034951413924603, 1522.382868172863937, 200.8029765415137433 ) ) ;
#32969 = ORIENTED_EDGE ( 'NONE', *, *, #85138, .F. ) ;
#32970 = ORIENTED_EDGE ( 'NONE', *, *, #10750, .T. ) ;
#32971 = CARTESIAN_POINT ( 'NONE',  ( -31.92192241209999892, 1384.697425913300094, 206.3077903497789691 ) ) ;
#32972 = CARTESIAN_POINT ( 'NONE',  ( -24.07249582042329905, 1410.733237779120145, 208.8823328027320088 ) ) ;
#32973 = ORIENTED_EDGE ( 'NONE', *, *, #49528, .T. ) ;
#32974 = CARTESIAN_POINT ( 'NONE',  ( -107.3060007717200079, 1358.631207110790001, 307.5510129087689961 ) ) ;
#32975 = CARTESIAN_POINT ( 'NONE',  ( -9.534219445089998857, 1428.030197386430018, 144.1938086916980239 ) ) ;
#32976 = CARTESIAN_POINT ( 'NONE',  ( -5.800026419229999064, 1498.346957321030231, 235.6600973397979999 ) ) ;
#32977 = CARTESIAN_POINT ( 'NONE',  ( 4.487359766195160304, 1509.034536885679927, 212.2379737843340024 ) ) ;
#32978 = ORIENTED_EDGE ( 'NONE', *, *, #10873, .T. ) ;
#32979 = CARTESIAN_POINT ( 'NONE',  ( 45.40562959789710362, 1446.095626619519862, 268.7700954888649676 ) ) ;
#32980 = CARTESIAN_POINT ( 'NONE',  ( -11.07039285444999877, 1391.913060387000087, 206.1852823654230065 ) ) ;
#32981 = EDGE_CURVE ( 'NONE', #109119, #59235, #77266, .T. ) ;
#32982 = CARTESIAN_POINT ( 'NONE',  ( 18.02257621027576917, 1526.382868172863937, 182.8951942368371988 ) ) ;
#32983 = CARTESIAN_POINT ( 'NONE',  ( -4.621897862544999569, 1516.858533673840157, 204.5099662467769974 ) ) ;
#32984 = ORIENTED_EDGE ( 'NONE', *, *, #57111, .F. ) ;
#32985 = CARTESIAN_POINT ( 'NONE',  ( 19.00284581381210103, 1457.321592500673205, 226.5478147772149953 ) ) ;
#32986 = CARTESIAN_POINT ( 'NONE',  ( 15.30997864848029977, 1512.715996828740117, 195.5972901532690003 ) ) ;
#32987 = DIRECTION ( 'NONE',  ( -1.755985294532469921E-16, 1.000000000000000000, -1.338183447452831989E-16 ) ) ;
#32988 = VERTEX_POINT ( 'NONE', #62126 ) ;
#32989 = DIRECTION ( 'NONE',  ( 0.9989456101410736366, 0.04590932679840484254, 4.114359441837505869E-05 ) ) ;
#32990 = CARTESIAN_POINT ( 'NONE',  ( 26.67349319650000083, 1451.732280616630078, 135.8047305359980044 ) ) ;
#32991 = CARTESIAN_POINT ( 'NONE',  ( -4.650616333688489590, 1508.551704408389924, 212.8644526986900019 ) ) ;
#32992 = CARTESIAN_POINT ( 'NONE',  ( 3.484502295585529819, 1452.791378885890026, 152.3153881425679970 ) ) ;
#32993 = CARTESIAN_POINT ( 'NONE',  ( 7.524255332260000095, 1421.856213011689988, 195.6731416337989913 ) ) ;
#32995 = B_SPLINE_SURFACE_WITH_KNOTS ( 'NONE', 4, 5, ( 
 ( #7968, #100908, #59499, #49986, #34276, #7422, #42135, #76841, #33167 ),
 ( #93072, #76285, #110435, #16889, #67906, #60055, #66265, #25298, #17444 ),
 ( #51641, #85779, #77395, #697, #37032, #70682, #71227, #96399, #18012 ),
 ( #62843, #70132, #69013, #80141, #61179, #28638, #86332, #46010, #34826 ),
 ( #11301, #88556, #88017, #69570, #52751, #61717, #9618, #96956, #35382 ),
 ( #18557, #86884, #52205, #104244, #78495, #105349, #104795, #79065, #28082 ),
 ( #19674, #10178, #103118, #26419, #53880, #36485, #43787, #27534, #45469 ),
 ( #1244, #53310, #20222, #62270, #103689, #77937, #79611, #94733, #26990 ),
 ( #44353, #54423, #95296, #1809, #2915, #11839, #35946, #60611, #87451 ) ),
 .UNSPECIFIED., .F., .F., .F.,
 ( 5, 4, 5 ),
 ( 6, 3, 6 ),
 ( 74.12006598165800142, 74.13176850000000684, 75.30202033419999452 ),
 ( 0.000000000000000000, 1.000000000000000000, 2.000000000000000000 ),
 .UNSPECIFIED. ) ;
#32994 = CARTESIAN_POINT ( 'NONE',  ( 0.7135751966820839121, 1431.574231143599945, 218.5858100304659786 ) ) ;
#32996 = CARTESIAN_POINT ( 'NONE',  ( 10.37029593331170041, 1479.421151158329849, 205.9993793812860190 ) ) ;
#32997 = AXIS2_PLACEMENT_3D ( 'NONE', #100071, #101153, #59738 ) ;
#32998 = CARTESIAN_POINT ( 'NONE',  ( 2.139403947300960063, 1408.987770019419941, 186.9664919645120165 ) ) ;
#33000 = CARTESIAN_POINT ( 'NONE',  ( -3.263114576272079827E-31, 1414.677402202029953, 209.1218459616989946 ) ) ;
#32999 = CARTESIAN_POINT ( 'NONE',  ( 30.95265250778348687, 1524.659148609483054, 196.4584948516175302 ) ) ;
#33001 = CARTESIAN_POINT ( 'NONE',  ( 11.64198556425840003, 1426.536525572139908, 206.5273548246410087 ) ) ;
#33002 = EDGE_CURVE ( 'NONE', #99650, #27637, #29065, .T. ) ;
#33003 = CARTESIAN_POINT ( 'NONE',  ( -12.04121675010000025, 1380.488207265379970, 215.2564011276290046 ) ) ;
#33004 = AXIS2_PLACEMENT_3D ( 'NONE', #36469, #62255, #71775 ) ;
#33005 = CARTESIAN_POINT ( 'NONE',  ( 3.125365561257785973, 1370.051980510865860, 207.8674606832949507 ) ) ;
#33006 = VERTEX_POINT ( 'NONE', #63239 ) ;
#33007 = CARTESIAN_POINT ( 'NONE',  ( 12.95840410776399843, 1416.218047878440075, 221.5780283176839873 ) ) ;
#33008 = VECTOR ( 'NONE', #13067, 1000.000000000000000 ) ;
#33009 = CYLINDRICAL_SURFACE ( 'NONE', #99902, 2.000000000000003553 ) ;
#33010 = B_SPLINE_SURFACE_WITH_KNOTS ( 'NONE', 5, 5, ( 
 ( #64460, #98576, #90727, #64998, #81768, #40878, #109206, #32491, #66663 ),
 ( #100766, #22955, #24056, #89628, #12916, #90168, #47096, #13450, #39220 ),
 ( #73396, #107532, #99116, #110286, #94580, #9483, #68873, #16743, #85075 ),
 ( #8367, #34683, #42535, #34133, #59913, #35238, #84534, #86191, #68321 ),
 ( #33022, #67208, #59364, #33562, #50409, #94033, #43647, #8924, #25712 ),
 ( #17857, #58794, #52056, #102974, #24600, #15644, #67756, #7822, #26273 ) ),
 .UNSPECIFIED., .F., .F., .F.,
 ( 6, 6 ),
 ( 6, 3, 6 ),
 ( 0.4666582265010000286, 2.797885342409359932 ),
 ( -1.082959936422979947E-05, 1.000000000000000000, 2.000000000000000000 ),
 .UNSPECIFIED. ) ;
#33011 = CARTESIAN_POINT ( 'NONE',  ( -11.88252267529999884, 1391.725460676640068, 205.4510509948789831 ) ) ;
#33012 =( BOUNDED_SURFACE ( )  B_SPLINE_SURFACE ( 4, 2, ( 
 ( #109003, #65911, #100029 ),
 ( #47447, #107884, #32287 ),
 ( #39016, #90531, #6534 ),
 ( #23321, #98930, #55863 ),
 ( #14914, #46914, #22750 ) ),
 .UNSPECIFIED., .F., .F., .F. ) 
 B_SPLINE_SURFACE_WITH_KNOTS ( ( 5, 5 ),
 ( 3, 3 ),
 ( 3.613988937040000238, 5.260361675040000407 ),
 ( 5.300753508049940166, 6.150216337544540224 ),
 .UNSPECIFIED. ) 
 GEOMETRIC_REPRESENTATION_ITEM ( )  RATIONAL_B_SPLINE_SURFACE ( (
 ( 0.8627701935039370218, 0.8230341786337309617, 0.9546103739810829492),
 ( 0.8627701935039370218, 0.8230341786337309617, 0.9546103739810829492),
 ( 0.8627701935039370218, 0.8230341786337309617, 0.9546103739810829492),
 ( 0.8627701935039370218, 0.8230341786337309617, 0.9546103739810829492),
 ( 0.8627701935039370218, 0.8230341786337309617, 0.9546103739810829492) ) ) 
 REPRESENTATION_ITEM ( '' )  SURFACE ( )  );
#33013 = CARTESIAN_POINT ( 'NONE',  ( 9.490676817001279630, 1424.811928784230076, 209.0801198070559792 ) ) ;
#33014 = CARTESIAN_POINT ( 'NONE',  ( 12.24717007643060107, 1426.243361053459921, 202.7748164033999956 ) ) ;
#33015 = CARTESIAN_POINT ( 'NONE',  ( -10.83720256795320047, 1462.826867853169915, 206.9403819536609888 ) ) ;
#33016 = CARTESIAN_POINT ( 'NONE',  ( -26.86204968941349946, 1508.007394745769943, 212.0120970035400205 ) ) ;
#33017 = EDGE_CURVE ( 'NONE', #9541, #56950, #8374, .T. ) ;
#33018 = CARTESIAN_POINT ( 'NONE',  ( -21.18003089992732768, 1508.593876776232719, 192.0369185836293013 ) ) ;
#33019 = CARTESIAN_POINT ( 'NONE',  ( 11.44209389759999951, 1433.338294488139809, 151.3396440961979863 ) ) ;
#33020 = CARTESIAN_POINT ( 'NONE',  ( 36.99165393049999295, 1454.692295987030093, 268.3665355201979992 ) ) ;
#33021 = B_SPLINE_SURFACE_WITH_KNOTS ( 'NONE', 5, 5, ( 
 ( #100880, #24174, #94144, #34248, #58362, #92487 ),
 ( #15757, #33683, #42655, #49958, #42108, #7395 ),
 ( #76809, #76255, #41560, #75715, #16317, #68431 ),
 ( #50518, #84642, #102533, #67877, #25825, #43217 ),
 ( #77367, #668, #66234, #100353, #34799, #79036 ),
 ( #1218, #88522, #2337, #35916, #10715, #54389 ),
 ( #79578, #96924, #18525, #69540, #94704, #44886 ),
 ( #87419, #11807, #19644, #35353, #53847, #68987 ),
 ( #20191, #60583, #52722, #80110, #87984, #96365 ) ),
 .UNSPECIFIED., .F., .F., .F.,
 ( 6, 3, 6 ),
 ( 6, 6 ),
 ( 8.898683856529999048, 17.98737357839999973, 25.59366590640000183 ),
 ( 0.000000000000000000, 2.000000000000000000 ),
 .UNSPECIFIED. ) ;
#33022 = CARTESIAN_POINT ( 'NONE',  ( 11.54244540325870005, 1414.913060387399810, 197.8963259754790158 ) ) ;
#33023 = LINE ( 'NONE', #67212, #20713 ) ;
#33024 = CARTESIAN_POINT ( 'NONE',  ( 8.573315781209160491, 1422.682987794119981, 197.1461458239759850 ) ) ;
#33025 = CARTESIAN_POINT ( 'NONE',  ( 9.619266338924012061, 1463.334782415319978, 214.5539088362909865 ) ) ;
#33026 = CARTESIAN_POINT ( 'NONE',  ( -11.41675697748640061, 1482.775670443970057, 205.7339590229720159 ) ) ;
#33027 = CARTESIAN_POINT ( 'NONE',  ( 12.49661969954494900, 1398.283518850857035, 212.9844610132695664 ) ) ;
#33028 = LINE ( 'NONE', #23527, #71410 ) ;
#33029 = CARTESIAN_POINT ( 'NONE',  ( 23.99427320690000087, 1410.919622257430092, 209.9798509652409848 ) ) ;
#33030 = CARTESIAN_POINT ( 'NONE',  ( 0.7266811281859989480, 1473.184386469690025, 216.5181916793989956 ) ) ;
#33031 = CARTESIAN_POINT ( 'NONE',  ( -15.17646696946499851, 1515.958428328729951, 225.0580773729669772 ) ) ;
#33032 = CARTESIAN_POINT ( 'NONE',  ( -14.31392993066779873, 1383.859213631680177, 219.1254165421789821 ) ) ;
#33033 = CARTESIAN_POINT ( 'NONE',  ( -2.580915939757335131, 1524.130440953581001, 175.8924427158433161 ) ) ;
#33035 = EDGE_CURVE ( 'NONE', #27986, #61245, #91149, .T. ) ;
#33034 = CIRCLE ( 'NONE', #52735, 0.9999999999999898970 ) ;
#33036 = CARTESIAN_POINT ( 'NONE',  ( -17.51543816364580053, 1417.552355716799866, 206.7803260042529701 ) ) ;
#33037 = CARTESIAN_POINT ( 'NONE',  ( -3.456072659400000191, 1414.971339025629959, 226.0233698056979961 ) ) ;
#33039 =( BOUNDED_SURFACE ( )  B_SPLINE_SURFACE ( 3, 2, ( 
 ( #110702, #57571, #14970 ),
 ( #96675, #51914, #61992 ),
 ( #43516, #9896, #86057 ),
 ( #103957, #10451, #45182 ),
 ( #53026, #79323, #26690 ),
 ( #60886, #2634, #87733 ),
 ( #78204, #44065, #36760 ),
 ( #9354, #78765, #69838 ),
 ( #70954, #8780, #69278 ),
 ( #95013, #105069, #27810 ) ),
 .UNSPECIFIED., .F., .F., .F. ) 
 B_SPLINE_SURFACE_WITH_KNOTS ( ( 4, 2, 2, 2, 4 ),
 ( 3, 3 ),
 ( 1.570796326794896558, 1.963495408493620697, 2.356194490192344837, 2.748893571891068976, 3.141592653589793116 ),
 ( 0.000000000000000000, 1.000000000000000000 ),
 .UNSPECIFIED. ) 
 GEOMETRIC_REPRESENTATION_ITEM ( )  RATIONAL_B_SPLINE_SURFACE ( (
 ( 1.000000000000000000, 0.7071067811865867636, 1.000000000000000000),
 ( 1.000000000000000000, 0.7166207884820130491, 1.000000000000000000),
 ( 1.000000000000000000, 0.7259222650909733510, 1.000000000000000000),
 ( 1.000000000000000000, 0.7428408967927655482, 1.000000000000000000),
 ( 1.000000000000000000, 0.7504512394527111940, 1.000000000000000000),
 ( 1.000000000000000000, 0.7630177051947926170, 1.000000000000000000),
 ( 1.000000000000000000, 0.7679730451972418548, 1.000000000000000000),
 ( 1.000000000000000000, 0.7746454561798022942, 1.000000000000000000),
 ( 1.000000000000000000, 0.7763684247034656760, 1.000000000000000000),
 ( 1.000000000000000000, 0.7763623250684373867, 1.000000000000000000) ) ) 
 REPRESENTATION_ITEM ( '' )  SURFACE ( )  );
#33038 = CARTESIAN_POINT ( 'NONE',  ( -9.278582903680890226, 1424.431248859760217, 204.6907556553629774 ) ) ;
#33040 = CARTESIAN_POINT ( 'NONE',  ( 0.1734663674328389971, 1478.296956495260247, 182.1675436825559871 ) ) ;
#33041 = EDGE_LOOP ( 'NONE', ( #85676, #104262, #6381, #70617, #82865, #106385, #97446, #99295 ) ) ;
#33042 = CARTESIAN_POINT ( 'NONE',  ( -20.24673233129999872, 1443.913060387330006, 162.1129423953979938 ) ) ;
#33043 = EDGE_CURVE ( 'NONE', #28487, #92672, #41923, .T. ) ;
#33044 = CARTESIAN_POINT ( 'NONE',  ( -7.965680540240001051, 1384.926148861439970, 199.4891222871690104 ) ) ;
#33045 = DIRECTION ( 'NONE',  ( -1.755985294532469921E-16, 1.000000000000000000, -1.338183447452831989E-16 ) ) ;
#33046 = CARTESIAN_POINT ( 'NONE',  ( -40.90250537898710093, 1447.119793117110021, 134.0999999985199906 ) ) ;
#33047 = CARTESIAN_POINT ( 'NONE',  ( -109.1655176280000035, 1384.872415562570040, 297.1329087283589843 ) ) ;
#33048 = ORIENTED_EDGE ( 'NONE', *, *, #11395, .F. ) ;
#33049 = CARTESIAN_POINT ( 'NONE',  ( -1.024097229660000163, 1484.039857070089965, 198.4653328332990156 ) ) ;
#33050 = AXIS2_PLACEMENT_3D ( 'NONE', #38625, #48709, #66068 ) ;
#33051 = CARTESIAN_POINT ( 'NONE',  ( 10.03326978499999989, 1480.064307681189803, 205.9776673489490122 ) ) ;
#33052 = CARTESIAN_POINT ( 'NONE',  ( -103.6828773697239399, 1379.966495660962892, 305.2745416132092942 ) ) ;
#33053 = PLANE ( 'NONE',  #66023 ) ;
#33055 = ADVANCED_FACE ( 'NONE', ( #92252 ), #57701, .T. ) ;
#33054 = CARTESIAN_POINT ( 'NONE',  ( -8.569414462087090456, 1437.093887118070143, 211.2561754816580049 ) ) ;
#33056 = CARTESIAN_POINT ( 'NONE',  ( 19.68364361504686855, 1519.551704408389924, 197.0079017805142030 ) ) ;
#33057 = CARTESIAN_POINT ( 'NONE',  ( 17.15254153798874981, 1516.551704399887512, 196.9190519997810611 ) ) ;
#33058 = LINE ( 'NONE', #60498, #84338 ) ;
#33059 = CARTESIAN_POINT ( 'NONE',  ( 18.05542497264820057, 1416.825784014559986, 208.7596466293869923 ) ) ;
#33060 = CARTESIAN_POINT ( 'NONE',  ( -78.64707799225199381, 1385.152071352919847, 281.2464940805660376 ) ) ;
#33061 = CARTESIAN_POINT ( 'NONE',  ( -19.07966196791873159, 1524.244163922424377, 239.0023935151694161 ) ) ;
#33062 = CARTESIAN_POINT ( 'NONE',  ( 11.90624125940899880, 1421.888678172720120, 209.0552753088340125 ) ) ;
#33063 = ORIENTED_EDGE ( 'NONE', *, *, #82941, .T. ) ;
#33064 = CARTESIAN_POINT ( 'NONE',  ( -33.29550093079999584, 1450.462297931059993, 136.2636478384980023 ) ) ;
#33065 = EDGE_CURVE ( 'NONE', #67895, #94689, #47508, .T. ) ;
#33066 = CARTESIAN_POINT ( 'NONE',  ( 3.827327205999999649, 1418.913060387330006, 172.2701767054979882 ) ) ;
#33068 = ORIENTED_EDGE ( 'NONE', *, *, #66255, .F. ) ;
#33067 = LINE ( 'NONE', #8410, #48392 ) ;
#33069 = CARTESIAN_POINT ( 'NONE',  ( 5.586191088959999718, 1473.645535070089863, 218.5932301067289814 ) ) ;
#33070 = CARTESIAN_POINT ( 'NONE',  ( -15.10371725490000117, 1409.440493816029857, 225.2902966875980155 ) ) ;
#33071 = CARTESIAN_POINT ( 'NONE',  ( -109.6459781550000088, 1384.546124173760063, 311.3068487942589968 ) ) ;
#33072 = CARTESIAN_POINT ( 'NONE',  ( -10.49051443589999977, 1493.796478401889999, 205.2036621587689922 ) ) ;
#33073 = CARTESIAN_POINT ( 'NONE',  ( 41.32342021774600482, 1446.574054804671050, 269.6346703930319677 ) ) ;
#33074 = CARTESIAN_POINT ( 'NONE',  ( -11.60004869885203505, 1427.693913909466573, 134.2641720911346681 ) ) ;
#33075 = CARTESIAN_POINT ( 'NONE',  ( 16.17016470285728857, 1432.043082342410344, 218.4496149275423988 ) ) ;
#33076 = CARTESIAN_POINT ( 'NONE',  ( 2.407361919430000441, 1417.795499740929927, 234.0370795184979897 ) ) ;
#33077 = CARTESIAN_POINT ( 'NONE',  ( 2.500000000000000000, 1434.142768437249970, 183.0182394769479970 ) ) ;
#33078 = CARTESIAN_POINT ( 'NONE',  ( -103.9363405868959518, 1366.350733876290633, 309.3918667846981521 ) ) ;
#33079 = FACE_OUTER_BOUND ( 'NONE', #36751, .T. ) ;
#33080 = VECTOR ( 'NONE', #107480, 1000.000000000000000 ) ;
#33081 = ADVANCED_FACE ( 'NONE', ( #5493 ), #106006, .F. ) ;
#33082 = CARTESIAN_POINT ( 'NONE',  ( 0.1599736409740009913, 1457.268902431789911, 199.5796105822190043 ) ) ;
#33083 = CARTESIAN_POINT ( 'NONE',  ( -1.136004312195000088, 1516.815173273089840, 206.2562091229970065 ) ) ;
#33084 = CARTESIAN_POINT ( 'NONE',  ( 2.715357296970000167, 1447.820972075539885, 154.4673902800980159 ) ) ;
#33085 = ORIENTED_EDGE ( 'NONE', *, *, #70946, .F. ) ;
#33087 = EDGE_CURVE ( 'NONE', #55445, #56930, #105969, .T. ) ;
#33086 = AXIS2_PLACEMENT_3D ( 'NONE', #46572, #88566, #46023 ) ;
#33088 = CARTESIAN_POINT ( 'NONE',  ( 13.89869200000000049, 1452.835253893030085, 223.8385666725980059 ) ) ;
#33089 = CARTESIAN_POINT ( 'NONE',  ( -2.109056957580000002, 1421.166295015029846, 183.8085771866980167 ) ) ;
#33091 = ORIENTED_EDGE ( 'NONE', *, *, #90698, .T. ) ;
#33090 = CARTESIAN_POINT ( 'NONE',  ( -68.65906241868358961, 1379.747658069470162, 280.2648999511130228 ) ) ;
#33092 = CARTESIAN_POINT ( 'NONE',  ( -9.445418716914016244, 1380.274608993225684, 217.1226397039540075 ) ) ;
#33093 = ORIENTED_EDGE ( 'NONE', *, *, #97304, .T. ) ;
#33094 = CARTESIAN_POINT ( 'NONE',  ( -32.78250617288048829, 1511.187213306747708, 199.9357095655695389 ) ) ;
#33095 = CARTESIAN_POINT ( 'NONE',  ( -23.75028666920000120, 1410.916158857830169, 207.2858998927080165 ) ) ;
#33097 = CARTESIAN_POINT ( 'NONE',  ( 15.78476754123740022, 1409.716999194859909, 192.1026167944760061 ) ) ;
#33096 = CARTESIAN_POINT ( 'NONE',  ( -11.73996803256352095, 1426.694174138938934, 144.3809647795363560 ) ) ;
#33098 = CARTESIAN_POINT ( 'NONE',  ( 1.136547584984999970, 1516.839862955080207, 211.5998212856970042 ) ) ;
#33099 = CARTESIAN_POINT ( 'NONE',  ( 38.76435533041719594, 1438.005125630080101, 136.3470787082570155 ) ) ;
#33100 = B_SPLINE_SURFACE_WITH_KNOTS ( 'NONE', 5, 5, ( 
 ( #9772, #78081, #1384, #35526, #61324, #95442, #30981, #65706, #81370 ),
 ( #74110, #107697, #29876, #30431, #108240, #39940, #90887, #21455, #55665 ),
 ( #81930, #66277, #40485, #91450, #48357, #56750, #14726, #107138, #47244 ),
 ( #89788, #13058, #99827, #5233, #20914, #74660, #48916, #82497, #14172 ),
 ( #64617, #4685, #38824, #73003, #23119, #55118, #5799, #98737, #13606 ),
 ( #21998, #56191, #90327, #65156, #99270, #47794, #39387, #73564, #22548 ) ),
 .UNSPECIFIED., .F., .F., .F.,
 ( 6, 6 ),
 ( 6, 3, 6 ),
 ( 10.26165209716149995, 12.52004467320000103 ),
 ( 0.000000000000000000, 1.000000000000000000, 2.000000000000000000 ),
 .UNSPECIFIED. ) ;
#33101 = CARTESIAN_POINT ( 'NONE',  ( -11.63658410760000095, 1425.864915301529891, 144.1607460166979990 ) ) ;
#33102 = CARTESIAN_POINT ( 'NONE',  ( 9.659057376369998948, 1477.882669201989984, 202.4105350377390096 ) ) ;
#33103 = CARTESIAN_POINT ( 'NONE',  ( 16.79818491188742513, 1460.579683146600928, 228.8802028025106665 ) ) ;
#33104 = CONTEXT_DEPENDENT_SHAPE_REPRESENTATION ( #89248, #91179 ) ;
#33105 = CARTESIAN_POINT ( 'NONE',  ( 37.84675541841409796, 1450.538956397299899, 134.0999999985309898 ) ) ;
#33106 = CARTESIAN_POINT ( 'NONE',  ( -38.53567264009640070, 1439.151675925619884, 136.6512514728599967 ) ) ;
#33107 = ORIENTED_EDGE ( 'NONE', *, *, #38384, .T. ) ;
#33108 = CARTESIAN_POINT ( 'NONE',  ( -18.47518245119999847, 1466.235720591789914, 200.8822878489689856 ) ) ;
#33109 = B_SPLINE_CURVE_WITH_KNOTS ( 'NONE', 5,
 ( #101211, #50840, #89660, #76042, #12946, #83330, #25057, #40227, #49202, #82781, #74410, #84971 ),
 .UNSPECIFIED., .F., .F.,
 ( 6, 3, 3, 6 ),
 ( 0.000000000000000000, 3.329846645400000416, 4.930332151970000076, 12.58720418400000085 ),
 .UNSPECIFIED. ) ;
#33110 = CARTESIAN_POINT ( 'NONE',  ( -18.57062135440000006, 1457.638594930429917, 227.6943395327979829 ) ) ;
#33111 = ORIENTED_EDGE ( 'NONE', *, *, #97559, .T. ) ;
#33112 = EDGE_LOOP ( 'NONE', ( #82988, #50281, #919, #36990 ) ) ;
#33113 = CARTESIAN_POINT ( 'NONE',  ( -0.9532864999229999636, 1432.163584394390000, 203.4075515145090094 ) ) ;
#33114 = CARTESIAN_POINT ( 'NONE',  ( 10.55262952197939974, 1452.742582998889930, 209.9734261203599885 ) ) ;
#33115 = CARTESIAN_POINT ( 'NONE',  ( -4.535342621894029591, 1507.667936859109886, 221.1848183489019846 ) ) ;
#33116 = CARTESIAN_POINT ( 'NONE',  ( 2.157536728407475568, 1397.913060387289988, 207.9431782750405659 ) ) ;
#33117 = DIRECTION ( 'NONE',  ( 0.000000000000000000, 1.000000000000000000, 0.000000000000000000 ) ) ;
#33118 = DIRECTION ( 'NONE',  ( 0.3390050494208853293, -0.7071067811868682051, 0.6205445805634673961 ) ) ;
#33119 = CARTESIAN_POINT ( 'NONE',  ( 40.71747596219820053, 1438.773003613790024, 135.0591077376159888 ) ) ;
#33120 = CARTESIAN_POINT ( 'NONE',  ( 5.018135791179288319, 1516.818301249119031, 214.7147315454415946 ) ) ;
#33121 = AXIS2_PLACEMENT_3D ( 'NONE', #36771, #55802, #97218 ) ;
#33122 = CARTESIAN_POINT ( 'NONE',  ( 26.28888947440000123, 1436.471222792599974, 136.7656709048980019 ) ) ;
#33123 = CARTESIAN_POINT ( 'NONE',  ( 38.12323339995595006, 1442.831169986191526, 136.9072173714204723 ) ) ;
#33124 = CARTESIAN_POINT ( 'NONE',  ( -76.44953714789230048, 1384.775617543210046, 277.8908186701659702 ) ) ;
#33125 = ORIENTED_EDGE ( 'NONE', *, *, #28818, .F. ) ;
#33126 = CARTESIAN_POINT ( 'NONE',  ( -7.718134667564999774, 1516.881930554049859, 201.7919159189069944 ) ) ;
#33127 = CARTESIAN_POINT ( 'NONE',  ( -6.562094107424999656, 1517.122674412569950, 208.3832410274270046 ) ) ;
#33128 = ORIENTED_EDGE ( 'NONE', *, *, #37848, .F. ) ;
#33129 = CARTESIAN_POINT ( 'NONE',  ( 8.515581525185789147, 1519.551704408389924, 191.3277396192498543 ) ) ;
#33130 = CARTESIAN_POINT ( 'NONE',  ( 3.112680624948092500, 1511.889619707009842, 217.0463476667217151 ) ) ;
#33131 = ORIENTED_EDGE ( 'NONE', *, *, #6246, .F. ) ;
#33132 = CARTESIAN_POINT ( 'NONE',  ( -13.91384509699999938, 1415.996778984329922, 221.6684481777979840 ) ) ;
#33133 = CARTESIAN_POINT ( 'NONE',  ( 5.805275416047459558, 1429.751446996589948, 216.6272687077410239 ) ) ;
#33134 = DIRECTION ( 'NONE',  ( -1.755985294532469921E-16, 1.000000000000000000, -1.338183447452830017E-16 ) ) ;
#33135 = CARTESIAN_POINT ( 'NONE',  ( -7.166932940584959333, 1489.833104379089491, 217.3880470055029264 ) ) ;
#33136 = CARTESIAN_POINT ( 'NONE',  ( -13.06606033770000153, 1422.974160590630163, 222.1234525822980004 ) ) ;
#33137 = CARTESIAN_POINT ( 'NONE',  ( 9.924145419382540467, 1468.837275789919886, 207.5733661434399835 ) ) ;
#33138 = CARTESIAN_POINT ( 'NONE',  ( -10.29442985670006117, 1469.837443877088390, 213.9189782992590665 ) ) ;
#33139 = CARTESIAN_POINT ( 'NONE',  ( 8.178501070643639181, 1441.152429762079919, 153.9860758848200248 ) ) ;
#33140 = CARTESIAN_POINT ( 'NONE',  ( -63.89205165820000332, 1379.749420737849960, 270.3321189449590065 ) ) ;
#33141 = CARTESIAN_POINT ( 'NONE',  ( -15.08386190559999918, 1451.324666099630122, 222.9201800246979985 ) ) ;
#33143 = CARTESIAN_POINT ( 'NONE',  ( 5.576745036960350177, 1467.101830086349992, 199.5044134152479955 ) ) ;
#33142 = CARTESIAN_POINT ( 'NONE',  ( -20.77679319119999946, 1505.353396285190229, 209.2699052164729778 ) ) ;
#33144 = FACE_OUTER_BOUND ( 'NONE', #62225, .T. ) ;
#33145 = EDGE_CURVE ( 'NONE', #2857, #7591, #23924, .T. ) ;
#33146 = B_SPLINE_SURFACE_WITH_KNOTS ( 'NONE', 5, 1, ( 
 ( #95921, #97576 ),
 ( #98109, #61800 ),
 ( #71873, #46094 ),
 ( #80778, #3544 ),
 ( #106523, #1889 ),
 ( #63998, #29265 ) ),
 .UNSPECIFIED., .F., .F., .F.,
 ( 6, 6 ),
 ( 2, 2 ),
 ( 0.000000000000000000, 3.864159766120000228 ),
 ( 0.000000000000000000, 14.00000000000000000 ),
 .UNSPECIFIED. ) ;
#33147 = CARTESIAN_POINT ( 'NONE',  ( -4.034908597844999889, 1517.068717944079935, 216.4577469658269990 ) ) ;
#33148 = ORIENTED_EDGE ( 'NONE', *, *, #26077, .F. ) ;
#33149 = LINE ( 'NONE', #58923, #53346 ) ;
#33150 = CARTESIAN_POINT ( 'NONE',  ( 1.739050608666847131, 1516.540855186845874, 216.8310492268561802 ) ) ;
#33151 = CARTESIAN_POINT ( 'NONE',  ( -4.611879723454999969, 1516.858533673840157, 213.7437437946470027 ) ) ;
#33152 = CARTESIAN_POINT ( 'NONE',  ( -2.908982738435793802, 1484.703267874767107, 183.2481867733562240 ) ) ;
#33153 = CARTESIAN_POINT ( 'NONE',  ( -30.90487439922565116, 1525.907212628473644, 201.8101144455181952 ) ) ;
#33155 = EDGE_LOOP ( 'NONE', ( #13918, #22949, #8973, #74930 ) ) ;
#33154 = CARTESIAN_POINT ( 'NONE',  ( -11.51256439133040033, 1501.104924895310205, 211.2032020787609952 ) ) ;
#33156 = CARTESIAN_POINT ( 'NONE',  ( -8.848600347999999727, 1384.909289574200102, 199.9247552632990050 ) ) ;
#33157 = CARTESIAN_POINT ( 'NONE',  ( -1.563447624619999976, 1508.551704408389924, 220.3217919041989887 ) ) ;
#33158 = EDGE_CURVE ( 'NONE', #102491, #67527, #64878, .T. ) ;
#33159 = CARTESIAN_POINT ( 'NONE',  ( -11.52457544480000173, 1428.535701648929944, 150.0557210695980075 ) ) ;
#33160 = CARTESIAN_POINT ( 'NONE',  ( 19.04937065429340137, 1456.924701486199865, 225.3692720049160130 ) ) ;
#33161 = CARTESIAN_POINT ( 'NONE',  ( -4.078211669849999943, 1440.299026235899873, 185.4566092242980062 ) ) ;
#33162 = DIRECTION ( 'NONE',  ( -1.836970198721029688E-16, -1.000000000000000000, 0.000000000000000000 ) ) ;
#33163 = CARTESIAN_POINT ( 'NONE',  ( -6.198495147294970309, 1426.943711827879952, 202.1453469996679928 ) ) ;
#33164 = CARTESIAN_POINT ( 'NONE',  ( 0.2637998666456179975, 1430.332984592310140, 190.1847976646700147 ) ) ;
#33166 = CARTESIAN_POINT ( 'NONE',  ( -8.141993531839686327, 1423.434677666080006, 137.0999999981440851 ) ) ;
#33165 = CARTESIAN_POINT ( 'NONE',  ( -22.75471552770000017, 1495.366693290230160, 223.7173521039980244 ) ) ;
#33167 = CARTESIAN_POINT ( 'NONE',  ( -16.17998770715999868, 1459.144433622870110, 230.7168371058380103 ) ) ;
#33168 = ORIENTED_EDGE ( 'NONE', *, *, #96685, .T. ) ;
#33169 = CARTESIAN_POINT ( 'NONE',  ( -1.715361130375000043, 1516.743010792419909, 205.6766444437269854 ) ) ;
#33170 = CARTESIAN_POINT ( 'NONE',  ( 4.991008440799999946, 1405.971275674329945, 268.4734096741979670 ) ) ;
#33171 = CARTESIAN_POINT ( 'NONE',  ( -0.1426365273169999948, 1409.853703886329868, 185.0414845334979930 ) ) ;
#33172 = CARTESIAN_POINT ( 'NONE',  ( 18.52231723690000464, 1430.306689337430043, 192.7617654628980119 ) ) ;
#33173 = FACE_OUTER_BOUND ( 'NONE', #79392, .T. ) ;
#33174 = CIRCLE ( 'NONE', #31331, 0.9999999999999873435 ) ;
#33175 = CARTESIAN_POINT ( 'NONE',  ( -9.873265212564325211, 1390.063525629135029, 216.5660449977083317 ) ) ;
#33176 = CARTESIAN_POINT ( 'NONE',  ( 11.90000415720300175, 1434.913060496859998, 147.6452464505769910 ) ) ;
#33177 = DIRECTION ( 'NONE',  ( -5.980589973904019347E-17, 1.000000000000000000, -1.736889445713099699E-16 ) ) ;
#33178 = CARTESIAN_POINT ( 'NONE',  ( -14.56536539080000026, 1417.270466440329983, 203.6292502051090025 ) ) ;
#33179 = CARTESIAN_POINT ( 'NONE',  ( -12.88374579789999963, 1445.168051104930100, 187.0888182765980048 ) ) ;
#33180 = EDGE_CURVE ( 'NONE', #3770, #41248, #72020, .T. ) ;
#33181 = B_SPLINE_SURFACE_WITH_KNOTS ( 'NONE', 5, 1, ( 
 ( #83198, #74268 ),
 ( #92145, #56901 ),
 ( #101622, #73717 ),
 ( #32782, #99981 ),
 ( #108955, #14321 ),
 ( #58010, #58560 ) ),
 .UNSPECIFIED., .F., .F., .F.,
 ( 6, 6 ),
 ( 2, 2 ),
 ( 0.000000000000000000, 15.56462730289999996 ),
 ( 0.000000000000000000, 14.00000000000000000 ),
 .UNSPECIFIED. ) ;
#33182 = CARTESIAN_POINT ( 'NONE',  ( -17.33706400627729138, 1419.403770296549055, 207.7192493357346450 ) ) ;
#33183 = CARTESIAN_POINT ( 'NONE',  ( 13.58968549309999929, 1409.153350369530017, 270.0972160545979932 ) ) ;
#33184 = EDGE_CURVE ( 'NONE', #19773, #77131, #78961, .T. ) ;
#33185 = CARTESIAN_POINT ( 'NONE',  ( 1.461819939759239961, 1494.181313383729730, 181.6773600568459983 ) ) ;
#33186 = CARTESIAN_POINT ( 'NONE',  ( -8.800012970690000103, 1429.116251061429921, 209.1218459616979999 ) ) ;
#33188 = EDGE_CURVE ( 'NONE', #6013, #79565, #64556, .T. ) ;
#33187 = CARTESIAN_POINT ( 'NONE',  ( -11.50563130876499862, 1508.158931577909925, 207.5673837874410026 ) ) ;
#33189 = DIRECTION ( 'NONE',  ( -5.980589973904019347E-17, 1.000000000000000000, -1.736889445713099699E-16 ) ) ;
#33190 = CARTESIAN_POINT ( 'NONE',  ( -6.972260506549999626, 1474.659203917630066, 269.6344785065979863 ) ) ;
#33191 = CARTESIAN_POINT ( 'NONE',  ( -30.41961987998705297, 1524.374578187332872, 196.3903468980581977 ) ) ;
#33192 = CARTESIAN_POINT ( 'NONE',  ( -22.96901158596646653, 1522.051704408389924, 211.6943887467578236 ) ) ;
#33193 = DIRECTION ( 'NONE',  ( 0.7044160264027579110, -0.08715574274767008689, -0.7044160264027579110 ) ) ;
#33194 = CARTESIAN_POINT ( 'NONE',  ( -53.58244648229940310, 1384.723190384210056, 269.0228002601600110 ) ) ;
#33195 = CARTESIAN_POINT ( 'NONE',  ( 1.951029616821370327, 1508.751449870507940, 237.3205679132474870 ) ) ;
#33196 = CARTESIAN_POINT ( 'NONE',  ( 11.57234447799390153, 1415.219159638040082, 222.8946685903029845 ) ) ;
#33197 = EDGE_CURVE ( 'NONE', #86349, #98568, #60321, .T. ) ;
#33198 = CARTESIAN_POINT ( 'NONE',  ( -107.0293272779999967, 1378.913060310580022, 300.7012236569590300 ) ) ;
#33199 = CARTESIAN_POINT ( 'NONE',  ( -1.906499846882070084E-08, 1517.051704408389924, 209.1218459511669892 ) ) ;
#33200 = CARTESIAN_POINT ( 'NONE',  ( -2.302358205752170317, 1507.635233240290063, 221.1829251670985741 ) ) ;
#33201 = CIRCLE ( 'NONE', #27862, 12.26364123839999998 ) ;
#33202 = CARTESIAN_POINT ( 'NONE',  ( -21.49788281959999736, 1409.663783000529975, 203.5162482710680081 ) ) ;
#33203 = CARTESIAN_POINT ( 'NONE',  ( -9.752354139992853277, 1380.553637087837387, 201.4862867480141233 ) ) ;
#33204 = CARTESIAN_POINT ( 'NONE',  ( 12.47858532031530032, 1421.602759672520051, 207.4039838217449869 ) ) ;
#33205 = CARTESIAN_POINT ( 'NONE',  ( 10.38589783937220012, 1479.770266300000003, 206.7566811546030010 ) ) ;
#33206 = FACE_OUTER_BOUND ( 'NONE', #90712, .T. ) ;
#33207 = CARTESIAN_POINT ( 'NONE',  ( 4.677539293532180231, 1434.888973739250105, 228.7640143593589812 ) ) ;
#33208 = CARTESIAN_POINT ( 'NONE',  ( 17.10350668511487626, 1524.477587234284556, 180.9723570393801708 ) ) ;
#33209 = AXIS2_PLACEMENT_3D ( 'NONE', #86997, #103807, #87570 ) ;
#33210 = CARTESIAN_POINT ( 'NONE',  ( -20.36853080836219831, 1464.956632874939942, 210.9458194777220115 ) ) ;
#33212 = CARTESIAN_POINT ( 'NONE',  ( -2.487935118526678480, 1508.884207228051082, 204.6305528479420843 ) ) ;
#33211 = CARTESIAN_POINT ( 'NONE',  ( -16.17592491924940035, 1416.577882651939944, 209.2335455203370032 ) ) ;
#33213 = CARTESIAN_POINT ( 'NONE',  ( 11.72262950227709943, 1426.705135300079974, 143.1384147304339933 ) ) ;
#33214 = CARTESIAN_POINT ( 'NONE',  ( 17.83486663330510424, 1523.678648413191695, 237.8759530894958516 ) ) ;
#33215 = CARTESIAN_POINT ( 'NONE',  ( -122.4487580624700058, 1378.528619065190014, 299.2784868977390147 ) ) ;
#33216 = CARTESIAN_POINT ( 'NONE',  ( -1.920602012799999869, 1420.567466289690174, 193.8392733480989989 ) ) ;
#33217 = CARTESIAN_POINT ( 'NONE',  ( 11.60004869885204748, 1428.977684734793684, 135.1000015630646089 ) ) ;
#33218 = CARTESIAN_POINT ( 'NONE',  ( -1.131796848745000084, 1516.659138130710289, 203.3488676535569937 ) ) ;
#33219 = CYLINDRICAL_SURFACE ( 'NONE', #87583, 2.000000000000003109 ) ;
#33220 = FACE_OUTER_BOUND ( 'NONE', #91897, .T. ) ;
#33221 = CARTESIAN_POINT ( 'NONE',  ( 15.10381381093499975, 1513.853571676670072, 194.2467028014669950 ) ) ;
#33222 = FACE_OUTER_BOUND ( 'NONE', #68418, .T. ) ;
#33223 = CARTESIAN_POINT ( 'NONE',  ( -39.19971590621860003, 1377.724600137430116, 229.1242316895250042 ) ) ;
#33224 = ADVANCED_FACE ( 'NONE', ( #8231 ), #85485, .T. ) ;
#33225 = CARTESIAN_POINT ( 'NONE',  ( 20.33996727594809784, 1508.367434211329964, 228.7312766114060310 ) ) ;
#33227 = VERTEX_POINT ( 'NONE', #34551 ) ;
#33226 = CARTESIAN_POINT ( 'NONE',  ( -25.97809490251969677, 1379.634779511279930, 215.3796568787460046 ) ) ;
#33228 = ORIENTED_EDGE ( 'NONE', *, *, #81444, .F. ) ;
#33229 = CARTESIAN_POINT ( 'NONE',  ( 11.68034705308759946, 1434.603008417340106, 151.2598176529760394 ) ) ;
#33230 = CARTESIAN_POINT ( 'NONE',  ( -13.25226091950000118, 1397.693633465330095, 207.3660310399680213 ) ) ;
#33231 = ORIENTED_EDGE ( 'NONE', *, *, #13224, .T. ) ;
#33232 = CARTESIAN_POINT ( 'NONE',  ( -106.6183162539999927, 1379.688366450070134, 308.3260602744589960 ) ) ;
#33233 = CARTESIAN_POINT ( 'NONE',  ( 0.08492873675443529669, 1416.830086716310007, 227.2254341622459890 ) ) ;
#33234 = CARTESIAN_POINT ( 'NONE',  ( -8.321621049119999114, 1385.382011555610006, 218.6716072806289901 ) ) ;
#33237 = EDGE_CURVE ( 'NONE', #27375, #102562, #60892, .T. ) ;
#33236 = DIRECTION ( 'NONE',  ( 5.980589973904019347E-17, -1.000000000000000000, 1.736889445713099699E-16 ) ) ;
#33235 = CARTESIAN_POINT ( 'NONE',  ( 1.285642914329999886, 1444.921654895390020, 199.8418900409189973 ) ) ;
#33238 = CARTESIAN_POINT ( 'NONE',  ( 13.07344732962040013, 1516.551188146170034, 192.4513774157680075 ) ) ;
#33239 = CARTESIAN_POINT ( 'NONE',  ( 0.1442700600540000044, 1449.244366658050012, 183.3525652805980144 ) ) ;
#33240 = CARTESIAN_POINT ( 'NONE',  ( 2.902322711624676882E-15, 1524.090675761330203, 185.4225825198192013 ) ) ;
#33241 = FACE_OUTER_BOUND ( 'NONE', #90026, .T. ) ;
#33242 = CARTESIAN_POINT ( 'NONE',  ( 10.65114734267110030, 1480.262814529339948, 208.4911516818010284 ) ) ;
#33243 = CARTESIAN_POINT ( 'NONE',  ( 0.9063479630919999419, 1415.579607672129896, 190.7747571620979841 ) ) ;
#33244 = CARTESIAN_POINT ( 'NONE',  ( 10.95578206839999957, 1431.353415687319966, 151.7028741494979727 ) ) ;
#33245 = CARTESIAN_POINT ( 'NONE',  ( 6.126746143464999683, 1514.923664147150021, 200.9956116846470309 ) ) ;
#33246 = ORIENTED_EDGE ( 'NONE', *, *, #62192, .F. ) ;
#33247 = CARTESIAN_POINT ( 'NONE',  ( 13.04378404802559999, 1435.095357528140084, 150.1247056565019875 ) ) ;
#33248 = VERTEX_POINT ( 'NONE', #103962 ) ;
#33249 = VERTEX_POINT ( 'NONE', #93894 ) ;
#33250 = CARTESIAN_POINT ( 'NONE',  ( 13.50674943976829923, 1444.060515704980617, 169.3531493163527841 ) ) ;
#33251 = CARTESIAN_POINT ( 'NONE',  ( -10.86270151549999952, 1462.682638981130140, 232.4998425783980167 ) ) ;
#33252 = DIRECTION ( 'NONE',  ( 0.000000000000000000, 0.000000000000000000, 1.000000000000000000 ) ) ;
#33253 = CARTESIAN_POINT ( 'NONE',  ( -3.454172653555000139, 1517.122088787240045, 216.8462693643270143 ) ) ;
#33254 = CARTESIAN_POINT ( 'NONE',  ( -8.143463389314709033, 1511.512554418091668, 212.9586518629134275 ) ) ;
#33255 = CARTESIAN_POINT ( 'NONE',  ( -11.92155900329999874, 1502.317141431590017, 208.8109435272550058 ) ) ;
#33256 = CARTESIAN_POINT ( 'NONE',  ( -1.795474957570000196, 1417.667352959230129, 185.7226290440979994 ) ) ;
#33257 = CARTESIAN_POINT ( 'NONE',  ( 8.345162679097549211E-14, 1380.413060387289988, 209.1218459572589836 ) ) ;
#33258 = VECTOR ( 'NONE', #20994, 1000.000000000000000 ) ;
#33259 = CIRCLE ( 'NONE', #51101, 95.87902101811344835 ) ;
#33260 = ORIENTED_EDGE ( 'NONE', *, *, #110424, .F. ) ;
#33261 = CARTESIAN_POINT ( 'NONE',  ( -4.042729840925000317, 1516.919782530640077, 205.8674445284970034 ) ) ;
#33262 = ORIENTED_EDGE ( 'NONE', *, *, #76944, .F. ) ;
#33263 = CARTESIAN_POINT ( 'NONE',  ( -103.5697756572089929, 1379.884498099829898, 304.5397370025139594 ) ) ;
#33264 = CARTESIAN_POINT ( 'NONE',  ( -19.41936053389999728, 1509.602162800930046, 231.4138353120980014 ) ) ;
#33265 = CARTESIAN_POINT ( 'NONE',  ( -2.825023580110000321, 1409.011712384230123, 187.6092932735979844 ) ) ;
#33266 = CARTESIAN_POINT ( 'NONE',  ( 7.668984210275000102, 1514.216129015430170, 215.2460172970970120 ) ) ;
#33268 = ORIENTED_EDGE ( 'NONE', *, *, #23541, .T. ) ;
#33267 = CARTESIAN_POINT ( 'NONE',  ( -0.04548916784355099691, 1416.835419214280137, 227.2860346676060033 ) ) ;
#33269 = CARTESIAN_POINT ( 'NONE',  ( 20.47396129670000064, 1428.228733271429974, 221.3183212327980129 ) ) ;
#33270 = CARTESIAN_POINT ( 'NONE',  ( -16.31523981255880074, 1508.551704408389924, 210.3829298100710048 ) ) ;
#33271 = DIRECTION ( 'NONE',  ( -0.7122454525621805255, 0.000000000000000000, -0.7019304917899598095 ) ) ;
#33272 = CARTESIAN_POINT ( 'NONE',  ( 0.003131168146805529684, 1465.436577107210042, 236.3247334268170050 ) ) ;
#33273 = CARTESIAN_POINT ( 'NONE',  ( 0.01306000193830150063, 1516.939762005280045, 213.7404293621069939 ) ) ;
#33274 = CARTESIAN_POINT ( 'NONE',  ( -2.543708339781890260, 1429.172938267450036, 200.1013465518929877 ) ) ;
#33275 = VECTOR ( 'NONE', #24323, 1000.000000000000000 ) ;
#33276 = CARTESIAN_POINT ( 'NONE',  ( -21.29838079570000176, 1509.400478363229922, 190.2048059474979880 ) ) ;
#33277 = CARTESIAN_POINT ( 'NONE',  ( -11.60004869885203682, 1422.222932908413441, 135.5999999980979851 ) ) ;
#33278 = CARTESIAN_POINT ( 'NONE',  ( 6.563254890855000134, 1517.139039350860003, 211.6051684241269868 ) ) ;
#33279 = CARTESIAN_POINT ( 'NONE',  ( 9.710109577146511128, 1434.985020983699997, 207.7973431748550013 ) ) ;
#33280 = CARTESIAN_POINT ( 'NONE',  ( 0.3035063570619999651, 1419.252315944230077, 184.6483515716980151 ) ) ;
#33281 = CARTESIAN_POINT ( 'NONE',  ( 0.3788332004054269508, 1408.926289534200123, 231.6114332047860103 ) ) ;
#33283 = VERTEX_POINT ( 'NONE', #41849 ) ;
#33282 = CARTESIAN_POINT ( 'NONE',  ( -68.75438398539999696, 1390.682777697860047, 280.7419924920590120 ) ) ;
#33284 = CARTESIAN_POINT ( 'NONE',  ( -40.89054236768439665, 1385.176891340569910, 243.6910935257890003 ) ) ;
#33285 = CARTESIAN_POINT ( 'NONE',  ( 5.805167347800000321, 1470.400767513130177, 255.2684315055980164 ) ) ;
#33286 = CARTESIAN_POINT ( 'NONE',  ( -16.99532478110185352, 1414.913372219064513, 207.6629708034409987 ) ) ;
#33287 = CARTESIAN_POINT ( 'NONE',  ( -5.106121334268481249, 1414.913060387329779, 224.8220620046302258 ) ) ;
#33288 = CARTESIAN_POINT ( 'NONE',  ( 7.799999999999999822, 1412.913060387329779, 209.1218459616989946 ) ) ;
#33289 = CARTESIAN_POINT ( 'NONE',  ( -23.97381281639999884, 1445.664824722570074, 212.8527451534280033 ) ) ;
#33290 = CARTESIAN_POINT ( 'NONE',  ( 4.987078416198220232, 1508.551704408389924, 211.6097810847190033 ) ) ;
#33292 = CARTESIAN_POINT ( 'NONE',  ( -7.769118763749999879, 1384.901714565510019, 218.9178983622890087 ) ) ;
#33291 = LINE ( 'NONE', #33848, #35753 ) ;
#33293 = CARTESIAN_POINT ( 'NONE',  ( -9.190572780844979306, 1449.577780504580005, 209.0393402580440068 ) ) ;
#33294 = CARTESIAN_POINT ( 'NONE',  ( -107.7743377200740014, 1382.722932455570117, 310.5776286012699643 ) ) ;
#33295 = ORIENTED_EDGE ( 'NONE', *, *, #93946, .F. ) ;
#33296 = CARTESIAN_POINT ( 'NONE',  ( -2.874588960795000148, 1516.606339319019980, 202.5748942495170013 ) ) ;
#33297 = DIRECTION ( 'NONE',  ( 0.000000000000000000, 0.000000000000000000, -1.000000000000000000 ) ) ;
#33298 = CARTESIAN_POINT ( 'NONE',  ( -4.348753001182549001E-06, 1471.791680084430027, 269.8654495627969823 ) ) ;
#33299 = CARTESIAN_POINT ( 'NONE',  ( -34.18677586421132730, 1522.906561336852519, 219.7932833225229388 ) ) ;
#33300 = CARTESIAN_POINT ( 'NONE',  ( -9.124411009920782689, 1461.277107961660022, 205.8277251432190837 ) ) ;
#33301 = CARTESIAN_POINT ( 'NONE',  ( 4.334458048930000196, 1466.050308755590095, 219.2818749650989787 ) ) ;
#33302 = CARTESIAN_POINT ( 'NONE',  ( 10.05619454328154028, 1417.844773168630354, 230.1417765312870358 ) ) ;
#33303 = CARTESIAN_POINT ( 'NONE',  ( 27.07894067153570106, 1435.916767153840055, 136.5177824053259883 ) ) ;
#33304 = CARTESIAN_POINT ( 'NONE',  ( 39.32311757029869170, 1447.249813977000031, 136.6052348694120155 ) ) ;
#33305 = CARTESIAN_POINT ( 'NONE',  ( -41.78301679711650962, 1454.669324826605816, 269.0815855111645760 ) ) ;
#33306 = CARTESIAN_POINT ( 'NONE',  ( -109.8773115550000057, 1385.345135485559922, 297.0432615881589982 ) ) ;
#33307 = ADVANCED_FACE ( 'NONE', ( #84938 ), #1675, .F. ) ;
#33308 = CARTESIAN_POINT ( 'NONE',  ( 10.37139043059999999, 1508.772077727729993, 183.3025791525980139 ) ) ;
#33309 = CARTESIAN_POINT ( 'NONE',  ( 4.704564003757560009, 1507.026338954369976, 219.8246688803149880 ) ) ;
#33310 = CARTESIAN_POINT ( 'NONE',  ( -18.42949978517250642, 1468.381198263613442, 269.3800990424684869 ) ) ;
#33311 = ORIENTED_EDGE ( 'NONE', *, *, #38519, .F. ) ;
#33312 = DIRECTION ( 'NONE',  ( -0.6736849260863841948, 0.000000000000000000, 0.7390186874254148774 ) ) ;
#33313 = CARTESIAN_POINT ( 'NONE',  ( -32.03120862260659152, 1416.568755244754811, 269.3150988356668449 ) ) ;
#33314 = DIRECTION ( 'NONE',  ( -0.8393249826168291960, -0.3829000781212070215, -0.3859029719113770129 ) ) ;
#33315 = CARTESIAN_POINT ( 'NONE',  ( 10.87197521136500633, 1424.812830435537762, 138.2079135145058046 ) ) ;
#33316 = CARTESIAN_POINT ( 'NONE',  ( 11.46786347449999965, 1502.092859008989990, 211.0284006470890006 ) ) ;
#33317 = CARTESIAN_POINT ( 'NONE',  ( -28.26971844339999862, 1508.651302072330054, 208.8373477021380324 ) ) ;
#33318 = CARTESIAN_POINT ( 'NONE',  ( -9.831691212836640048, 1438.525609616689962, 210.5507346167850073 ) ) ;
#33319 = CARTESIAN_POINT ( 'NONE',  ( -6.501609782144663896, 1517.051704408389924, 200.8207946853451631 ) ) ;
#33320 = PRODUCT_DEFINITION_FORMATION_WITH_SPECIFIED_SOURCE ( 'ANY', '', #48283, .NOT_KNOWN. ) ;
#33321 = PLANE ( 'NONE',  #34257 ) ;
#33323 = ADVANCED_FACE ( 'NONE', ( #18287 ), #917, .T. ) ;
#33322 = CARTESIAN_POINT ( 'NONE',  ( -14.45746094946127869, 1451.170343819680056, 150.0640874590992269 ) ) ;
#33324 = CARTESIAN_POINT ( 'NONE',  ( -11.60004869885203682, 1411.254281879943164, 134.0999999980979851 ) ) ;
#33325 = CARTESIAN_POINT ( 'NONE',  ( 24.13987143119999956, 1435.346625637479974, 136.7217067365980085 ) ) ;
#33326 = CARTESIAN_POINT ( 'NONE',  ( 5.551188674472009588, 1510.480349264700180, 216.6723492941099778 ) ) ;
#33327 = ORIENTED_EDGE ( 'NONE', *, *, #2899, .T. ) ;
#33328 = CARTESIAN_POINT ( 'NONE',  ( -0.3622025830936350110, 1416.825783990419950, 191.0664212414500014 ) ) ;
#33329 = CARTESIAN_POINT ( 'NONE',  ( -13.04207679966010147, 1409.368499744919745, 225.9431846064669855 ) ) ;
#33330 = EDGE_CURVE ( 'NONE', #102937, #110607, #46756, .T. ) ;
#33331 = ORIENTED_EDGE ( 'NONE', *, *, #29064, .F. ) ;
#33332 = ORIENTED_EDGE ( 'NONE', *, *, #11217, .T. ) ;
#33333 = CARTESIAN_POINT ( 'NONE',  ( 4.208240993269999564, 1434.939300248989866, 227.0651965576989824 ) ) ;
#33334 = CARTESIAN_POINT ( 'NONE',  ( -19.00259723423865665, 1526.382868172570852, 232.9129335399678098 ) ) ;
#33336 = CARTESIAN_POINT ( 'NONE',  ( -28.01911545699999806, 1442.727873585590032, 231.7019063253979994 ) ) ;
#33335 = CARTESIAN_POINT ( 'NONE',  ( 4.301794564619999761, 1454.418299454290036, 217.4807569431989975 ) ) ;
#33337 = CARTESIAN_POINT ( 'NONE',  ( -7.305751433210000201, 1447.589639846790078, 214.8024071067289924 ) ) ;
#33338 = CARTESIAN_POINT ( 'NONE',  ( -11.07594373419999911, 1433.015750972510205, 151.6980226098980040 ) ) ;
#33339 = CARTESIAN_POINT ( 'NONE',  ( -12.30920746619560013, 1378.375653480090023, 209.8169089701579821 ) ) ;
#33340 = B_SPLINE_CURVE_WITH_KNOTS ( 'NONE', 4,
 ( #30847, #90756, #89109, #72873, #73973 ),
 .UNSPECIFIED., .F., .F.,
 ( 5, 5 ),
 ( 9.931291899967220616E-17, 0.009483690916888028524 ),
 .UNSPECIFIED. ) ;
#33341 = CARTESIAN_POINT ( 'NONE',  ( -2.740720916264808515, 1420.074197278511519, 186.0641697093491302 ) ) ;
#33342 = CARTESIAN_POINT ( 'NONE',  ( 7.346975979479999808, 1425.060309264630177, 212.5630391892889861 ) ) ;
#33343 = CARTESIAN_POINT ( 'NONE',  ( -24.63975812940000054, 1440.017819941759853, 210.6779373860979945 ) ) ;
#33344 = FACE_BOUND ( 'NONE', #97058, .T. ) ;
#33345 = CARTESIAN_POINT ( 'NONE',  ( -2.825023819243769996, 1409.011713080599975, 187.6092914852009983 ) ) ;
#33346 = CARTESIAN_POINT ( 'NONE',  ( 6.528782948190136715, 1363.530450965401315, 208.3718459617061285 ) ) ;
#33347 = CARTESIAN_POINT ( 'NONE',  ( -20.55130959458017870, 1509.748513648901735, 230.9769706060577903 ) ) ;
#33349 = VERTEX_POINT ( 'NONE', #11568 ) ;
#33348 = CARTESIAN_POINT ( 'NONE',  ( -2.407902493171400187E-09, 1415.709304463629906, 241.9018706941139669 ) ) ;
#33350 = ORIENTED_EDGE ( 'NONE', *, *, #11102, .F. ) ;
#33351 = CARTESIAN_POINT ( 'NONE',  ( -11.80969502400810001, 1428.721338179349914, 148.6497889493599871 ) ) ;
#33352 = CARTESIAN_POINT ( 'NONE',  ( 7.540791903005830576, 1510.557600718605045, 203.3531818223969765 ) ) ;
#33353 = CARTESIAN_POINT ( 'NONE',  ( -4.832500121020000705, 1471.592195475830067, 269.8673040278980011 ) ) ;
#33354 = CARTESIAN_POINT ( 'NONE',  ( 11.89349302229567407, 1433.282476700868756, 147.6489928588556779 ) ) ;
#33355 =( BOUNDED_CURVE ( )  B_SPLINE_CURVE ( 3, ( #66613, #66060, #67155, #30770 ),
 .UNSPECIFIED., .F., .F. ) 
 B_SPLINE_CURVE_WITH_KNOTS ( ( 4, 4 ),
 ( 4.177898400101880405, 5.246901559513639235 ),
 .UNSPECIFIED. ) 
 CURVE ( )  GEOMETRIC_REPRESENTATION_ITEM ( )  RATIONAL_B_SPLINE_CURVE ( ( 1.000000000000000000, 0.9070150916865978852, 0.9070150916865978852, 1.000000000000000000 ) ) 
 REPRESENTATION_ITEM ( '' )  );
#33357 = EDGE_CURVE ( 'NONE', #44161, #17382, #88275, .T. ) ;
#33356 = CARTESIAN_POINT ( 'NONE',  ( -107.0745166769187335, 1314.643966242389979, 314.8853230801587415 ) ) ;
#33358 = CARTESIAN_POINT ( 'NONE',  ( 20.55257633559999775, 1497.713060387329961, 201.0220267247279935 ) ) ;
#33359 = FACE_OUTER_BOUND ( 'NONE', #49634, .T. ) ;
#33360 = FACE_BOUND ( 'NONE', #45368, .T. ) ;
#33361 = CARTESIAN_POINT ( 'NONE',  ( -14.59882275880000080, 1475.513060387329915, 194.5230232033979973 ) ) ;
#33362 = CARTESIAN_POINT ( 'NONE',  ( 6.358435812109480167, 1368.427897723174055, 210.6218459616991936 ) ) ;
#33363 = CARTESIAN_POINT ( 'NONE',  ( -8.662982322953059366, 1448.248813715330016, 211.9993685260630230 ) ) ;
#33364 = CARTESIAN_POINT ( 'NONE',  ( -18.68320425524010275, 1409.179517572200211, 269.1629733292540436 ) ) ;
#33365 = CARTESIAN_POINT ( 'NONE',  ( -13.25378446100000041, 1435.222382017790096, 150.0797423395979990 ) ) ;
#33366 = ORIENTED_EDGE ( 'NONE', *, *, #84206, .T. ) ;
#33367 = DIRECTION ( 'NONE',  ( -0.4090087482554183862, -0.000000000000000000, 0.9125304618754026542 ) ) ;
#33368 = ORIENTED_EDGE ( 'NONE', *, *, #108894, .T. ) ;
#33369 = ORIENTED_EDGE ( 'NONE', *, *, #950, .T. ) ;
#33370 = CARTESIAN_POINT ( 'NONE',  ( -21.98270307515648270, 1506.436298853318931, 209.4394080128124074 ) ) ;
#33371 = DIRECTION ( 'NONE',  ( 1.755985294532464991E-16, -1.000000000000000000, 1.338183447452830017E-16 ) ) ;
#33372 = CARTESIAN_POINT ( 'NONE',  ( -6.935457963315000640, 1516.627618683580067, 212.5772239474869991 ) ) ;
#33373 = CARTESIAN_POINT ( 'NONE',  ( -17.93127365029999964, 1485.487435208230181, 188.8314909439980056 ) ) ;
#33374 = DIRECTION ( 'NONE',  ( 1.755985294532464991E-16, -1.000000000000000000, 1.338183447452830017E-16 ) ) ;
#33375 = EDGE_LOOP ( 'NONE', ( #33434, #1191, #106655, #11382 ) ) ;
#33376 = CARTESIAN_POINT ( 'NONE',  ( 22.74803453391460906, 1523.678648413191695, 234.5603111028696901 ) ) ;
#33377 = CARTESIAN_POINT ( 'NONE',  ( -2.486474780875000512, 1516.560253536979872, 202.1879665292270261 ) ) ;
#33378 = CARTESIAN_POINT ( 'NONE',  ( -29.21606572689999837, 1509.871156552030016, 208.2743117722099839 ) ) ;
#33379 = CARTESIAN_POINT ( 'NONE',  ( 8.598096571001718758, 1427.995879741943554, 134.0999999980979567 ) ) ;
#33380 = CARTESIAN_POINT ( 'NONE',  ( -43.99263692700240114, 1384.595883470080025, 217.1388236433490135 ) ) ;
#33381 = CARTESIAN_POINT ( 'NONE',  ( -5.257351103029999528, 1408.563318624929934, 196.5782129565980085 ) ) ;
#33382 = DIRECTION ( 'NONE',  ( 0.000000000000000000, 0.000000000000000000, 1.000000000000000000 ) ) ;
#33384 = ORIENTED_EDGE ( 'NONE', *, *, #62735, .F. ) ;
#33383 = CARTESIAN_POINT ( 'NONE',  ( -38.48250450509210197, 1443.291876352919871, 137.1415221903179997 ) ) ;
#33385 = CARTESIAN_POINT ( 'NONE',  ( -27.45150841124540264, 1488.737809751009991, 209.5843002502519994 ) ) ;
#33386 = CARTESIAN_POINT ( 'NONE',  ( 26.53391208749999919, 1488.685287627230082, 213.4463815460780154 ) ) ;
#33387 = CARTESIAN_POINT ( 'NONE',  ( -57.81504981494947515, 1379.719253180389387, 261.4703589277106630 ) ) ;
#33388 = CARTESIAN_POINT ( 'NONE',  ( 2.236830499208590339, 1495.676457082710158, 221.2569898128769807 ) ) ;
#33389 = CARTESIAN_POINT ( 'NONE',  ( -3.487592467065220081, 1508.551704408389924, 204.1347675093749956 ) ) ;
#33390 = CARTESIAN_POINT ( 'NONE',  ( 0.1595995995380000143, 1486.508831850330125, 181.8147405652979671 ) ) ;
#33391 = CARTESIAN_POINT ( 'NONE',  ( 2.881548424445000034, 1516.909589401870107, 211.4054166033970148 ) ) ;
#33392 = CARTESIAN_POINT ( 'NONE',  ( -68.33454988889999981, 1379.748399532440089, 279.2380605676589767 ) ) ;
#33393 = CARTESIAN_POINT ( 'NONE',  ( -2.418881086572150174, 1484.257535334039858, 183.1979755142290003 ) ) ;
#33394 = VECTOR ( 'NONE', #39950, 1000.000000000000000 ) ;
#33395 = CARTESIAN_POINT ( 'NONE',  ( -5.970282146669999790, 1449.727869094690050, 209.8750552241949947 ) ) ;
#33396 = CARTESIAN_POINT ( 'NONE',  ( 11.33192158579999820, 1414.988017870030035, 222.3303153933979956 ) ) ;
#33397 = CARTESIAN_POINT ( 'NONE',  ( -3.462835665494999660, 1517.038650117239968, 208.0021282158369900 ) ) ;
#33398 = EDGE_LOOP ( 'NONE', ( #30224, #83895, #48426, #92497 ) ) ;
#33399 = DIRECTION ( 'NONE',  ( -1.000000000000000000, 0.000000000000000000, 0.000000000000000000 ) ) ;
#33400 = CARTESIAN_POINT ( 'NONE',  ( -10.79543140439999860, 1471.481918345589975, 207.1280613816090010 ) ) ;
#33401 = CARTESIAN_POINT ( 'NONE',  ( -1.253790794730949977E-15, 1385.340268378329938, 218.5931445290690078 ) ) ;
#33402 = ORIENTED_EDGE ( 'NONE', *, *, #74787, .T. ) ;
#33403 = PLANE ( 'NONE',  #30194 ) ;
#33404 = CARTESIAN_POINT ( 'NONE',  ( 12.97215231279360026, 1434.791734578659998, 149.5093031009719766 ) ) ;
#33405 = CARTESIAN_POINT ( 'NONE',  ( 17.80303567514379992, 1459.309267358430134, 228.1638295836210375 ) ) ;
#33406 = CARTESIAN_POINT ( 'NONE',  ( 17.83486663330506872, 1523.678648413191695, 237.8759530894958800 ) ) ;
#33407 = CARTESIAN_POINT ( 'NONE',  ( 2.446787376320000096, 1432.353341358199941, 150.2884730787980061 ) ) ;
#33408 = CARTESIAN_POINT ( 'NONE',  ( 9.702207697720000468, 1489.235137281590141, 203.6117652758089775 ) ) ;
#33409 = CARTESIAN_POINT ( 'NONE',  ( -5.940539706237879969, 1519.551704408389924, 229.2045057392767262 ) ) ;
#33410 = CARTESIAN_POINT ( 'NONE',  ( -15.10371725490000117, 1409.440493816029857, 225.2902966875980155 ) ) ;
#33412 = CARTESIAN_POINT ( 'NONE',  ( -4.487249775048080203, 1509.038615934839981, 211.6097811040130239 ) ) ;
#33411 = CARTESIAN_POINT ( 'NONE',  ( -5.775236830874999505, 1516.804776704140068, 214.1294346171470124 ) ) ;
#33413 = CARTESIAN_POINT ( 'NONE',  ( 20.15452299509999889, 1507.845791384329914, 189.3412703934979788 ) ) ;
#33414 = CARTESIAN_POINT ( 'NONE',  ( -5.002593397454999646, 1516.960844870249957, 215.6810146069769871 ) ) ;
#33415 = ORIENTED_EDGE ( 'NONE', *, *, #76082, .T. ) ;
#33416 = CARTESIAN_POINT ( 'NONE',  ( 3.968827103902559550, 1519.551704408389924, 188.7040005461919918 ) ) ;
#33417 = CARTESIAN_POINT ( 'NONE',  ( -16.54305653649999641, 1420.580047969900079, 203.3927685990690009 ) ) ;
#33418 = ORIENTED_EDGE ( 'NONE', *, *, #11184, .F. ) ;
#33419 = CARTESIAN_POINT ( 'NONE',  ( 1.196415586119999874, 1420.167066172730074, 184.5944197207980153 ) ) ;
#33420 = CARTESIAN_POINT ( 'NONE',  ( 32.28466283162151029, 1512.187213306747481, 199.0684425896244250 ) ) ;
#33421 = CARTESIAN_POINT ( 'NONE',  ( 2.311636021096358018, 1525.506916460682305, 176.4384780102049035 ) ) ;
#33422 = CARTESIAN_POINT ( 'NONE',  ( 1273.316865285499944, 2833.596074015639715, 9977.675558181130327 ) ) ;
#33423 = FACE_OUTER_BOUND ( 'NONE', #66621, .T. ) ;
#33424 = CARTESIAN_POINT ( 'NONE',  ( -5.066920007859089914, 1508.235255472309291, 220.4033713207047924 ) ) ;
#33425 = DIRECTION ( 'NONE',  ( 1.192122195693504081E-14, -4.372198439846870180E-16, -1.000000000000000000 ) ) ;
#33426 = CARTESIAN_POINT ( 'NONE',  ( 18.06510344782403621, 1424.836155016811063, 224.7141253419370344 ) ) ;
#33427 = CARTESIAN_POINT ( 'NONE',  ( 11.84242369139999873, 1431.324257919750153, 147.6543138610979895 ) ) ;
#33428 = CARTESIAN_POINT ( 'NONE',  ( -7.419509149259999603, 1440.444625599219989, 149.7273825585979807 ) ) ;
#33429 = CARTESIAN_POINT ( 'NONE',  ( 45.65827091464620224, 1440.913060379439912, 266.1743358949399862 ) ) ;
#33431 = CARTESIAN_POINT ( 'NONE',  ( -20.51044083270000229, 1453.146242308330102, 207.5895558364179863 ) ) ;
#33430 = CARTESIAN_POINT ( 'NONE',  ( -10.55936701243939879, 1471.180347189670101, 209.5615340540499858 ) ) ;
#33432 = CARTESIAN_POINT ( 'NONE',  ( 12.78657892559999887, 1416.813004075630033, 222.2779166417979866 ) ) ;
#33433 = ORIENTED_EDGE ( 'NONE', *, *, #41792, .T. ) ;
#33434 = ORIENTED_EDGE ( 'NONE', *, *, #44069, .T. ) ;
#33435 = CARTESIAN_POINT ( 'NONE',  ( 14.59276606620000116, 1436.244837803880046, 149.8707691859979718 ) ) ;
#33436 = CARTESIAN_POINT ( 'NONE',  ( -19.67818152874250259, 1485.241807130695179, 190.3342238627110419 ) ) ;
#33437 = AXIS2_PLACEMENT_3D ( 'NONE', #105478, #61848, #19801 ) ;
#33438 = CARTESIAN_POINT ( 'NONE',  ( -1.191524307911311809, 1526.382868172863937, 179.0083900503167911 ) ) ;
#33439 = CARTESIAN_POINT ( 'NONE',  ( 9.651066088509999474, 1425.440658930580184, 195.4941615409990163 ) ) ;
#33440 = CARTESIAN_POINT ( 'NONE',  ( -13.15726448721240160, 1416.851343896870048, 221.9096085506390068 ) ) ;
#33441 = CARTESIAN_POINT ( 'NONE',  ( 9.971732002342131196, 1422.489342820810180, 212.1848988156249902 ) ) ;
#33442 = B_SPLINE_CURVE_WITH_KNOTS ( 'NONE', 3,
 ( #44827, #26328, #77856, #80488, #72116, #106231, #29517, #63707, #4336, #97818 ),
 .UNSPECIFIED., .F., .F.,
 ( 4, 2, 2, 2, 4 ),
 ( 0.000000000000000000, 0.0007189769279725889304, 0.001437953855945177861, 0.002156930783917766683, 0.002875907711890355722 ),
 .UNSPECIFIED. ) ;
#33443 = PLANE ( 'NONE',  #98735 ) ;
#33444 = CARTESIAN_POINT ( 'NONE',  ( 10.37959279779999910, 1453.090483345690018, 190.0119662633989890 ) ) ;
#33445 = CARTESIAN_POINT ( 'NONE',  ( -67.95646974556258613, 1383.787266834509865, 292.3773730337559869 ) ) ;
#33446 = CARTESIAN_POINT ( 'NONE',  ( -107.4538559658096801, 1379.578066768433700, 299.0810616127055823 ) ) ;
#33447 = DIRECTION ( 'NONE',  ( 0.1144950856934970618, -0.9861828161603604093, 0.1197260559028810595 ) ) ;
#33448 = CARTESIAN_POINT ( 'NONE',  ( 11.44464715210460071, 1491.838548702460230, 209.9183825457590160 ) ) ;
#33450 = ORIENTED_EDGE ( 'NONE', *, *, #108159, .F. ) ;
#33449 = CARTESIAN_POINT ( 'NONE',  ( -2.280001584889999933, 1457.248781993690045, 218.7633449024490062 ) ) ;
#33451 = CARTESIAN_POINT ( 'NONE',  ( 33.17484411121481713, 1525.713797967457140, 217.3801513758794215 ) ) ;
#33452 = CARTESIAN_POINT ( 'NONE',  ( -43.54658723890000260, 1380.341181800959930, 221.0116611961589967 ) ) ;
#33453 = CARTESIAN_POINT ( 'NONE',  ( -3.100192419969999946, 1431.506313241990028, 216.9304414810590060 ) ) ;
#33454 = VERTEX_POINT ( 'NONE', #45744 ) ;
#33455 = CARTESIAN_POINT ( 'NONE',  ( 14.90569475453980175, 1509.413384249990031, 233.7754132121639827 ) ) ;
#33456 = DIRECTION ( 'NONE',  ( 0.000000000000000000, -0.02617694830808806397, 0.9996573249755517088 ) ) ;
#33457 = CARTESIAN_POINT ( 'NONE',  ( 36.93857276712569870, 1437.876021133649829, 136.5569222567030181 ) ) ;
#33459 = CARTESIAN_POINT ( 'NONE',  ( -7.649034438594999763, 1514.243099272629934, 203.4721261815869866 ) ) ;
#33458 = CARTESIAN_POINT ( 'NONE',  ( 17.83486663330486621, 1523.678648413191695, 180.3677388339000061 ) ) ;
#33460 = CARTESIAN_POINT ( 'NONE',  ( -9.771542533679999920, 1462.553261080089896, 206.2413439940889930 ) ) ;
#33461 = AXIS2_PLACEMENT_3D ( 'NONE', #31645, #16473, #33850 ) ;
#33462 = CARTESIAN_POINT ( 'NONE',  ( -108.4209992690000064, 1381.081465263680002, 298.0761733255590116 ) ) ;
#33463 = CARTESIAN_POINT ( 'NONE',  ( -6.867847813526624101, 1447.894038402013166, 185.5948811633518574 ) ) ;
#33464 = CARTESIAN_POINT ( 'NONE',  ( -11.42381040596369246, 1434.696338602614333, 151.4779332080243250 ) ) ;
#33465 = CARTESIAN_POINT ( 'NONE',  ( -10.41491974136950027, 1508.551704408389924, 218.0827215060540141 ) ) ;
#33466 = CARTESIAN_POINT ( 'NONE',  ( 2.880836473691240407, 1368.383867273139913, 210.4211859087380105 ) ) ;
#33467 = CARTESIAN_POINT ( 'NONE',  ( 1.910568182230000023, 1408.979778898429913, 186.9030642623980043 ) ) ;
#33468 = CARTESIAN_POINT ( 'NONE',  ( -0.4061581754453899573, 1486.016806840350000, 197.2250015105809950 ) ) ;
#33469 = DIRECTION ( 'NONE',  ( 0.2054769195713296304, 0.000000000000000000, -0.9786619618251631847 ) ) ;
#33470 = CARTESIAN_POINT ( 'NONE',  ( -2.500000000000000000, 1439.162586052440020, 158.2749544336289773 ) ) ;
#33471 = CIRCLE ( 'NONE', #105039, 1.000000000000000888 ) ;
#33472 = CARTESIAN_POINT ( 'NONE',  ( -1.806676058779320027, 1450.408993861640056, 183.0756166235049989 ) ) ;
#33473 = EDGE_LOOP ( 'NONE', ( #49198, #657, #95671, #100733 ) ) ;
#33474 = CARTESIAN_POINT ( 'NONE',  ( -2.953102495588340481, 1470.057161604909879, 187.4194597744339887 ) ) ;
#33475 = CARTESIAN_POINT ( 'NONE',  ( -0.8066080222970000158, 1426.500992774829911, 146.0666368882980066 ) ) ;
#33476 = CARTESIAN_POINT ( 'NONE',  ( -2.189515144162804905, 1407.000063894707182, 196.1218408969885161 ) ) ;
#33477 = CARTESIAN_POINT ( 'NONE',  ( 7.722580339391510229, 1517.051704402239920, 213.7119063846940037 ) ) ;
#33478 = CARTESIAN_POINT ( 'NONE',  ( 16.04953034249999888, 1449.500693692240020, 190.3237195885979816 ) ) ;
#33479 = CARTESIAN_POINT ( 'NONE',  ( -4.654638212716369785E-09, 1475.687699392280138, 266.6817061415500234 ) ) ;
#33480 = CARTESIAN_POINT ( 'NONE',  ( -12.78494549719999895, 1502.727917388590186, 208.9468085136539912 ) ) ;
#33481 = CARTESIAN_POINT ( 'NONE',  ( -13.59512407998240135, 1507.703338069740084, 209.3532897553030239 ) ) ;
#33482 = CARTESIAN_POINT ( 'NONE',  ( -20.17395953629999994, 1505.644431352489846, 209.1238650338669913 ) ) ;
#33483 = CARTESIAN_POINT ( 'NONE',  ( -1.886715933359999875, 1476.714922781289943, 198.9125049787990065 ) ) ;
#33484 = CARTESIAN_POINT ( 'NONE',  ( -108.0434378409999994, 1387.272578177979995, 310.5209596992589809 ) ) ;
#33485 = CARTESIAN_POINT ( 'NONE',  ( -7.551708712715099026, 1510.523965798400013, 214.8518856309849809 ) ) ;
#33486 = CARTESIAN_POINT ( 'NONE',  ( -6.297634499852111212, 1360.310814921950850, 207.6218459616987673 ) ) ;
#33487 = CARTESIAN_POINT ( 'NONE',  ( -46.09936160196500055, 1439.223420885880159, 268.2062399438970033 ) ) ;
#33488 = CARTESIAN_POINT ( 'NONE',  ( 3.085209382068490047, 1428.771282319309876, 216.8020061943259975 ) ) ;
#33489 = CARTESIAN_POINT ( 'NONE',  ( -7.544801320229999497, 1425.914425209869933, 205.6925056590089866 ) ) ;
#33490 = CARTESIAN_POINT ( 'NONE',  ( -6.949703372784999722, 1517.130100026000036, 208.3827239650380250 ) ) ;
#33491 = DIRECTION ( 'NONE',  ( -1.000000000000000000, 0.000000000000000000, 0.000000000000000000 ) ) ;
#33492 = CIRCLE ( 'NONE', #55054, 1.999999999862774658 ) ;
#33493 = CARTESIAN_POINT ( 'NONE',  ( 19.29679066396858289, 1456.533063871148443, 224.7183538900586655 ) ) ;
#33494 = CARTESIAN_POINT ( 'NONE',  ( 7.461100860251050015, 1426.110972386630010, 212.4219345183129803 ) ) ;
#33495 = CARTESIAN_POINT ( 'NONE',  ( -25.98931941724259786, 1450.776361986090023, 136.7278132101320125 ) ) ;
#33496 = ORIENTED_EDGE ( 'NONE', *, *, #30950, .T. ) ;
#33497 = CARTESIAN_POINT ( 'NONE',  ( 25.86260026499999753, 1439.222596320959838, 221.4996202120980229 ) ) ;
#33499 = CARTESIAN_POINT ( 'NONE',  ( -15.28055240982140006, 1513.058738973559912, 223.0831704950950041 ) ) ;
#33498 = CARTESIAN_POINT ( 'NONE',  ( -3.017174818680797177, 1525.408337840050081, 176.9098480759781182 ) ) ;
#33500 = CARTESIAN_POINT ( 'NONE',  ( -6.403692060479999171, 1460.996305860290249, 208.5086931504900178 ) ) ;
#33501 = CARTESIAN_POINT ( 'NONE',  ( -3.984081755090763011, 1515.551704407335137, 207.2788837462810534 ) ) ;
#33502 = CARTESIAN_POINT ( 'NONE',  ( 3.552717040180000119, 1420.594650159299817, 205.3542343418889971 ) ) ;
#33503 = DIRECTION ( 'NONE',  ( 1.788933584601080738E-15, 0.000000000000000000, 1.000000000000000000 ) ) ;
#33504 = CARTESIAN_POINT ( 'NONE',  ( -9230.682934426007705, 2837.541834147241843, -5630.801423372711724 ) ) ;
#33505 = ORIENTED_EDGE ( 'NONE', *, *, #9115, .F. ) ;
#33506 = CARTESIAN_POINT ( 'NONE',  ( -1.847327201898169902, 1408.584742853789976, 270.4287613073750549 ) ) ;
#33507 = CARTESIAN_POINT ( 'NONE',  ( 6.270129375719379894, 1418.078661284499958, 232.0014322324400098 ) ) ;
#33508 = CARTESIAN_POINT ( 'NONE',  ( -5.513435596820279727, 1509.038615934079871, 216.6345961782780023 ) ) ;
#33509 = ORIENTED_EDGE ( 'NONE', *, *, #75298, .F. ) ;
#33510 = EDGE_LOOP ( 'NONE', ( #89919, #98645, #5857, #67774, #761, #31685 ) ) ;
#33511 = CARTESIAN_POINT ( 'NONE',  ( -22.82353090123229933, 1409.710023875719799, 209.0053221533019894 ) ) ;
#33512 = CARTESIAN_POINT ( 'NONE',  ( -3.696362419970000257, 1424.349081209429869, 185.3675292160980064 ) ) ;
#33513 = CARTESIAN_POINT ( 'NONE',  ( -104.3512419375300055, 1378.528619065190014, 309.1652050167789980 ) ) ;
#33514 = CIRCLE ( 'NONE', #96123, 1.749999999999997558 ) ;
#33515 = CARTESIAN_POINT ( 'NONE',  ( -7.214502255410000231, 1427.316505021429975, 144.1938086916980239 ) ) ;
#33516 = CARTESIAN_POINT ( 'NONE',  ( -18.89036777432109915, 1416.702560751849887, 207.5747689616710261 ) ) ;
#33517 = CARTESIAN_POINT ( 'NONE',  ( -22.55028051829999924, 1415.846227990229863, 213.4522806374379797 ) ) ;
#33518 = EDGE_CURVE ( 'NONE', #63746, #21533, #79218, .T. ) ;
#33519 = CARTESIAN_POINT ( 'NONE',  ( 28.57628399200979885, 1468.636142906849955, 267.5038535851290362 ) ) ;
#33520 = EDGE_CURVE ( 'NONE', #102192, #42879, #67334, .T. ) ;
#33521 = CARTESIAN_POINT ( 'NONE',  ( -10.31714591064990039, 1391.913060387289988, 204.4067887391230158 ) ) ;
#33522 = CARTESIAN_POINT ( 'NONE',  ( -16.78273306371495721, 1421.715029943856734, 226.9035938626332438 ) ) ;
#33523 = CARTESIAN_POINT ( 'NONE',  ( -6.948321743994999800, 1517.049325831759916, 205.0875650164470017 ) ) ;
#33524 = ORIENTED_EDGE ( 'NONE', *, *, #8349, .T. ) ;
#33525 = LINE ( 'NONE', #58215, #83050 ) ;
#33526 = CARTESIAN_POINT ( 'NONE',  ( 15.31239853924400052, 1512.759354980439866, 195.5364289879649959 ) ) ;
#33527 = CARTESIAN_POINT ( 'NONE',  ( 22.99329315949999852, 1409.822368751529893, 208.3677801514749888 ) ) ;
#33528 = VERTEX_POINT ( 'NONE', #95566 ) ;
#33529 = CARTESIAN_POINT ( 'NONE',  ( -11.60381925561519800, 1481.105444724209974, 211.4046900983030071 ) ) ;
#33530 = EDGE_CURVE ( 'NONE', #88484, #106272, #5833, .T. ) ;
#33531 = CARTESIAN_POINT ( 'NONE',  ( 26.86339342382879991, 1451.975050932460135, 134.9994894959820044 ) ) ;
#33532 = EDGE_CURVE ( 'NONE', #9564, #87392, #48507, .T. ) ;
#33533 = CARTESIAN_POINT ( 'NONE',  ( -4.206093650348769586, 1508.551704408389924, 213.4237127473219857 ) ) ;
#33534 = CARTESIAN_POINT ( 'NONE',  ( -6.355004503879999156, 1384.926023117790010, 199.7181650675090054 ) ) ;
#33535 = CARTESIAN_POINT ( 'NONE',  ( 7.372986420420000186, 1422.271846737719898, 195.5865301424989866 ) ) ;
#33536 = CARTESIAN_POINT ( 'NONE',  ( -1.578050994240060012, 1432.480027970319952, 218.5065461788099981 ) ) ;
#33537 = CARTESIAN_POINT ( 'NONE',  ( -4.396663909700000872, 1496.560935200589938, 198.7783260529990059 ) ) ;
#33538 = CARTESIAN_POINT ( 'NONE',  ( 1.358157591254900209, 1408.960488295489995, 186.7573064037119934 ) ) ;
#33540 = LINE ( 'NONE', #84516, #93775 ) ;
#33539 = CARTESIAN_POINT ( 'NONE',  ( 30.38288201977627878, 1524.477587234266139, 196.4016200325754369 ) ) ;
#33541 = CIRCLE ( 'NONE', #97969, 2.500000000000002220 ) ;
#33542 = CARTESIAN_POINT ( 'NONE',  ( 1.099392875928770108, 1450.807449935850173, 181.4766395928249949 ) ) ;
#33543 = B_SPLINE_CURVE_WITH_KNOTS ( 'NONE', 5,
 ( #94742, #27546, #2380, #51651, #162, #102569 ),
 .UNSPECIFIED., .F., .F.,
 ( 6, 6 ),
 ( -2.000000000000000000, 0.000000000000000000 ),
 .UNSPECIFIED. ) ;
#33544 = CARTESIAN_POINT ( 'NONE',  ( -12.20251463719999840, 1379.349961885989842, 213.2031273694090032 ) ) ;
#33545 = CARTESIAN_POINT ( 'NONE',  ( 2.340423001224530619, 1525.425686270222059, 241.8895327159822841 ) ) ;
#33546 = ORIENTED_EDGE ( 'NONE', *, *, #106146, .F. ) ;
#33547 = CARTESIAN_POINT ( 'NONE',  ( 11.48654377539569893, 1414.913057860449953, 220.8288015276069984 ) ) ;
#33548 = CARTESIAN_POINT ( 'NONE',  ( 11.72314628525600000, 1432.337468529400212, 150.7717701949150069 ) ) ;
#33549 = VECTOR ( 'NONE', #14066, 1000.000000000000114 ) ;
#33550 = CARTESIAN_POINT ( 'NONE',  ( -10.38271356220340103, 1483.373521473610026, 203.2896237654969980 ) ) ;
#33551 = TOROIDAL_SURFACE ( 'NONE', #74756, 7.016581249619999738, 2.000000000000000000 ) ;
#33552 = CARTESIAN_POINT ( 'NONE',  ( 8.729815835326180107, 1423.787549604110154, 211.0527875084169978 ) ) ;
#33553 = EDGE_CURVE ( 'NONE', #94371, #18109, #71327, .T. ) ;
#33554 = CARTESIAN_POINT ( 'NONE',  ( 11.00321081153069969, 1423.193864714949996, 203.2865044889030059 ) ) ;
#33555 = B_SPLINE_CURVE_WITH_KNOTS ( 'NONE', 5,
 ( #20826, #19158, #29245, #37090, #96454, #40253 ),
 .UNSPECIFIED., .F., .F.,
 ( 6, 6 ),
 ( 0.000000000000000000, 1.000000000000000000 ),
 .UNSPECIFIED. ) ;
#33556 = CARTESIAN_POINT ( 'NONE',  ( 1.338019556329999915, 1431.361302696190023, 218.5179664551590122 ) ) ;
#33557 = CARTESIAN_POINT ( 'NONE',  ( -1.636503137890000126, 1433.447543843880112, 150.4001344053979778 ) ) ;
#33558 = B_SPLINE_CURVE_WITH_KNOTS ( 'NONE', 5,
 ( #45029, #80812, #35489, #37156, #103805, #10283, #71349, #10857, #44460, #79175, #36598, #27646, #61833, #2482, #28753 ),
 .UNSPECIFIED., .F., .F.,
 ( 6, 3, 3, 3, 6 ),
 ( 0.000000000000000000, 0.3169994908698778313, 0.4228046033745412324, 0.6719997599498082064, 1.000000000000000000 ),
 .UNSPECIFIED. ) ;
#33559 = CARTESIAN_POINT ( 'NONE',  ( -21.33887670626219801, 1508.922069394937125, 191.9015789802110703 ) ) ;
#33560 = CARTESIAN_POINT ( 'NONE',  ( 11.87929288849999843, 1433.122288330840092, 150.0887009630980060 ) ) ;
#33561 = CARTESIAN_POINT ( 'NONE',  ( 6.215408291410000174, 1454.402584563930077, 214.3676144197379756 ) ) ;
#33562 = CARTESIAN_POINT ( 'NONE',  ( 12.02797161417169924, 1415.088136167450102, 197.1259520390879914 ) ) ;
#33563 = ADVANCED_FACE ( 'NONE', ( #88822 ), #73200, .F. ) ;
#33564 = CARTESIAN_POINT ( 'NONE',  ( 2.470168521978398868, 1501.977400791986611, 242.8787258963054683 ) ) ;
#33565 = CARTESIAN_POINT ( 'NONE',  ( 9.076018398308100643, 1424.724030148510110, 196.5059690868249902 ) ) ;
#33566 = EDGE_CURVE ( 'NONE', #8681, #43690, #52098, .T. ) ;
#33567 = CARTESIAN_POINT ( 'NONE',  ( 9.777144235831070063, 1463.043760913599954, 213.2472973885180068 ) ) ;
#33568 = FACE_OUTER_BOUND ( 'NONE', #52891, .T. ) ;
#33569 = CARTESIAN_POINT ( 'NONE',  ( 6.252266454184999489, 1511.741868877540128, 217.9101624594169948 ) ) ;
#33570 = CARTESIAN_POINT ( 'NONE',  ( 0.04886115394894129799, 1508.952074335740008, 238.8419220553400351 ) ) ;
#33571 = AXIS2_PLACEMENT_3D ( 'NONE', #108655, #42555, #19 ) ;
#33572 = CARTESIAN_POINT ( 'NONE',  ( 23.67770893690000023, 1410.915352766729939, 211.2317889356880016 ) ) ;
#33573 = CARTESIAN_POINT ( 'NONE',  ( -0.2116227187891456529, 1477.625743691535718, 198.7159279415461697 ) ) ;
#33574 = CARTESIAN_POINT ( 'NONE',  ( -34.93121270820218172, 1435.717331548646598, 135.0378024103818575 ) ) ;
#33575 = CARTESIAN_POINT ( 'NONE',  ( -16.90947605223539796, 1383.856729902519874, 219.7128039564150015 ) ) ;
#33576 = CARTESIAN_POINT ( 'NONE',  ( 12.75035444685179975, 1426.659570474229895, 203.9315474661299845 ) ) ;
#33577 = CARTESIAN_POINT ( 'NONE',  ( 18.99431337219000326, 1459.501208559760016, 220.3864240110139860 ) ) ;
#33578 = CARTESIAN_POINT ( 'NONE',  ( -2.478306858074999841, 1516.938330505699923, 212.5844667883370107 ) ) ;
#33579 = CARTESIAN_POINT ( 'NONE',  ( -13.24697265328699913, 1421.521121240300090, 208.1594402398530121 ) ) ;
#33580 = CARTESIAN_POINT ( 'NONE',  ( 0.1926304896301150038, 1467.201837219709887, 182.6439754155339870 ) ) ;
#33582 = ORIENTED_EDGE ( 'NONE', *, *, #102175, .T. ) ;
#33581 = FACE_OUTER_BOUND ( 'NONE', #7362, .T. ) ;
#33583 = CARTESIAN_POINT ( 'NONE',  ( -25.00312495901935250, 1451.477102942365264, 137.4959198732346408 ) ) ;
#33584 = CARTESIAN_POINT ( 'NONE',  ( -34.00767267269074523, 1443.913060387329324, 154.9192896682974663 ) ) ;
#33585 = CARTESIAN_POINT ( 'NONE',  ( 11.87507418750000099, 1433.007222232190088, 149.7888126920979914 ) ) ;
#33586 = CARTESIAN_POINT ( 'NONE',  ( -41.65030538158350026, 1443.228731900419916, 134.0999999981379744 ) ) ;
#33587 = CARTESIAN_POINT ( 'NONE',  ( -34.35673827249829770, 1445.503283575680143, 137.0830489703820092 ) ) ;
#33588 = ORIENTED_EDGE ( 'NONE', *, *, #29773, .T. ) ;
#33589 = CARTESIAN_POINT ( 'NONE',  ( -10.94922717770000098, 1470.861560407889783, 209.5255082979219878 ) ) ;
#33590 = CARTESIAN_POINT ( 'NONE',  ( 10.47956906020000112, 1478.583002912489974, 204.7952642272489925 ) ) ;
#33591 = CARTESIAN_POINT ( 'NONE',  ( -17.36177561119999879, 1416.518532928330160, 214.4540685280980199 ) ) ;
#33592 = CARTESIAN_POINT ( 'NONE',  ( 8.212352435486090840, 1503.127186295949969, 210.4119011823910057 ) ) ;
#33593 = CARTESIAN_POINT ( 'NONE',  ( 6.250429024355669938, 1467.523505036979941, 206.1081765850969987 ) ) ;
#33594 = VECTOR ( 'NONE', #29772, 1000.000000000000000 ) ;
#33595 = CARTESIAN_POINT ( 'NONE',  ( -108.0762150893491338, 1380.825853547843508, 310.0506996129533377 ) ) ;
#33596 = CARTESIAN_POINT ( 'NONE',  ( -16.21478424889999559, 1417.659049898350077, 209.2181137195750296 ) ) ;
#33597 = CARTESIAN_POINT ( 'NONE',  ( 7.926558117193340358, 1409.189861896230013, 221.8168932242559777 ) ) ;
#33598 = CARTESIAN_POINT ( 'NONE',  ( -12.56636063060000019, 1391.397300678690044, 209.2272092290610033 ) ) ;
#33599 = CARTESIAN_POINT ( 'NONE',  ( -74.21234409784548802, 1385.132681138179805, 274.0804497861159916 ) ) ;
#33600 = CARTESIAN_POINT ( 'NONE',  ( -11.49366809032010117, 1391.913060387289988, 210.9873680687220201 ) ) ;
#33601 = CARTESIAN_POINT ( 'NONE',  ( 10.86658986439489816, 1422.901391916879902, 206.8975148066129748 ) ) ;
#33602 = ORIENTED_EDGE ( 'NONE', *, *, #13996, .T. ) ;
#33603 = CARTESIAN_POINT ( 'NONE',  ( -33.91369268630000278, 1451.728774195029928, 134.7155787906980038 ) ) ;
#33604 = CARTESIAN_POINT ( 'NONE',  ( 12.73318793669440829, 1442.831169986190389, 164.6858276811441328 ) ) ;
#33606 = ORIENTED_EDGE ( 'NONE', *, *, #93229, .F. ) ;
#33605 = CARTESIAN_POINT ( 'NONE',  ( 2.370970874524633398, 1427.002265528473799, 134.0999999980980135 ) ) ;
#33607 = CARTESIAN_POINT ( 'NONE',  ( 0.000000000000000000, 1516.051704408390151, 209.1218459616989946 ) ) ;
#33608 = CARTESIAN_POINT ( 'NONE',  ( -17.38483621660000011, 1410.884422118429939, 225.7833436061980024 ) ) ;
#33609 = CARTESIAN_POINT ( 'NONE',  ( -7.426018358933801800, 1364.078817793960070, 208.3718459617061285 ) ) ;
#33610 = CARTESIAN_POINT ( 'NONE',  ( -10.73077433369999945, 1492.937000258489888, 206.1586420614789859 ) ) ;
#33611 = CARTESIAN_POINT ( 'NONE',  ( 37.99560157342931177, 1453.980171722192608, 269.5760773822823921 ) ) ;
#33612 = CARTESIAN_POINT ( 'NONE',  ( 2.182463076968403026, 1517.051704408389924, 201.3992656178301104 ) ) ;
#33613 = CARTESIAN_POINT ( 'NONE',  ( 17.49699257007802089, 1434.033957849185526, 216.2913140874469775 ) ) ;
#33614 = CARTESIAN_POINT ( 'NONE',  ( -10855.50032577649290, 5181.793945261120825, 7511.881964575620259 ) ) ;
#33615 = CARTESIAN_POINT ( 'NONE',  ( 2.500000000000039968, 1439.615672328189930, 182.7715275322960053 ) ) ;
#33616 = DIRECTION ( 'NONE',  ( 0.000000000000000000, 0.000000000000000000, -1.000000000000000000 ) ) ;
#33617 = CARTESIAN_POINT ( 'NONE',  ( 11.89850863680000082, 1497.713060387329961, 228.0402318450979919 ) ) ;
#33618 = AXIS2_PLACEMENT_3D ( 'NONE', #7552, #31644, #107807 ) ;
#33619 = CARTESIAN_POINT ( 'NONE',  ( -9.105994434067794074, 1449.807959746201050, 207.8187243124739041 ) ) ;
#33620 = ADVANCED_FACE ( 'NONE', ( #52360 ), #6162, .T. ) ;
#33621 = CARTESIAN_POINT ( 'NONE',  ( 4.996642160164999957, 1516.697242742309982, 206.2447328616370044 ) ) ;
#33622 = AXIS2_PLACEMENT_3D ( 'NONE', #27145, #18713, #45071 ) ;
#33624 = EDGE_CURVE ( 'NONE', #23648, #67802, #30658, .T. ) ;
#33623 = CARTESIAN_POINT ( 'NONE',  ( 2.500000000000000000, 1448.831169023560051, 156.2564136193980175 ) ) ;
#33625 = CARTESIAN_POINT ( 'NONE',  ( 1.121218327409999826, 1416.837080243330092, 190.1583373011980029 ) ) ;
#33626 = CARTESIAN_POINT ( 'NONE',  ( 14.00886214219999992, 1416.826388498530150, 196.3918802162980057 ) ) ;
#33629 = EDGE_LOOP ( 'NONE', ( #18136, #54652, #104041, #21362 ) ) ;
#33628 = CARTESIAN_POINT ( 'NONE',  ( -68.71065145783319394, 1379.747782736039881, 280.3144169757910049 ) ) ;
#33627 = AXIS2_PLACEMENT_3D ( 'NONE', #102011, #6857, #42679 ) ;
#33630 = CARTESIAN_POINT ( 'NONE',  ( 40.60394929974220446, 1444.189591584570053, 137.0481280076579935 ) ) ;
#33631 = VERTEX_POINT ( 'NONE', #88157 ) ;
#33632 = AXIS2_PLACEMENT_3D ( 'NONE', #52733, #44335, #45988 ) ;
#33633 = CARTESIAN_POINT ( 'NONE',  ( -16.51878316591069051, 1514.214507862061282, 223.4467145224746503 ) ) ;
#33634 = CARTESIAN_POINT ( 'NONE',  ( -25.48925201569999999, 1449.802587361850101, 207.5067252115079839 ) ) ;
#33636 = CARTESIAN_POINT ( 'NONE',  ( 16.41296274929999655, 1409.863099034130073, 192.1158788459979974 ) ) ;
#33635 = CARTESIAN_POINT ( 'NONE',  ( -10.23174647188330155, 1425.154542701060109, 108.4581586724669933 ) ) ;
#33637 = CARTESIAN_POINT ( 'NONE',  ( 6.951175128784999657, 1517.170721208160103, 211.4121022339570004 ) ) ;
#33638 = CARTESIAN_POINT ( 'NONE',  ( -17.84054676580458221, 1523.580203803270933, 180.3625987673426607 ) ) ;
#33639 = EDGE_CURVE ( 'NONE', #46740, #88970, #79209, .T. ) ;
#33640 = CARTESIAN_POINT ( 'NONE',  ( -18.95884613770000016, 1416.837177098929942, 207.7798960437979758 ) ) ;
#33641 = CARTESIAN_POINT ( 'NONE',  ( -10.81506866279999990, 1424.921186100929845, 144.1620444789979842 ) ) ;
#33642 = CARTESIAN_POINT ( 'NONE',  ( 19.12646062745870168, 1509.604355955109895, 231.7508453187430177 ) ) ;
#33643 = CARTESIAN_POINT ( 'NONE',  ( 10.30873441802069657, 1464.609330832652631, 232.2540526936852814 ) ) ;
#33644 = APPLICATION_PROTOCOL_DEFINITION ( 'draft international standard', 'automotive_design', 1998, #14836 ) ;
#33645 = CARTESIAN_POINT ( 'NONE',  ( 2.843730423744790237, 1508.551704408389924, 214.0849298366779863 ) ) ;
#33646 = B_SPLINE_CURVE_WITH_KNOTS ( 'NONE', 3,
 ( #87163, #103385, #2635, #11012, #36761, #36211, #60887, #68729, #51915, #95014 ),
 .UNSPECIFIED., .F., .F.,
 ( 4, 2, 2, 2, 4 ),
 ( 3.469446951953614189E-18, 0.0007406479101618190525, 0.001481295820323634636, 0.002221943730485450436, 0.002962591640647265802 ),
 .UNSPECIFIED. ) ;
#33647 = CARTESIAN_POINT ( 'NONE',  ( -35.20867138851480149, 1437.188504188790148, 136.5366439520919926 ) ) ;
#33648 = ORIENTED_EDGE ( 'NONE', *, *, #90466, .T. ) ;
#33649 = CARTESIAN_POINT ( 'NONE',  ( 9.759055691533209398, 1396.253854122790017, 215.8358679858959874 ) ) ;
#33650 = CARTESIAN_POINT ( 'NONE',  ( 9.694462811961930271, 1462.254523745029928, 208.2086536884339978 ) ) ;
#33651 = CARTESIAN_POINT ( 'NONE',  ( -18.51931868289999983, 1457.242090721130126, 228.6951897570979781 ) ) ;
#33652 = ORIENTED_EDGE ( 'NONE', *, *, #2147, .T. ) ;
#33653 = ORIENTED_EDGE ( 'NONE', *, *, #98518, .F. ) ;
#33654 = CARTESIAN_POINT ( 'NONE',  ( 1.121604517039999971, 1425.801401066219796, 191.0761181822990125 ) ) ;
#33655 = CARTESIAN_POINT ( 'NONE',  ( -9.400735546954820165, 1432.346475316169972, 153.1462981359680100 ) ) ;
#33656 = FACE_OUTER_BOUND ( 'NONE', #64054, .T. ) ;
#33657 = AXIS2_PLACEMENT_3D ( 'NONE', #94224, #69069, #42188 ) ;
#33658 = DIRECTION ( 'NONE',  ( -0.3363363969979655810, -0.9417419115949056119, 0.000000000000000000 ) ) ;
#33659 = EDGE_CURVE ( 'NONE', #74525, #17686, #96775, .T. ) ;
#33660 = CARTESIAN_POINT ( 'NONE',  ( 3.829620113550000315, 1515.551704408389924, 210.9648081929590262 ) ) ;
#33661 = CARTESIAN_POINT ( 'NONE',  ( -2.472529913803013013, 1523.678648413191695, 242.8674788698241684 ) ) ;
#33662 = CARTESIAN_POINT ( 'NONE',  ( -13.64528653743296793, 1409.389564293140211, 225.5043415784803926 ) ) ;
#33663 = CARTESIAN_POINT ( 'NONE',  ( 7.709487153813650018, 1516.551696783219995, 206.3620776923469862 ) ) ;
#33664 = ADVANCED_FACE ( 'NONE', ( #11445 ), #84289, .F. ) ;
#33665 = CARTESIAN_POINT ( 'NONE',  ( 9.218353480593270532, 1451.410954820720008, 210.0417286664930145 ) ) ;
#33666 =( BOUNDED_CURVE ( )  B_SPLINE_CURVE ( 3, ( #83790, #102238, #16010, #7627 ),
 .UNSPECIFIED., .F., .F. ) 
 B_SPLINE_CURVE_WITH_KNOTS ( ( 4, 4 ),
 ( 5.113530135711883418, 5.899158457943692646 ),
 .UNSPECIFIED. ) 
 CURVE ( )  GEOMETRIC_REPRESENTATION_ITEM ( )  RATIONAL_B_SPLINE_CURVE ( ( 1.000000000000000000, 0.9492236582716190307, 0.9492236582716190307, 1.000000000000000000 ) ) 
 REPRESENTATION_ITEM ( '' )  );
#33667 = CARTESIAN_POINT ( 'NONE',  ( 37.71876581398180406, 1442.773887286369245, 136.8568823567051709 ) ) ;
#33668 = CARTESIAN_POINT ( 'NONE',  ( -91.22062739730009184, 1384.843445976460089, 293.2615258250190209 ) ) ;
#33669 = ORIENTED_EDGE ( 'NONE', *, *, #22303, .T. ) ;
#33670 = CARTESIAN_POINT ( 'NONE',  ( -4.616861546545000472, 1516.666407245520077, 201.4093549791169835 ) ) ;
#33671 = CARTESIAN_POINT ( 'NONE',  ( -2.292217048824999992, 1516.941178807709775, 209.1350424789999920 ) ) ;
#33672 = ORIENTED_EDGE ( 'NONE', *, *, #94644, .T. ) ;
#33674 = EDGE_CURVE ( 'NONE', #73741, #55526, #7404, .T. ) ;
#33673 = CARTESIAN_POINT ( 'NONE',  ( 11.75441003104140059, 1426.806845251099958, 145.3811685653730024 ) ) ;
#33675 = CARTESIAN_POINT ( 'NONE',  ( 3.747594548549652682, 1511.538158271216844, 217.2371947740062978 ) ) ;
#33676 = VERTEX_POINT ( 'NONE', #97101 ) ;
#33677 = CARTESIAN_POINT ( 'NONE',  ( -13.53550618839999942, 1416.067629290630066, 221.7501982114980308 ) ) ;
#33678 = CARTESIAN_POINT ( 'NONE',  ( -12.73318793669440829, 1442.831169986190389, 164.6858276811441328 ) ) ;
#33679 = CARTESIAN_POINT ( 'NONE',  ( -7.472882595364333191, 1434.765136914032610, 213.3156276624751229 ) ) ;
#33680 = CARTESIAN_POINT ( 'NONE',  ( -6.351474700609002433, 1489.557796261735803, 218.0707846636206853 ) ) ;
#33681 = CARTESIAN_POINT ( 'NONE',  ( -13.53916864039999979, 1429.119334014829747, 222.2883575813980030 ) ) ;
#33682 = CARTESIAN_POINT ( 'NONE',  ( 14.44257447436980080, 1436.255103877649844, 149.9682557532709950 ) ) ;
#33683 = CARTESIAN_POINT ( 'NONE',  ( -9.864626116910001130, 1473.082391558989912, 206.3028941057989982 ) ) ;
#33684 = CARTESIAN_POINT ( 'NONE',  ( 5.389719913101400195, 1440.971386073809981, 154.8246291173960003 ) ) ;
#33685 = CARTESIAN_POINT ( 'NONE',  ( -62.09998818780000818, 1379.733235768160057, 266.3407746977590023 ) ) ;
#33686 = CARTESIAN_POINT ( 'NONE',  ( -15.37779627350000133, 1473.856793900130015, 223.6695348900979923 ) ) ;
#33687 = EDGE_CURVE ( 'NONE', #45131, #82569, #68260, .T. ) ;
#33689 = CARTESIAN_POINT ( 'NONE',  ( 3.383995498396490387, 1466.337167523709923, 198.5968663170720276 ) ) ;
#33688 = CARTESIAN_POINT ( 'NONE',  ( -5.387811863060000483, 1496.648312753189884, 199.2595355468089906 ) ) ;
#33690 = LINE ( 'NONE', #17985, #11172 ) ;
#33691 = CARTESIAN_POINT ( 'NONE',  ( -2.499950939289320218, 1420.110720408840052, 91.61080890135978905 ) ) ;
#33692 = VERTEX_POINT ( 'NONE', #29329 ) ;
#33693 = EDGE_CURVE ( 'NONE', #42748, #100324, #59301, .T. ) ;
#33694 = CARTESIAN_POINT ( 'NONE',  ( -1.266603054566116215, 1486.256723992427851, 181.7971939238652226 ) ) ;
#33695 = CARTESIAN_POINT ( 'NONE',  ( 2.086567662868722639, 1516.527846576654156, 216.8307085844099902 ) ) ;
#33696 = CARTESIAN_POINT ( 'NONE',  ( 2.877744946244999991, 1516.723920667490120, 213.7309102736070088 ) ) ;
#33697 = CARTESIAN_POINT ( 'NONE',  ( -2.995264515017130424, 1485.700673117452425, 182.6181475772214924 ) ) ;
#33698 = CARTESIAN_POINT ( 'NONE',  ( -14.68224860129999954, 1415.739699861750069, 213.1708190345090088 ) ) ;
#33700 = EDGE_LOOP ( 'NONE', ( #58897, #69510, #28145, #34633, #23095, #105008 ) ) ;
#33699 = CARTESIAN_POINT ( 'NONE',  ( -4.138543391158297169, 1515.492058413688255, 211.4519800883778373 ) ) ;
#33701 = CARTESIAN_POINT ( 'NONE',  ( 0.9093771269469999030, 1453.154616238429981, 188.6184110473980127 ) ) ;
#33702 = CARTESIAN_POINT ( 'NONE',  ( 0.7310778633389990455, 1508.461242302289975, 220.4858708957989961 ) ) ;
#33703 = CARTESIAN_POINT ( 'NONE',  ( -11.74266240329999889, 1430.299105537730156, 150.4823647192980047 ) ) ;
#33704 = LINE ( 'NONE', #104235, #55775 ) ;
#33705 = FACE_OUTER_BOUND ( 'NONE', #364, .T. ) ;
#33706 = EDGE_CURVE ( 'NONE', #61502, #10270, #4613, .T. ) ;
#33707 = CARTESIAN_POINT ( 'NONE',  ( -9.500116237244998985, 1517.051704408389924, 222.5297078019669925 ) ) ;
#33708 = CARTESIAN_POINT ( 'NONE',  ( 21.13734888319999783, 1496.938803861589804, 209.1218459616989946 ) ) ;
#33709 = EDGE_CURVE ( 'NONE', #20056, #28187, #85943, .T. ) ;
#33710 = PLANE ( 'NONE',  #81923 ) ;
#33712 = CARTESIAN_POINT ( 'NONE',  ( -10.48474031351270064, 1480.275052362939959, 208.2232303084710168 ) ) ;
#33711 = CARTESIAN_POINT ( 'NONE',  ( -26.30611563449999935, 1495.365312711930073, 211.9622044710779960 ) ) ;
#33713 = CARTESIAN_POINT ( 'NONE',  ( -19.53786426059057746, 1512.187213306747481, 180.5239794925695946 ) ) ;
#33714 = ORIENTED_EDGE ( 'NONE', *, *, #68020, .F. ) ;
#33716 = AXIS2_PLACEMENT_3D ( 'NONE', #41089, #75266, #13109 ) ;
#33715 = CARTESIAN_POINT ( 'NONE',  ( -2.879956963085000154, 1516.827328999679821, 205.8693153165069702 ) ) ;
#33717 = CARTESIAN_POINT ( 'NONE',  ( 35.90626991010000069, 1418.667692805230217, 268.5344559059980156 ) ) ;
#33718 = CARTESIAN_POINT ( 'NONE',  ( 7.454017752073605507, 1508.783371651613606, 214.6352815282469919 ) ) ;
#33719 = EDGE_CURVE ( 'NONE', #8175, #94093, #60590, .T. ) ;
#33720 = CARTESIAN_POINT ( 'NONE',  ( 24.93912320480000133, 1469.150327946329753, 204.6358346344680115 ) ) ;
#33721 = AXIS2_PLACEMENT_3D ( 'NONE', #26829, #72704, #21150 ) ;
#33722 = CARTESIAN_POINT ( 'NONE',  ( -0.02424329741014210129, 1507.629757353219702, 237.3744802823229918 ) ) ;
#33723 = CARTESIAN_POINT ( 'NONE',  ( 2.588318195730309856, 1454.459320507460006, 218.1543517672069754 ) ) ;
#33724 = CARTESIAN_POINT ( 'NONE',  ( -15.85591190879999779, 1415.880081504350073, 209.4912631162540038 ) ) ;
#33725 = CARTESIAN_POINT ( 'NONE',  ( -18.61729373446216584, 1457.059787195335730, 228.1786572006384972 ) ) ;
#33726 = CARTESIAN_POINT ( 'NONE',  ( -10.04630323299999972, 1461.008343231690105, 213.6807241916089879 ) ) ;
#33727 = CARTESIAN_POINT ( 'NONE',  ( -12.65996588039999970, 1445.259821888419992, 186.8996239715980039 ) ) ;
#33728 = CARTESIAN_POINT ( 'NONE',  ( -3.805396659119999914, 1495.647976226690162, 219.6495707272989932 ) ) ;
#33729 = CARTESIAN_POINT ( 'NONE',  ( -8.638504774626840188, 1437.522490713840170, 208.5429851243989958 ) ) ;
#33730 = CARTESIAN_POINT ( 'NONE',  ( 8.322172261349999545, 1408.217606231929949, 270.1222559176979416 ) ) ;
#33731 = CARTESIAN_POINT ( 'NONE',  ( 1.462200250809050139, 1493.817013747780038, 181.6932468947250072 ) ) ;
#33732 = CARTESIAN_POINT ( 'NONE',  ( 7.649034400464999273, 1514.243099272629934, 214.7715657207469917 ) ) ;
#33733 = CARTESIAN_POINT ( 'NONE',  ( -1.842962231260000028, 1515.064792882589927, 213.4512947377390049 ) ) ;
#33734 = CARTESIAN_POINT ( 'NONE',  ( -12.27691143406236840, 1378.140212871909853, 210.1884462337374089 ) ) ;
#33735 = CARTESIAN_POINT ( 'NONE',  ( -18.31336108710000232, 1473.001052085330002, 268.9136774873980471 ) ) ;
#33737 = AXIS2_PLACEMENT_3D ( 'NONE', #92746, #60269, #50752 ) ;
#33736 = LINE ( 'NONE', #34850, #80015 ) ;
#33738 = CARTESIAN_POINT ( 'NONE',  ( -20.99625264690000392, 1509.712722401030078, 187.9206951049980034 ) ) ;
#33739 = CARTESIAN_POINT ( 'NONE',  ( -24.36918344492354649, 1444.649591787489271, 211.1821244689920434 ) ) ;
#33740 = CARTESIAN_POINT ( 'NONE',  ( -53.77010317427249930, 1384.722329602369882, 269.3966670172729891 ) ) ;
#33741 = CARTESIAN_POINT ( 'NONE',  ( -10.89685441944650002, 1384.934403369409893, 200.0946264938700097 ) ) ;
#33742 = CARTESIAN_POINT ( 'NONE',  ( -9.587366264599999965, 1440.450814879359996, 153.1449006345979740 ) ) ;
#33743 = ADVANCED_FACE ( 'NONE', ( #48917 ), #98738, .F. ) ;
#33744 = CARTESIAN_POINT ( 'NONE',  ( -25.17882212385940122, 1457.411782445480185, 210.8729951149459794 ) ) ;
#33745 = CARTESIAN_POINT ( 'NONE',  ( -18.66420869458074705, 1526.382868172864164, 185.4599087859683095 ) ) ;
#33746 = CARTESIAN_POINT ( 'NONE',  ( -1.997114499468346294, 1519.551704408389924, 229.8748770085109072 ) ) ;
#33747 = CARTESIAN_POINT ( 'NONE',  ( -23.65074497499999850, 1410.660584268429830, 206.9527459116580133 ) ) ;
#33748 = CARTESIAN_POINT ( 'NONE',  ( -11.62722270852152207, 1378.375229821887842, 205.0204712162364160 ) ) ;
#33749 = B_SPLINE_CURVE_WITH_KNOTS ( 'NONE', 3,
 ( #27822, #69850, #53038, #53599, #17724, #105080, #96121 ),
 .UNSPECIFIED., .F., .F.,
 ( 4, 3, 4 ),
 ( -157.7844419379999863, -101.5362237811699941, -30.93609007946849943 ),
 .UNSPECIFIED. ) ;
#33750 = CARTESIAN_POINT ( 'NONE',  ( 4.825596943430000785, 1484.194153470290075, 219.9364766577990054 ) ) ;
#33751 = CARTESIAN_POINT ( 'NONE',  ( -31.11217220549999851, 1415.581976973229757, 269.3348318802979975 ) ) ;
#33752 = PLANE ( 'NONE',  #37396 ) ;
#33753 = CARTESIAN_POINT ( 'NONE',  ( -19.04698835603899809, 1444.155774679960132, 199.5979800297200200 ) ) ;
#33754 = CARTESIAN_POINT ( 'NONE',  ( -3.829619994797929916, 1515.551704292389786, 210.9648097401420159 ) ) ;
#33755 = LINE ( 'NONE', #102061, #105421 ) ;
#33757 = CARTESIAN_POINT ( 'NONE',  ( 13.89764133033322580, 1452.801221801048314, 223.6909718731195085 ) ) ;
#33756 = CARTESIAN_POINT ( 'NONE',  ( -22.15124423910000218, 1409.851346931930038, 211.3136525823379941 ) ) ;
#33758 = CARTESIAN_POINT ( 'NONE',  ( 11.72168562826050042, 1426.705748779369969, 143.0708505248780114 ) ) ;
#33759 = LINE ( 'NONE', #61766, #9293 ) ;
#33760 = CARTESIAN_POINT ( 'NONE',  ( -7.722580350941189664, 1517.051704403100075, 204.5317855550379988 ) ) ;
#33761 = CARTESIAN_POINT ( 'NONE',  ( 4.616666844463280128, 1447.066147660239949, 200.0483904391570036 ) ) ;
#33762 = CARTESIAN_POINT ( 'NONE',  ( -11.36018337610000195, 1414.996442546130083, 195.9645814914979951 ) ) ;
#33763 = ADVANCED_FACE ( 'NONE', ( #48358 ), #100037, .T. ) ;
#33764 = CARTESIAN_POINT ( 'NONE',  ( 2.869693458934999608, 1517.070197312179971, 203.3343689375869872 ) ) ;
#33765 = CARTESIAN_POINT ( 'NONE',  ( -8.742206007015797198, 1511.494976269418885, 214.8332494757211464 ) ) ;
#33766 = B_SPLINE_CURVE_WITH_KNOTS ( 'NONE', 3,
 ( #23236, #57434, #91560, #89352, #46824, #50661, #68038, #6996, #41154, #59079, #75863, #51211, #84253, #93199, #75329, #66929 ),
 .UNSPECIFIED., .F., .F.,
 ( 4, 3, 3, 3, 3, 4 ),
 ( -6.921060107978769693, -6.805780737513280165, -5.885806138044639368, -4.993439783500069673, -4.118990261660390395, -3.271583732334530037 ),
 .UNSPECIFIED. ) ;
#33767 = CARTESIAN_POINT ( 'NONE',  ( -30.61611611309821157, 1526.069472839380751, 201.6871119896482867 ) ) ;
#33768 = CARTESIAN_POINT ( 'NONE',  ( 15.90990501073499885, 1514.921193539169963, 193.9190473980669935 ) ) ;
#33769 = FACE_BOUND ( 'NONE', #94302, .T. ) ;
#33770 = CARTESIAN_POINT ( 'NONE',  ( 2.716629276539999971, 1509.007927172130167, 238.2585658352980147 ) ) ;
#33771 = CARTESIAN_POINT ( 'NONE',  ( 20.00300088520139852, 1507.847439178179911, 229.0979933904550023 ) ) ;
#33772 = AXIS2_PLACEMENT_3D ( 'NONE', #96980, #93764, #102716 ) ;
#33774 = VERTEX_POINT ( 'NONE', #71242 ) ;
#33773 = CARTESIAN_POINT ( 'NONE',  ( -40.76586742162339760, 1379.696137550030016, 229.2042884337240025 ) ) ;
#33775 = EDGE_LOOP ( 'NONE', ( #74056, #26478, #108291, #70463, #16830 ) ) ;
#33776 = CARTESIAN_POINT ( 'NONE',  ( 12.02944668659279870, 1433.769975373530087, 150.0279833908939793 ) ) ;
#33777 = CARTESIAN_POINT ( 'NONE',  ( -7.331557526720001050, 1396.349310000530068, 219.0774438792280137 ) ) ;
#33778 = EDGE_LOOP ( 'NONE', ( #71547, #37546, #50488, #16699, #9439, #30339 ) ) ;
#33779 = CARTESIAN_POINT ( 'NONE',  ( -106.3768849420000038, 1379.360965665230196, 307.8405492843589855 ) ) ;
#33780 = CARTESIAN_POINT ( 'NONE',  ( -109.8254558940000010, 1384.920634213669928, 311.3807750492590003 ) ) ;
#33781 = CARTESIAN_POINT ( 'NONE',  ( 3.644351594699349661, 1515.551704204689941, 205.8497219879369879 ) ) ;
#33783 = CARTESIAN_POINT ( 'NONE',  ( -14.28944875984979923, 1509.439638412510021, 183.0899159983670188 ) ) ;
#33782 = CARTESIAN_POINT ( 'NONE',  ( 3.909710721586129534, 1522.051704408389924, 220.4764703678949900 ) ) ;
#33784 = CARTESIAN_POINT ( 'NONE',  ( 15.61733546277139872, 1498.109274936660086, 231.4603964206870330 ) ) ;
#33785 = VECTOR ( 'NONE', #59283, 1000.000000000000000 ) ;
#33786 = EDGE_CURVE ( 'NONE', #52697, #90692, #56399, .T. ) ;
#33787 = CARTESIAN_POINT ( 'NONE',  ( 2.585682588340000088, 1449.237988204799876, 183.8872507908980083 ) ) ;
#33788 = DIRECTION ( 'NONE',  ( 1.139346649588226023E-16, 0.3666799630584695047, -0.9303471420343265574 ) ) ;
#33789 = CARTESIAN_POINT ( 'NONE',  ( 5.371346801045000063, 1516.551704408390151, 199.4837300725270097 ) ) ;
#33790 = B_SPLINE_SURFACE_WITH_KNOTS ( 'NONE', 5, 5, ( 
 ( #106548, #4643, #29836, #40435, #47748, #89196 ),
 ( #89743, #56145, #64022, #22501, #107650, #106012 ),
 ( #98135, #65661, #14682, #14123, #65111, #13016 ),
 ( #12488, #47202, #38781, #107094, #56702, #30383 ),
 ( #64574, #108190, #21952, #90281, #48870, #82996 ),
 ( #81883, #5186, #90838, #48312, #82454, #39893 ) ),
 .UNSPECIFIED., .F., .F., .F.,
 ( 6, 6 ),
 ( 6, 6 ),
 ( 3.723869972580000187, 4.458425423349980043 ),
 ( 0.000000000000000000, 2.000000000000000000 ),
 .UNSPECIFIED. ) ;
#33791 = CARTESIAN_POINT ( 'NONE',  ( 4.073985546776730082, 1396.055327098900079, 198.8729011744260049 ) ) ;
#33792 = CARTESIAN_POINT ( 'NONE',  ( 1.362314668290000030, 1416.021639799829927, 190.3543332225980009 ) ) ;
#33793 = CARTESIAN_POINT ( 'NONE',  ( 10.96595508919999951, 1432.092997362309916, 151.7666336219979826 ) ) ;
#33794 = CARTESIAN_POINT ( 'NONE',  ( 7.179127081225000317, 1513.978875661340226, 201.3127820188869919 ) ) ;
#33795 = VERTEX_POINT ( 'NONE', #3475 ) ;
#33796 = CARTESIAN_POINT ( 'NONE',  ( 13.45603295267449973, 1435.141892408729973, 149.7441957230019796 ) ) ;
#33797 = ADVANCED_FACE ( 'NONE', ( #84422 ), #43202, .T. ) ;
#33798 = ORIENTED_EDGE ( 'NONE', *, *, #47269, .F. ) ;
#33799 = VERTEX_POINT ( 'NONE', #13470 ) ;
#33800 = CARTESIAN_POINT ( 'NONE',  ( 13.11924748619371783, 1444.785942371835063, 169.4030629633686829 ) ) ;
#33801 = CARTESIAN_POINT ( 'NONE',  ( -12.69622108839999974, 1461.420101681630058, 231.9855631372980156 ) ) ;
#33802 = CARTESIAN_POINT ( 'NONE',  ( -13.31488284758549945, 1407.448340439549838, 207.9555150571470108 ) ) ;
#33803 = CARTESIAN_POINT ( 'NONE',  ( -2.872208748294999836, 1517.145312756229941, 216.4596396827270155 ) ) ;
#33804 = CARTESIAN_POINT ( 'NONE',  ( -8.280691316095005305, 1511.427926070383592, 213.3861107695062458 ) ) ;
#33805 = B_SPLINE_SURFACE_WITH_KNOTS ( 'NONE', 5, 5, ( 
 ( #478, #34602, #60373, #94496, #17767, #51971 ),
 ( #5128, #39284, #73459, #69338, #1031, #27308 ),
 ( #28978, #88328, #44683, #61489, #104012, #96173 ),
 ( #95618, #103446, #78828, #2140, #35154, #26752 ),
 ( #97267, #60940, #19448, #87221, #20543, #79379 ),
 ( #28421, #87790, #18885, #2695, #18336, #86112 ) ),
 .UNSPECIFIED., .F., .F., .F.,
 ( 6, 6 ),
 ( 6, 6 ),
 ( 8.897216823040000833, 11.87860904800000128 ),
 ( 0.000000000000000000, 1.460858415939999988 ),
 .UNSPECIFIED. ) ;
#33806 = AXIS2_PLACEMENT_3D ( 'NONE', #78316, #18941, #532 ) ;
#33807 = CARTESIAN_POINT ( 'NONE',  ( 12.33374228401319961, 1421.685547970650077, 207.8899185667679888 ) ) ;
#33808 = DIRECTION ( 'NONE',  ( 0.9417419115949662300, -0.2378257470769920556, 0.2378257470769920556 ) ) ;
#33809 = CARTESIAN_POINT ( 'NONE',  ( -26.01089419480000231, 1380.250345454860053, 212.5061481324489705 ) ) ;
#33810 = VERTEX_POINT ( 'NONE', #109088 ) ;
#33811 = CARTESIAN_POINT ( 'NONE',  ( 2.476733476015000157, 1516.858326417339867, 206.6281461634669938 ) ) ;
#33812 = ORIENTED_EDGE ( 'NONE', *, *, #75677, .T. ) ;
#33813 = CARTESIAN_POINT ( 'NONE',  ( 20.69345393905350150, 1440.913060387330006, 220.6334537215260241 ) ) ;
#33814 = CARTESIAN_POINT ( 'NONE',  ( -19.28053373810000082, 1508.539880042930236, 229.7797826120979892 ) ) ;
#33815 = ADVANCED_FACE ( 'NONE', ( #81788 ), #15097, .T. ) ;
#33816 = CARTESIAN_POINT ( 'NONE',  ( -7.164186635890001043, 1409.330595797830028, 188.0408233170979884 ) ) ;
#33817 = B_SPLINE_CURVE_WITH_KNOTS ( 'NONE', 5,
 ( #20273, #1862, #46066, #89145, #2969, #19731 ),
 .UNSPECIFIED., .F., .F.,
 ( 6, 6 ),
 ( 0.000000000000000000, 1.000000000000000000 ),
 .UNSPECIFIED. ) ;
#33818 = CARTESIAN_POINT ( 'NONE',  ( 7.266995407845000088, 1512.686126173240154, 215.9029788489869759 ) ) ;
#33819 = ADVANCED_FACE ( 'NONE', ( #94455 ), #58063, .F. ) ;
#33821 = EDGE_LOOP ( 'NONE', ( #32913, #6803, #71895, #109249 ) ) ;
#33820 = CARTESIAN_POINT ( 'NONE',  ( -0.3106767230313050021, 1415.088506334920112, 226.1862806902549892 ) ) ;
#33822 = CARTESIAN_POINT ( 'NONE',  ( 24.54570628209999938, 1439.590004835240052, 212.8530392935280133 ) ) ;
#33823 = CARTESIAN_POINT ( 'NONE',  ( -113.4000000000000057, 1305.714868215269917, 304.2218459572590064 ) ) ;
#33824 = CARTESIAN_POINT ( 'NONE',  ( -3.829620113550000315, 1515.551704408389924, 207.2788837304390199 ) ) ;
#33825 = DIRECTION ( 'NONE',  ( 3.828568698926946970E-16, 0.000000000000000000, -1.000000000000000000 ) ) ;
#33826 = ADVANCED_FACE ( 'NONE', ( #25597 ), #50941, .F. ) ;
#33827 = CARTESIAN_POINT ( 'NONE',  ( 21.86721050905282482, 1523.611961620354123, 183.2036325349477579 ) ) ;
#33828 = AXIS2_PLACEMENT_3D ( 'NONE', #20339, #53425, #78048 ) ;
#33829 = B_SPLINE_SURFACE_WITH_KNOTS ( 'NONE', 5, 5, ( 
 ( #60245, #27188, #35577, #69770, #95490, #94363 ),
 ( #19872, #51846, #103888, #18758, #78694, #36145 ),
 ( #35024, #69203, #103312, #70329, #27733, #61923 ),
 ( #21511, #107197, #37246, #106637, #45673, #46770 ),
 ( #64119, #97148, #46219, #28847, #81980, #72508 ),
 ( #80353, #55170, #5289, #54622, #20416, #73056 ),
 ( #90379, #89841, #13114, #54077, #98240, #106099 ),
 ( #22053, #37797, #107749, #55723, #98792, #30485 ),
 ( #29927, #99327, #47297, #47847, #31033, #64674 ),
 ( #79811, #39446, #88754, #11498, #81421, #65215 ),
 ( #73620, #56250, #12037, #38329, #80900, #20966 ),
 ( #88203, #3670, #71986, #13657, #29377, #3117 ) ),
 .UNSPECIFIED., .F., .F., .F.,
 ( 6, 3, 3, 6 ),
 ( 6, 6 ),
 ( -1.028409222517709891E-05, 6.405353355340000832, 10.57568960840000116, 14.18574420394130087 ),
 ( -1.028409222599429936E-05, 1.510873114410000051 ),
 .UNSPECIFIED. ) ;
#33830 = CARTESIAN_POINT ( 'NONE',  ( -7.325541825264999751, 1516.710692850270107, 214.1269169785269924 ) ) ;
#33831 = EDGE_CURVE ( 'NONE', #79801, #13899, #49059, .T. ) ;
#33832 = CARTESIAN_POINT ( 'NONE',  ( -3.253889150190400148, 1428.778859686050055, 200.3401300163330063 ) ) ;
#33833 = CARTESIAN_POINT ( 'NONE',  ( -21.33073281829999956, 1509.431426448229786, 190.3502236029979997 ) ) ;
#33834 = LINE ( 'NONE', #15368, #33275 ) ;
#33835 = CARTESIAN_POINT ( 'NONE',  ( 5.788097227154999302, 1517.099836525840146, 211.6039138304569747 ) ) ;
#33836 = CARTESIAN_POINT ( 'NONE',  ( 42.15865170690000241, 1431.016965136909903, 271.1218459616979999 ) ) ;
#33837 = CARTESIAN_POINT ( 'NONE',  ( -11.86441352026110074, 1482.079730296919934, 208.3752912375910284 ) ) ;
#33838 = CARTESIAN_POINT ( 'NONE',  ( 20.81306254364009689, 1578.884139734249857, 255.0940092270310231 ) ) ;
#33840 = VERTEX_POINT ( 'NONE', #81518 ) ;
#33839 = CARTESIAN_POINT ( 'NONE',  ( -54.22998853240000017, 1386.694956673949946, 270.3205869870589595 ) ) ;
#33841 = CARTESIAN_POINT ( 'NONE',  ( -57.27474470154499642, 1385.080142571920078, 276.1243206708509774 ) ) ;
#33842 = CARTESIAN_POINT ( 'NONE',  ( 19.16281588599999708, 1470.534656580030060, 262.3397497982979871 ) ) ;
#33843 = CARTESIAN_POINT ( 'NONE',  ( -28.63327877612760020, 1509.912956515240012, 215.5831518558169932 ) ) ;
#33844 = CARTESIAN_POINT ( 'NONE',  ( -4.045189757455589508, 1509.066000099900066, 238.3989657214699776 ) ) ;
#33845 = ADVANCED_FACE ( 'NONE', ( #73714 ), #107838, .F. ) ;
#33846 = CARTESIAN_POINT ( 'NONE',  ( 12.45662329989999861, 1427.088120873819889, 206.6493142630589830 ) ) ;
#33847 = CARTESIAN_POINT ( 'NONE',  ( -31.92108011125334954, 1511.187213306747708, 220.9591791661900686 ) ) ;
#33849 = CARTESIAN_POINT ( 'NONE',  ( 17.98629411888249763, 1410.716562210689972, 222.9725041732099839 ) ) ;
#33848 = CARTESIAN_POINT ( 'NONE',  ( -1.906499580428539872E-08, 1509.038615934239942, 216.6345961781970288 ) ) ;
#33850 = DIRECTION ( 'NONE',  ( -1.000000000000000000, 0.000000000000000000, 0.000000000000000000 ) ) ;
#33851 = CARTESIAN_POINT ( 'NONE',  ( -1.550613577669627485, 1515.551704304084296, 205.2291798131859935 ) ) ;
#33852 = VERTEX_POINT ( 'NONE', #47941 ) ;
#33853 = CARTESIAN_POINT ( 'NONE',  ( -3.456007423304999993, 1516.647534046129977, 202.5739645571870255 ) ) ;
#33854 = CARTESIAN_POINT ( 'NONE',  ( -8.654560031179620694, 1508.432825899400086, 219.2516281120300050 ) ) ;
#33855 = EDGE_CURVE ( 'NONE', #67278, #102730, #61866, .T. ) ;
#33856 = CARTESIAN_POINT ( 'NONE',  ( 4.987078416198220232, 1508.551704408389924, 211.6097810847190033 ) ) ;
#33857 = CARTESIAN_POINT ( 'NONE',  ( 12.27023112350000211, 1416.839692139429872, 223.5796784320980066 ) ) ;
#33858 = CARTESIAN_POINT ( 'NONE',  ( 10.94310694154670038, 1460.970394390260026, 208.7352916610030320 ) ) ;
#33859 = CARTESIAN_POINT ( 'NONE',  ( -13.31089767776890120, 1503.456584347970193, 208.6977459380580058 ) ) ;
#33860 = CARTESIAN_POINT ( 'NONE',  ( 3.869834123409999993, 1466.682401882589829, 218.6841892407390162 ) ) ;
#33861 = CARTESIAN_POINT ( 'NONE',  ( 8.510016363196779565, 1417.253316583138258, 230.6448116059823121 ) ) ;
#33862 = CARTESIAN_POINT ( 'NONE',  ( 32.66530384042000179, 1436.114947058330017, 136.3376366257210179 ) ) ;
#33863 = AXIS2_PLACEMENT_3D ( 'NONE', #30459, #3092, #64643 ) ;
#33864 = CARTESIAN_POINT ( 'NONE',  ( -42.02418941567508881, 1454.249290662224666, 269.0750561195100090 ) ) ;
#33865 = CARTESIAN_POINT ( 'NONE',  ( -108.9467996200000073, 1386.017383885020081, 297.2678332311589884 ) ) ;
#33866 = FACE_OUTER_BOUND ( 'NONE', #79953, .T. ) ;
#33867 = CARTESIAN_POINT ( 'NONE',  ( -21.30909630337585270, 1524.964158026965606, 184.3255832943751784 ) ) ;
#33868 = CARTESIAN_POINT ( 'NONE',  ( -9.105545352350659982, 1449.059046520889979, 210.1350150939630055 ) ) ;
#33870 = ORIENTED_EDGE ( 'NONE', *, *, #71271, .T. ) ;
#33869 = B_SPLINE_CURVE_WITH_KNOTS ( 'NONE', 5,
 ( #26222, #52561, #7774, #9437, #102383, #27337, #25665, #69373, #43052 ),
 .UNSPECIFIED., .F., .F.,
 ( 6, 3, 6 ),
 ( 0.000000000000000000, 0.4999964781214675247, 1.000000000000000000 ),
 .UNSPECIFIED. ) ;
#33871 = CARTESIAN_POINT ( 'NONE',  ( -32.78250617288048829, 1511.187213306747708, 199.9357095655695389 ) ) ;
#33872 = DIRECTION ( 'NONE',  ( -1.000000000000000000, 0.000000000000000000, 0.000000000000000000 ) ) ;
#33873 = CARTESIAN_POINT ( 'NONE',  ( -4.554954843304989787, 1508.731366866819826, 212.6094325583730154 ) ) ;
#33874 = CARTESIAN_POINT ( 'NONE',  ( 14.30089278887709980, 1424.546528003230151, 190.6949013431569995 ) ) ;
#33875 = CARTESIAN_POINT ( 'NONE',  ( 10.86613173150421296, 1424.804654287561107, 138.2012213579507147 ) ) ;
#33877 = CARTESIAN_POINT ( 'NONE',  ( -4.623067421070000016, 1470.601194648889987, 189.6761541078989808 ) ) ;
#33876 = CARTESIAN_POINT ( 'NONE',  ( 12.26398290010000025, 1500.757830321889969, 209.2458525896959998 ) ) ;
#33878 = CARTESIAN_POINT ( 'NONE',  ( -29.78452513100000232, 1510.001069743030257, 209.1046444409799960 ) ) ;
#33879 = CARTESIAN_POINT ( 'NONE',  ( 7.565836366640000143, 1425.419877822159833, 211.6547584071689982 ) ) ;
#33880 = CARTESIAN_POINT ( 'NONE',  ( 16.64685983873516761, 1523.847233649538339, 180.5000230624021640 ) ) ;
#33881 = CARTESIAN_POINT ( 'NONE',  ( 44.43455570398290178, 1440.913041958179974, 270.0922447040700263 ) ) ;
#33882 = CARTESIAN_POINT ( 'NONE',  ( -16.06427069504690053, 1414.913060387399810, 209.3174525065670082 ) ) ;
#33883 = CARTESIAN_POINT ( 'NONE',  ( 25.88156921539999900, 1436.664060738580019, 136.9978706268979920 ) ) ;
#33884 = CARTESIAN_POINT ( 'NONE',  ( -7.489155007101369499, 1396.174587443169912, 200.9962419971890313 ) ) ;
#33885 = VERTEX_POINT ( 'NONE', #24371 ) ;
#33886 = DIRECTION ( 'NONE',  ( -1.755985294532469921E-16, 1.000000000000000000, -1.338183447452831989E-16 ) ) ;
#33887 = CARTESIAN_POINT ( 'NONE',  ( 21.53951928259277082, 1509.203566000515593, 226.5093279692427188 ) ) ;
#33888 = ORIENTED_EDGE ( 'NONE', *, *, #102706, .T. ) ;
#33889 = VERTEX_POINT ( 'NONE', #30582 ) ;
#33890 = CARTESIAN_POINT ( 'NONE',  ( -5.311724842150000292, 1500.891271500089942, 229.7588813323989996 ) ) ;
#33891 = CARTESIAN_POINT ( 'NONE',  ( -15.49932866405858789, 1415.988126884580197, 207.5283249126204907 ) ) ;
#33893 = CARTESIAN_POINT ( 'NONE',  ( -27.31923407390000236, 1446.350545702490081, 231.7128707201979978 ) ) ;
#33892 = CARTESIAN_POINT ( 'NONE',  ( 11.03772332119999966, 1426.504772946829917, 93.46069203369791012 ) ) ;
#33894 = CARTESIAN_POINT ( 'NONE',  ( -8.557208171940001051, 1448.617778667089851, 212.3361775886790213 ) ) ;
#33895 = CARTESIAN_POINT ( 'NONE',  ( 4.161911742251380275, 1424.201536654089978, 184.5072953679090233 ) ) ;
#33896 = CARTESIAN_POINT ( 'NONE',  ( -12.29913530678689959, 1378.337136344450073, 209.9620885240399843 ) ) ;
#33897 = VECTOR ( 'NONE', #65311, 1000.000000000000114 ) ;
#33898 = CARTESIAN_POINT ( 'NONE',  ( -2.807571324851497963, 1419.859960676956007, 186.1401237969660656 ) ) ;
#33899 = CARTESIAN_POINT ( 'NONE',  ( -0.5770119038902407071, 1525.581535527370761, 243.3912443123663820 ) ) ;
#33900 = CARTESIAN_POINT ( 'NONE',  ( -24.28401183249999917, 1438.913208742730149, 212.0820208524479824 ) ) ;
#33901 = DIRECTION ( 'NONE',  ( -0.9243714516270737924, -0.3790700632520799807, -0.04293374620179828127 ) ) ;
#33902 = CARTESIAN_POINT ( 'NONE',  ( 1.860632309006911456, 1494.734257013992419, 220.1210481096561580 ) ) ;
#33903 = CARTESIAN_POINT ( 'NONE',  ( 7.697803989957441750, 1363.443082852748375, 210.6218459617142003 ) ) ;
#33904 = CARTESIAN_POINT ( 'NONE',  ( -28.64971979848531802, 1510.024744496989797, 218.0290981197058215 ) ) ;
#33906 = ORIENTED_EDGE ( 'NONE', *, *, #60370, .F. ) ;
#33905 = CARTESIAN_POINT ( 'NONE',  ( 2.236830499208590339, 1495.676457082710158, 221.2569898128769807 ) ) ;
#33907 = ORIENTED_EDGE ( 'NONE', *, *, #46120, .T. ) ;
#33908 = CARTESIAN_POINT ( 'NONE',  ( -11.82581238847500060, 1429.643984554019880, 149.2867293954069794 ) ) ;
#33910 = CARTESIAN_POINT ( 'NONE',  ( 8.881784196999999612E-15, 1434.913060387330006, 126.8032249175980155 ) ) ;
#33909 = B_SPLINE_CURVE_WITH_KNOTS ( 'NONE', 3,
 ( #31674, #41190, #66416, #75361 ),
 .UNSPECIFIED., .F., .F.,
 ( 4, 4 ),
 ( 0.000000000000000000, 0.0002220129587134778018 ),
 .UNSPECIFIED. ) ;
#33911 = CARTESIAN_POINT ( 'NONE',  ( -0.4742355963789999795, 1472.045055685530087, 270.0713874948980333 ) ) ;
#33912 = DIRECTION ( 'NONE',  ( 0.06309892600015151731, -0.9660070198143602127, -0.2506969549216855886 ) ) ;
#33913 = CARTESIAN_POINT ( 'NONE',  ( -122.7187414971600390, 1311.832804576490389, 313.5405874544188691 ) ) ;
#33914 = AXIS2_PLACEMENT_3D ( 'NONE', #73016, #30446, #79347 ) ;
#33915 = FACE_OUTER_BOUND ( 'NONE', #40458, .T. ) ;
#33916 = CARTESIAN_POINT ( 'NONE',  ( 2.326513286163319538, 1476.258183507229887, 197.8633931498989966 ) ) ;
#33917 =( LENGTH_UNIT ( ) NAMED_UNIT ( * ) SI_UNIT ( .MILLI., .METRE. ) );
#33918 = CARTESIAN_POINT ( 'NONE',  ( -23.56404405089999798, 1519.913060387329779, 208.1422009162390054 ) ) ;
#33919 = CARTESIAN_POINT ( 'NONE',  ( 4.720156707528646578, 1369.933505578754648, 207.6218459616987673 ) ) ;
#33920 = CARTESIAN_POINT ( 'NONE',  ( -9.244740828173918956, 1448.612708514039923, 209.9868122805330017 ) ) ;
#33921 = CARTESIAN_POINT ( 'NONE',  ( -23.91557117702000212, 1411.440207489660224, 269.2971849165700178 ) ) ;
#33922 = CARTESIAN_POINT ( 'NONE',  ( -13.66262475276990074, 1434.970346796020067, 148.6600349200319897 ) ) ;
#33923 = ORIENTED_EDGE ( 'NONE', *, *, #6332, .F. ) ;
#33924 = CARTESIAN_POINT ( 'NONE',  ( 2.356894939219843721, 1525.394081235439444, 241.9297540029686786 ) ) ;
#33925 = CARTESIAN_POINT ( 'NONE',  ( 13.50156143719999946, 1443.545633684710083, 188.4056194818979861 ) ) ;
#33926 = B_SPLINE_SURFACE_WITH_KNOTS ( 'NONE', 5, 1, ( 
 ( #11974, #45051 ),
 ( #45603, #46155 ),
 ( #37178, #2501 ),
 ( #98724, #36622 ),
 ( #63517, #64605 ),
 ( #54559, #105486 ),
 ( #104932, #96534 ),
 ( #28219, #97633 ),
 ( #80285, #107126 ),
 ( #20354, #64052 ),
 ( #30418, #98171 ),
 ( #62406, #21985 ),
 ( #106579, #47233 ),
 ( #19808, #54014 ),
 ( #21442, #81360 ),
 ( #80831, #88144 ),
 ( #55652, #71928 ),
 ( #79745, #3052 ),
 ( #4674, #89775 ),
 ( #20901, #71374 ),
 ( #28777, #38812 ) ),
 .UNSPECIFIED., .F., .F., .F.,
 ( 6, 3, 3, 3, 3, 3, 6 ),
 ( 2, 2 ),
 ( 122.5058924469999937, 122.5666549750000058, 128.3589772969999956, 134.1528038509999874, 139.9378092970000012, 146.0761118390000206, 146.2671766279999872 ),
 ( 0.000000000000000000, 4.092150885356249823 ),
 .UNSPECIFIED. ) ;
#33927 = VERTEX_POINT ( 'NONE', #91030 ) ;
#33928 = EDGE_LOOP ( 'NONE', ( #56587, #38847, #83555, #72605, #57626, #41742, #46894, #49633 ) ) ;
#33929 = DIRECTION ( 'NONE',  ( 0.3090169943749582204, -0.000000000000000000, 0.9510565162951500895 ) ) ;
#33930 = CARTESIAN_POINT ( 'NONE',  ( -18.83642247210000065, 1444.248298674089938, 209.1218459616989946 ) ) ;
#33931 = CARTESIAN_POINT ( 'NONE',  ( -7.323974644434999348, 1516.647924054489977, 213.1579656147470132 ) ) ;
#33932 = CARTESIAN_POINT ( 'NONE',  ( -4.702036906180000031, 1485.478603201629994, 183.4821513001980122 ) ) ;
#33933 = DIRECTION ( 'NONE',  ( -1.000000000000000000, 0.000000000000000000, 0.000000000000000000 ) ) ;
#33934 = B_SPLINE_SURFACE_WITH_KNOTS ( 'NONE', 5, 5, ( 
 ( #18551, #25847, #104238, #61712, #7963, #93605 ),
 ( #42130, #60049, #43240, #20757, #88549, #46556 ),
 ( #71785, #87445, #105904, #79060, #28633, #29183 ),
 ( #104790, #2364, #65419, #71220, #79605, #105344 ),
 ( #11295, #62838, #63374, #97490, #89083, #4002 ),
 ( #54956, #62264, #31785, #2909, #65976, #96951 ),
 ( #31236, #48615, #53304, #45463, #99526, #19101 ),
 ( #37027, #28076, #12370, #10740, #88012, #36478 ),
 ( #38128, #22811, #80692, #20217, #54416, #11833 ),
 ( #57018, #46004, #70676, #80135, #72309, #96393 ),
 ( #19669, #106441, #91143, #3454, #37582, #44913 ),
 ( #14420, #82747, #6039, #40191, #53874, #74373 ) ),
 .UNSPECIFIED., .F., .F., .F.,
 ( 6, 3, 3, 6 ),
 ( 6, 6 ),
 ( -1.511236047250149958E-08, 21.98079552259999758, 65.92107459599999686, 113.3791245040000035 ),
 ( -2.177276631571330257E-05, 0.4689188558010000119 ),
 .UNSPECIFIED. ) ;
#33935 = ORIENTED_EDGE ( 'NONE', *, *, #34595, .T. ) ;
#33936 = CYLINDRICAL_SURFACE ( 'NONE', #56411, 2.000000000000003109 ) ;
#33937 = CARTESIAN_POINT ( 'NONE',  ( 2.482067860225000366, 1517.099836525840146, 203.3337487049469985 ) ) ;
#33938 = EDGE_CURVE ( 'NONE', #68673, #106239, #41378, .T. ) ;
#33939 = AXIS2_PLACEMENT_3D ( 'NONE', #33789, #57919, #42208 ) ;
#33940 = B_SPLINE_CURVE_WITH_KNOTS ( 'NONE', 3,
 ( #79987, #106825, #72700, #105754, #81078, #65409, #90577, #37437, #22247, #55906, #89485, #57005, #54799, #12217, #12780, #4395, #3859, #11677, #21701, #99515, #45854, #29039, #97330, #13857, #63224, #73806, #22800, #30114, #38522, #80544, #20600, #106286, #98429, #46412, #29571, #90024, #39062 ),
 .UNSPECIFIED., .F., .F.,
 ( 4, 3, 3, 3, 3, 3, 3, 3, 3, 3, 3, 3, 4 ),
 ( -67.60074812010000755, -65.74721505525899090, -64.06766111199499392, -62.52389936639999490, -62.11498414264809753, -60.91890502392639917, -59.67710013614709652, -58.39611896704169425, -57.02019216725560113, -55.62461436954049532, -54.01815956887700310, -52.05859542260679973, -50.07766623440000586 ),
 .UNSPECIFIED. ) ;
#33941 = CARTESIAN_POINT ( 'NONE',  ( -28.99152844629999848, 1509.869562750330033, 206.5812832654980014 ) ) ;
#33942 = ADVANCED_FACE ( 'NONE', ( #58006 ), #32239, .F. ) ;
#33943 = B_SPLINE_SURFACE_WITH_KNOTS ( 'NONE', 5, 1, ( 
 ( #23529, #39797 ),
 ( #29733, #73956 ),
 ( #99673, #91294 ),
 ( #22965, #57172 ),
 ( #82891, #6182 ),
 ( #40335, #74516 ) ),
 .UNSPECIFIED., .F., .F., .F.,
 ( 6, 6 ),
 ( 2, 2 ),
 ( 0.000000000000000000, 3.835535759499999919 ),
 ( 0.000000000000000000, 14.00000000000000000 ),
 .UNSPECIFIED. ) ;
#33944 = DIRECTION ( 'NONE',  ( -1.000000000000000000, 0.000000000000000000, 0.000000000000000000 ) ) ;
#33945 = CARTESIAN_POINT ( 'NONE',  ( -31.12598708176519935, 1384.558886231360020, 206.2155377277939863 ) ) ;
#33946 = CARTESIAN_POINT ( 'NONE',  ( -3.872760563090000385, 1407.067887183629864, 196.6093298303979964 ) ) ;
#33947 = CARTESIAN_POINT ( 'NONE',  ( -7.098163004017622235, 1512.239113741280107, 216.2722064511740996 ) ) ;
#33948 = AXIS2_PLACEMENT_3D ( 'NONE', #11505, #55177, #64126 ) ;
#33950 = ORIENTED_EDGE ( 'NONE', *, *, #94120, .F. ) ;
#33949 = CARTESIAN_POINT ( 'NONE',  ( -11.02428140918887145, 1512.359593911811089, 193.2458125109432672 ) ) ;
#33951 = CARTESIAN_POINT ( 'NONE',  ( -27.12610615285149862, 1488.751143559889897, 210.2942340960309764 ) ) ;
#33952 = CARTESIAN_POINT ( 'NONE',  ( 26.79586899809999778, 1488.686659793930176, 212.4508664459980025 ) ) ;
#33953 = CARTESIAN_POINT ( 'NONE',  ( -46.93859675662718445, 1379.681402112373007, 240.0333065786191753 ) ) ;
#33954 = CARTESIAN_POINT ( 'NONE',  ( -6.031288452957631385, 1442.578928665805051, 201.0498015145549573 ) ) ;
#33955 = CARTESIAN_POINT ( 'NONE',  ( -25.05784678700000256, 1436.599307041280099, 137.8256365093980094 ) ) ;
#33957 = CARTESIAN_POINT ( 'NONE',  ( 3.269184908365000197, 1516.940296199220029, 211.4060453336370244 ) ) ;
#33956 = AXIS2_PLACEMENT_3D ( 'NONE', #3820, #27324, #97288 ) ;
#33958 = CARTESIAN_POINT ( 'NONE',  ( -68.63570658849999973, 1379.747733383370132, 279.8437119496589958 ) ) ;
#33959 = EDGE_CURVE ( 'NONE', #12156, #102960, #91419, .T. ) ;
#33960 = CARTESIAN_POINT ( 'NONE',  ( 3.066583199566000534E-32, 1507.508085020990166, 209.1218459616989946 ) ) ;
#33961 = CARTESIAN_POINT ( 'NONE',  ( -12.98226561589999939, 1414.913060387329779, 219.9156672276980089 ) ) ;
#33962 = CARTESIAN_POINT ( 'NONE',  ( 7.719640903004999721, 1516.939452820819952, 209.1117431028050078 ) ) ;
#33963 = EDGE_LOOP ( 'NONE', ( #96374, #24432, #52417, #80912, #64004, #85765, #19903, #65146 ) ) ;
#33964 = CARTESIAN_POINT ( 'NONE',  ( 7.191383079060839734, 1407.162969929539940, 222.2855843901380126 ) ) ;
#33965 = CARTESIAN_POINT ( 'NONE',  ( 2.472529913803023227, 1523.678648413191695, 242.8674788698241400 ) ) ;
#33966 = CARTESIAN_POINT ( 'NONE',  ( -19.60082009959915439, 1457.065427842446070, 225.8893376101511592 ) ) ;
#33967 = VERTEX_POINT ( 'NONE', #65309 ) ;
#33968 = DIRECTION ( 'NONE',  ( 1.000000000000000000, 0.000000000000000000, 0.000000000000000000 ) ) ;
#33969 = CARTESIAN_POINT ( 'NONE',  ( -3.994937584009999654, 1430.106198397690150, 201.8091617978890042 ) ) ;
#33970 = CARTESIAN_POINT ( 'NONE',  ( 12.61799612763599931, 1435.605627051659894, 150.8454502525350165 ) ) ;
#33971 = CARTESIAN_POINT ( 'NONE',  ( -4.069861486464248834, 1440.920437169861543, 184.9827668850385294 ) ) ;
#33972 = CARTESIAN_POINT ( 'NONE',  ( -6.929999671550000073, 1413.957734829029960, 207.7807066811290042 ) ) ;
#33973 = CARTESIAN_POINT ( 'NONE',  ( -16.51370628721510769, 1525.137881624908914, 237.1983654728897477 ) ) ;
#33974 = CARTESIAN_POINT ( 'NONE',  ( 5.288836944179999833, 1486.626846567689881, 199.6980016761590093 ) ) ;
#33975 = FACE_OUTER_BOUND ( 'NONE', #25684, .T. ) ;
#33976 = DIRECTION ( 'NONE',  ( -0.5877852522924820189, 0.000000000000000000, -0.8090169943749410120 ) ) ;
#33977 = AXIS2_PLACEMENT_3D ( 'NONE', #5497, #39653, #98448 ) ;
#33979 = CARTESIAN_POINT ( 'NONE',  ( -10.97132182545054846, 1448.375239271800638, 192.9928798521789304 ) ) ;
#33978 = CARTESIAN_POINT ( 'NONE',  ( 1.133516965105000107, 1516.713079096360161, 213.7319258036569920 ) ) ;
#33980 = CARTESIAN_POINT ( 'NONE',  ( 20.38220676649999774, 1509.051558510829864, 188.9487562874980142 ) ) ;
#33982 = B_SPLINE_CURVE_WITH_KNOTS ( 'NONE', 3,
 ( #83831, #100086, #82736, #66519, #57004, #58101, #56444, #23369, #49701, #64864, #38521, #72699, #82176, #107381, #5476, #39636, #31226, #14409, #106822, #35082, #68713, #17696, #102817, #43501, #7675, #77645, #51900, #84387, #94999, #101715, #67058, #959, #41831, #59752, #16055, #76533, #75462, #86041, #25007, #109596 ),
 .UNSPECIFIED., .F., .F.,
 ( 4, 3, 3, 3, 3, 3, 3, 3, 3, 3, 3, 3, 3, 4 ),
 ( -69.76875995564780908, -68.67202237711899215, -65.92006359279810113, -64.08310293337700614, -62.52400609995530090, -62.22018943289130277, -61.00809290194970202, -59.74958159879579966, -58.45048782992339653, -57.09264840657949946, -55.60843193452539879, -53.96858821142179607, -51.98595283854560023, -50.09514683520000489 ),
 .UNSPECIFIED. ) ;
#33981 = CARTESIAN_POINT ( 'NONE',  ( 4.035490712554999249, 1516.630499592039996, 216.8333966482170183 ) ) ;
#33983 = ORIENTED_EDGE ( 'NONE', *, *, #102639, .T. ) ;
#33984 = FACE_OUTER_BOUND ( 'NONE', #74016, .T. ) ;
#33985 = ADVANCED_FACE ( 'NONE', ( #48508 ), #38966, .T. ) ;
#33986 = CARTESIAN_POINT ( 'NONE',  ( 15.93867488059997761, 1409.469629780827972, 193.0035952271976782 ) ) ;
#33987 = EDGE_LOOP ( 'NONE', ( #15074, #51270 ) ) ;
#33988 = CARTESIAN_POINT ( 'NONE',  ( 2.134333270180000408, 1421.175322270330071, 183.7859593446980000 ) ) ;
#33989 = DIRECTION ( 'NONE',  ( -0.02359658529091402182, 0.000000000000000000, 0.9997215618173935781 ) ) ;
#33990 = EDGE_CURVE ( 'NONE', #110334, #102960, #83195, .T. ) ;
#33991 = CARTESIAN_POINT ( 'NONE',  ( 2.340429037510286747, 1525.425665131969026, 176.3541395084411079 ) ) ;
#33992 = DIRECTION ( 'NONE',  ( 0.4978433412588781914, 0.000000000000000000, 0.8672669759446606230 ) ) ;
#33993 = CARTESIAN_POINT ( 'NONE',  ( -11.24713962180850046, 1471.253631266729826, 207.1712745178000148 ) ) ;
#33994 = CARTESIAN_POINT ( 'NONE',  ( 1.758995549052309482, 1416.415802373853694, 232.5708266743504566 ) ) ;
#33995 = AXIS2_PLACEMENT_3D ( 'NONE', #67965, #8569, #102074 ) ;
#33996 = CARTESIAN_POINT ( 'NONE',  ( 18.78419925920000111, 1416.547221146729953, 209.8405087369400235 ) ) ;
#33997 = FACE_OUTER_BOUND ( 'NONE', #16309, .T. ) ;
#33998 = CARTESIAN_POINT ( 'NONE',  ( -4.946284671489999951, 1438.194204504490017, 150.2421849576980151 ) ) ;
#33999 = CARTESIAN_POINT ( 'NONE',  ( 44.31826854632529944, 1440.913060365109914, 264.7143195917649905 ) ) ;
#34001 = DIRECTION ( 'NONE',  ( 0.8774038027816709606, -0.3849049474659920200, 0.2863751879623379626 ) ) ;
#34000 = CARTESIAN_POINT ( 'NONE',  ( -1.920586321285300047, 1420.567450626859909, 193.8392714366590326 ) ) ;
#34002 = CARTESIAN_POINT ( 'NONE',  ( 10.83054619811773023, 1424.983886448836756, 145.3935680669089834 ) ) ;
#34003 = ORIENTED_EDGE ( 'NONE', *, *, #106857, .F. ) ;
#34004 = ORIENTED_EDGE ( 'NONE', *, *, #79417, .T. ) ;
#34005 = CARTESIAN_POINT ( 'NONE',  ( 1.549183660830179887, 1416.134159091179981, 190.3847494287900020 ) ) ;
#34006 = CARTESIAN_POINT ( 'NONE',  ( 17.38027391549962530, 1410.701563970856796, 192.4672136578822688 ) ) ;
#34007 = CARTESIAN_POINT ( 'NONE',  ( -24.37050405849999990, 1442.224873102559968, 212.1537385852479929 ) ) ;
#34008 = CARTESIAN_POINT ( 'NONE',  ( 7.603309374910287133, 1410.551554993347054, 187.4403096356234926 ) ) ;
#34009 = CARTESIAN_POINT ( 'NONE',  ( -3.336075057610619066, 1426.003189273603766, 185.7745020016922695 ) ) ;
#34010 = DIRECTION ( 'NONE',  ( -0.1402804634180439824, -0.9901118076173108795, 0.000000000000000000 ) ) ;
#34011 = CARTESIAN_POINT ( 'NONE',  ( -1.523962952789999825, 1477.830549788930057, 230.7236636456979966 ) ) ;
#34012 = CARTESIAN_POINT ( 'NONE',  ( 13.20369377709999981, 1414.913528139930122, 198.1182872744979875 ) ) ;
#34013 = CARTESIAN_POINT ( 'NONE',  ( -57.76806226941249633, 1383.799805416490017, 276.6705433862790073 ) ) ;
#34014 = CARTESIAN_POINT ( 'NONE',  ( 7.089350657599999828, 1452.665494806429933, 152.4157077411979913 ) ) ;
#34016 = CARTESIAN_POINT ( 'NONE',  ( -27.44625323641425751, 1509.338203236318805, 212.0845200277061906 ) ) ;
#34015 =( BOUNDED_SURFACE ( )  B_SPLINE_SURFACE ( 5, 5, ( 
 ( #108694, #31431, #99725, #32546, #31986, #66176 ),
 ( #23578, #66720, #83480, #70041, #53221, #52662 ),
 ( #16801, #61089, #68930, #19018, #51004, #10090 ),
 ( #103600, #36396, #87360, #17917, #60519, #94085 ),
 ( #26327, #70585, #59, #94642, #95204, #62182 ),
 ( #44825, #10656, #2282, #43156, #104702, #27439 ),
 ( #85136, #44264, #8422, #78978, #52113, #1164 ),
 ( #77312, #51551, #27997, #35857, #34190, #78406 ),
 ( #8984, #86243, #18465, #26900, #86799, #104153 ),
 ( #9534, #42593, #76747, #61622, #1718, #95754 ),
 ( #17355, #43702, #77855, #68374, #102482, #103030 ),
 ( #25771, #59970, #85687, #610, #35294, #34740 ),
 ( #69479, #30183, #4461, #54332, #36941, #47562 ),
 ( #106896, #38055, #4990, #80053, #38589, #39135 ),
 ( #80610, #81684, #11215, #3374, #3925, #106356 ),
 ( #73313, #87928, #98498, #88462, #64375, #2822 ),
 ( #81146, #105825, #21766, #90090, #72232, #45379 ),
 ( #71707, #54873, #29103, #28552, #55967, #88996 ),
 ( #13374, #107449, #63829, #30745, #96308, #62751 ),
 ( #63289, #53791, #71138, #97403, #55418, #37501 ),
 ( #96869, #19587, #47021, #12284, #79518, #46478 ),
 ( #11748, #21209, #97941, #89552, #20673, #20138 ),
 ( #105258, #45917, #29642, #12841, #72768, #23979 ),
 ( #14487, #66592, #83351, #49226, #64926, #99589 ),
 ( #22872, #65480, #50339, #100158, #99039, #23443 ),
 ( #40803, #67135, #109669, #48679, #57081, #73871 ),
 ( #83905, #57638, #108559, #90646, #100696, #13929 ),
 ( #92856, #91752, #82802, #22317, #41369, #107999 ),
 ( #40251, #31296, #91205, #31849, #66036, #16132 ),
 ( #74433, #6096, #15027, #6650, #74982, #84464 ),
 ( #56519, #109130, #41916, #32412, #101233, #32945 ),
 ( #58174, #92302, #48116, #15572, #49774, #7211 ),
 ( #75534, #39705, #24533, #58721, #7751, #82255 ),
 ( #76072, #110213, #5556, #52534, #86667, #69906 ),
 ( #69345, #33486, #77726, #85548, #35717, #67688 ),
 ( #61496, #9415, #53090, #104020, #34611, #77185 ),
 ( #85000, #95626, #43577, #44134, #86121, #87229 ),
 ( #9963, #10518, #95077, #17779, #18895, #59290 ),
 ( #51980, #1039, #26196, #44692, #25086, #27315 ),
 ( #78268, #50870, #78839, #18343, #43027, #101796 ),
 ( #35161, #93407, #94505, #8844, #102898, #488 ),
 ( #60384, #59833, #1582, #16672, #8295, #103455 ),
 ( #26761, #60950, #42457, #76616, #68797, #110768 ),
 ( #34058, #68251, #102358, #25642, #93956, #17221 ),
 ( #51417, #36268, #21648, #105136, #37938, #3807 ),
 ( #11626, #45250, #46906, #71015, #45804, #71580 ),
 ( #3253, #46357, #55856, #106233, #89975, #13249 ),
 ( #87799, #79937, #2150, #29519, #70458, #38469 ),
 ( #97276, #105702, #28426, #36825, #72646, #21098 ),
 ( #63710, #98376, #62625, #37380, #72118, #12167 ),
 ( #79386, #4338, #28984, #30062, #106771, #81029 ),
 ( #64253, #80491, #97820, #55300, #89433, #88334 ),
 ( #63172, #2700, #104579, #12725, #47439, #27874 ),
 ( #20549, #62055, #96180, #19455, #96743, #53654 ),
 ( #11083, #54753, #20014, #54209, #88883, #14357 ),
 ( #58047, #82686, #14907, #101113, #74850, #58594 ),
 ( #24409, #56391, #48549, #5976, #49098, #40676 ),
 ( #107331, #75405, #15454, #30627, #90523, #73754 ),
 ( #82122, #109544, #13799, #23313, #73186, #74306 ),
 ( #91631, #47985, #107877, #5424, #6524, #41233 ),
 ( #81563, #39582, #108994, #32280, #100021, #100573 ),
 ( #40121, #108436, #32816, #64815, #91074, #83782 ),
 ( #66464, #23855, #31717, #98923, #65903, #22193 ),
 ( #31165, #57506, #83233, #92725, #65355, #92183 ),
 ( #16001, #99463, #67003, #7077, #4866, #22741 ),
 ( #49646, #39009, #56945, #42330, #27190, #50730 ),
 ( #59156, #102758, #41777, #42892, #35027, #60249 ),
 ( #76482, #24945, #85986, #9828, #8713, #50204 ),
 ( #77595, #43446, #68658, #69206, #103315, #86534 ),
 ( #9284, #84329, #94366, #102227, #52409, #7619 ),
 ( #78132, #26054, #69773, #43997, #51280, #93809 ),
 ( #101658, #1435, #17648, #60819, #51849, #103891 ),
 ( #26623, #61373, #901, #34483, #35581, #75932 ),
 ( #94944, #18213, #77050, #95492, #110087, #33362 ),
 ( #67555, #93276, #16539, #84863, #59696, #8161 ),
 ( #110634, #33919, #356, #25506, #68114, #17088 ),
 ( #85414, #88206, #46772, #55172, #63580, #97150 ),
 ( #28849, #63044, #20419, #54624, #105000, #106102 ) ),
 .UNSPECIFIED., .F., .F., .F. ) 
 B_SPLINE_SURFACE_WITH_KNOTS ( ( 6, 3, 3, 3, 3, 3, 3, 3, 3, 3, 3, 3, 3, 3, 3, 3, 3, 3, 3, 3, 3, 3, 3, 3, 3, 6 ),
 ( 6, 6 ),
 ( 0.000000000000000000, 3.902585213099999617, 6.240861926940000082, 6.790072646649999655, 8.377982366400001268, 8.928580102349998882, 10.97133995140000096, 12.98949692180000071, 13.60228008900000063, 15.24737252870000148, 15.86745694640000082, 18.51059426890000026, 22.57641725190000059, 26.75087197450000076, 31.16005629229999840, 33.90953505430000092, 34.60237748540000524, 36.31249047570000243, 36.97255805550000218, 38.99052022429999909, 41.04947707190000017, 41.62972334150000364, 43.19545136810000230, 43.76106149099999953, 46.17824368760000198, 50.04091111600000374 ),
 ( 0.000000000000000000, 4.712388980389100368 ),
 .UNSPECIFIED. ) 
 GEOMETRIC_REPRESENTATION_ITEM ( )  RATIONAL_B_SPLINE_SURFACE ( (
 ( 1.000000000000000000, 0.5999999999996520339, 0.3999999999996514677, 0.2999999999997390310, 0.2499999999998260003, 0.2500000000000000000),
 ( 1.000000000000000000, 0.5999999999996520339, 0.3999999999996514677, 0.2999999999997390310, 0.2499999999998260003, 0.2500000000000000000),
 ( 1.000000000000000000, 0.5999999999996520339, 0.3999999999996514677, 0.2999999999997390310, 0.2499999999998260003, 0.2500000000000000000),
 ( 1.000000000000000000, 0.5999999999996520339, 0.3999999999996514677, 0.2999999999997390310, 0.2499999999998260003, 0.2500000000000000000),
 ( 1.000000000000000000, 0.5999999999996520339, 0.3999999999996514677, 0.2999999999997390310, 0.2499999999998260003, 0.2500000000000000000),
 ( 1.000000000000000000, 0.5999999999996520339, 0.3999999999996514677, 0.2999999999997390310, 0.2499999999998260003, 0.2500000000000000000),
 ( 1.000000000000000000, 0.5999999999996520339, 0.3999999999996514677, 0.2999999999997390310, 0.2499999999998260003, 0.2500000000000000000),
 ( 1.000000000000000000, 0.5999999999996520339, 0.3999999999996514677, 0.2999999999997390310, 0.2499999999998260003, 0.2500000000000000000),
 ( 1.000000000000000000, 0.5999999999996520339, 0.3999999999996514677, 0.2999999999997390310, 0.2499999999998260003, 0.2500000000000000000),
 ( 1.000000000000000000, 0.5999999999996520339, 0.3999999999996514677, 0.2999999999997390310, 0.2499999999998260003, 0.2500000000000000000),
 ( 1.000000000000000000, 0.5999999999996520339, 0.3999999999996514677, 0.2999999999997390310, 0.2499999999998260003, 0.2500000000000000000),
 ( 1.000000000000000000, 0.5999999999996520339, 0.3999999999996514677, 0.2999999999997390310, 0.2499999999998260003, 0.2500000000000000000),
 ( 1.000000000000000000, 0.5999999999996520339, 0.3999999999996514677, 0.2999999999997390310, 0.2499999999998260003, 0.2500000000000000000),
 ( 1.000000000000000000, 0.5999999999996520339, 0.3999999999996514677, 0.2999999999997390310, 0.2499999999998260003, 0.2500000000000000000),
 ( 1.000000000000000000, 0.5999999999996520339, 0.3999999999996514677, 0.2999999999997390310, 0.2499999999998260003, 0.2500000000000000000),
 ( 1.000000000000000000, 0.5999999999996520339, 0.3999999999996514677, 0.2999999999997390310, 0.2499999999998260003, 0.2500000000000000000),
 ( 1.000000000000000000, 0.5999999999996520339, 0.3999999999996514677, 0.2999999999997390310, 0.2499999999998260003, 0.2500000000000000000),
 ( 1.000000000000000000, 0.5999999999996520339, 0.3999999999996514677, 0.2999999999997390310, 0.2499999999998260003, 0.2500000000000000000),
 ( 1.000000000000000000, 0.5999999999996520339, 0.3999999999996514677, 0.2999999999997390310, 0.2499999999998260003, 0.2500000000000000000),
 ( 1.000000000000000000, 0.5999999999996520339, 0.3999999999996514677, 0.2999999999997390310, 0.2499999999998260003, 0.2500000000000000000),
 ( 1.000000000000000000, 0.5999999999996520339, 0.3999999999996514677, 0.2999999999997390310, 0.2499999999998260003, 0.2500000000000000000),
 ( 1.000000000000000000, 0.5999999999996520339, 0.3999999999996514677, 0.2999999999997390310, 0.2499999999998260003, 0.2500000000000000000),
 ( 1.000000000000000000, 0.5999999999996520339, 0.3999999999996514677, 0.2999999999997390310, 0.2499999999998260003, 0.2500000000000000000),
 ( 1.000000000000000000, 0.5999999999996520339, 0.3999999999996514677, 0.2999999999997390310, 0.2499999999998260003, 0.2500000000000000000),
 ( 1.000000000000000000, 0.5999999999996520339, 0.3999999999996514677, 0.2999999999997390310, 0.2499999999998260003, 0.2500000000000000000),
 ( 1.000000000000000000, 0.5999999999996520339, 0.3999999999996514677, 0.2999999999997390310, 0.2499999999998260003, 0.2500000000000000000),
 ( 1.000000000000000000, 0.5999999999996520339, 0.3999999999996514677, 0.2999999999997390310, 0.2499999999998260003, 0.2500000000000000000),
 ( 1.000000000000000000, 0.5999999999996520339, 0.3999999999996514677, 0.2999999999997390310, 0.2499999999998260003, 0.2500000000000000000),
 ( 1.000000000000000000, 0.5999999999996520339, 0.3999999999996514677, 0.2999999999997390310, 0.2499999999998260003, 0.2500000000000000000),
 ( 1.000000000000000000, 0.5999999999996520339, 0.3999999999996514677, 0.2999999999997390310, 0.2499999999998260003, 0.2500000000000000000),
 ( 1.000000000000000000, 0.5999999999996520339, 0.3999999999996514677, 0.2999999999997390310, 0.2499999999998260003, 0.2500000000000000000),
 ( 1.000000000000000000, 0.5999999999996520339, 0.3999999999996514677, 0.2999999999997390310, 0.2499999999998260003, 0.2500000000000000000),
 ( 1.000000000000000000, 0.5999999999996520339, 0.3999999999996514677, 0.2999999999997390310, 0.2499999999998260003, 0.2500000000000000000),
 ( 1.000000000000000000, 0.5999999999996520339, 0.3999999999996514677, 0.2999999999997390310, 0.2499999999998260003, 0.2500000000000000000),
 ( 1.000000000000000000, 0.5999999999996520339, 0.3999999999996514677, 0.2999999999997390310, 0.2499999999998260003, 0.2500000000000000000),
 ( 1.000000000000000000, 0.5999999999996520339, 0.3999999999996514677, 0.2999999999997390310, 0.2499999999998260003, 0.2500000000000000000),
 ( 1.000000000000000000, 0.5999999999996520339, 0.3999999999996514677, 0.2999999999997390310, 0.2499999999998260003, 0.2500000000000000000),
 ( 1.000000000000000000, 0.5999999999996520339, 0.3999999999996514677, 0.2999999999997390310, 0.2499999999998260003, 0.2500000000000000000),
 ( 1.000000000000000000, 0.5999999999996520339, 0.3999999999996514677, 0.2999999999997390310, 0.2499999999998260003, 0.2500000000000000000),
 ( 1.000000000000000000, 0.5999999999996520339, 0.3999999999996514677, 0.2999999999997390310, 0.2499999999998260003, 0.2500000000000000000),
 ( 1.000000000000000000, 0.5999999999996520339, 0.3999999999996514677, 0.2999999999997390310, 0.2499999999998260003, 0.2500000000000000000),
 ( 1.000000000000000000, 0.5999999999996520339, 0.3999999999996514677, 0.2999999999997390310, 0.2499999999998260003, 0.2500000000000000000),
 ( 1.000000000000000000, 0.5999999999996520339, 0.3999999999996514677, 0.2999999999997390310, 0.2499999999998260003, 0.2500000000000000000),
 ( 1.000000000000000000, 0.5999999999996520339, 0.3999999999996514677, 0.2999999999997390310, 0.2499999999998260003, 0.2500000000000000000),
 ( 1.000000000000000000, 0.5999999999996520339, 0.3999999999996514677, 0.2999999999997390310, 0.2499999999998260003, 0.2500000000000000000),
 ( 1.000000000000000000, 0.5999999999996520339, 0.3999999999996514677, 0.2999999999997390310, 0.2499999999998260003, 0.2500000000000000000),
 ( 1.000000000000000000, 0.5999999999996520339, 0.3999999999996514677, 0.2999999999997390310, 0.2499999999998260003, 0.2500000000000000000),
 ( 1.000000000000000000, 0.5999999999996520339, 0.3999999999996514677, 0.2999999999997390310, 0.2499999999998260003, 0.2500000000000000000),
 ( 1.000000000000000000, 0.5999999999996520339, 0.3999999999996514677, 0.2999999999997390310, 0.2499999999998260003, 0.2500000000000000000),
 ( 1.000000000000000000, 0.5999999999996520339, 0.3999999999996514677, 0.2999999999997390310, 0.2499999999998260003, 0.2500000000000000000),
 ( 1.000000000000000000, 0.5999999999996520339, 0.3999999999996514677, 0.2999999999997390310, 0.2499999999998260003, 0.2500000000000000000),
 ( 1.000000000000000000, 0.5999999999996520339, 0.3999999999996514677, 0.2999999999997390310, 0.2499999999998260003, 0.2500000000000000000),
 ( 1.000000000000000000, 0.5999999999996520339, 0.3999999999996514677, 0.2999999999997390310, 0.2499999999998260003, 0.2500000000000000000),
 ( 1.000000000000000000, 0.5999999999996520339, 0.3999999999996514677, 0.2999999999997390310, 0.2499999999998260003, 0.2500000000000000000),
 ( 1.000000000000000000, 0.5999999999996520339, 0.3999999999996514677, 0.2999999999997390310, 0.2499999999998260003, 0.2500000000000000000),
 ( 1.000000000000000000, 0.5999999999996520339, 0.3999999999996514677, 0.2999999999997390310, 0.2499999999998260003, 0.2500000000000000000),
 ( 1.000000000000000000, 0.5999999999996520339, 0.3999999999996514677, 0.2999999999997390310, 0.2499999999998260003, 0.2500000000000000000),
 ( 1.000000000000000000, 0.5999999999996520339, 0.3999999999996514677, 0.2999999999997390310, 0.2499999999998260003, 0.2500000000000000000),
 ( 1.000000000000000000, 0.5999999999996520339, 0.3999999999996514677, 0.2999999999997390310, 0.2499999999998260003, 0.2500000000000000000),
 ( 1.000000000000000000, 0.5999999999996520339, 0.3999999999996514677, 0.2999999999997390310, 0.2499999999998260003, 0.2500000000000000000),
 ( 1.000000000000000000, 0.5999999999996520339, 0.3999999999996514677, 0.2999999999997390310, 0.2499999999998260003, 0.2500000000000000000),
 ( 1.000000000000000000, 0.5999999999996520339, 0.3999999999996514677, 0.2999999999997390310, 0.2499999999998260003, 0.2500000000000000000),
 ( 1.000000000000000000, 0.5999999999996520339, 0.3999999999996514677, 0.2999999999997390310, 0.2499999999998260003, 0.2500000000000000000),
 ( 1.000000000000000000, 0.5999999999996520339, 0.3999999999996514677, 0.2999999999997390310, 0.2499999999998260003, 0.2500000000000000000),
 ( 1.000000000000000000, 0.5999999999996520339, 0.3999999999996514677, 0.2999999999997390310, 0.2499999999998260003, 0.2500000000000000000),
 ( 1.000000000000000000, 0.5999999999996520339, 0.3999999999996514677, 0.2999999999997390310, 0.2499999999998260003, 0.2500000000000000000),
 ( 1.000000000000000000, 0.5999999999996520339, 0.3999999999996514677, 0.2999999999997390310, 0.2499999999998260003, 0.2500000000000000000),
 ( 1.000000000000000000, 0.5999999999996520339, 0.3999999999996514677, 0.2999999999997390310, 0.2499999999998260003, 0.2500000000000000000),
 ( 1.000000000000000000, 0.5999999999996520339, 0.3999999999996514677, 0.2999999999997390310, 0.2499999999998260003, 0.2500000000000000000),
 ( 1.000000000000000000, 0.5999999999996520339, 0.3999999999996514677, 0.2999999999997390310, 0.2499999999998260003, 0.2500000000000000000),
 ( 1.000000000000000000, 0.5999999999996520339, 0.3999999999996514677, 0.2999999999997390310, 0.2499999999998260003, 0.2500000000000000000),
 ( 1.000000000000000000, 0.5999999999996520339, 0.3999999999996514677, 0.2999999999997390310, 0.2499999999998260003, 0.2500000000000000000),
 ( 1.000000000000000000, 0.5999999999996520339, 0.3999999999996514677, 0.2999999999997390310, 0.2499999999998260003, 0.2500000000000000000),
 ( 1.000000000000000000, 0.5999999999996520339, 0.3999999999996514677, 0.2999999999997390310, 0.2499999999998260003, 0.2500000000000000000),
 ( 1.000000000000000000, 0.5999999999996520339, 0.3999999999996514677, 0.2999999999997390310, 0.2499999999998260003, 0.2500000000000000000),
 ( 1.000000000000000000, 0.5999999999996520339, 0.3999999999996514677, 0.2999999999997390310, 0.2499999999998260003, 0.2500000000000000000),
 ( 1.000000000000000000, 0.5999999999996520339, 0.3999999999996514677, 0.2999999999997390310, 0.2499999999998260003, 0.2500000000000000000),
 ( 1.000000000000000000, 0.5999999999996520339, 0.3999999999996514677, 0.2999999999997390310, 0.2499999999998260003, 0.2500000000000000000) ) ) 
 REPRESENTATION_ITEM ( '' )  SURFACE ( )  );
#34017 = DIRECTION ( 'NONE',  ( 0.000000000000000000, 0.000000000000000000, -1.000000000000000000 ) ) ;
#34019 = ORIENTED_EDGE ( 'NONE', *, *, #14901, .F. ) ;
#34018 = CARTESIAN_POINT ( 'NONE',  ( 23.69809918860000053, 1507.890500233530020, 195.1972782134980093 ) ) ;
#34020 = CARTESIAN_POINT ( 'NONE',  ( 33.05665451062220228, 1523.390106123591067, 217.3123061710359423 ) ) ;
#34021 = CIRCLE ( 'NONE', #73451, 2.000000000000003109 ) ;
#34022 = CARTESIAN_POINT ( 'NONE',  ( -32.23247795450000552, 1383.839374993809770, 229.8499276021589992 ) ) ;
#34023 = CARTESIAN_POINT ( 'NONE',  ( -16.28817577849460108, 1409.481856019149973, 224.8534995302130142 ) ) ;
#34024 = ORIENTED_EDGE ( 'NONE', *, *, #23975, .T. ) ;
#34025 = ORIENTED_EDGE ( 'NONE', *, *, #99506, .F. ) ;
#34026 = CARTESIAN_POINT ( 'NONE',  ( 18.88376639685650105, 1507.757527395500119, 229.9162007811029866 ) ) ;
#34027 = B_SPLINE_CURVE_WITH_KNOTS ( 'NONE', 3,
 ( #30867, #65044, #99159, #42037, #101353, #49344, #6764, #23567, #40926, #67261, #75105, #66708, #92417, #109791, #84028, #15153, #100816, #48245, #58843, #7329, #41492, #66166, #7870, #32536, #15690, #75652, #58295, #33608 ),
 .UNSPECIFIED., .F., .F.,
 ( 4, 2, 2, 1, 2, 2, 2, 1, 1, 1, 1, 1, 2, 2, 2, 2, 4 ),
 ( 0.000000000000000000, 0.2499999999999318878, 0.3749999999998951394, 0.4374999999998763767, 0.4687499999998644973, 0.4999999999998526734, 0.6249999999998108180, 0.6874999999997875033, 0.7187499999997730704, 0.7343749999997656319, 0.7421874999997594147, 0.7460937499997561950, 0.7480468749997573052, 0.7499999999997585265, 0.8749999999998818723, 0.9374999999999408251, 1.000000000000000000 ),
 .UNSPECIFIED. ) ;
#34028 = DIRECTION ( 'NONE',  ( -0.02359658529091402182, 0.000000000000000000, 0.9997215618173935781 ) ) ;
#34029 = CARTESIAN_POINT ( 'NONE',  ( 39.95031265526250763, 1441.572021889720190, 136.8870288321719784 ) ) ;
#34031 = DIRECTION ( 'NONE',  ( -0.9510565162951518658, 0.000000000000000000, 0.3090169943749528914 ) ) ;
#34030 = CARTESIAN_POINT ( 'NONE',  ( 19.82086717690000199, 1452.811554597230042, 209.2880291464769869 ) ) ;
#34032 = VECTOR ( 'NONE', #106227, 1000.000000000000000 ) ;
#34033 = CARTESIAN_POINT ( 'NONE',  ( -8.930212406729999941, 1461.403864792989907, 205.1993326667990232 ) ) ;
#34034 = CARTESIAN_POINT ( 'NONE',  ( -109.1500278820000034, 1384.113452266690047, 297.1923599218590084 ) ) ;
#34035 = CARTESIAN_POINT ( 'NONE',  ( -21.54116136303244389, 1523.462669333492613, 234.3126182784949947 ) ) ;
#34036 = CARTESIAN_POINT ( 'NONE',  ( 41.65927937599999353, 1443.915252855300196, 135.6909788338979865 ) ) ;
#34037 = CYLINDRICAL_SURFACE ( 'NONE', #40610, 4.000000000000006217 ) ;
#34038 = CARTESIAN_POINT ( 'NONE',  ( 1.411045156649999965, 1409.467890906029879, 185.4969889618979835 ) ) ;
#34039 = CARTESIAN_POINT ( 'NONE',  ( 4.520455601509999255, 1424.084465838330061, 184.9550280210980020 ) ) ;
#34040 = CARTESIAN_POINT ( 'NONE',  ( 1.248280726178319977, 1432.832982257020149, 200.7627227404510108 ) ) ;
#34041 = CARTESIAN_POINT ( 'NONE',  ( -2.712996093226240024, 1440.235714014299901, 157.0895377761229952 ) ) ;
#34042 = AXIS2_PLACEMENT_3D ( 'NONE', #62632, #88341, #63717 ) ;
#34043 = CARTESIAN_POINT ( 'NONE',  ( 11.84242365151049903, 1431.324256260269976, 147.6543138665190043 ) ) ;
#34044 = CARTESIAN_POINT ( 'NONE',  ( 0.1422329807200000129, 1466.041212668930029, 235.8555543989980094 ) ) ;
#34045 = ORIENTED_EDGE ( 'NONE', *, *, #66692, .T. ) ;
#34046 = CARTESIAN_POINT ( 'NONE',  ( 20.67523678790000119, 1478.097707044290019, 217.5712452575990028 ) ) ;
#34047 = CARTESIAN_POINT ( 'NONE',  ( -20.70484064406422320, 1525.907212628473644, 185.0411015109855839 ) ) ;
#34048 = CARTESIAN_POINT ( 'NONE',  ( -25.98102620619109970, 1446.564900598659960, 138.2990622187889755 ) ) ;
#34049 = CARTESIAN_POINT ( 'NONE',  ( 15.72751745975079984, 1522.051704408389924, 206.8816388537309763 ) ) ;
#34050 = CARTESIAN_POINT ( 'NONE',  ( 3.066583199566000534E-32, 1507.508085020990166, 209.1218459616989946 ) ) ;
#34051 = CARTESIAN_POINT ( 'NONE',  ( -9.599706269345578398E-10, 1471.041207172160057, 256.6978854479500001 ) ) ;
#34052 = DIRECTION ( 'NONE',  ( 0.8775825618903763115, 0.000000000000000000, 0.4794255386041965106 ) ) ;
#34053 = CARTESIAN_POINT ( 'NONE',  ( -0.9063479630909999640, 1415.579607672129896, 227.4689347612980157 ) ) ;
#34054 = CARTESIAN_POINT ( 'NONE',  ( -6.479667820239999543, 1418.395698601130107, 233.3433503499980191 ) ) ;
#34055 = CARTESIAN_POINT ( 'NONE',  ( 0.8317469223220009811, 1476.953783366089965, 198.6245987969989812 ) ) ;
#34056 = CARTESIAN_POINT ( 'NONE',  ( -106.2645803829999949, 1391.084643298059973, 307.7533666201589426 ) ) ;
#34057 = CARTESIAN_POINT ( 'NONE',  ( -0.6140284191404157266, 1485.453369257635131, 181.9287747154768908 ) ) ;
#34058 = CARTESIAN_POINT ( 'NONE',  ( 5.604365146370000161, 1361.139420828410039, 207.6218459616989946 ) ) ;
#34059 = CARTESIAN_POINT ( 'NONE',  ( -45.74118403190329474, 1438.479771586579773, 268.7597751522629324 ) ) ;
#34060 = CARTESIAN_POINT ( 'NONE',  ( 0.7301090186228299528, 1429.703966172960008, 217.4049395672290075 ) ) ;
#34061 = CARTESIAN_POINT ( 'NONE',  ( -7.604290685550000539, 1426.735974020640015, 206.0921002386889995 ) ) ;
#34062 = ORIENTED_EDGE ( 'NONE', *, *, #59929, .F. ) ;
#34063 = CARTESIAN_POINT ( 'NONE',  ( 2.873919002525000099, 1516.940252185109784, 209.1085733957019954 ) ) ;
#34064 = AXIS2_PLACEMENT_3D ( 'NONE', #92973, #77299, #59406 ) ;
#34065 = CARTESIAN_POINT ( 'NONE',  ( -5.402319840979999732, 1434.355786217680134, 154.6519182847980005 ) ) ;
#34066 = B_SPLINE_SURFACE_WITH_KNOTS ( 'NONE', 5, 5, ( 
 ( #81516, #40083, #63129, #72074, #97231, #4820 ),
 ( #46316, #106727, #38423, #106189, #30581, #4295 ),
 ( #3759, #72598, #98881, #37891, #29472, #63664 ),
 ( #21054, #55258, #12680, #5381, #21608, #46860 ),
 ( #80989, #55813, #22148, #41191, #74263, #100534 ),
 ( #110596, #93236, #57465, #67516, #59659, #66417 ) ),
 .UNSPECIFIED., .F., .F., .F.,
 ( 6, 6 ),
 ( 6, 6 ),
 ( -1.600009832348449890E-05, 6.607489203828340152 ),
 ( -1.600009834268530264E-05, 2.000000000000000000 ),
 .UNSPECIFIED. ) ;
#34067 = CARTESIAN_POINT ( 'NONE',  ( 19.32507466223246340, 1456.645243537790293, 224.6377563528816950 ) ) ;
#34068 = CARTESIAN_POINT ( 'NONE',  ( 7.474209936774370178, 1426.071330082020040, 212.3877608208809704 ) ) ;
#34069 = CARTESIAN_POINT ( 'NONE',  ( -26.06749262380980170, 1451.758091925960116, 135.9256846038920230 ) ) ;
#34070 = ORIENTED_EDGE ( 'NONE', *, *, #12130, .T. ) ;
#34071 = CARTESIAN_POINT ( 'NONE',  ( 16.68183166340000056, 1424.849819094029954, 221.4660109932979992 ) ) ;
#34073 = CARTESIAN_POINT ( 'NONE',  ( -15.30763532073890154, 1512.674009804170055, 222.5874652136580210 ) ) ;
#34072 = CARTESIAN_POINT ( 'NONE',  ( -3.177699364621945133, 1525.042337199240137, 176.6379248602500525 ) ) ;
#34074 = CARTESIAN_POINT ( 'NONE',  ( -1.927277385857209868, 1419.501960165059927, 185.7627030526099929 ) ) ;
#34075 = AXIS2_PLACEMENT_3D ( 'NONE', #78187, #2065, #46281 ) ;
#34076 = CARTESIAN_POINT ( 'NONE',  ( 3.331783404088237699, 1522.051704408389924, 197.4348858789911674 ) ) ;
#34077 = CARTESIAN_POINT ( 'NONE',  ( -3.835404308833623155, 1396.046995657106436, 202.1011854665750036 ) ) ;
#34078 = CARTESIAN_POINT ( 'NONE',  ( -22.74821099489519938, 1452.118675354829747, 139.2359698183670105 ) ) ;
#34079 = CARTESIAN_POINT ( 'NONE',  ( 4.939530087350459949E-13, 1547.051704408389924, 209.1218459616989946 ) ) ;
#34080 = ORIENTED_EDGE ( 'NONE', *, *, #74621, .F. ) ;
#34081 = CARTESIAN_POINT ( 'NONE',  ( -0.6098768256049610370, 1408.561131195760026, 270.4290843811310197 ) ) ;
#34082 = CARTESIAN_POINT ( 'NONE',  ( 6.582508756332179800, 1418.411819419869744, 233.6284590037290059 ) ) ;
#34083 = CARTESIAN_POINT ( 'NONE',  ( -7.112123039035762595, 1509.032357807246171, 215.8638904077538996 ) ) ;
#34084 = EDGE_LOOP ( 'NONE', ( #39749, #79301, #93165, #66187, #57367 ) ) ;
#34085 = VERTEX_POINT ( 'NONE', #82077 ) ;
#34086 = CARTESIAN_POINT ( 'NONE',  ( -23.44508921861510231, 1410.148484811090157, 210.0298535335690246 ) ) ;
#34087 = CARTESIAN_POINT ( 'NONE',  ( -4.363122647540000010, 1423.854802298929826, 184.2546043570980032 ) ) ;
#34088 = CARTESIAN_POINT ( 'NONE',  ( -11.49747574035130171, 1416.913060341609935, 197.9009878090930101 ) ) ;
#34089 = CARTESIAN_POINT ( 'NONE',  ( -45.16578704421618795, 1435.656933826767045, 266.2029088751467611 ) ) ;
#34090 = CARTESIAN_POINT ( 'NONE',  ( -20.30416289926380458, 1484.529698969839956, 192.9143954880039757 ) ) ;
#34091 = CARTESIAN_POINT ( 'NONE',  ( 4.556906905527969620, 1508.729448404669938, 212.2592272162939935 ) ) ;
#34092 = EDGE_CURVE ( 'NONE', #45960, #76272, #52440, .T. ) ;
#34093 = CARTESIAN_POINT ( 'NONE',  ( 29.93303073770439582, 1467.353064289500026, 266.6087639478620304 ) ) ;
#34094 = CARTESIAN_POINT ( 'NONE',  ( -4.429741958790829770, 1508.551704408389924, 204.3196020111140001 ) ) ;
#34095 = CARTESIAN_POINT ( 'NONE',  ( -17.31863478597802697, 1422.547962107037165, 226.6134709424001414 ) ) ;
#34096 = CARTESIAN_POINT ( 'NONE',  ( 2.284199363404999961, 1516.940296199220029, 205.8526610237369994 ) ) ;
#34097 = ORIENTED_EDGE ( 'NONE', *, *, #87037, .T. ) ;
#34098 = CARTESIAN_POINT ( 'NONE',  ( 18.51214429768622693, 1458.740534512576005, 227.6070309199760118 ) ) ;
#34099 = CARTESIAN_POINT ( 'NONE',  ( -1.156571746234419829, 1444.424822986080017, 199.1343848052200087 ) ) ;
#34100 = AXIS2_PLACEMENT_3D ( 'NONE', #15458, #51285, #83785 ) ;
#34101 = CARTESIAN_POINT ( 'NONE',  ( -109.9849726248329915, 1384.916895159399928, 311.4561123681800154 ) ) ;
#34102 = ORIENTED_EDGE ( 'NONE', *, *, #83267, .T. ) ;
#34103 = CARTESIAN_POINT ( 'NONE',  ( 3.931911118920000447, 1448.296755884660115, 184.2998928590980086 ) ) ;
#34105 = EDGE_CURVE ( 'NONE', #71856, #32890, #43408, .T. ) ;
#34104 = CARTESIAN_POINT ( 'NONE',  ( 5.589575339105699925, 1434.643108874500058, 202.6764547222993258 ) ) ;
#34106 = CARTESIAN_POINT ( 'NONE',  ( -4.391179462891900087, 1508.551704408389924, 213.2284805894280169 ) ) ;
#34107 = CARTESIAN_POINT ( 'NONE',  ( -16.33302336319999881, 1384.944327755149970, 200.5749513780490076 ) ) ;
#34108 = CARTESIAN_POINT ( 'NONE',  ( 7.549774212029999987, 1421.876882727210159, 195.6872530139989976 ) ) ;
#34109 = CARTESIAN_POINT ( 'NONE',  ( -2.427052486703370260, 1432.867848442830109, 218.3435047856359859 ) ) ;
#34110 = CARTESIAN_POINT ( 'NONE',  ( -3.467940584279999960, 1495.562067875890079, 197.2905559997990110 ) ) ;
#34111 = CARTESIAN_POINT ( 'NONE',  ( 1.968667276625390095, 1408.981807763489996, 186.9191247717589874 ) ) ;
#34113 = CARTESIAN_POINT ( 'NONE',  ( -17.83359347479203905, 1423.458363862109991, 226.0411963962040147 ) ) ;
#34112 = CARTESIAN_POINT ( 'NONE',  ( 1.270493918489999929, 1416.663721100529983, 233.2811219237980254 ) ) ;
#34114 = CARTESIAN_POINT ( 'NONE',  ( 13.31824321100000041, 1409.378143688529917, 226.7832290943979956 ) ) ;
#34115 = B_SPLINE_CURVE_WITH_KNOTS ( 'NONE', 3,
 ( #81910, #31508, #30411, #41014, #56730, #64600, #24199, #58385, #49438, #108220, #22530, #83560, #92511, #23101, #65689, #5215, #6853, #66258, #108774 ),
 .UNSPECIFIED., .F., .F.,
 ( 4, 3, 3, 3, 3, 3, 4 ),
 ( -6.813843844574179798, -6.758570408419999787, -5.962361183245239893, -5.075104183334910424, -4.429419003180000480, -4.352120018539999968, -4.284224695669999861 ),
 .UNSPECIFIED. ) ;
#34116 = CARTESIAN_POINT ( 'NONE',  ( -12.36377300989999917, 1379.230270180880098, 212.7119248548690109 ) ) ;
#34117 = CARTESIAN_POINT ( 'NONE',  ( -7.891238773387773797, 1517.051704408389924, 228.7291753153190825 ) ) ;
#34118 = ORIENTED_EDGE ( 'NONE', *, *, #50782, .T. ) ;
#34119 = CARTESIAN_POINT ( 'NONE',  ( -32.86802468386296994, 1523.382868172864164, 201.0396662540046577 ) ) ;
#34120 = VECTOR ( 'NONE', #25906, 1000.000000000000000 ) ;
#34121 = CARTESIAN_POINT ( 'NONE',  ( 11.60004869885203682, 1411.254281879943164, 137.0999999980979851 ) ) ;
#34122 = CARTESIAN_POINT ( 'NONE',  ( 31.99468309217332873, 1524.860077346004573, 202.1252391477154617 ) ) ;
#34123 = CARTESIAN_POINT ( 'NONE',  ( -10.39050546589999868, 1389.480500668439845, 202.2954434700990021 ) ) ;
#34124 = CARTESIAN_POINT ( 'NONE',  ( 9.741659962066350431, 1422.546270596229988, 212.4615314579379799 ) ) ;
#34125 = B_SPLINE_CURVE_WITH_KNOTS ( 'NONE', 3,
 ( #104373, #105485, #94869, #95974, #79744, #19235, #28776, #71373, #10878, #45050, #79194, #104931, #11431, #43376, #28218, #62405, #96533, #19807, #54013, #64604, #31512, #38263 ),
 .UNSPECIFIED., .F., .F.,
 ( 4, 2, 2, 1, 1, 1, 1, 2, 2, 2, 2, 2, 4 ),
 ( 0.000000000000000000, 0.2500000000000847655, 0.3750000000001300071, 0.4375000000001500466, 0.4687500000001631473, 0.4843750000001671441, 0.4921875000001716960, 0.4960937500001712519, 0.5000000000001707523, 0.7500000000000853762, 0.8125000000000641709, 0.8750000000000429656, 1.000000000000000000 ),
 .UNSPECIFIED. ) ;
#34126 = CARTESIAN_POINT ( 'NONE',  ( -34.99794265375160052, 1450.308730971829846, 136.2298232396449862 ) ) ;
#34127 = AXIS2_PLACEMENT_3D ( 'NONE', #99618, #14517, #49257 ) ;
#34128 = CARTESIAN_POINT ( 'NONE',  ( 1.124949149999999953, 1430.908435203989939, 217.7868727458690046 ) ) ;
#34129 = DIRECTION ( 'NONE',  ( 0.1070030146457237041, 0.000000000000000000, -0.9942586961433764747 ) ) ;
#34130 = CARTESIAN_POINT ( 'NONE',  ( -3.500000000000000000, 1422.625370988529994, 168.5578661042980286 ) ) ;
#34131 = CARTESIAN_POINT ( 'NONE',  ( 11.72722094679999927, 1433.446908946229996, 150.8820538568979828 ) ) ;
#34132 = CARTESIAN_POINT ( 'NONE',  ( 12.48077398530000082, 1459.371347868330076, 243.9198229428980085 ) ) ;
#34133 = CARTESIAN_POINT ( 'NONE',  ( 12.28605913131140071, 1415.088506334930116, 197.2751500656220287 ) ) ;
#34134 = CIRCLE ( 'NONE', #39500, 2.000000000000002220 ) ;
#34135 = CARTESIAN_POINT ( 'NONE',  ( -22.53878221424140094, 1411.058442688259902, 212.0450776560099939 ) ) ;
#34136 = B_SPLINE_CURVE_WITH_KNOTS ( 'NONE', 3,
 ( #91747, #49221, #83347, #109665, #40799, #74978, #76610, #109126, #32407, #15568 ),
 .UNSPECIFIED., .F., .F.,
 ( 4, 2, 2, 2, 4 ),
 ( 0.000000000000000000, 0.2499999999999998890, 0.4999999999999998890, 0.7499999999999998890, 1.000000000000000000 ),
 .UNSPECIFIED. ) ;
#34137 = CARTESIAN_POINT ( 'NONE',  ( 10.53309060615429793, 1424.587086563600224, 199.9078566869370093 ) ) ;
#34138 = CARTESIAN_POINT ( 'NONE',  ( 9.224637020051591918, 1464.192156177939978, 212.6135812687480211 ) ) ;
#34139 = CARTESIAN_POINT ( 'NONE',  ( -19.01375814760000083, 1486.340012975929994, 189.2527429762979807 ) ) ;
#34140 = APPLICATION_CONTEXT ( 'automotive_design' ) ;
#34141 = CIRCLE ( 'NONE', #3724, 2.000000000000001776 ) ;
#34142 = CARTESIAN_POINT ( 'NONE',  ( 10.63098969396934379, 1398.228131935662532, 216.6347355816575089 ) ) ;
#34143 = CARTESIAN_POINT ( 'NONE',  ( -29.45841291127520023, 1509.941770834379895, 211.8256419367419880 ) ) ;
#34144 = CARTESIAN_POINT ( 'NONE',  ( 23.43227205659999868, 1410.913138743030004, 212.1033097375579928 ) ) ;
#34145 = PLANE ( 'NONE',  #41366 ) ;
#34146 = CARTESIAN_POINT ( 'NONE',  ( 26.21349280692992778, 1436.698295471538813, 136.8766113756052221 ) ) ;
#34147 = CARTESIAN_POINT ( 'NONE',  ( -1.485893011569999977, 1515.551703577890066, 205.2152226796090133 ) ) ;
#34148 = CARTESIAN_POINT ( 'NONE',  ( 21.79083509029999988, 1497.713060387329961, 214.0856487658080027 ) ) ;
#34149 = CARTESIAN_POINT ( 'NONE',  ( -21.47379561725159647, 1487.892728963219952, 202.0847257228780052 ) ) ;
#34150 = CARTESIAN_POINT ( 'NONE',  ( -0.7356989727169980231, 1517.020847257979995, 212.5827121409169820 ) ) ;
#34151 = CARTESIAN_POINT ( 'NONE',  ( -21.23871617420000391, 1418.070708022229837, 210.0663963951400319 ) ) ;
#34152 = CARTESIAN_POINT ( 'NONE',  ( 0.1759063265243840102, 1476.870715021929982, 182.2288026130389653 ) ) ;
#34154 = ORIENTED_EDGE ( 'NONE', *, *, #35626, .F. ) ;
#34153 = CARTESIAN_POINT ( 'NONE',  ( -5.370514330159649852, 1422.356910281434239, 139.1416123588654727 ) ) ;
#34155 = FACE_OUTER_BOUND ( 'NONE', #25835, .T. ) ;
#34156 = CARTESIAN_POINT ( 'NONE',  ( -12.09621839340030824, 1446.031655959586260, 193.6906851894976853 ) ) ;
#34157 = CARTESIAN_POINT ( 'NONE',  ( 13.19843678480000015, 1434.900414026109956, 149.6995543751980051 ) ) ;
#34158 = CARTESIAN_POINT ( 'NONE',  ( -41.60033908840290451, 1444.718971643000032, 134.0999999983919793 ) ) ;
#34159 = DIRECTION ( 'NONE',  ( -1.836970198721029688E-16, -1.000000000000000000, 0.000000000000000000 ) ) ;
#34160 = ORIENTED_EDGE ( 'NONE', *, *, #10728, .F. ) ;
#34161 = CARTESIAN_POINT ( 'NONE',  ( -10.57294294639999954, 1471.242314994889966, 209.3037664082490323 ) ) ;
#34162 = CARTESIAN_POINT ( 'NONE',  ( -11.87131397077319939, 1392.058811529140030, 212.5838674967049826 ) ) ;
#34163 = CARTESIAN_POINT ( 'NONE',  ( 7.224377867204991865, 1447.376750353422722, 203.6098548312575929 ) ) ;
#34164 = CARTESIAN_POINT ( 'NONE',  ( -22.03465957474533354, 1522.382868172863937, 235.4136513321633117 ) ) ;
#34165 = CARTESIAN_POINT ( 'NONE',  ( -8.498308697023119862, 1436.913760846189916, 212.4344101014090143 ) ) ;
#34166 = CARTESIAN_POINT ( 'NONE',  ( -13.20398174397830005, 1430.333021908660157, 195.5447948587090252 ) ) ;
#34167 = DIRECTION ( 'NONE',  ( -0.1402804634201463563, 0.9901118076170130067, 0.000000000000000000 ) ) ;
#34168 = CARTESIAN_POINT ( 'NONE',  ( 8.469197029634038643, 1409.208811264400083, 221.4585696155599805 ) ) ;
#34169 = CARTESIAN_POINT ( 'NONE',  ( -11.88051395989999826, 1391.844827726459926, 207.0742441280090134 ) ) ;
#34170 = CARTESIAN_POINT ( 'NONE',  ( -81.42081042106549660, 1385.163088500089998, 284.9116589515040232 ) ) ;
#34171 = CARTESIAN_POINT ( 'NONE',  ( -11.35261338943339915, 1391.913060387289988, 211.5365630498070004 ) ) ;
#34172 = CARTESIAN_POINT ( 'NONE',  ( 11.59960881601659999, 1426.963225802300030, 207.4389891066049927 ) ) ;
#34173 = VERTEX_POINT ( 'NONE', #24906 ) ;
#34174 = CARTESIAN_POINT ( 'NONE',  ( -29.31190787429999745, 1451.889799756029788, 135.2848617097980082 ) ) ;
#34175 = CARTESIAN_POINT ( 'NONE',  ( -15.77958100662340080, 1409.472299422209971, 225.4880743202079998 ) ) ;
#34177 = ORIENTED_EDGE ( 'NONE', *, *, #86959, .T. ) ;
#34176 = DIRECTION ( 'NONE',  ( 0.000000000000000000, -1.000000000000000000, 0.000000000000000000 ) ) ;
#34178 = CARTESIAN_POINT ( 'NONE',  ( 5.242187580730000462, 1473.743341493890057, 218.7973554873690034 ) ) ;
#34179 = ADVANCED_FACE ( 'NONE', ( #77012 ), #14496, .T. ) ;
#34180 = CARTESIAN_POINT ( 'NONE',  ( 19.31452971239999883, 1455.192177364190002, 208.1916251275950174 ) ) ;
#34181 = CARTESIAN_POINT ( 'NONE',  ( -7.992490671317017181, 1364.617306788744372, 208.3718459617061285 ) ) ;
#34182 = CARTESIAN_POINT ( 'NONE',  ( -0.1548099527865300085, 1420.468350699849907, 182.8372881064299804 ) ) ;
#34183 = CARTESIAN_POINT ( 'NONE',  ( -7.947250565765000552, 1514.433282224309778, 212.1193490295570143 ) ) ;
#34184 = CARTESIAN_POINT ( 'NONE',  ( -11.60004869885203505, 1428.425991026145311, 134.1711281075547788 ) ) ;
#34185 = EDGE_CURVE ( 'NONE', #83271, #65641, #39615, .T. ) ;
#34186 = CARTESIAN_POINT ( 'NONE',  ( 19.00883633615545421, 1437.780163653907039, 213.2322572209417899 ) ) ;
#34187 = CARTESIAN_POINT ( 'NONE',  ( 1.873062257339999981, 1417.577345317929939, 233.6032974765979873 ) ) ;
#34188 = CARTESIAN_POINT ( 'NONE',  ( 5.981358413060000601, 1447.780665424890003, 201.2187644437790084 ) ) ;
#34189 = CARTESIAN_POINT ( 'NONE',  ( -23.28153290659989949, 1507.877024493434192, 223.8845470390981802 ) ) ;
#34190 = CARTESIAN_POINT ( 'NONE',  ( -8.882606460297679973, 1368.497287369286596, 210.6218459617030021 ) ) ;
#34191 = CARTESIAN_POINT ( 'NONE',  ( -30.37359097063588109, 1526.143142182216252, 216.9284661788367998 ) ) ;
#34192 = CARTESIAN_POINT ( 'NONE',  ( 2.283570633165000086, 1516.909589401870107, 206.2402975076569760 ) ) ;
#34193 = CARTESIAN_POINT ( 'NONE',  ( 9.862951377358559313, 1517.151704408390060, 189.8497022443989977 ) ) ;
#34194 = COLOUR_RGB ( '', 0.66274510, 0.83137255, 0.94901961) ;
#34195 = CARTESIAN_POINT ( 'NONE',  ( -2.500000000000000000, 1434.283878676689937, 157.5533472140980109 ) ) ;
#34196 = FACE_OUTER_BOUND ( 'NONE', #47572, .T. ) ;
#34198 = ORIENTED_EDGE ( 'NONE', *, *, #96968, .F. ) ;
#34197 = CARTESIAN_POINT ( 'NONE',  ( -3.126045989589999685, 1496.690033224690069, 220.3233446123989836 ) ) ;
#34199 = CARTESIAN_POINT ( 'NONE',  ( -33.93529341107537078, 1435.841716432657222, 135.9421945816383470 ) ) ;
#34200 = ORIENTED_EDGE ( 'NONE', *, *, #89043, .F. ) ;
#34201 = CARTESIAN_POINT ( 'NONE',  ( -16.55311987254050976, 1514.160701262670727, 223.3688575977173514 ) ) ;
#34202 = CARTESIAN_POINT ( 'NONE',  ( -21.12097961670000146, 1430.346877887030132, 198.3664044052980273 ) ) ;
#34204 = CARTESIAN_POINT ( 'NONE',  ( 16.85684277289790245, 1410.872046192200060, 191.8747558144809773 ) ) ;
#34203 = CARTESIAN_POINT ( 'NONE',  ( -11.06783048073080167, 1426.044759707710000, 103.8947504975569984 ) ) ;
#34205 = CARTESIAN_POINT ( 'NONE',  ( 0.7579843820170020230, 1516.883361325900069, 211.4083188566570186 ) ) ;
#34206 = CLOSED_SHELL ( 'NONE', ( #74966, #61184, #92370, #7900, #41766, #53548, #66841, #98059, #103639, #24627, #76834, #93325, #12459, #91525 ) ) ;
#34207 = CARTESIAN_POINT ( 'NONE',  ( 17.11918923422064864, 1509.631155535743119, 184.4835570923741841 ) ) ;
#34208 = CARTESIAN_POINT ( 'NONE',  ( 1.520098423109999874, 1489.452917662129948, 187.0062982106979916 ) ) ;
#34209 = CARTESIAN_POINT ( 'NONE',  ( -7.132051953269999522, 1405.830933579630027, 267.2558761556979903 ) ) ;
#34210 = CARTESIAN_POINT ( 'NONE',  ( 16.35567120235890215, 1509.488510095419770, 233.6167396447019655 ) ) ;
#34211 = CARTESIAN_POINT ( 'NONE',  ( 2.344512076345889984, 1516.526058371499857, 216.8306617650070223 ) ) ;
#34212 = CARTESIAN_POINT ( 'NONE',  ( 4.530018341142350025, 1508.551704408389924, 213.0522568375050128 ) ) ;
#34213 = CARTESIAN_POINT ( 'NONE',  ( -38.63631528028910367, 1439.261520478130024, 136.6606707570919923 ) ) ;
#34214 = ORIENTED_EDGE ( 'NONE', *, *, #109828, .T. ) ;
#34215 = CARTESIAN_POINT ( 'NONE',  ( 11.36773274011689949, 1396.369100750580174, 213.4700073609069761 ) ) ;
#34216 = CARTESIAN_POINT ( 'NONE',  ( 10.76124213208149882, 1460.439160552989961, 207.1949203455349959 ) ) ;
#34217 = CARTESIAN_POINT ( 'NONE',  ( -16.63810603980000025, 1458.859429223330153, 229.6331253552980058 ) ) ;
#34218 = ORIENTED_EDGE ( 'NONE', *, *, #65041, .F. ) ;
#34219 = ORIENTED_EDGE ( 'NONE', *, *, #102943, .T. ) ;
#34220 = CARTESIAN_POINT ( 'NONE',  ( -0.5698918850559979710, 1425.422772561009879, 191.0863376515989955 ) ) ;
#34221 = CARTESIAN_POINT ( 'NONE',  ( -16.68599179819999989, 1461.099982565929849, 230.2790296985980092 ) ) ;
#34222 = VECTOR ( 'NONE', #92958, 1000.000000000000114 ) ;
#34223 = CARTESIAN_POINT ( 'NONE',  ( -14.30929470490690036, 1380.323785527690006, 209.9761919504450134 ) ) ;
#34224 = CARTESIAN_POINT ( 'NONE',  ( -14.20525283303160080, 1416.384016890880048, 203.1489016136929706 ) ) ;
#34225 = CARTESIAN_POINT ( 'NONE',  ( -6.541070373676360461, 1517.051704644259871, 205.4524592699869743 ) ) ;
#34226 = CARTESIAN_POINT ( 'NONE',  ( -2.621078202464676821, 1523.542365884047513, 242.1599611597541752 ) ) ;
#34227 = CARTESIAN_POINT ( 'NONE',  ( 21.38516915557986309, 1512.187213306747481, 237.8497028174237471 ) ) ;
#34228 = CARTESIAN_POINT ( 'NONE',  ( 0.9370951295164038353, 1516.671995221453471, 216.5711338223802045 ) ) ;
#34229 = CARTESIAN_POINT ( 'NONE',  ( 10.44647102983249987, 1451.860058722380018, 207.7484592784610129 ) ) ;
#34230 = CARTESIAN_POINT ( 'NONE',  ( -10.66758891619999972, 1391.248054696180134, 215.3132018404290022 ) ) ;
#34231 = CARTESIAN_POINT ( 'NONE',  ( -99.64292198833310010, 1384.873041396320104, 296.2006670694589729 ) ) ;
#34232 = ORIENTED_EDGE ( 'NONE', *, *, #89960, .F. ) ;
#34233 = CARTESIAN_POINT ( 'NONE',  ( 5.776491095245000373, 1516.858301627840092, 203.3390965304970166 ) ) ;
#34234 = CARTESIAN_POINT ( 'NONE',  ( -0.7402208985179988820, 1516.992029636990083, 209.8751463226419958 ) ) ;
#34235 = ORIENTED_EDGE ( 'NONE', *, *, #75460, .T. ) ;
#34236 = CARTESIAN_POINT ( 'NONE',  ( 11.75600116617299840, 1426.829850492249989, 145.4901315597400071 ) ) ;
#34237 = AXIS2_PLACEMENT_3D ( 'NONE', #110010, #40043, #91555 ) ;
#34238 = CARTESIAN_POINT ( 'NONE',  ( 19.76363181259999990, 1497.691518898830054, 228.7599396882980045 ) ) ;
#34239 = ORIENTED_EDGE ( 'NONE', *, *, #14729, .F. ) ;
#34240 = CARTESIAN_POINT ( 'NONE',  ( -13.35004134540000109, 1415.296882282229944, 221.1257189973979962 ) ) ;
#34241 = ADVANCED_FACE ( 'NONE', ( #42852, #110597 ), #33321, .F. ) ;
#34242 = CARTESIAN_POINT ( 'NONE',  ( -11.35814853775019984, 1432.342270311689845, 151.4015281471440062 ) ) ;
#34243 = CARTESIAN_POINT ( 'NONE',  ( -4.329341231296617742, 1515.068899845850183, 212.0800850781405131 ) ) ;
#34244 = AXIS2_PLACEMENT_3D ( 'NONE', #9771, #60193, #35525 ) ;
#34245 = CARTESIAN_POINT ( 'NONE',  ( -3.672026810689013931, 1488.783744143340982, 219.3790594625757819 ) ) ;
#34246 = CARTESIAN_POINT ( 'NONE',  ( -4.869499518229999602, 1422.270630277530017, 184.7950624201980077 ) ) ;
#34247 = CARTESIAN_POINT ( 'NONE',  ( 10.75512883408480036, 1470.091788688690031, 207.0349106889550228 ) ) ;
#34248 = CARTESIAN_POINT ( 'NONE',  ( -10.38017158409999929, 1471.876108471190037, 207.0077964733490035 ) ) ;
#34249 = CARTESIAN_POINT ( 'NONE',  ( -10.01745403176274785, 1410.637555081950040, 188.4336630067121234 ) ) ;
#34250 = CARTESIAN_POINT ( 'NONE',  ( -14.12491790450000018, 1379.654561017129936, 208.1472458495740057 ) ) ;
#34251 = CARTESIAN_POINT ( 'NONE',  ( 22.63922376101739786, 1413.302736438429747, 206.1995960539140356 ) ) ;
#34253 = CARTESIAN_POINT ( 'NONE',  ( -6.754078978114156584, 1519.913060387329779, 184.4732361498326156 ) ) ;
#34252 = DIRECTION ( 'NONE',  ( -1.755985294532469921E-16, 1.000000000000000000, -1.338183447452831989E-16 ) ) ;
#34254 = CARTESIAN_POINT ( 'NONE',  ( -4.649812432218794811, 1423.695263795027358, 184.4549038447098610 ) ) ;
#34255 = CARTESIAN_POINT ( 'NONE',  ( -5.311690196159160493, 1500.891276851109978, 229.7589207481180154 ) ) ;
#34256 = ORIENTED_EDGE ( 'NONE', *, *, #77742, .F. ) ;
#34257 = AXIS2_PLACEMENT_3D ( 'NONE', #93768, #318, #101618 ) ;
#34258 = CARTESIAN_POINT ( 'NONE',  ( 18.27238427227369755, 1424.505937855529965, 223.6578119888600042 ) ) ;
#34259 = CARTESIAN_POINT ( 'NONE',  ( 0.8535652294838238507, 1516.694903845322870, 216.8350831329449306 ) ) ;
#34260 = CARTESIAN_POINT ( 'NONE',  ( -2.902680970014407613, 1484.524336014886785, 183.2878275774386339 ) ) ;
#34261 = CARTESIAN_POINT ( 'NONE',  ( -14.60558113189999929, 1415.677402202029953, 212.8314178170890045 ) ) ;
#34263 = ORIENTED_EDGE ( 'NONE', *, *, #24188, .F. ) ;
#34262 = CARTESIAN_POINT ( 'NONE',  ( 0.6417514479943100536, 1515.135428326259898, 204.7942468399390066 ) ) ;
#34264 = CARTESIAN_POINT ( 'NONE',  ( 1.323582945269999867, 1489.466620109829819, 186.9612537963979833 ) ) ;
#34265 = FACE_OUTER_BOUND ( 'NONE', #85279, .T. ) ;
#34266 = CARTESIAN_POINT ( 'NONE',  ( -11.16757872979999888, 1425.149737177430097, 145.1863048323980081 ) ) ;
#34267 = DIRECTION ( 'NONE',  ( -0.4090087482554383147, 0.000000000000000000, -0.9125304618753937724 ) ) ;
#34268 = CARTESIAN_POINT ( 'NONE',  ( -10.90851772964620103, 1461.964075312410159, 210.6186257616180058 ) ) ;
#34269 = DIRECTION ( 'NONE',  ( 0.000000000000000000, 0.000000000000000000, -1.000000000000000000 ) ) ;
#34270 = CARTESIAN_POINT ( 'NONE',  ( -5.838032942621479648, 1427.197080586870015, 201.8313282331189953 ) ) ;
#34271 = CARTESIAN_POINT ( 'NONE',  ( -16.53923917176500069, 1512.406775501100128, 221.4068228132670129 ) ) ;
#34272 = CARTESIAN_POINT ( 'NONE',  ( 13.12523828760000022, 1473.126683452290081, 192.9578767172990013 ) ) ;
#34273 = EDGE_CURVE ( 'NONE', #77021, #55879, #66418, .T. ) ;
#34275 = CARTESIAN_POINT ( 'NONE',  ( -10.28629954290000015, 1479.827768412789965, 212.1118048706690047 ) ) ;
#34274 = CARTESIAN_POINT ( 'NONE',  ( -19.89091575900000208, 1495.374792094930172, 228.3689221276979993 ) ) ;
#34276 = CARTESIAN_POINT ( 'NONE',  ( -16.32629271558399608, 1459.450551812079993, 228.9510548132139718 ) ) ;
#34277 = ORIENTED_EDGE ( 'NONE', *, *, #67242, .T. ) ;
#34278 = CARTESIAN_POINT ( 'NONE',  ( 3.252530615595000452, 1516.827328999679821, 206.2418890071470230 ) ) ;
#34279 = CARTESIAN_POINT ( 'NONE',  ( 21.85509849029999785, 1410.191647020929850, 266.7712709411979972 ) ) ;
#34280 =( GEOMETRIC_REPRESENTATION_CONTEXT ( 3 ) GLOBAL_UNCERTAINTY_ASSIGNED_CONTEXT ( ( #28917 ) ) GLOBAL_UNIT_ASSIGNED_CONTEXT ( ( #80223, #71870, #80776 ) ) REPRESENTATION_CONTEXT ( 'NONE', 'WORKASPACE' ) );
#34281 = CARTESIAN_POINT ( 'NONE',  ( 24.25229055349999996, 1435.770029208010101, 138.8216067376980050 ) ) ;
#34282 = CARTESIAN_POINT ( 'NONE',  ( 18.16373175749999902, 1430.308745069530005, 192.1900383825980043 ) ) ;
#34283 = CARTESIAN_POINT ( 'NONE',  ( -0.1466225642774790228, 1507.635109844429962, 237.3673378143610080 ) ) ;
#34284 = FACE_OUTER_BOUND ( 'NONE', #1321, .T. ) ;
#34285 = DIRECTION ( 'NONE',  ( 0.4258765256105080388, -0.006533365793910755025, 0.9047577024072938068 ) ) ;
#34286 = CARTESIAN_POINT ( 'NONE',  ( -33.93019615848938031, 1524.726013923371283, 220.5829544587965927 ) ) ;
#34287 = CARTESIAN_POINT ( 'NONE',  ( -15.25967915520000062, 1416.619611601430051, 206.0080059597690081 ) ) ;
#34288 = CARTESIAN_POINT ( 'NONE',  ( -13.64317476579999955, 1445.682466854349968, 188.2845503314979965 ) ) ;
#34289 = CARTESIAN_POINT ( 'NONE',  ( -2.917647860963519690, 1485.453250951370137, 197.5824647639669820 ) ) ;
#34290 = CARTESIAN_POINT ( 'NONE',  ( 17.84338787571921614, 1512.187213306747481, 180.3600277896298110 ) ) ;
#34291 = CARTESIAN_POINT ( 'NONE',  ( 4.301461580539999829, 1407.800349814830042, 270.1336327149980434 ) ) ;
#34292 = ORIENTED_EDGE ( 'NONE', *, *, #34980, .F. ) ;
#34293 = CARTESIAN_POINT ( 'NONE',  ( 1.456838540400960058, 1499.011618624379935, 181.4667026936230059 ) ) ;
#34294 = CARTESIAN_POINT ( 'NONE',  ( -13.98332703483129968, 1409.401368927429758, 203.8662359848739811 ) ) ;
#34295 = CARTESIAN_POINT ( 'NONE',  ( 10.52837420263239920, 1481.199010226290284, 208.2608686310830137 ) ) ;
#34296 = CARTESIAN_POINT ( 'NONE',  ( 2.562340869413359812, 1517.151704408390060, 221.9545077427458182 ) ) ;
#34297 = VECTOR ( 'NONE', #87633, 1000.000000000000000 ) ;
#34298 = CARTESIAN_POINT ( 'NONE',  ( -21.81807642700000116, 1471.495927914430240, 269.1143084626980340 ) ) ;
#34299 = CARTESIAN_POINT ( 'NONE',  ( 1.358935478622729898, 1412.145631141479953, 232.7165187772180275 ) ) ;
#34300 = CARTESIAN_POINT ( 'NONE',  ( -10.67458942334280003, 1390.939239166159950, 215.3172498179779666 ) ) ;
#34301 = CARTESIAN_POINT ( 'NONE',  ( -24.12916442465748545, 1444.472920415359567, 211.7107983591160405 ) ) ;
#34302 = CARTESIAN_POINT ( 'NONE',  ( -67.78736533448140733, 1384.668913691839862, 292.4440920854070214 ) ) ;
#34303 = CARTESIAN_POINT ( 'NONE',  ( -16.95405163836110063, 1384.945347557320019, 200.9633990510879755 ) ) ;
#34304 = CARTESIAN_POINT ( 'NONE',  ( -3.346415545340000186, 1442.759383208520148, 155.7539078627980018 ) ) ;
#34305 = DIRECTION ( 'NONE',  ( 0.000000000000000000, 0.000000000000000000, -1.000000000000000000 ) ) ;
#34306 = CARTESIAN_POINT ( 'NONE',  ( -17.19739463999666285, 1525.960063244516959, 181.9833109756550584 ) ) ;
#34307 = CARTESIAN_POINT ( 'NONE',  ( -2.664535259099999805E-15, 1422.937291763169924, 209.1218459616989946 ) ) ;
#34308 = ADVANCED_FACE ( 'NONE', ( #85377 ), #22208, .F. ) ;
#34309 = CARTESIAN_POINT ( 'NONE',  ( -22.62661505969999709, 1409.703199196130072, 206.8548854524279932 ) ) ;
#34310 = ADVANCED_FACE ( 'NONE', ( #91261 ), #92923, .F. ) ;
#34311 = ADVANCED_FACE ( 'NONE', ( #104626 ), #26249, .F. ) ;
#34312 = CARTESIAN_POINT ( 'NONE',  ( 14.66127812029999866, 1415.087974639930053, 199.4957085038979869 ) ) ;
#34313 = VECTOR ( 'NONE', #16215, 1000.000000000000114 ) ;
#34314 = CARTESIAN_POINT ( 'NONE',  ( 5.009762976649999366, 1485.882962529690076, 218.6550994417989671 ) ) ;
#34315 = CARTESIAN_POINT ( 'NONE',  ( 4.482879682490001017, 1422.721247146459973, 194.3586833993989842 ) ) ;
#34316 = EDGE_CURVE ( 'NONE', #79273, #63621, #96858, .T. ) ;
#34317 = CARTESIAN_POINT ( 'NONE',  ( 0.8251472201360000591, 1438.194204504490017, 150.6035180695979818 ) ) ;
#34318 = EDGE_CURVE ( 'NONE', #11716, #90525, #36869, .T. ) ;
#34319 = CARTESIAN_POINT ( 'NONE',  ( 11.78523210350000028, 1435.905840746989952, 225.6005139738989840 ) ) ;
#34320 = CARTESIAN_POINT ( 'NONE',  ( 17.12670006681583246, 1524.374142163904253, 180.9415281674935443 ) ) ;
#34321 = CARTESIAN_POINT ( 'NONE',  ( 10.59813991437289893, 1477.524080021249802, 229.9254213493549912 ) ) ;
#34323 = CARTESIAN_POINT ( 'NONE',  ( -12.26989794379589860, 1378.707268951720152, 210.4706525970389919 ) ) ;
#34322 = CARTESIAN_POINT ( 'NONE',  ( -21.99779640679999915, 1409.845345977029865, 211.9582514417379855 ) ) ;
#34324 = CARTESIAN_POINT ( 'NONE',  ( 11.70097560617689858, 1426.719468243919891, 141.5896315292509939 ) ) ;
#34325 = CARTESIAN_POINT ( 'NONE',  ( 9.764985867364520900, 1436.011985270369905, 210.2792758222440170 ) ) ;
#34326 = CARTESIAN_POINT ( 'NONE',  ( -10.69722738760000169, 1491.094497843389945, 211.6881357245790127 ) ) ;
#34327 = CARTESIAN_POINT ( 'NONE',  ( 9.159631730552030504, 1450.106319786690165, 204.1877701249059953 ) ) ;
#34328 = EDGE_CURVE ( 'NONE', #49199, #22340, #103952, .T. ) ;
#34329 = CARTESIAN_POINT ( 'NONE',  ( -16.56954065640239904, 1507.336002802359872, 224.6960143935069993 ) ) ;
#34330 = B_SPLINE_CURVE_WITH_KNOTS ( 'NONE', 5,
 ( #35798, #3326, #11697, #45869, #29054, #95702 ),
 .UNSPECIFIED., .F., .F.,
 ( 6, 6 ),
 ( -1.469182821640000025, -2.166508562106983504E-06 ),
 .UNSPECIFIED. ) ;
#34331 = CARTESIAN_POINT ( 'NONE',  ( 5.776491095245000373, 1516.858301627840092, 203.3390965304970166 ) ) ;
#34332 = CARTESIAN_POINT ( 'NONE',  ( -9.119309862993969062, 1398.183652844645621, 218.3944131779407201 ) ) ;
#34333 = CARTESIAN_POINT ( 'NONE',  ( -3.524418834340278472, 1440.781073485925162, 156.7014001434145598 ) ) ;
#34334 = DIRECTION ( 'NONE',  ( -5.980589973904019347E-17, 1.000000000000000000, -1.736889445713099699E-16 ) ) ;
#34335 = CARTESIAN_POINT ( 'NONE',  ( 1.413944454890000202, 1507.072543608730030, 236.8050756195980284 ) ) ;
#34336 = CARTESIAN_POINT ( 'NONE',  ( -1.906499846882070084E-08, 1508.551704408389924, 216.6218459511670176 ) ) ;
#34338 = ORIENTED_EDGE ( 'NONE', *, *, #56744, .F. ) ;
#34337 = CARTESIAN_POINT ( 'NONE',  ( -63.32122928202920065, 1379.740723965109964, 271.7760642072729524 ) ) ;
#34339 = ORIENTED_EDGE ( 'NONE', *, *, #33145, .T. ) ;
#34340 = CARTESIAN_POINT ( 'NONE',  ( 11.97251399677129946, 1433.655889273449930, 150.1647575922700071 ) ) ;
#34341 = CARTESIAN_POINT ( 'NONE',  ( 20.88378052024278020, 1525.556089352344770, 184.5817669221027586 ) ) ;
#34342 = EDGE_LOOP ( 'NONE', ( #58219, #37217, #106253, #67614 ) ) ;
#34343 = CARTESIAN_POINT ( 'NONE',  ( -0.0002531825210758750105, 1396.493310238344520, 221.5300458565427562 ) ) ;
#34344 = CARTESIAN_POINT ( 'NONE',  ( -21.59613672980000132, 1509.442267788030222, 191.6826760664980043 ) ) ;
#34345 = LINE ( 'NONE', #85282, #17624 ) ;
#34346 =( BOUNDED_CURVE ( )  B_SPLINE_CURVE ( 3, ( #6207, #4570, #14603, #22426 ),
 .UNSPECIFIED., .F., .F. ) 
 B_SPLINE_CURVE_WITH_KNOTS ( ( 4, 4 ),
 ( 2.436781329611989122, 3.141592653589793116 ),
 .UNSPECIFIED. ) 
 CURVE ( )  GEOMETRIC_REPRESENTATION_ITEM ( )  RATIONAL_B_SPLINE_CURVE ( ( 1.000000000000000000, 0.9590300661663093695, 0.9590300661663093695, 1.000000000000000000 ) ) 
 REPRESENTATION_ITEM ( '' )  );
#34348 = CARTESIAN_POINT ( 'NONE',  ( 2.286265947080000416, 1427.727383903629971, 112.4493539157979995 ) ) ;
#34347 = DIRECTION ( 'NONE',  ( -1.755985294532469921E-16, 1.000000000000000000, -1.338183447452831989E-16 ) ) ;
#34349 = CARTESIAN_POINT ( 'NONE',  ( 18.53962229561609831, 1488.413181566670119, 229.1505926759119802 ) ) ;
#34350 = EDGE_CURVE ( 'NONE', #57276, #76827, #9566, .T. ) ;
#34351 = AXIS2_PLACEMENT_3D ( 'NONE', #14067, #76606, #31428 ) ;
#34352 = CARTESIAN_POINT ( 'NONE',  ( 2.046362623379999857, 1488.173483295229971, 182.0543892500980121 ) ) ;
#34353 = CARTESIAN_POINT ( 'NONE',  ( -0.3142747835549999924, 1415.426210663629945, 191.6391921992979803 ) ) ;
#34354 = DIRECTION ( 'NONE',  ( 1.755985294532464991E-16, -1.000000000000000000, 1.338183447452830017E-16 ) ) ;
#34355 = CARTESIAN_POINT ( 'NONE',  ( 7.337793712495000342, 1517.145312756229941, 211.9940546803969994 ) ) ;
#34357 = ADVANCED_FACE ( 'NONE', ( #70511 ), #55706, .T. ) ;
#34356 = CARTESIAN_POINT ( 'NONE',  ( 10.51790268500719883, 1480.734060164550101, 208.3818872041500185 ) ) ;
#34358 = CARTESIAN_POINT ( 'NONE',  ( 13.86388155043169945, 1415.301705643500100, 197.4576564492959960 ) ) ;
#34359 = CARTESIAN_POINT ( 'NONE',  ( 11.85132026249999981, 1431.246777428639916, 150.3007239271979927 ) ) ;
#34360 = CARTESIAN_POINT ( 'NONE',  ( 6.648850764465000118, 1513.600111798339867, 201.6549557653970055 ) ) ;
#34361 = ORIENTED_EDGE ( 'NONE', *, *, #6913, .F. ) ;
#34362 = CARTESIAN_POINT ( 'NONE',  ( 14.36662627577019968, 1436.257422054949984, 150.0160098068969887 ) ) ;
#34364 = ORIENTED_EDGE ( 'NONE', *, *, #105536, .T. ) ;
#34363 = B_SPLINE_CURVE_WITH_KNOTS ( 'NONE', 3,
 ( #36573, #86971, #26504, #52295, #25941, #60700, #94823, #87543, #86420, #9710, #52845, #1327, #10831, #45003, #104883, #28173, #62360, #106531, #12471, #55051, #47185, #81864, #107630, #97045, #39323, #46654, #82435, #90820, #48292, #37676, #63465, #38763, #105997, #71325, #21392, #64006, #72400, #5165, #99205, #54511, #80786, #13546, #105439, #73494, #21935, #97584, #4093, #80234, #89179, #29273 ),
 .UNSPECIFIED., .F., .F.,
 ( 4, 2, 2, 1, 1, 2, 2, 2, 2, 1, 1, 1, 2, 2, 2, 2, 1, 1, 1, 2, 2, 2, 2, 1, 1, 1, 1, 2, 2, 2, 4 ),
 ( 0.000000000000000000, 0.1249999999980263010, 0.1874999999970458908, 0.2187499999965475395, 0.2343749999963077590, 0.2421874999962046471, 0.2499999999961015629, 0.3749999999939591100, 0.4374999999929196082, 0.4687499999924066851, 0.4843749999921764249, 0.4921874999920613503, 0.4960937499919773064, 0.4999999999918932625, 0.6249999999912395632, 0.6874999999909128245, 0.7187499999907493997, 0.7343749999906674653, 0.7421874999906323822, 0.7460937499905788695, 0.7499999999905252457, 0.8124999999901119097, 0.8437499999898635528, 0.8593749999897393188, 0.8671874999896397318, 0.8710937499896164171, 0.8730468749896052039, 0.8740234374895728964, 0.8749999999895405889, 0.9374999999947704055, 1.000000000000000000 ),
 .UNSPECIFIED. ) ;
#34365 = EDGE_CURVE ( 'NONE', #12028, #72956, #75038, .T. ) ;
#34366 = EDGE_LOOP ( 'NONE', ( #7931, #49399, #103898, #66972 ) ) ;
#34367 = CARTESIAN_POINT ( 'NONE',  ( 13.05599175049793281, 1444.836491748568505, 169.4127969366490731 ) ) ;
#34368 = CARTESIAN_POINT ( 'NONE',  ( -2.855376345160000273, 1466.858753905630010, 235.0846608803980189 ) ) ;
#34369 = DIRECTION ( 'NONE',  ( 0.000000000000000000, 0.000000000000000000, 1.000000000000000000 ) ) ;
#34370 = CARTESIAN_POINT ( 'NONE',  ( -3.260357166894999992, 1517.133889586189980, 216.8465783791270098 ) ) ;
#34371 = CARTESIAN_POINT ( 'NONE',  ( -7.892149748326827030, 1512.076650117315467, 212.1052314332001743 ) ) ;
#34372 = EDGE_CURVE ( 'NONE', #46666, #33840, #76412, .T. ) ;
#34373 = CARTESIAN_POINT ( 'NONE',  ( -18.78398581570814940, 1444.618302659428537, 213.1331773526644611 ) ) ;
#34374 = CARTESIAN_POINT ( 'NONE',  ( -58.44481929797314734, 1379.719446205599070, 257.8613692807373923 ) ) ;
#34375 = CARTESIAN_POINT ( 'NONE',  ( -7.567621161420000853, 1380.366160257679894, 208.3364483334960084 ) ) ;
#34376 = ORIENTED_EDGE ( 'NONE', *, *, #53098, .F. ) ;
#34377 = CARTESIAN_POINT ( 'NONE',  ( -4.625359562974999506, 1517.025470194390209, 206.6416589153869836 ) ) ;
#34378 = ORIENTED_EDGE ( 'NONE', *, *, #37865, .F. ) ;
#34379 = CARTESIAN_POINT ( 'NONE',  ( -105.0114562248090095, 1379.360439012370080, 304.5078138772479974 ) ) ;
#34380 = CARTESIAN_POINT ( 'NONE',  ( -18.65451756079999868, 1507.632629717229975, 229.7110761602979778 ) ) ;
#34381 = VERTEX_POINT ( 'NONE', #55900 ) ;
#34382 = CARTESIAN_POINT ( 'NONE',  ( -2.923521387370000113, 1410.394928919130280, 186.6127609212979905 ) ) ;
#34383 = CARTESIAN_POINT ( 'NONE',  ( 8.038901785834998037, 1514.330398624150121, 216.0318990019970045 ) ) ;
#34385 = ORIENTED_EDGE ( 'NONE', *, *, #79857, .F. ) ;
#34384 = CARTESIAN_POINT ( 'NONE',  ( -11.04992432776889899, 1414.913526854310021, 195.9912987695080346 ) ) ;
#34386 = CARTESIAN_POINT ( 'NONE',  ( 23.65786361689999850, 1434.694201751649871, 215.1063102513179786 ) ) ;
#34387 = CARTESIAN_POINT ( 'NONE',  ( -20.20959865099510111, 1511.187213306747708, 182.0120230947222524 ) ) ;
#34388 = CARTESIAN_POINT ( 'NONE',  ( -96.24310955420000369, 1384.607824056739901, 310.5744048422590140 ) ) ;
#34389 = SPHERICAL_SURFACE ( 'NONE', #69628, 2.000000000000000000 ) ;
#34390 = CARTESIAN_POINT ( 'NONE',  ( 21.61975802671112135, 1524.130440953581001, 183.7557183496562061 ) ) ;
#34391 = CARTESIAN_POINT ( 'NONE',  ( -3.449777353855000062, 1516.974592746400049, 214.1332139170270068 ) ) ;
#34392 = CARTESIAN_POINT ( 'NONE',  ( -3.472682794772799841, 1428.654985552910148, 200.4267480108129860 ) ) ;
#34393 = EDGE_CURVE ( 'NONE', #29176, #84984, #43107, .T. ) ;
#34394 = CARTESIAN_POINT ( 'NONE',  ( -20.60407645530000309, 1508.351959126529891, 190.1129144765980072 ) ) ;
#34395 = DIRECTION ( 'NONE',  ( -0.9455185755993178454, 0.000000000000000000, 0.3255681544571537578 ) ) ;
#34396 = CARTESIAN_POINT ( 'NONE',  ( 7.338753830235000386, 1517.184383877180153, 211.4127322367170052 ) ) ;
#34397 = EDGE_CURVE ( 'NONE', #65085, #65905, #105732, .T. ) ;
#34398 = CARTESIAN_POINT ( 'NONE',  ( 14.55268257189999836, 1410.361135901630178, 191.4983566902979817 ) ) ;
#34399 = CARTESIAN_POINT ( 'NONE',  ( -16.74093840945409539, 1486.115613468081847, 187.5028501039167281 ) ) ;
#34401 = EDGE_LOOP ( 'NONE', ( #35444, #84732, #32754, #11992 ) ) ;
#34400 = CARTESIAN_POINT ( 'NONE',  ( -63.53051246150000253, 1388.282315597190063, 254.4959482329590230 ) ) ;
#34402 = CARTESIAN_POINT ( 'NONE',  ( -73.70661426834119823, 1385.011922779980068, 298.8812608434159870 ) ) ;
#34403 = CARTESIAN_POINT ( 'NONE',  ( 13.60517974880000125, 1473.691213157429956, 264.8398836597979766 ) ) ;
#34404 = CARTESIAN_POINT ( 'NONE',  ( 1.610433614691386461, 1452.674093572039055, 183.5081501456340902 ) ) ;
#34405 = CARTESIAN_POINT ( 'NONE',  ( -7.583791944165000132, 1511.751588929339960, 211.4475770739170173 ) ) ;
#34406 = CARTESIAN_POINT ( 'NONE',  ( -7.334500520190000650, 1507.579365412929974, 235.5537206881979841 ) ) ;
#34407 = CARTESIAN_POINT ( 'NONE',  ( -24.04315183079999940, 1445.026065454899936, 213.4541038299180116 ) ) ;
#34408 = EDGE_CURVE ( 'NONE', #43746, #49156, #41709, .T. ) ;
#34410 = CARTESIAN_POINT ( 'NONE',  ( 17.14579715356120104, 1409.552403581870067, 222.3181863344280202 ) ) ;
#34409 = CARTESIAN_POINT ( 'NONE',  ( 1.708092266164999984, 1516.523379810429788, 216.8305916180169959 ) ) ;
#34411 = CARTESIAN_POINT ( 'NONE',  ( -9.105402976021849781, 1449.059321480550125, 210.1353435409779991 ) ) ;
#34412 = CARTESIAN_POINT ( 'NONE',  ( -109.3456642170559974, 1383.364683205310030, 311.1052009544930002 ) ) ;
#34413 = VERTEX_POINT ( 'NONE', #107377 ) ;
#34414 = CARTESIAN_POINT ( 'NONE',  ( 2.288357407604999949, 1517.116049120239950, 203.3334095979369920 ) ) ;
#34415 = CARTESIAN_POINT ( 'NONE',  ( 0.1075185588789999980, 1406.066315318429815, 269.0456997844980265 ) ) ;
#34416 = CIRCLE ( 'NONE', #61237, 2.000000000000000000 ) ;
#34417 = DIRECTION ( 'NONE',  ( 0.000000000000000000, 0.000000000000000000, 1.000000000000000000 ) ) ;
#34418 = CARTESIAN_POINT ( 'NONE',  ( 13.15345997939999911, 1428.696580737029990, 223.2895104518979963 ) ) ;
#34419 = CARTESIAN_POINT ( 'NONE',  ( -8.554652906407122614, 1461.548920753501307, 204.5271286160454167 ) ) ;
#34420 = CARTESIAN_POINT ( 'NONE',  ( 21.02847232690000467, 1496.614785848189968, 206.9633919846189940 ) ) ;
#34421 = CARTESIAN_POINT ( 'NONE',  ( 12.49401126939999962, 1451.800774058590150, 193.6953293048989906 ) ) ;
#34422 = CARTESIAN_POINT ( 'NONE',  ( 26.79407919707900021, 1435.433162376700011, 135.2875019197180109 ) ) ;
#34423 = EDGE_CURVE ( 'NONE', #49356, #75164, #13849, .T. ) ;
#34424 = CARTESIAN_POINT ( 'NONE',  ( 34.85401832400309274, 1450.338014512889913, 136.2298619501380017 ) ) ;
#34425 = CARTESIAN_POINT ( 'NONE',  ( -42.00585553703391639, 1454.281673901052727, 269.0755534770359532 ) ) ;
#34426 = CARTESIAN_POINT ( 'NONE',  ( -2.096701719259999930, 1429.602646753990030, 200.3590733686490069 ) ) ;
#34427 = CARTESIAN_POINT ( 'NONE',  ( 13.79910387159999807, 1508.398165315730012, 185.5292457990980211 ) ) ;
#34428 = CARTESIAN_POINT ( 'NONE',  ( 10.86111838972819932, 1480.525208337349795, 210.6924698787690033 ) ) ;
#34429 = CARTESIAN_POINT ( 'NONE',  ( -20.70484064406419122, 1525.907212628473644, 185.0411015109856692 ) ) ;
#34430 = CARTESIAN_POINT ( 'NONE',  ( -10.33299300126450149, 1447.717326489380184, 209.8084994042759774 ) ) ;
#34431 = ORIENTED_EDGE ( 'NONE', *, *, #20758, .T. ) ;
#34433 = EDGE_CURVE ( 'NONE', #63865, #28394, #61771, .T. ) ;
#34432 = CARTESIAN_POINT ( 'NONE',  ( 1.623075365390000080, 1428.602351821930142, 149.4837496357980058 ) ) ;
#34434 = CARTESIAN_POINT ( 'NONE',  ( 2.109745707098269918, 1456.459472160349833, 219.5317045544409780 ) ) ;
#34435 = CARTESIAN_POINT ( 'NONE',  ( 19.57175081105178194, 1452.229599788707219, 144.4156370992074585 ) ) ;
#34436 = CARTESIAN_POINT ( 'NONE',  ( 16.33822231007999903, 1488.657264317530007, 188.6886238127860054 ) ) ;
#34437 = CARTESIAN_POINT ( 'NONE',  ( 11.44793483447996074, 1425.801405795868959, 139.0695979703967851 ) ) ;
#34439 = FACE_OUTER_BOUND ( 'NONE', #40703, .T. ) ;
#34438 = CARTESIAN_POINT ( 'NONE',  ( -2.370970874524634286, 1427.002265528474027, 134.0999999980980135 ) ) ;
#34440 = CARTESIAN_POINT ( 'NONE',  ( -28.83583423950000224, 1509.587522268929888, 209.1203260760459841 ) ) ;
#34441 = CARTESIAN_POINT ( 'NONE',  ( 9.722209888710001024, 1428.114071763990069, 212.2005363753689835 ) ) ;
#34442 = CARTESIAN_POINT ( 'NONE',  ( -7.330468918998392702, 1514.095142040229348, 217.2263680036883784 ) ) ;
#34443 = CARTESIAN_POINT ( 'NONE',  ( 42.85028971309680657, 1440.913025295369835, 270.2009442048760093 ) ) ;
#34444 = CARTESIAN_POINT ( 'NONE',  ( -10.59239855707533984, 1451.301507702100480, 152.0626276528745393 ) ) ;
#34445 = CARTESIAN_POINT ( 'NONE',  ( -5.787664699130000479, 1484.577383496389984, 199.2118460601089964 ) ) ;
#34446 = CARTESIAN_POINT ( 'NONE',  ( 25.31932687029999940, 1435.570944935079979, 136.4448942406980052 ) ) ;
#34447 = EDGE_CURVE ( 'NONE', #47729, #106390, #39631, .T. ) ;
#34448 = CARTESIAN_POINT ( 'NONE',  ( 11.90000415720300175, 1434.913060496859998, 147.6452464505769910 ) ) ;
#34449 = ORIENTED_EDGE ( 'NONE', *, *, #39255, .T. ) ;
#34450 = CARTESIAN_POINT ( 'NONE',  ( -16.44160288201669928, 1409.512366239009907, 225.1669717104299764 ) ) ;
#34451 = EDGE_CURVE ( 'NONE', #41248, #87307, #80538, .T. ) ;
#34452 = CARTESIAN_POINT ( 'NONE',  ( 7.435066116149999793, 1441.600846913620217, 149.7516446007980164 ) ) ;
#34453 = ORIENTED_EDGE ( 'NONE', *, *, #105016, .F. ) ;
#34454 = ORIENTED_EDGE ( 'NONE', *, *, #5630, .T. ) ;
#34455 = CARTESIAN_POINT ( 'NONE',  ( 4.219439031349260461, 1446.230224802979819, 182.3842141579679890 ) ) ;
#34456 = CARTESIAN_POINT ( 'NONE',  ( 7.152679178757631817, 1516.546162712742898, 206.8624663984998904 ) ) ;
#34458 = CARTESIAN_POINT ( 'NONE',  ( -1.427750768948659932, 1457.410439390729834, 219.6702089923480230 ) ) ;
#34457 = CARTESIAN_POINT ( 'NONE',  ( 10.90929167140000011, 1426.089277454929970, 92.68786258269780376 ) ) ;
#34459 = CARTESIAN_POINT ( 'NONE',  ( 23.55538394579999917, 1409.900238729630018, 209.4988520729140191 ) ) ;
#34460 = CARTESIAN_POINT ( 'NONE',  ( 4.202765219874719627, 1425.034743857860121, 185.2477664996769988 ) ) ;
#34461 = EDGE_CURVE ( 'NONE', #79544, #96193, #37430, .T. ) ;
#34462 = CARTESIAN_POINT ( 'NONE',  ( 5.614206143365000123, 1512.939243228069927, 214.7360521135969975 ) ) ;
#34463 = CARTESIAN_POINT ( 'NONE',  ( 7.458660324640000283, 1423.927228631740036, 212.7475639799289979 ) ) ;
#34464 = CARTESIAN_POINT ( 'NONE',  ( 10.75631864630000045, 1451.138109685189875, 190.3409053448989994 ) ) ;
#34465 = CARTESIAN_POINT ( 'NONE',  ( 8.482876245789999103, 1508.704763218230028, 182.5447702950980329 ) ) ;
#34466 = CARTESIAN_POINT ( 'NONE',  ( -101.6055713061119974, 1379.039955027740234, 305.9123634697640455 ) ) ;
#34467 = CARTESIAN_POINT ( 'NONE',  ( 9.984115569220000097, 1365.258395869459946, 207.6218459616989946 ) ) ;
#34468 = EDGE_CURVE ( 'NONE', #19916, #36663, #22241, .T. ) ;
#34469 = ADVANCED_FACE ( 'NONE', ( #12210 ), #5249, .T. ) ;
#34471 = VERTEX_POINT ( 'NONE', #33406 ) ;
#34470 = CARTESIAN_POINT ( 'NONE',  ( -2.776018498009749713E-09, 1414.697267606029982, 245.4362868392339863 ) ) ;
#34472 = ORIENTED_EDGE ( 'NONE', *, *, #97405, .T. ) ;
#34473 = CARTESIAN_POINT ( 'NONE',  ( -40.71480956220000280, 1443.734648304970051, 137.1148404093979991 ) ) ;
#34474 = FACE_OUTER_BOUND ( 'NONE', #11362, .T. ) ;
#34475 = CARTESIAN_POINT ( 'NONE',  ( -0.4721143188960000292, 1471.791680839530045, 269.8654495172979750 ) ) ;
#34476 = CARTESIAN_POINT ( 'NONE',  ( -110.0628542964510075, 1384.912107091729922, 296.9513069434060526 ) ) ;
#34477 = CARTESIAN_POINT ( 'NONE',  ( -125.3156758023000918, 1368.558218059089995, 316.1375217595589220 ) ) ;
#34478 = CARTESIAN_POINT ( 'NONE',  ( 16.39250384509999847, 1431.113060387329824, 198.8961368102980316 ) ) ;
#34479 = CARTESIAN_POINT ( 'NONE',  ( 13.80546151116429954, 1434.979654507460054, 148.5370226032280243 ) ) ;
#34480 = CARTESIAN_POINT ( 'NONE',  ( 11.78824854703250047, 1522.051704408389924, 211.4132493584619965 ) ) ;
#34481 = CARTESIAN_POINT ( 'NONE',  ( 0.000000000000000000, 0.000000000000000000, 0.000000000000000000 ) ) ;
#34482 = CARTESIAN_POINT ( 'NONE',  ( -19.31623058889999811, 1475.513060387329915, 200.7139244924079833 ) ) ;
#34483 = CARTESIAN_POINT ( 'NONE',  ( 8.335050544726017918, 1369.730095592100042, 209.6218459617033432 ) ) ;
#34484 = CARTESIAN_POINT ( 'NONE',  ( -0.06979922123900890452, 1408.910622944780016, 194.4360052272290034 ) ) ;
#34485 = CARTESIAN_POINT ( 'NONE',  ( -12.05032705967369999, 1407.437450256659986, 269.2402808039070123 ) ) ;
#34486 = CARTESIAN_POINT ( 'NONE',  ( -14.49936296086660015, 1436.121868349760007, 149.8980290887049875 ) ) ;
#34487 = ORIENTED_EDGE ( 'NONE', *, *, #65149, .F. ) ;
#34488 = DIRECTION ( 'NONE',  ( 1.000000000000000000, 0.000000000000000000, 0.000000000000000000 ) ) ;
#34489 = CARTESIAN_POINT ( 'NONE',  ( 13.94587001030000017, 1445.277640235309946, 189.2991415692980013 ) ) ;
#34490 = ORIENTED_EDGE ( 'NONE', *, *, #64103, .T. ) ;
#34491 = EDGE_LOOP ( 'NONE', ( #18921, #24616, #91686, #57475 ) ) ;
#34492 = CARTESIAN_POINT ( 'NONE',  ( 4.724912038846999174, 1422.196582765026051, 184.1782025151506730 ) ) ;
#34493 = CARTESIAN_POINT ( 'NONE',  ( -21.63731731441981410, 1524.599984580802129, 183.5692477652812329 ) ) ;
#34494 = EDGE_CURVE ( 'NONE', #44794, #41855, #47080, .T. ) ;
#34495 = CARTESIAN_POINT ( 'NONE',  ( -6.937338783705000012, 1516.706638732659940, 213.7399656364970042 ) ) ;
#34496 = CARTESIAN_POINT ( 'NONE',  ( -18.66657011559999901, 1485.489288798229836, 189.3324219145979725 ) ) ;
#34497 = ORIENTED_EDGE ( 'NONE', *, *, #32311, .T. ) ;
#34498 = CARTESIAN_POINT ( 'NONE',  ( -113.4000000000000057, 1374.413060387289988, 303.4364477938589744 ) ) ;
#34499 = DIRECTION ( 'NONE',  ( -4.137698748469999823E-18, -2.750577543510000101E-14, -1.000000000000000000 ) ) ;
#34500 = CARTESIAN_POINT ( 'NONE',  ( 2.869693458934999608, 1517.070197312179971, 203.3343689375869872 ) ) ;
#34501 = CARTESIAN_POINT ( 'NONE',  ( -27.17282701799999955, 1509.164027956230029, 203.0634631091180324 ) ) ;
#34502 = CARTESIAN_POINT ( 'NONE',  ( -1.527354483230000115, 1467.880741325629970, 230.2836666281979774 ) ) ;
#34503 = CARTESIAN_POINT ( 'NONE',  ( -48.41198906934850044, 1384.612818244999971, 222.9035708180709889 ) ) ;
#34504 = CARTESIAN_POINT ( 'NONE',  ( -6.825986770030000983, 1409.091027441730148, 196.5037157050980170 ) ) ;
#34505 = CARTESIAN_POINT ( 'NONE',  ( -108.1428528709999881, 1386.591709523359896, 310.8553624892590506 ) ) ;
#34507 = EDGE_LOOP ( 'NONE', ( #48534, #45108, #3565 ) ) ;
#34506 = CARTESIAN_POINT ( 'NONE',  ( 2.149988386126029882E-09, 1405.989059316979819, 266.9611530767110139 ) ) ;
#34508 = CARTESIAN_POINT ( 'NONE',  ( 4.576312612474010777, 1517.151704408390060, 195.8593501239998318 ) ) ;
#34509 = CARTESIAN_POINT ( 'NONE',  ( 26.28495520090000070, 1469.245429234630137, 210.9605151810879988 ) ) ;
#34510 = CARTESIAN_POINT ( 'NONE',  ( 19.59849823883310194, 1467.109269350429940, 224.9849522125649912 ) ) ;
#34511 = CARTESIAN_POINT ( 'NONE',  ( -25.02785746449999849, 1436.442580334869945, 137.8071743735980021 ) ) ;
#34512 = CARTESIAN_POINT ( 'NONE',  ( 2.299014030735000436, 1516.811292230880099, 211.9858893885470081 ) ) ;
#34513 = CARTESIAN_POINT ( 'NONE',  ( -68.71730874239999309, 1379.747867717230065, 280.0458894567590278 ) ) ;
#34514 = B_SPLINE_CURVE_WITH_KNOTS ( 'NONE', 5,
 ( #91131, #91681, #32339, #64307, #58100, #109053 ),
 .UNSPECIFIED., .F., .F.,
 ( 6, 6 ),
 ( -7.104449043337727865, 0.000000000000000000 ),
 .UNSPECIFIED. ) ;
#34515 = CARTESIAN_POINT ( 'NONE',  ( -15.10917143540000041, 1420.422469564430003, 227.0222420103980028 ) ) ;
#34516 = CARTESIAN_POINT ( 'NONE',  ( 18.59085833919679942, 1477.390785077480132, 218.3860272671680320 ) ) ;
#34517 = CARTESIAN_POINT ( 'NONE',  ( -6.563915562015000482, 1517.184063036290127, 207.9975562766469750 ) ) ;
#34518 = ORIENTED_EDGE ( 'NONE', *, *, #108925, .T. ) ;
#34519 = PLANE ( 'NONE',  #31248 ) ;
#34520 = CARTESIAN_POINT ( 'NONE',  ( -5.977046268519999650, 1412.833511534230183, 231.6136271241979898 ) ) ;
#34521 = CARTESIAN_POINT ( 'NONE',  ( -22.69270896030000273, 1385.265743060869909, 222.0224438233589979 ) ) ;
#34522 = ORIENTED_EDGE ( 'NONE', *, *, #100179, .T. ) ;
#34523 = CARTESIAN_POINT ( 'NONE',  ( -15.10282486604810082, 1385.294410954709974, 219.4312743640260237 ) ) ;
#34524 = CARTESIAN_POINT ( 'NONE',  ( -3.710825917439999788, 1429.315763692190103, 201.5588532918390001 ) ) ;
#34525 = CARTESIAN_POINT ( 'NONE',  ( 12.48193344527700077, 1434.439583145440110, 149.7136235699300073 ) ) ;
#34526 = CARTESIAN_POINT ( 'NONE',  ( 16.33619008302309794, 1459.305500065469914, 229.1019625438389937 ) ) ;
#34527 = CARTESIAN_POINT ( 'NONE',  ( -21.84222827614330242, 1507.845630688500023, 226.4317230014339941 ) ) ;
#34528 = CARTESIAN_POINT ( 'NONE',  ( -2.923263677340000033, 1409.521015946229909, 186.8216734875980194 ) ) ;
#34529 = DIRECTION ( 'NONE',  ( -3.323949399211515826E-08, -0.03085664264949944391, -0.9995238204287079098 ) ) ;
#34530 = DIRECTION ( 'NONE',  ( -0.9455185755993168462, -1.224646799147349756E-16, 0.3255681544571569219 ) ) ;
#34531 = B_SPLINE_CURVE_WITH_KNOTS ( 'NONE', 3,
 ( #9454, #60430, #43620, #1628, #35205, #69948, #69392, #103503, #26805, #95669, #27355, #55895, #98416, #106811, #71621, #47482, #55340, #56433, #21688, #91122, #46946, #97858 ),
 .UNSPECIFIED., .F., .F.,
 ( 4, 2, 2, 2, 2, 2, 2, 2, 2, 2, 4 ),
 ( 0.000000000000000000, 0.2500000000000149325, 0.3750000000000188183, 0.4375000000000142109, 0.4687500000000092704, 0.5000000000000043299, 0.6250000000000006661, 0.6875000000000005551, 0.7500000000000003331, 0.8750000000000002220, 1.000000000000000000 ),
 .UNSPECIFIED. ) ;
#34533 = DIRECTION ( 'NONE',  ( -0.03489950508427384218, 0.9993908267263977852, -8.612351889057847367E-09 ) ) ;
#34532 = CARTESIAN_POINT ( 'NONE',  ( 7.333070134885000257, 1516.955859323880077, 214.9008457440070003 ) ) ;
#34534 = CARTESIAN_POINT ( 'NONE',  ( 20.17745194909999995, 1509.606869831929998, 187.6124617494980100 ) ) ;
#34535 = CARTESIAN_POINT ( 'NONE',  ( -1.710012758625000018, 1517.232977404109988, 216.8491730849570160 ) ) ;
#34536 = ORIENTED_EDGE ( 'NONE', *, *, #21249, .T. ) ;
#34537 = CARTESIAN_POINT ( 'NONE',  ( -12.78755503160000018, 1416.844618635429924, 195.3259367831980171 ) ) ;
#34538 = FACE_OUTER_BOUND ( 'NONE', #87743, .T. ) ;
#34539 = ORIENTED_EDGE ( 'NONE', *, *, #22731, .T. ) ;
#34540 = CARTESIAN_POINT ( 'NONE',  ( 5.752297360424160289, 1487.277805609919824, 203.3775840806389965 ) ) ;
#34541 = CARTESIAN_POINT ( 'NONE',  ( -113.4000000000000057, 1378.813060387289852, 304.2218459572590064 ) ) ;
#34542 = CARTESIAN_POINT ( 'NONE',  ( 2.385609062334842712, 1525.697947650493916, 177.1458780446492653 ) ) ;
#34543 = UNCERTAINTY_MEASURE_WITH_UNIT (LENGTH_MEASURE( 1.000000000000000082E-05 ), #96849, 'distance_accuracy_value', 'NONE');
#34544 = CARTESIAN_POINT ( 'NONE',  ( -9788.078716723830439, 2833.596074015639715, 1421.913706742800059 ) ) ;
#34545 = FACE_OUTER_BOUND ( 'NONE', #55003, .T. ) ;
#34546 = FACE_OUTER_BOUND ( 'NONE', #91777, .T. ) ;
#34547 = ADVANCED_FACE ( 'NONE', ( #92776 ), #75440, .T. ) ;
#34548 = CARTESIAN_POINT ( 'NONE',  ( 18.82708389389999581, 1416.254459046630018, 210.0516237558479986 ) ) ;
#34549 = FACE_OUTER_BOUND ( 'NONE', #50511, .T. ) ;
#34550 = CARTESIAN_POINT ( 'NONE',  ( 17.29882006758224122, 1523.542365884046376, 180.8528181918412940 ) ) ;
#34551 = CARTESIAN_POINT ( 'NONE',  ( -21.97938480444670262, 1506.433683733529961, 209.5040264213440082 ) ) ;
#34552 = CARTESIAN_POINT ( 'NONE',  ( 41.65366836192780653, 1440.913060353889932, 261.5143753377130338 ) ) ;
#34554 = CARTESIAN_POINT ( 'NONE',  ( -5.098507870328135461, 1391.860130066733973, 203.6232600018305163 ) ) ;
#34553 = CARTESIAN_POINT ( 'NONE',  ( -13.61671581806340114, 1417.869541547810059, 201.5013355043030003 ) ) ;
#34555 = CARTESIAN_POINT ( 'NONE',  ( 7.512750207965000371, 1509.038615934239942, 203.6084103740869864 ) ) ;
#34556 = ORIENTED_EDGE ( 'NONE', *, *, #24049, .T. ) ;
#34557 = CARTESIAN_POINT ( 'NONE',  ( 1.549551291508020068, 1416.073666489970037, 190.4139934404920211 ) ) ;
#34558 = B_SPLINE_CURVE_WITH_KNOTS ( 'NONE', 5,
 ( #38965, #64771, #12124, #54712, #56897, #107837, #88838, #80446, #97778 ),
 .UNSPECIFIED., .F., .F.,
 ( 6, 3, 6 ),
 ( 0.000000000000000000, 0.3174986011340940051, 1.000000000000000000 ),
 .UNSPECIFIED. ) ;
#34560 = CARTESIAN_POINT ( 'NONE',  ( 25.99851496269999984, 1488.583638219929981, 206.2264607038780184 ) ) ;
#34559 = B_SPLINE_CURVE_WITH_KNOTS ( 'NONE', 3,
 ( #38999, #108425, #55843, #107320, #12711, #46895, #82675, #13788, #64243, #46348, #106222, #80477, #30051, #4327, #5966, #107866, #39570, #63162, #106761, #74293, #20539, #22730, #38457, #73743, #98365, #54743, #13239, #82112, #65344, #99453, #3795, #56932, #14346, #12157, #72107, #40111, #37926, #51272, #66991, #83222, #23298, #93800, #84851, #75393, #92172, #92714, #41221, #49635, #83771, #76473, #102218, #91620, #33908, #7066, #77038, #85404, #42881, #32268, #58035, #33351, #100563, #24935, #75923, #8152, #15991, #109530, #23844, #6513, #31707, #42320, #65891, #110626, #16531, #15444, #32806, #74838, #59687, #50193, #101101, #101647, #100010, #68103, #40666, #108982, #66448, #25497, #84319, #7610, #24401, #58585, #57495 ),
 .UNSPECIFIED., .F., .F.,
 ( 4, 3, 3, 3, 3, 3, 3, 3, 3, 3, 3, 3, 3, 3, 3, 3, 3, 3, 3, 3, 3, 3, 3, 3, 3, 3, 3, 3, 3, 3, 4 ),
 ( 3.477816786180000008, 3.521729306530609893, 3.570087198783100213, 3.634106538065850156, 3.694755914534010088, 3.741217293045549841, 3.763403968410900191, 3.897984528872969978, 4.045194602964830466, 4.230054492803989596, 4.406723692118539759, 4.558577338311470051, 4.583392891433089922, 5.418196481693069444, 5.757360972090920015, 6.611787513787080073, 7.464496660483499468, 8.330048250581310043, 9.169744169958040203, 10.05608535847590090, 10.93306408244489880, 11.79628248831910042, 12.57647286233950013, 13.46759305193459966, 14.34455184101869918, 15.23010248451859994, 16.12090556754780124, 17.01703777043580246, 17.90344418320950126, 18.80443928115469987, 19.70543437909999795 ),
 .UNSPECIFIED. ) ;
#34561 = CARTESIAN_POINT ( 'NONE',  ( -27.70707313569999997, 1508.597282338030027, 210.5802476146679680 ) ) ;
#34562 = CARTESIAN_POINT ( 'NONE',  ( 8.880307795244190672, 1425.079377176630032, 195.6786652326489957 ) ) ;
#34563 = CARTESIAN_POINT ( 'NONE',  ( 4.971111079171492975, 1423.228780049225634, 194.5224207974501951 ) ) ;
#34564 = CARTESIAN_POINT ( 'NONE',  ( -113.4000000000000057, 1305.913060387289988, 304.2218459572590064 ) ) ;
#34565 = CARTESIAN_POINT ( 'NONE',  ( -2.851657392136500047, 1487.618571494400157, 219.7563995687149827 ) ) ;
#34566 = CARTESIAN_POINT ( 'NONE',  ( 13.15471227499809892, 1414.913526845469960, 198.0875664529170024 ) ) ;
#34567 = CARTESIAN_POINT ( 'NONE',  ( -55.19953390322370268, 1383.803617683420043, 271.8223894180929960 ) ) ;
#34568 = CARTESIAN_POINT ( 'NONE',  ( 7.341327630490000367, 1451.411706688430058, 153.5270054828980051 ) ) ;
#34569 = CARTESIAN_POINT ( 'NONE',  ( -27.27513993222922295, 1509.144914828118999, 212.0641667297481945 ) ) ;
#34570 = CARTESIAN_POINT ( 'NONE',  ( -2.656885837651520088, 1516.545501335879862, 201.4125211066549923 ) ) ;
#34572 = EDGE_LOOP ( 'NONE', ( #101223, #62614, #19329, #37807 ) ) ;
#34571 = FACE_OUTER_BOUND ( 'NONE', #77602, .T. ) ;
#34573 = CARTESIAN_POINT ( 'NONE',  ( -18.49678403027447970, 1458.777394600179377, 227.6249456275781995 ) ) ;
#34574 = CARTESIAN_POINT ( 'NONE',  ( -50.19412065850000459, 1382.330029049169980, 260.6313422064590100 ) ) ;
#34575 = EDGE_CURVE ( 'NONE', #76843, #63015, #57554, .T. ) ;
#34576 = CARTESIAN_POINT ( 'NONE',  ( 8.440216524157060363, 1436.746754282560005, 207.3499268363860040 ) ) ;
#34577 = VERTEX_POINT ( 'NONE', #58097 ) ;
#34578 = VERTEX_POINT ( 'NONE', #49147 ) ;
#34579 = CARTESIAN_POINT ( 'NONE',  ( 18.40016863884620335, 1509.233986100049833, 231.0028230578649868 ) ) ;
#34580 = CARTESIAN_POINT ( 'NONE',  ( -4.859106712929900596, 1457.993497594239898, 213.8797617162830136 ) ) ;
#34581 = CARTESIAN_POINT ( 'NONE',  ( 38.18239218310520044, 1438.793797181449918, 136.6214554205140246 ) ) ;
#34583 = CARTESIAN_POINT ( 'NONE',  ( -34.21122884870000291, 1452.338597683630042, 254.6787128983980040 ) ) ;
#34582 = CARTESIAN_POINT ( 'NONE',  ( 22.03740498310000007, 1506.809279316830043, 209.0321213382090093 ) ) ;
#34584 = EDGE_CURVE ( 'NONE', #18765, #59443, #68509, .T. ) ;
#34585 = CARTESIAN_POINT ( 'NONE',  ( 8.765059777696018628, 1436.630117689859844, 209.3499172591779995 ) ) ;
#34586 = CARTESIAN_POINT ( 'NONE',  ( -109.9774785470000040, 1383.769209515950024, 297.0228034975589821 ) ) ;
#34587 = EDGE_CURVE ( 'NONE', #40948, #83491, #287, .T. ) ;
#34588 = CARTESIAN_POINT ( 'NONE',  ( 41.65810716170000205, 1443.954329772089977, 135.6863066689980144 ) ) ;
#34589 = DIRECTION ( 'NONE',  ( -0.000000000000000000, -1.000000000000000000, 0.000000000000000000 ) ) ;
#34590 = CARTESIAN_POINT ( 'NONE',  ( 2.251183906690000125, 1409.929084408430072, 185.5254149766979879 ) ) ;
#34591 = CARTESIAN_POINT ( 'NONE',  ( 0.3440135400725780057, 1508.975747044360105, 179.3936242082560000 ) ) ;
#34592 = CARTESIAN_POINT ( 'NONE',  ( -5.820774585580000604, 1441.874794574320049, 154.7773490368980163 ) ) ;
#34593 = CARTESIAN_POINT ( 'NONE',  ( -9.173749095941850840, 1450.559996438570124, 208.1432995907519796 ) ) ;
#34594 = CARTESIAN_POINT ( 'NONE',  ( -14.05984932083289962, 1421.816753890520204, 203.6799934543310258 ) ) ;
#34595 = EDGE_CURVE ( 'NONE', #7480, #73940, #45080, .T. ) ;
#34596 = CARTESIAN_POINT ( 'NONE',  ( -3.284456177274770017, 1450.616812660400001, 184.8091138726430245 ) ) ;
#34597 = CARTESIAN_POINT ( 'NONE',  ( 0.7047506966600000089, 1466.680917148029948, 235.5111193182980003 ) ) ;
#34598 = ORIENTED_EDGE ( 'NONE', *, *, #85923, .T. ) ;
#34599 = CARTESIAN_POINT ( 'NONE',  ( 10.83350752517260140, 1478.706377548199953, 229.8680168337830025 ) ) ;
#34600 = CARTESIAN_POINT ( 'NONE',  ( -42.85030031610000378, 1442.445295568030133, 270.2009491864980077 ) ) ;
#34601 = CARTESIAN_POINT ( 'NONE',  ( -23.73562864992240051, 1436.101657882206609, 211.7975321304884062 ) ) ;
#34602 = CARTESIAN_POINT ( 'NONE',  ( 16.63506016420000222, 1409.493969489730034, 224.1775087685979884 ) ) ;
#34603 = CARTESIAN_POINT ( 'NONE',  ( -6.915889856759999788, 1473.238612421190055, 208.0311295872689925 ) ) ;
#34604 = CARTESIAN_POINT ( 'NONE',  ( -2.970495864810880160E-09, 1471.612866569869993, 258.0852669518579887 ) ) ;
#34605 = CARTESIAN_POINT ( 'NONE',  ( -11.15120484727999894, 1522.051704408389924, 198.0995572319588405 ) ) ;
#34606 = CARTESIAN_POINT ( 'NONE',  ( -1.549353400650000046, 1416.067629296030191, 227.8551223243979962 ) ) ;
#34607 = CARTESIAN_POINT ( 'NONE',  ( -9.828586186369999922, 1419.295296778730062, 230.7940941524979905 ) ) ;
#34608 = CARTESIAN_POINT ( 'NONE',  ( 0.4281874960050009449, 1475.888370069490065, 197.6396167722989787 ) ) ;
#34609 = CARTESIAN_POINT ( 'NONE',  ( -107.6642996119999935, 1387.006294017490063, 310.6297471052590140 ) ) ;
#34610 = CARTESIAN_POINT ( 'NONE',  ( -0.1353638497925449269, 1486.099632963759177, 181.8223423097216482 ) ) ;
#34611 = CARTESIAN_POINT ( 'NONE',  ( -5.023830084653720718, 1359.755008646306578, 210.6218459617030021 ) ) ;
#34612 = CARTESIAN_POINT ( 'NONE',  ( -45.83221320203880111, 1439.239226866460058, 266.4138812322049716 ) ) ;
#34613 = CARTESIAN_POINT ( 'NONE',  ( -3.083980574099999927, 1426.000842419329956, 185.7246353708979996 ) ) ;
#34614 = CARTESIAN_POINT ( 'NONE',  ( -7.703873474549999933, 1425.539119294559896, 205.4402485642290230 ) ) ;
#34615 = AXIS2_PLACEMENT_3D ( 'NONE', #34079, #7229, #25661 ) ;
#34616 = ORIENTED_EDGE ( 'NONE', *, *, #20010, .T. ) ;
#34617 = CARTESIAN_POINT ( 'NONE',  ( -6.556851034704999748, 1516.939568781210028, 209.1335575761840175 ) ) ;
#34618 = CARTESIAN_POINT ( 'NONE',  ( -11.74761972249999964, 1388.317445593919956, 202.1816773684589919 ) ) ;
#34619 = EDGE_CURVE ( 'NONE', #598, #53542, #107634, .T. ) ;
#34620 = CARTESIAN_POINT ( 'NONE',  ( -7.265312330176009858, 1471.117001311926515, 216.1747626545108290 ) ) ;
#34621 = CARTESIAN_POINT ( 'NONE',  ( 7.539305306222179759, 1425.626486982010192, 212.1832883622500106 ) ) ;
#34622 = CARTESIAN_POINT ( 'NONE',  ( -26.80483817892169895, 1451.972128888919997, 135.0832124891520039 ) ) ;
#34623 = ORIENTED_EDGE ( 'NONE', *, *, #265, .T. ) ;
#34624 = CARTESIAN_POINT ( 'NONE',  ( -17.59976141832330043, 1419.797097700060021, 206.6695233765389901 ) ) ;
#34626 = CARTESIAN_POINT ( 'NONE',  ( 15.80679505899999704, 1506.802866779429905, 193.5570146056979866 ) ) ;
#34625 = CARTESIAN_POINT ( 'NONE',  ( -11.48963409184570139, 1491.507525978150170, 206.8509400678860004 ) ) ;
#34627 = EDGE_CURVE ( 'NONE', #98127, #48829, #37755, .T. ) ;
#34628 = CARTESIAN_POINT ( 'NONE',  ( -15.20279581456499862, 1514.921193718960012, 223.6175349654670299 ) ) ;
#34629 = CARTESIAN_POINT ( 'NONE',  ( -22.41760174960000285, 1433.133604864480048, 211.9349560710080027 ) ) ;
#34630 = CARTESIAN_POINT ( 'NONE',  ( -12.31752010984839885, 1377.944433743309901, 209.1218459601290078 ) ) ;
#34631 = DIRECTION ( 'NONE',  ( -0.3282391760791589785, 0.000000000000000000, -0.9445946449598763284 ) ) ;
#34632 = DIRECTION ( 'NONE',  ( 5.980589973904019347E-17, -1.000000000000000000, 1.736889445713099699E-16 ) ) ;
#34633 = ORIENTED_EDGE ( 'NONE', *, *, #30262, .F. ) ;
#34634 = CARTESIAN_POINT ( 'NONE',  ( -1.808643355405459952, 1409.804319575560157, 270.0715077186459894 ) ) ;
#34635 = CARTESIAN_POINT ( 'NONE',  ( -1.133653179125000188, 1516.978425811520083, 208.3843950493249793 ) ) ;
#34636 = CARTESIAN_POINT ( 'NONE',  ( 12.56618776640000057, 1419.039214449530164, 229.1641305307979906 ) ) ;
#34637 = CARTESIAN_POINT ( 'NONE',  ( -7.512705432632942326, 1509.036904577181758, 214.8970115796141158 ) ) ;
#34639 = ORIENTED_EDGE ( 'NONE', *, *, #36962, .F. ) ;
#34638 = CARTESIAN_POINT ( 'NONE',  ( -3.005276066430000448, 1369.205039411269809, 207.6218459616989946 ) ) ;
#34640 = ORIENTED_EDGE ( 'NONE', *, *, #82333, .T. ) ;
#34641 = CARTESIAN_POINT ( 'NONE',  ( -23.61214897399189994, 1410.728070274019956, 210.3394959279470129 ) ) ;
#34642 = CARTESIAN_POINT ( 'NONE',  ( -10.51574440819999978, 1480.737039981889893, 208.3487666310030306 ) ) ;
#34643 = CARTESIAN_POINT ( 'NONE',  ( -103.4258854324899914, 1345.325269380309919, 309.6707295794789729 ) ) ;
#34644 = CARTESIAN_POINT ( 'NONE',  ( -2.205156445730000137, 1428.435894572430016, 91.31218443469779800 ) ) ;
#34645 = CARTESIAN_POINT ( 'NONE',  ( -18.92589261422770264, 1440.479205312120030, 194.3132821826760050 ) ) ;
#34646 = CARTESIAN_POINT ( 'NONE',  ( -21.44238663129999978, 1420.826072400230260, 218.5102530039179953 ) ) ;
#34647 = CARTESIAN_POINT ( 'NONE',  ( 35.50728543074449561, 1462.949734127829970, 266.4725766108469998 ) ) ;
#34648 = CARTESIAN_POINT ( 'NONE',  ( -2.694550232742050078, 1466.860812160213754, 235.1051272382491106 ) ) ;
#34649 = CARTESIAN_POINT ( 'NONE',  ( -16.05250651547230945, 1420.807636012746570, 227.0341330612096158 ) ) ;
#34650 = CARTESIAN_POINT ( 'NONE',  ( 4.027697225915000345, 1516.766397346390022, 206.2431526829570032 ) ) ;
#34651 = ORIENTED_EDGE ( 'NONE', *, *, #72050, .F. ) ;
#34652 = CARTESIAN_POINT ( 'NONE',  ( 18.61165322248807996, 1458.518385769609040, 227.4849388126852148 ) ) ;
#34653 = CARTESIAN_POINT ( 'NONE',  ( 2.093110410547600164, 1445.759653694790131, 199.2445041395880025 ) ) ;
#34654 = DIRECTION ( 'NONE',  ( 0.000000000000000000, 1.000000000000000000, 0.000000000000000000 ) ) ;
#34655 = ORIENTED_EDGE ( 'NONE', *, *, #17644, .F. ) ;
#34656 = CARTESIAN_POINT ( 'NONE',  ( 4.019735481669824750, 1515.589562461881087, 208.4997842682788303 ) ) ;
#34657 = CARTESIAN_POINT ( 'NONE',  ( 26.74463060723959984, 1450.709319562289920, 136.4676450310559801 ) ) ;
#34658 = CARTESIAN_POINT ( 'NONE',  ( -4.072632511706010483, 1508.551704408389924, 213.5435155163000047 ) ) ;
#34659 = CARTESIAN_POINT ( 'NONE',  ( -5.959427381639999410, 1385.323914143830052, 218.4985401614089824 ) ) ;
#34660 = CARTESIAN_POINT ( 'NONE',  ( 6.701092419766749408, 1517.051709179849922, 212.9150655973879793 ) ) ;
#34661 = CARTESIAN_POINT ( 'NONE',  ( 18.03239664030000000, 1409.542765553830122, 196.5032867080979884 ) ) ;
#34662 = CARTESIAN_POINT ( 'NONE',  ( 13.76936860679999874, 1443.913060387329097, 176.3340081878980641 ) ) ;
#34663 = CARTESIAN_POINT ( 'NONE',  ( 6.302973467031479871, 1409.133165070860059, 188.4343998575660066 ) ) ;
#34665 = CARTESIAN_POINT ( 'NONE',  ( -23.23380771384215393, 1433.713381843580237, 214.0813135894918560 ) ) ;
#34664 = CARTESIAN_POINT ( 'NONE',  ( -1.693092047772239983, 1443.235800395060096, 218.9922115469449864 ) ) ;
#34666 = CARTESIAN_POINT ( 'NONE',  ( 0.9766799065800328972, 1451.035295161389968, 182.3741153617290252 ) ) ;
#34667 = DIRECTION ( 'NONE',  ( -1.755985294532469921E-16, 1.000000000000000000, -1.338183447452831989E-16 ) ) ;
#34668 = CARTESIAN_POINT ( 'NONE',  ( -8.399519332060000565, 1383.604135713759888, 218.5402868535989853 ) ) ;
#34669 = LINE ( 'NONE', #35224, #51738 ) ;
#34670 = ORIENTED_EDGE ( 'NONE', *, *, #67993, .F. ) ;
#34671 = CARTESIAN_POINT ( 'NONE',  ( 11.49746945757270034, 1414.913060387399810, 220.3426859905620177 ) ) ;
#34672 = FACE_OUTER_BOUND ( 'NONE', #85385, .T. ) ;
#34673 = CARTESIAN_POINT ( 'NONE',  ( -6.968573436492549789, 1484.503278946609953, 199.4663635475509977 ) ) ;
#34674 = CARTESIAN_POINT ( 'NONE',  ( -12.37007360149999968, 1392.005019490570021, 208.3240639513470001 ) ) ;
#34675 = CARTESIAN_POINT ( 'NONE',  ( 8.405716135139408962, 1426.718822582190114, 211.2875594345169930 ) ) ;
#34676 =( BOUNDED_CURVE ( )  B_SPLINE_CURVE ( 3, ( #8783, #84936, #102294, #101737 ),
 .UNSPECIFIED., .F., .T. ) 
 B_SPLINE_CURVE_WITH_KNOTS ( ( 4, 4 ),
 ( 0.9946974666264819520, 2.146895183780889838 ),
 .UNSPECIFIED. ) 
 CURVE ( )  GEOMETRIC_REPRESENTATION_ITEM ( )  RATIONAL_B_SPLINE_CURVE ( ( 1.000000000000000000, 0.8923961322389445394, 0.8923961322389445394, 1.000000000000000000 ) ) 
 REPRESENTATION_ITEM ( '' )  );
#34677 = CARTESIAN_POINT ( 'NONE',  ( 12.58719134636679904, 1426.438815673830049, 202.7206058308819934 ) ) ;
#34678 = DIRECTION ( 'NONE',  ( -0.7071067811865475727, 1.631342908290929020E-16, -0.7071067811865475727 ) ) ;
#34679 = CARTESIAN_POINT ( 'NONE',  ( -31.70762145559999468, 1463.873751786229832, 271.1218459616979999 ) ) ;
#34680 = CARTESIAN_POINT ( 'NONE',  ( -8.860621825987630373, 1384.732557084630116, 218.6806150536880011 ) ) ;
#34681 = CARTESIAN_POINT ( 'NONE',  ( 11.76781850380000094, 1433.613318462829966, 150.8452650320979842 ) ) ;
#34682 = DIRECTION ( 'NONE',  ( -0.9999999999901589831, -4.435753632623349643E-06, 7.907321890110700723E-08 ) ) ;
#34683 = CARTESIAN_POINT ( 'NONE',  ( 12.03795434198629977, 1414.913057855109855, 197.8276465654620040 ) ) ;
#34684 = CARTESIAN_POINT ( 'NONE',  ( -9.713507356099999157, 1424.012636679030038, 192.3806507662989702 ) ) ;
#34685 = CARTESIAN_POINT ( 'NONE',  ( 9.816351554025828818, 1424.339539135469977, 198.3139274869160147 ) ) ;
#34686 = CIRCLE ( 'NONE', #66930, 1.999999999999998668 ) ;
#34687 = CARTESIAN_POINT ( 'NONE',  ( 8.441029897509530144, 1464.999488427009965, 214.2962224928130297 ) ) ;
#34688 = CARTESIAN_POINT ( 'NONE',  ( -5.874389180599999705, 1486.518516977929949, 182.2223446999980183 ) ) ;
#34689 = CARTESIAN_POINT ( 'NONE',  ( 11.91596713793072126, 1398.266359275336981, 214.3189465422430828 ) ) ;
#34690 = CARTESIAN_POINT ( 'NONE',  ( -21.82221913530460000, 1509.753632376169890, 231.7352721600289840 ) ) ;
#34691 = CARTESIAN_POINT ( 'NONE',  ( -7.604289863101939773, 1426.735970264149955, 206.0920986175900111 ) ) ;
#34692 = DIRECTION ( 'NONE',  ( 0.03489949670250328678, 0.9993908270190956511, 0.000000000000000000 ) ) ;
#34693 = CARTESIAN_POINT ( 'NONE',  ( 26.30126752569496418, 1436.707550332054780, 136.8509528689714898 ) ) ;
#34694 = CARTESIAN_POINT ( 'NONE',  ( 3.401869620952525874, 1507.778041293768410, 220.3126522683182316 ) ) ;
#34695 = CARTESIAN_POINT ( 'NONE',  ( 11.28309680436896834, 1434.414735108999821, 151.5611147865129169 ) ) ;
#34696 = CARTESIAN_POINT ( 'NONE',  ( -9.609628611790521191, 1464.248357633179921, 228.1965958858790202 ) ) ;
#34697 = CARTESIAN_POINT ( 'NONE',  ( -6.548821979184999975, 1516.688761843659904, 213.1592242262869945 ) ) ;
#34698 = CARTESIAN_POINT ( 'NONE',  ( -10.53793291988730019, 1423.359083101020133, 205.8279893113830212 ) ) ;
#34699 = CARTESIAN_POINT ( 'NONE',  ( -2.330134126739549671, 1515.219201591195770, 204.7964405199902842 ) ) ;
#34701 = VERTEX_POINT ( 'NONE', #43498 ) ;
#34700 = CARTESIAN_POINT ( 'NONE',  ( 18.12237639339999973, 1431.228556021990016, 206.5934752596589874 ) ) ;
#34702 = DIRECTION ( 'NONE',  ( -1.755985294532469921E-16, 1.000000000000000000, -1.338183447452831989E-16 ) ) ;
#34703 = CARTESIAN_POINT ( 'NONE',  ( -34.00767267269074523, 1444.324653571828776, 154.9192896682974663 ) ) ;
#34704 = ADVANCED_FACE ( 'NONE', ( #94996 ), #67938, .F. ) ;
#34705 = LINE ( 'NONE', #8948, #108668 ) ;
#34706 = CARTESIAN_POINT ( 'NONE',  ( -31.81424859196000909, 1524.964230758882877, 216.6572717949418347 ) ) ;
#34707 = DIRECTION ( 'NONE',  ( 0.6709778558543747495, 0.000000000000000000, 0.7414773880254650340 ) ) ;
#34708 = ORIENTED_EDGE ( 'NONE', *, *, #32906, .T. ) ;
#34709 = B_SPLINE_SURFACE_WITH_KNOTS ( 'NONE', 5, 5, ( 
 ( #79751, #54020, #12529, #46709, #80837, #90320 ),
 ( #81366, #3608, #4679, #104938, #21991, #37731 ),
 ( #80292, #88150, #11438, #37184, #28226, #62413 ),
 ( #19814, #45610, #107132, #62984, #97639, #71934 ),
 ( #20908, #96540, #28784, #63524, #71382, #29871 ),
 ( #47787, #13598, #3059, #72995, #56182, #21448 ),
 ( #54566, #89235, #105492, #97095, #46162, #106046 ),
 ( #2507, #29323, #88699, #55110, #11980, #30423 ),
 ( #36629, #4145, #38818, #38269, #70827, #72455 ) ),
 .UNSPECIFIED., .F., .F., .F.,
 ( 6, 3, 6 ),
 ( 6, 6 ),
 ( 2.324858856890000158, 4.970096098099999971, 7.657659707949999728 ),
 ( 0.000000000000000000, 0.5000000000000000000 ),
 .UNSPECIFIED. ) ;
#34710 = LINE ( 'NONE', #8394, #34222 ) ;
#34711 = CARTESIAN_POINT ( 'NONE',  ( -12.11525460871600046, 1391.926222251029913, 211.6230311456439779 ) ) ;
#34712 = CARTESIAN_POINT ( 'NONE',  ( -14.74831627590000060, 1414.913060387329779, 216.2126386790480126 ) ) ;
#34713 = CARTESIAN_POINT ( 'NONE',  ( 8.044362178399680374, 1504.012373259569813, 212.2082695997949884 ) ) ;
#34714 = CARTESIAN_POINT ( 'NONE',  ( -6.982434334785139640, 1435.340673196930084, 214.9240378055680196 ) ) ;
#34715 = CARTESIAN_POINT ( 'NONE',  ( -108.9994242794780774, 1382.084811078559824, 310.8140300984987334 ) ) ;
#34716 = CARTESIAN_POINT ( 'NONE',  ( -15.11179371579999930, 1419.704522818860141, 212.3545469124089777 ) ) ;
#34717 = CARTESIAN_POINT ( 'NONE',  ( -5.370514330159649852, 1422.356910281434239, 139.1416123588654727 ) ) ;
#34718 = CARTESIAN_POINT ( 'NONE',  ( -12.40942180589999921, 1391.563918014709998, 208.1819200904450042 ) ) ;
#34719 = B_SPLINE_SURFACE_WITH_KNOTS ( 'NONE', 5, 1, ( 
 ( #33592, #32520 ),
 ( #34713, #41477 ),
 ( #101897, #50438 ),
 ( #17329, #8956 ),
 ( #43129, #8397 ),
 ( #42567, #77288 ) ),
 .UNSPECIFIED., .F., .F., .F.,
 ( 6, 6 ),
 ( 2, 2 ),
 ( -9.395743872997430171E-05, 18.06269844883869879 ),
 ( 0.000000000000000000, 14.00009395743870044 ),
 .UNSPECIFIED. ) ;
#34720 = CARTESIAN_POINT ( 'NONE',  ( -86.96116641772189837, 1385.182907219819754, 290.4451672760540077 ) ) ;
#34721 = CARTESIAN_POINT ( 'NONE',  ( 2.689344463419570452, 1464.716346866380036, 236.9361821190090041 ) ) ;
#34722 = CARTESIAN_POINT ( 'NONE',  ( 10.95716479804320009, 1427.278218707250062, 209.1113885757679896 ) ) ;
#34723 = EDGE_LOOP ( 'NONE', ( #78845, #66223, #21808 ) ) ;
#34724 = FACE_OUTER_BOUND ( 'NONE', #29751, .T. ) ;
#34725 = EDGE_CURVE ( 'NONE', #10311, #88376, #49657, .T. ) ;
#34727 = ORIENTED_EDGE ( 'NONE', *, *, #1747, .T. ) ;
#34726 = CARTESIAN_POINT ( 'NONE',  ( -2.500000000000000000, 1448.894380913990062, 183.1110264324979937 ) ) ;
#34728 = CARTESIAN_POINT ( 'NONE',  ( -33.36586802512168504, 1518.913060387330006, 216.3367586934473366 ) ) ;
#34729 = ORIENTED_EDGE ( 'NONE', *, *, #27407, .F. ) ;
#34730 = CARTESIAN_POINT ( 'NONE',  ( 1.842962214296182122, 1515.219201590508419, 204.7964405199711280 ) ) ;
#34731 = CARTESIAN_POINT ( 'NONE',  ( -9.505471540905400474, 1363.500209798490005, 210.6218459616987957 ) ) ;
#34732 = CARTESIAN_POINT ( 'NONE',  ( -10.68791968979999929, 1492.481557180890150, 204.6992124531689967 ) ) ;
#34733 = EDGE_CURVE ( 'NONE', #87972, #105626, #30541, .T. ) ;
#34734 = CARTESIAN_POINT ( 'NONE',  ( 36.12323184972498069, 1456.485569746546389, 269.5474412128850190 ) ) ;
#34735 = DIRECTION ( 'NONE',  ( 6.997424531968003289E-18, -1.000000000000000000, 0.000000000000000000 ) ) ;
#34736 = CARTESIAN_POINT ( 'NONE',  ( 18.88366234174538860, 1437.295717261725713, 213.5084043479270974 ) ) ;
#34737 = DIRECTION ( 'NONE',  ( -0.000000000000000000, -1.000000000000000000, -0.000000000000000000 ) ) ;
#34738 = CARTESIAN_POINT ( 'NONE',  ( -6.807912280453931153, 1516.613882035576353, 212.2734087009808945 ) ) ;
#34739 = CARTESIAN_POINT ( 'NONE',  ( -107.4576979188310162, 1306.483669372790018, 307.4681404593670777 ) ) ;
#34740 = CARTESIAN_POINT ( 'NONE',  ( -9.209502321771219968, 1366.683160837834066, 210.6218459616991936 ) ) ;
#34741 = CARTESIAN_POINT ( 'NONE',  ( -1.337878788439999855, 1456.624765931489947, 199.6947203986289878 ) ) ;
#34742 = CARTESIAN_POINT ( 'NONE',  ( -2.299014068865000038, 1516.811292230880099, 206.2578025137869986 ) ) ;
#34743 = B_SPLINE_CURVE_WITH_KNOTS ( 'NONE', 3,
 ( #7593, #75907, #82093, #39552, #110059, #98893, #23282, #66431, #100547, #73726, #22711, #56909, #52929, #61349, #16515, #26027, #77571, #69746, #93249, #93781, #34456, #52387, #87062, #60223, #18191, #94341, #17619, #17058, #50705, #84836, #103865, #60791 ),
 .UNSPECIFIED., .F., .F.,
 ( 4, 2, 1, 2, 2, 1, 1, 2, 2, 2, 2, 2, 2, 1, 2, 2, 2, 4 ),
 ( 0.000000000000000000, 0.2303738508824927089, 0.2447722165626507185, 0.2483718079826913450, 0.2501716036927140729, 0.2519713994027368287, 0.2591705822428356787, 0.2879673136032326330, 0.3455607763240182706, 0.4607477017655827178, 0.4895444331259781734, 0.4967436159660749140, 0.5003432073861219243, 0.5039427988061689900, 0.5183411644863570311, 0.5759346272071285133, 0.6911215526486663707, 0.9214954035317776126 ),
 .UNSPECIFIED. ) ;
#34744 = CARTESIAN_POINT ( 'NONE',  ( 2.704720143340000327, 1447.053020108410010, 167.4681767528979890 ) ) ;
#34745 = B_SPLINE_SURFACE_WITH_KNOTS ( 'NONE', 5, 1, ( 
 ( #66572, #6630 ),
 ( #49754, #75514 ),
 ( #50314, #36121 ),
 ( #92834, #27711 ),
 ( #7189, #109647 ),
 ( #83884, #70305 ),
 ( #83334, #41888 ),
 ( #59264, #87064 ),
 ( #61897, #41344 ) ),
 .UNSPECIFIED., .F., .F., .F.,
 ( 6, 3, 6 ),
 ( 2, 2 ),
 ( 0.000000000000000000, 3.592628445999999975, 7.162337568599999926 ),
 ( 0.000000000000000000, 14.00000000000000000 ),
 .UNSPECIFIED. ) ;
#34746 = DIRECTION ( 'NONE',  ( -1.000000000000000000, 0.000000000000000000, 0.000000000000000000 ) ) ;
#34747 = CARTESIAN_POINT ( 'NONE',  ( -2.112801085030000081, 1497.385224591190081, 198.0352397674990073 ) ) ;
#34749 = ORIENTED_EDGE ( 'NONE', *, *, #41104, .T. ) ;
#34748 = CARTESIAN_POINT ( 'NONE',  ( 0.7246754490289990525, 1495.521260695290039, 220.6941092417989978 ) ) ;
#34750 = CARTESIAN_POINT ( 'NONE',  ( 40.34236413014900080, 1444.188521476819915, 137.0964790503469999 ) ) ;
#34751 = ORIENTED_EDGE ( 'NONE', *, *, #38524, .T. ) ;
#34752 = CARTESIAN_POINT ( 'NONE',  ( -16.77415066853143344, 1513.652806713756945, 222.5401386658989225 ) ) ;
#34753 = CARTESIAN_POINT ( 'NONE',  ( -24.05801048130000197, 1430.354717888529876, 205.3269550452980070 ) ) ;
#34755 = CARTESIAN_POINT ( 'NONE',  ( 16.89642274560129920, 1409.876247450909887, 192.5027543463019981 ) ) ;
#34754 = CARTESIAN_POINT ( 'NONE',  ( -10.12873630343129960, 1425.173784052110250, 102.3098040917019915 ) ) ;
#34756 = CARTESIAN_POINT ( 'NONE',  ( 2.493699768634999536, 1516.858326417339867, 211.5985794462469869 ) ) ;
#34757 = EDGE_CURVE ( 'NONE', #86293, #28591, #51038, .T. ) ;
#34758 = CARTESIAN_POINT ( 'NONE',  ( 26.93887127448497765, 1509.966274285299505, 195.8255540051888772 ) ) ;
#34759 = B_SPLINE_CURVE_WITH_KNOTS ( 'NONE', 3,
 ( #209, #52262, #86387, #95349, #93661, #17499, #34333, #104299, #16942, #68511, #9675, #51696, #85837 ),
 .UNSPECIFIED., .F., .F.,
 ( 4, 2, 2, 1, 2, 2, 4 ),
 ( 0.000000000000000000, 0.2500000000001801892, 0.3750000000003406719, 0.4375000000004209411, 0.4687500000003957390, 0.5000000000003705924, 1.000000000000000000 ),
 .UNSPECIFIED. ) ;
#34760 = CARTESIAN_POINT ( 'NONE',  ( -19.70592387159999959, 1434.997135647919777, 208.2149306268859732 ) ) ;
#34761 = CARTESIAN_POINT ( 'NONE',  ( -13.51598722900789973, 1379.587471014289804, 208.3760841589739812 ) ) ;
#34762 = CARTESIAN_POINT ( 'NONE',  ( 28.35149942427150194, 1508.694958909449952, 209.4206421715829833 ) ) ;
#34763 = APPLICATION_PROTOCOL_DEFINITION ( 'draft international standard', 'automotive_design', 1998, #5534 ) ;
#34764 = CARTESIAN_POINT ( 'NONE',  ( 4.363515742428809574, 1508.551704408389924, 213.2628643576499883 ) ) ;
#34765 = CARTESIAN_POINT ( 'NONE',  ( -38.73227730840289951, 1439.373716823020004, 136.6705320380260105 ) ) ;
#34766 = ORIENTED_EDGE ( 'NONE', *, *, #94757, .F. ) ;
#34767 = CARTESIAN_POINT ( 'NONE',  ( 10.99547339623849851, 1397.334305137690080, 216.7175448681140040 ) ) ;
#34768 = CARTESIAN_POINT ( 'NONE',  ( -19.73883108929999963, 1465.087274007090173, 209.8242536915520020 ) ) ;
#34769 = CARTESIAN_POINT ( 'NONE',  ( -17.64460054589999771, 1459.279091107629938, 228.2703492655979858 ) ) ;
#34770 = VERTEX_POINT ( 'NONE', #80405 ) ;
#34771 = VERTEX_POINT ( 'NONE', #72562 ) ;
#34772 = B_SPLINE_CURVE_WITH_KNOTS ( 'NONE', 3,
 ( #106551, #11944, #20328, #36593, #64025, #96503, #21413, #13019, #54532, #79717, #95949, #55624 ),
 .UNSPECIFIED., .F., .F.,
 ( 4, 2, 1, 1, 2, 2, 4 ),
 ( 0.000000000000000000, 0.2499999999993910982, 0.3749999999990865640, 0.4374999999989341304, 0.4687499999988572474, 0.4999999999987803645, 1.000000000000000000 ),
 .UNSPECIFIED. ) ;
#34773 = CIRCLE ( 'NONE', #97280, 40.51314971913410545 ) ;
#34774 = CARTESIAN_POINT ( 'NONE',  ( -113.4825880485180960, 1378.913060387289988, 307.7208714236177798 ) ) ;
#34775 = CARTESIAN_POINT ( 'NONE',  ( -9.364590633786502138, 1429.570621513040123, 153.1245166651970067 ) ) ;
#34776 = ORIENTED_EDGE ( 'NONE', *, *, #102955, .F. ) ;
#34777 = FACE_OUTER_BOUND ( 'NONE', #70461, .T. ) ;
#34778 = CARTESIAN_POINT ( 'NONE',  ( -10.58718094483835337, 1418.062149160418812, 197.9312562613863520 ) ) ;
#34779 = CARTESIAN_POINT ( 'NONE',  ( -1.019681180111194907, 1443.417322147287450, 200.2632829245056314 ) ) ;
#34780 = CARTESIAN_POINT ( 'NONE',  ( -13.10038389319999830, 1470.475446589029843, 230.9320392344980064 ) ) ;
#34781 = CARTESIAN_POINT ( 'NONE',  ( 7.507423019669499986, 1508.880864719049896, 202.9817166117040017 ) ) ;
#34782 = CARTESIAN_POINT ( 'NONE',  ( 9.144930279399812179, 1450.428525763479911, 207.9341771728810215 ) ) ;
#34783 = LINE ( 'NONE', #77350, #80738 ) ;
#34784 = CARTESIAN_POINT ( 'NONE',  ( -98.60731883373840390, 1384.869673098270141, 295.9819570146710248 ) ) ;
#34785 = ORIENTED_EDGE ( 'NONE', *, *, #83533, .T. ) ;
#34786 = CARTESIAN_POINT ( 'NONE',  ( -5.781490582474999584, 1516.807958722750072, 202.5702025453269925 ) ) ;
#34787 = CARTESIAN_POINT ( 'NONE',  ( 3.267039691854999983, 1517.012231669750008, 209.8574146130079896 ) ) ;
#34788 = ORIENTED_EDGE ( 'NONE', *, *, #62600, .T. ) ;
#34789 = CARTESIAN_POINT ( 'NONE',  ( 11.76802314650979930, 1427.065976753699942, 146.2965458495970097 ) ) ;
#34790 = CARTESIAN_POINT ( 'NONE',  ( 3.141734923518147760, 1511.860489184966582, 217.0543433876719916 ) ) ;
#34791 = VERTEX_POINT ( 'NONE', #55219 ) ;
#34792 = CARTESIAN_POINT ( 'NONE',  ( 10.73506988043325627, 1424.972993549859893, 139.1354236083641922 ) ) ;
#34793 = CARTESIAN_POINT ( 'NONE',  ( -11.19477969735920020, 1432.344513997310059, 151.5793346050809873 ) ) ;
#34794 = CARTESIAN_POINT ( 'NONE',  ( 9.235801728380000242, 1509.178085974530177, 236.1490528632979817 ) ) ;
#34795 = CARTESIAN_POINT ( 'NONE',  ( -7.514677712297311629, 1489.952809768607949, 217.0828538730388857 ) ) ;
#34796 = CARTESIAN_POINT ( 'NONE',  ( -5.196096933339999779, 1423.860580957830052, 185.9637380877979922 ) ) ;
#34797 = CARTESIAN_POINT ( 'NONE',  ( 6.437126619989999909, 1408.573915340330132, 270.3863109990980433 ) ) ;
#34798 = CARTESIAN_POINT ( 'NONE',  ( 9.214423736713580837, 1450.766440915549992, 209.7350477037440157 ) ) ;
#34799 = CARTESIAN_POINT ( 'NONE',  ( -8.617927921830000670, 1473.119234900290166, 202.1039715580190261 ) ) ;
#34800 = CARTESIAN_POINT ( 'NONE',  ( -15.22113058945292252, 1410.816735285091454, 190.8741554679031651 ) ) ;
#34801 = CARTESIAN_POINT ( 'NONE',  ( -18.87405122379999867, 1379.591274692699926, 208.8065027751330263 ) ) ;
#34802 = CARTESIAN_POINT ( 'NONE',  ( -15.27240770310000073, 1451.322057353730088, 222.8125034062979921 ) ) ;
#34804 = CARTESIAN_POINT ( 'NONE',  ( 4.098642029037120160, 1466.578069225399986, 198.8310470422320009 ) ) ;
#34803 = CARTESIAN_POINT ( 'NONE',  ( 17.41558615450000147, 1458.233052838630101, 229.8710874142980174 ) ) ;
#34805 = CARTESIAN_POINT ( 'NONE',  ( -5.026496579103560514, 1422.965951282957121, 184.8230535773238046 ) ) ;
#34806 = CARTESIAN_POINT ( 'NONE',  ( 11.95229909155720094, 1492.825378593110145, 212.2580762583590115 ) ) ;
#34807 = AXIS2_PLACEMENT_3D ( 'NONE', #45538, #71860, #79677 ) ;
#34808 = CARTESIAN_POINT ( 'NONE',  ( 0.02089856015480650100, 1507.111761549349922, 237.3522809668369860 ) ) ;
#34809 = ORIENTED_EDGE ( 'NONE', *, *, #65082, .T. ) ;
#34810 = DIRECTION ( 'NONE',  ( 0.000000000000000000, 1.000000000000000000, 0.000000000000000000 ) ) ;
#34811 = CARTESIAN_POINT ( 'NONE',  ( 2.719262146893400038E-32, 1524.051704408389924, 209.1218459616989946 ) ) ;
#34812 = CARTESIAN_POINT ( 'NONE',  ( -2.927822177874543907, 1485.046176849765743, 183.1207224758785799 ) ) ;
#34813 = CARTESIAN_POINT ( 'NONE',  ( -14.59826557239999900, 1415.739699861750069, 213.4694186940990051 ) ) ;
#34815 = ORIENTED_EDGE ( 'NONE', *, *, #31524, .T. ) ;
#34814 = CARTESIAN_POINT ( 'NONE',  ( -0.6516344982487189963, 1515.134688985600178, 204.7942274797200071 ) ) ;
#34816 = CARTESIAN_POINT ( 'NONE',  ( 1.539250766859999953, 1434.996842493070062, 189.4157229410979824 ) ) ;
#34817 = CARTESIAN_POINT ( 'NONE',  ( -15.17327376173290077, 1507.614846683550240, 191.8716176117989960 ) ) ;
#34818 = CARTESIAN_POINT ( 'NONE',  ( -11.23709411539999969, 1427.780306893930174, 149.8953276417979907 ) ) ;
#34819 = CARTESIAN_POINT ( 'NONE',  ( 19.25040279134129761, 1456.938452318830059, 224.7542541199149753 ) ) ;
#34820 = FACE_OUTER_BOUND ( 'NONE', #34342, .T. ) ;
#34821 = DIRECTION ( 'NONE',  ( -0.9455185755993178454, 0.000000000000000000, 0.3255681544571539243 ) ) ;
#34822 = CARTESIAN_POINT ( 'NONE',  ( -14.83698687666500149, 1514.217947259989842, 224.2462661523670135 ) ) ;
#34823 = PLANE ( 'NONE',  #64059 ) ;
#34825 = CARTESIAN_POINT ( 'NONE',  ( -10.46710872037930073, 1480.356471093349910, 207.9758824041080061 ) ) ;
#34824 = CARTESIAN_POINT ( 'NONE',  ( -109.7114252020000009, 1385.241546091740020, 297.0985743051589907 ) ) ;
#34826 = CARTESIAN_POINT ( 'NONE',  ( -16.17675210188999912, 1459.146314904164228, 230.7168972899330015 ) ) ;
#34827 = CARTESIAN_POINT ( 'NONE',  ( 1.118903270415000151, 1517.003078582959688, 206.2405205581369785 ) ) ;
#34828 = CARTESIAN_POINT ( 'NONE',  ( 23.70172896860000122, 1410.698151209229991, 267.2984425158979889 ) ) ;
#34829 = CARTESIAN_POINT ( 'NONE',  ( 24.00431267890000342, 1435.335553928009858, 137.4619543163979927 ) ) ;
#34830 = B_SPLINE_SURFACE_WITH_KNOTS ( 'NONE', 5, 1, ( 
 ( #67333, #66786 ),
 ( #39352, #23646 ),
 ( #40447, #49964 ),
 ( #22512, #14693 ),
 ( #24722, #91416 ),
 ( #23082, #49420 ) ),
 .UNSPECIFIED., .F., .F., .F.,
 ( 6, 6 ),
 ( 2, 2 ),
 ( 0.000000000000000000, 3.773583235669999869 ),
 ( 0.000000000000000000, 14.00000000000000000 ),
 .UNSPECIFIED. ) ;
#34831 = CARTESIAN_POINT ( 'NONE',  ( 18.83143426909999718, 1449.734590623980012, 191.7271620068980269 ) ) ;
#34832 = CARTESIAN_POINT ( 'NONE',  ( 17.49859608733503435, 1506.366982236113927, 222.3988492512606001 ) ) ;
#34833 = CARTESIAN_POINT ( 'NONE',  ( -0.1289163742206849983, 1508.852627678509862, 238.3730907446190201 ) ) ;
#34834 = CARTESIAN_POINT ( 'NONE',  ( -15.27212236273409829, 1418.081934325779912, 203.1274159867730020 ) ) ;
#34835 = CARTESIAN_POINT ( 'NONE',  ( -1.218484027960000216, 1451.352790356229889, 183.4814141646979806 ) ) ;
#34836 = DIRECTION ( 'NONE',  ( 0.9995237784460414554, 0.03085800254233316345, -2.148909692663481157E-07 ) ) ;
#34837 = CARTESIAN_POINT ( 'NONE',  ( -14.43176891870000134, 1417.361915031260196, 203.3004091609390116 ) ) ;
#34838 = CARTESIAN_POINT ( 'NONE',  ( -13.40733795300000075, 1443.346361125539943, 187.0475323698980219 ) ) ;
#34839 = FACE_OUTER_BOUND ( 'NONE', #80647, .T. ) ;
#34840 = CARTESIAN_POINT ( 'NONE',  ( -31.77787794420000012, 1436.502309427420187, 136.5769674634980220 ) ) ;
#34841 = CARTESIAN_POINT ( 'NONE',  ( -9.163890685529999303, 1498.531675235289867, 216.1508746217490113 ) ) ;
#34842 = VERTEX_POINT ( 'NONE', #106689 ) ;
#34843 = CARTESIAN_POINT ( 'NONE',  ( 5.593955189962967367, 1510.491946825949526, 216.6725509186245802 ) ) ;
#34844 = CARTESIAN_POINT ( 'NONE',  ( -14.26819836422360055, 1409.411316853469771, 213.5416273160190030 ) ) ;
#34845 = B_SPLINE_SURFACE_WITH_KNOTS ( 'NONE', 5, 5, ( 
 ( #54537, #52866, #86993, #70245, #96508, #20333, #46130, #19213, #3577 ),
 ( #10282, #53416, #44459, #87567, #79174, #36597, #70795, #28196, #104908 ),
 ( #19788, #3029, #37155, #71904, #106020, #105462, #28752, #100354, #40993 ),
 ( #30391, #57284, #39348, #107102, #91412, #29843, #23642, #72964, #6833 ),
 ( #56710, #98143, #4650, #57824, #74619, #40443, #108199, #82461, #81336 ),
 ( #64029, #14689, #56153, #108754, #31487, #32046, #48878, #89751, #74070 ) ),
 .UNSPECIFIED., .F., .F., .F.,
 ( 6, 6 ),
 ( 6, 3, 6 ),
 ( 7.734716563360000130, 13.39941603910000012 ),
 ( -5.551115123129999410E-17, 1.000000000000000000, 2.000000000000000000 ),
 .UNSPECIFIED. ) ;
#34846 = AXIS2_PLACEMENT_3D ( 'NONE', #52847, #242, #25943 ) ;
#34847 = CARTESIAN_POINT ( 'NONE',  ( -11.76846763270469864, 1508.551704408290107, 209.7988299663460339 ) ) ;
#34848 = LINE ( 'NONE', #43266, #108148 ) ;
#34849 = CARTESIAN_POINT ( 'NONE',  ( -9.884517834100000400, 1475.002332015830007, 269.0083476225979666 ) ) ;
#34850 = CARTESIAN_POINT ( 'NONE',  ( -113.0811840974239857, 1310.214785017040640, 303.2740292976359910 ) ) ;
#34851 = CARTESIAN_POINT ( 'NONE',  ( 32.85805783624304155, 1523.678648413191695, 201.0453875934054508 ) ) ;
#34852 = CARTESIAN_POINT ( 'NONE',  ( -24.21504902646103119, 1444.549419358813111, 211.4668081895553655 ) ) ;
#34853 = CARTESIAN_POINT ( 'NONE',  ( -71.67470056025189251, 1384.657983990050070, 296.8765295567630460 ) ) ;
#34854 = CARTESIAN_POINT ( 'NONE',  ( -12.32867557342049913, 1384.937034356689992, 200.2425605594509932 ) ) ;
#34856 = B_SPLINE_CURVE_WITH_KNOTS ( 'NONE', 5,
 ( #36676, #97678, #28830, #63028, #45657, #53496 ),
 .UNSPECIFIED., .F., .F.,
 ( 6, 6 ),
 ( 0.000000000000000000, 1.000000000000000000 ),
 .UNSPECIFIED. ) ;
#34855 = CARTESIAN_POINT ( 'NONE',  ( 18.51177196075189713, 1425.457256880149998, 226.0354587072230004 ) ) ;
#34857 = CARTESIAN_POINT ( 'NONE',  ( -6.661338147749999709E-15, 1443.913060387330006, 155.8032249175980155 ) ) ;
#34858 = B_SPLINE_CURVE_WITH_KNOTS ( 'NONE', 3,
 ( #46506, #29672, #63856, #13960 ),
 .UNSPECIFIED., .F., .F.,
 ( 4, 4 ),
 ( -87.06999293020000152, -29.77037676858719806 ),
 .UNSPECIFIED. ) ;
#34859 = CARTESIAN_POINT ( 'NONE',  ( 9.862951377358559313, 1522.051704408389924, 189.8497022443989977 ) ) ;
#34860 = CARTESIAN_POINT ( 'NONE',  ( -16.57584690634401170, 1524.538969332612623, 237.5592196072092008 ) ) ;
#34861 = CARTESIAN_POINT ( 'NONE',  ( 32.97913964219439720, 1512.187213306747481, 220.2739374644211807 ) ) ;
#34862 = CARTESIAN_POINT ( 'NONE',  ( -23.60058029740000052, 1410.232510812830014, 207.4740788330479973 ) ) ;
#34863 = CARTESIAN_POINT ( 'NONE',  ( 16.96258621739999839, 1415.088016306429836, 208.8510859400770130 ) ) ;
#34864 = CARTESIAN_POINT ( 'NONE',  ( 4.252899391840000654, 1485.733079649889987, 219.0121294742889972 ) ) ;
#34865 = CARTESIAN_POINT ( 'NONE',  ( -15.69795926856320101, 1517.051704408389924, 195.4758181589010064 ) ) ;
#34866 = B_SPLINE_SURFACE_WITH_KNOTS ( 'NONE', 5, 5, ( 
 ( #58259, #101315, #17306, #68329, #100774, #24608, #51501, #86199, #9490, #24065, #25720, #85634, #75066, #34144, #109750, #109216, #25168, #33572, #66671, #94041, #92379, #84542, #67219, #15652, #33029, #83991, #9 ),
 ( #8934, #58802, #16213, #59372, #93483, #42001, #77267, #565, #42545, #7830, #110295, #85085, #67764, #50958, #45878, #79471, #61038, #96264, #69433, #2781, #36901, #61576, #2235, #27955, #71095, #10044, #62707 ),
 ( #78360, #104106, #1117, #105220, #44215, #28508, #1668, #45333, #35247, #96827, #80014, #62138, #20096, #36349, #10609, #53748, #88413, #18418, #95709, #27394, #54289, #11705, #103548, #69991, #43656, #52617, #86755 ),
 ( #87882, #77808, #44778, #18975, #26850, #53171, #35809, #95160, #87313, #78928, #70541, #104658, #19540, #11173, #59725, #110659, #102792, #34509, #388, #42355, #75962, #42923, #67582, #76509, #44026, #86015, #7648 ),
 ( #84358, #110114, #78163, #102256, #93845, #50230, #26650, #32840, #41804, #33386, #59185, #33952, #85442, #58622, #101688, #103348, #68146, #77080, #68685, #17117, #24979, #84897, #51879, #25535, #51305, #92753, #26088 ),
 ( #60278, #93304, #8740, #16566, #94396, #17676, #50760, #9315, #43478, #77622, #69239, #934, #35058, #67033, #60849, #8189, #94974, #86564, #18242, #52437, #9859, #101140, #24434, #16031, #12623, #46801, #97173 ) ),
 .UNSPECIFIED., .F., .F., .F.,
 ( 6, 6 ),
 ( 6, 3, 3, 3, 3, 3, 3, 3, 6 ),
 ( 2.214628065779999933, 99.53245534309999698 ),
 ( 27.66703431970000082, 34.17017219750000123, 36.60162405460000201, 37.81734998310000151, 38.42521294739999860, 39.03307591160000101, 39.44313445259999895, 39.85319299350000222, 40.67331007530000164 ),
 .UNSPECIFIED. ) ;
#34867 = CARTESIAN_POINT ( 'NONE',  ( 5.551115123129999164E-15, 1443.913060387330006, 150.8032249175980155 ) ) ;
#34868 = CARTESIAN_POINT ( 'NONE',  ( 20.24316163930199863, 1432.051856502529972, 214.9276842344050067 ) ) ;
#34869 = CARTESIAN_POINT ( 'NONE',  ( 17.50742245788203988, 1524.972383263452912, 180.8652753437762897 ) ) ;
#34870 = CARTESIAN_POINT ( 'NONE',  ( 24.11200242905490043, 1496.633641595180052, 206.8275340915270135 ) ) ;
#34872 = CARTESIAN_POINT ( 'NONE',  ( -9.529255394169998894, 1383.081092453330029, 200.4708585788389712 ) ) ;
#34871 = CARTESIAN_POINT ( 'NONE',  ( -21.13431233169999857, 1409.651086836630157, 211.8287207610080145 ) ) ;
#34873 = DIRECTION ( 'NONE',  ( -1.000000000000000000, 0.000000000000000000, 0.000000000000000000 ) ) ;
#34874 = DIRECTION ( 'NONE',  ( -0.6736849260863839728, 0.000000000000000000, 0.7390186874254150995 ) ) ;
#34875 = CARTESIAN_POINT ( 'NONE',  ( -10.77749580200000068, 1490.550318827689807, 211.8705906801690162 ) ) ;
#34876 = CARTESIAN_POINT ( 'NONE',  ( 7.961513149873700179, 1449.132914919729956, 202.5404456399149922 ) ) ;
#34877 = CARTESIAN_POINT ( 'NONE',  ( -0.3434805840468270199, 1419.890415353459957, 184.4011449006650025 ) ) ;
#34878 = CARTESIAN_POINT ( 'NONE',  ( 1.708102589285000139, 1517.199196846569976, 202.5572672468869939 ) ) ;
#34879 = CARTESIAN_POINT ( 'NONE',  ( -4.794426340529999386, 1463.608615258990085, 228.2108236244990280 ) ) ;
#34880 = FILL_AREA_STYLE ('',( #43844 ) ) ;
#34881 = CARTESIAN_POINT ( 'NONE',  ( -1.078902958008049989E-15, 1372.293237941190000, 209.1218459616989946 ) ) ;
#34882 = CARTESIAN_POINT ( 'NONE',  ( 2.301262189390000046, 1508.993422234030049, 237.8174349189979750 ) ) ;
#34883 = CARTESIAN_POINT ( 'NONE',  ( -10.16358567940831747, 1422.552167032401030, 210.6545967428373842 ) ) ;
#34885 = VERTEX_POINT ( 'NONE', #98845 ) ;
#34884 = CARTESIAN_POINT ( 'NONE',  ( -63.29683978332329986, 1379.736344894609829, 271.7896898339670315 ) ) ;
#34886 = ORIENTED_EDGE ( 'NONE', *, *, #79151, .F. ) ;
#34887 = CARTESIAN_POINT ( 'NONE',  ( 11.90437301253190050, 1433.618833607449915, 150.4807851880309784 ) ) ;
#34888 = CARTESIAN_POINT ( 'NONE',  ( 26.88198749810000265, 1509.167631437430146, 216.0681759784479823 ) ) ;
#34889 = ORIENTED_EDGE ( 'NONE', *, *, #36788, .T. ) ;
#34890 = CARTESIAN_POINT ( 'NONE',  ( -106.9474174639999973, 1379.784802923450115, 308.7531441963589600 ) ) ;
#34891 = AXIS2_PLACEMENT_3D ( 'NONE', #68382, #59978, #19029 ) ;
#34892 = CARTESIAN_POINT ( 'NONE',  ( -10.33299300126450149, 1447.717326489380184, 209.8084994042759774 ) ) ;
#34893 = CARTESIAN_POINT ( 'NONE',  ( 4.259777698987599948, 1515.374151778960140, 206.1850281986660036 ) ) ;
#34895 = CARTESIAN_POINT ( 'NONE',  ( 6.742596065479999901, 1428.329919402730184, 101.8807690336980016 ) ) ;
#34894 = DIRECTION ( 'NONE',  ( -8.600353058048917082E-15, 1.000000000000000000, 0.000000000000000000 ) ) ;
#34896 = CARTESIAN_POINT ( 'NONE',  ( 13.95343569979999998, 1507.808995617830078, 232.8046479664980097 ) ) ;
#34897 = CARTESIAN_POINT ( 'NONE',  ( 0.6607295372420000090, 1507.643385047829952, 180.9543164539980182 ) ) ;
#34898 = CARTESIAN_POINT ( 'NONE',  ( 3.235048537869999574, 1466.472015836390028, 219.6884158037989891 ) ) ;
#34899 = LINE ( 'NONE', #10250, #76882 ) ;
#34900 =( NAMED_UNIT ( * ) SI_UNIT ( $, .STERADIAN. ) SOLID_ANGLE_UNIT ( ) );
#34901 = CARTESIAN_POINT ( 'NONE',  ( 4.043990307595000111, 1516.983612918759945, 211.6010928179370012 ) ) ;
#34903 = AXIS2_PLACEMENT_3D ( 'NONE', #68408, #7371, #41534 ) ;
#34902 = CARTESIAN_POINT ( 'NONE',  ( 35.12295699368850421, 1435.816162438370156, 134.0999999976959884 ) ) ;
#34904 = CARTESIAN_POINT ( 'NONE',  ( 11.29532840559999940, 1431.858520139869825, 151.5063415908980176 ) ) ;
#34905 = CARTESIAN_POINT ( 'NONE',  ( 6.834484283424999695, 1513.760531203560049, 201.6007729010970024 ) ) ;
#34906 = EDGE_LOOP ( 'NONE', ( #55869, #104182 ) ) ;
#34907 = CARTESIAN_POINT ( 'NONE',  ( 13.91387582277720014, 1435.949825113400038, 150.1916920758069978 ) ) ;
#34908 = DIRECTION ( 'NONE',  ( 0.9455185755993178454, 0.000000000000000000, -0.3255681544571539243 ) ) ;
#34909 = ORIENTED_EDGE ( 'NONE', *, *, #54520, .F. ) ;
#34910 = ORIENTED_EDGE ( 'NONE', *, *, #34433, .F. ) ;
#34911 = ADVANCED_FACE ( 'NONE', ( #47352 ), #64743, .F. ) ;
#34912 = CARTESIAN_POINT ( 'NONE',  ( -7.645353532535000163, 1513.311928781879942, 216.5003517853270125 ) ) ;
#34913 = CARTESIAN_POINT ( 'NONE',  ( -1.489041045350000037, 1466.651558513829968, 235.3699858007980197 ) ) ;
#34914 = CARTESIAN_POINT ( 'NONE',  ( -8.251582857397114168, 1474.733389988602312, 202.9883399646709279 ) ) ;
#34915 = CARTESIAN_POINT ( 'NONE',  ( 7.329925222404999552, 1516.833976295079992, 216.8387248732070134 ) ) ;
#34916 = CARTESIAN_POINT ( 'NONE',  ( 0.2753775948021700004, 1465.468850400709925, 198.1161068840000041 ) ) ;
#34917 = CARTESIAN_POINT ( 'NONE',  ( 11.32781805967280064, 1422.100515973739903, 210.2113672716099870 ) ) ;
#34918 = CARTESIAN_POINT ( 'NONE',  ( -59.11715075928610474, 1379.721731477463663, 259.3860365151069800 ) ) ;
#34919 = CARTESIAN_POINT ( 'NONE',  ( -26.01089419480000231, 1375.250345454859826, 212.5061481324989927 ) ) ;
#34920 = EDGE_LOOP ( 'NONE', ( #20183, #54742 ) ) ;
#34921 = CARTESIAN_POINT ( 'NONE',  ( -6.562635860634999929, 1517.111322026010157, 206.2508942643169974 ) ) ;
#34922 = EDGE_LOOP ( 'NONE', ( #71484, #66988, #34239, #109558 ) ) ;
#34923 = CARTESIAN_POINT ( 'NONE',  ( -103.5761608689879978, 1379.883057947149837, 303.9966227597010402 ) ) ;
#34924 = CARTESIAN_POINT ( 'NONE',  ( -1.543833121739990100, 1424.175334750540060, 228.3471663839470125 ) ) ;
#34925 = ORIENTED_EDGE ( 'NONE', *, *, #67215, .T. ) ;
#34926 = CARTESIAN_POINT ( 'NONE',  ( -12.82273990640000072, 1409.360840331729833, 190.7207006441979900 ) ) ;
#34927 = CARTESIAN_POINT ( 'NONE',  ( 7.585800431785000519, 1513.656171171930055, 215.2887577227170084 ) ) ;
#34929 = ORIENTED_EDGE ( 'NONE', *, *, #25444, .F. ) ;
#34928 = CARTESIAN_POINT ( 'NONE',  ( -7.052967567875161770, 1427.664849047028611, 134.0999999980979851 ) ) ;
#34930 = CARTESIAN_POINT ( 'NONE',  ( 22.87026108289999726, 1432.627911869309855, 216.8958265276880297 ) ) ;
#34931 = CARTESIAN_POINT ( 'NONE',  ( -17.83658993330359976, 1508.551704408389924, 210.4067863104130254 ) ) ;
#34932 = CARTESIAN_POINT ( 'NONE',  ( 1.363474410897823397, 1457.370847949542167, 199.6942262104683437 ) ) ;
#34933 = CARTESIAN_POINT ( 'NONE',  ( -3.968827101022720072, 1517.051704408389924, 229.5396913742049776 ) ) ;
#34934 = CARTESIAN_POINT ( 'NONE',  ( 30.60461244942486303, 1523.621879633029039, 221.8232741897817277 ) ) ;
#34935 = CARTESIAN_POINT ( 'NONE',  ( -1.705466448594999962, 1517.120861839400050, 214.1360410720469929 ) ) ;
#34936 = CARTESIAN_POINT ( 'NONE',  ( -2.480175250669919951, 1429.207669930499833, 200.0830571243679969 ) ) ;
#34937 = CARTESIAN_POINT ( 'NONE',  ( -20.83047217639999715, 1508.917604325230059, 190.1019414035980049 ) ) ;
#34939 = EDGE_CURVE ( 'NONE', #72223, #86431, #38927, .T. ) ;
#34938 = CARTESIAN_POINT ( 'NONE',  ( 29.78122808599999871, 1510.000412735329974, 208.8654317619979963 ) ) ;
#34940 = CARTESIAN_POINT ( 'NONE',  ( 1.717084711415000076, 1516.819260244609950, 211.5980165671369946 ) ) ;
#34941 = EDGE_CURVE ( 'NONE', #26525, #66058, #64731, .T. ) ;
#34942 = DIRECTION ( 'NONE',  ( -1.000000000000000000, 0.000000000000000000, 0.000000000000000000 ) ) ;
#34943 = CARTESIAN_POINT ( 'NONE',  ( 30.29139560038433743, 1523.843271061948371, 222.4926161930171418 ) ) ;
#34944 = EDGE_CURVE ( 'NONE', #20305, #19532, #19629, .T. ) ;
#34946 = ORIENTED_EDGE ( 'NONE', *, *, #110287, .F. ) ;
#34945 = CARTESIAN_POINT ( 'NONE',  ( -102.7967040260000005, 1388.030066489820001, 310.3607065762589627 ) ) ;
#34947 = CARTESIAN_POINT ( 'NONE',  ( 12.45246947889999944, 1471.374055768729932, 259.9010460380980589 ) ) ;
#34948 = EDGE_CURVE ( 'NONE', #18861, #75410, #52185, .T. ) ;
#34949 = DIRECTION ( 'NONE',  ( -0.9401064044234715977, -0.2476038136701678993, 0.2342910579129318938 ) ) ;
#34950 = CARTESIAN_POINT ( 'NONE',  ( -29.17964204711229925, 1509.932035941090135, 212.3228751013100180 ) ) ;
#34951 = EDGE_CURVE ( 'NONE', #20905, #36027, #88801, .T. ) ;
#34952 = CARTESIAN_POINT ( 'NONE',  ( -5.516207685745849965, 1508.892374888589984, 237.2164510697560047 ) ) ;
#34953 = CARTESIAN_POINT ( 'NONE',  ( -19.74442643889999971, 1455.875379726729989, 227.8590200344979735 ) ) ;
#34955 = CARTESIAN_POINT ( 'NONE',  ( 17.92730072119849893, 1410.437638468129990, 222.9214644749860099 ) ) ;
#34954 = DIRECTION ( 'NONE',  ( 1.499379627120000069E-16, 0.000000000000000000, 1.000000000000000000 ) ) ;
#34956 = CARTESIAN_POINT ( 'NONE',  ( -9.922530801272239742, 1448.008349691420108, 209.5732083501220018 ) ) ;
#34957 = CARTESIAN_POINT ( 'NONE',  ( -108.2374560124399920, 1381.012625538590100, 310.2283385330259762 ) ) ;
#34958 = VERTEX_POINT ( 'NONE', #6450 ) ;
#34959 = CARTESIAN_POINT ( 'NONE',  ( -2.295485539174999978, 1516.651306816259876, 204.1261199623870368 ) ) ;
#34960 = CARTESIAN_POINT ( 'NONE',  ( -12.71621933285400097, 1508.444018394370232, 217.3234386178750128 ) ) ;
#34961 = CARTESIAN_POINT ( 'NONE',  ( 29.11003140420000079, 1509.929605083930028, 206.3377952053380113 ) ) ;
#34962 = AXIS2_PLACEMENT_3D ( 'NONE', #14125, #64024, #74063 ) ;
#34963 = CARTESIAN_POINT ( 'NONE',  ( 13.15366522099999891, 1428.703228679430140, 223.0784815107979853 ) ) ;
#34964 = DIRECTION ( 'NONE',  ( -1.156023075842281927E-31, 1.000000000000000000, -1.698192320643030073E-16 ) ) ;
#34965 = EDGE_CURVE ( 'NONE', #56930, #65868, #50659, .T. ) ;
#34966 = CARTESIAN_POINT ( 'NONE',  ( -19.23853081770000273, 1466.576780668189940, 213.8528554934590034 ) ) ;
#34967 = DIRECTION ( 'NONE',  ( 0.000000000000000000, 1.000000000000000000, 0.000000000000000000 ) ) ;
#34968 = CARTESIAN_POINT ( 'NONE',  ( 27.05706547295939757, 1436.771164537570030, 136.7742348819220126 ) ) ;
#34969 = CARTESIAN_POINT ( 'NONE',  ( 35.10515667903409565, 1450.286879874510078, 136.2298007626710046 ) ) ;
#34970 = CARTESIAN_POINT ( 'NONE',  ( -41.91367227552535013, 1454.443418938217519, 269.0780518638181888 ) ) ;
#34971 = CARTESIAN_POINT ( 'NONE',  ( -109.9639389480000062, 1385.359154056490070, 297.0096814836590511 ) ) ;
#34972 = CARTESIAN_POINT ( 'NONE',  ( 10.55550475196309890, 1481.771801338060186, 210.0110538323510241 ) ) ;
#34973 = FACE_OUTER_BOUND ( 'NONE', #66159, .T. ) ;
#34974 = EDGE_CURVE ( 'NONE', #30773, #11858, #58898, .T. ) ;
#34975 = CIRCLE ( 'NONE', #77907, 95.87902122902171698 ) ;
#34976 = DIRECTION ( 'NONE',  ( 0.000000000000000000, 0.000000000000000000, -1.000000000000000000 ) ) ;
#34977 = ORIENTED_EDGE ( 'NONE', *, *, #24711, .T. ) ;
#34978 = CARTESIAN_POINT ( 'NONE',  ( -3.677837710089999800E-15, 1426.566393376330097, 144.1938086916980239 ) ) ;
#34979 = CARTESIAN_POINT ( 'NONE',  ( 13.50143743689999987, 1434.968984401219814, 146.9207468050980196 ) ) ;
#34980 = EDGE_CURVE ( 'NONE', #65067, #67251, #65716, .T. ) ;
#34981 = CARTESIAN_POINT ( 'NONE',  ( 3.436083655040000018, 1486.341471508789937, 198.7604659685989645 ) ) ;
#34982 = CARTESIAN_POINT ( 'NONE',  ( 16.40780854804009792, 1490.854571769470112, 188.6199282104909969 ) ) ;
#34983 = CARTESIAN_POINT ( 'NONE',  ( -8.692880859580000054E-10, 1475.561145520330001, 269.2947192204980524 ) ) ;
#34985 = CARTESIAN_POINT ( 'NONE',  ( 30.80549360313082374, 1524.130440953581001, 196.3987987232744956 ) ) ;
#34984 = CARTESIAN_POINT ( 'NONE',  ( 11.60325616329999932, 1501.577980218590028, 209.3671369954699912 ) ) ;
#34986 = CARTESIAN_POINT ( 'NONE',  ( -28.79939865020000056, 1509.589074244230005, 208.7222596598339805 ) ) ;
#34987 = CARTESIAN_POINT ( 'NONE',  ( 7.537605568320000060, 1427.603033106790008, 212.6450987096289964 ) ) ;
#34988 = CARTESIAN_POINT ( 'NONE',  ( -11.88161848974299950, 1384.885346608229838, 218.9388788513960264 ) ) ;
#34989 = CARTESIAN_POINT ( 'NONE',  ( -11.16241964406192366, 1418.574901742673774, 229.3346417604220449 ) ) ;
#34990 = CARTESIAN_POINT ( 'NONE',  ( -17.35267690140000241, 1414.988017870030035, 207.7949262546180194 ) ) ;
#34991 = CARTESIAN_POINT ( 'NONE',  ( -13.80599379854099951, 1434.979619881170038, 146.4346930281899972 ) ) ;
#34992 = CARTESIAN_POINT ( 'NONE',  ( 25.23965222440000034, 1435.378833613199731, 135.6964465882980164 ) ) ;
#34993 =( BOUNDED_CURVE ( )  B_SPLINE_CURVE ( 3, ( #63116, #37877, #88824, #36217 ),
 .UNSPECIFIED., .F., .F. ) 
 B_SPLINE_CURVE_WITH_KNOTS ( ( 4, 4 ),
 ( 4.712388980384689674, 6.283185307179586232 ),
 .UNSPECIFIED. ) 
 CURVE ( )  GEOMETRIC_REPRESENTATION_ITEM ( )  RATIONAL_B_SPLINE_CURVE ( ( 1.000000000000000000, 0.8047378541243649375, 0.8047378541243649375, 1.000000000000000000 ) ) 
 REPRESENTATION_ITEM ( '' )  );
#34994 = DIRECTION ( 'NONE',  ( 0.9822959463214659959, 0.1391731009602450164, 0.1254014426134129889 ) ) ;
#34995 = ORIENTED_EDGE ( 'NONE', *, *, #67363, .T. ) ;
#34996 = CARTESIAN_POINT ( 'NONE',  ( -17.16958586411000098, 1410.457766366860142, 225.9676320225469794 ) ) ;
#34997 = CARTESIAN_POINT ( 'NONE',  ( 7.419509149259999603, 1440.444625599219989, 149.7273825585979807 ) ) ;
#34998 = ORIENTED_EDGE ( 'NONE', *, *, #99444, .T. ) ;
#34999 = ORIENTED_EDGE ( 'NONE', *, *, #17890, .T. ) ;
#35000 = CARTESIAN_POINT ( 'NONE',  ( 1.083797102072519891, 1435.612377985999956, 227.5537550227259942 ) ) ;
#35001 = B_SPLINE_CURVE_WITH_KNOTS ( 'NONE', 3,
 ( #2990, #105423, #28714, #87528, #105984, #78568, #55038, #55587, #70757, #4079, #62920, #54497, #46638, #38204 ),
 .UNSPECIFIED., .F., .F.,
 ( 4, 2, 1, 1, 1, 1, 2, 2, 4 ),
 ( 0.000000000000000000, 0.2500000000002161049, 0.3750000000003220202, 0.4375000000003748113, 0.4687500000004317102, 0.4843750000004864997, 0.4921875000005116463, 0.5000000000005367928, 1.000000000000000000 ),
 .UNSPECIFIED. ) ;
#35002 = CARTESIAN_POINT ( 'NONE',  ( -14.91528134978724651, 1416.112049509652024, 205.1592457836539438 ) ) ;
#35004 = CARTESIAN_POINT ( 'NONE',  ( -9.977345552905569903, 1439.328177480719887, 208.7903818577229913 ) ) ;
#35003 = CARTESIAN_POINT ( 'NONE',  ( 10.94214974360000170, 1426.073836398730009, 94.99432300369781501 ) ) ;
#35005 = CARTESIAN_POINT ( 'NONE',  ( -0.1147974981524840093, 1507.118024595949919, 237.3465355752350092 ) ) ;
#35006 = CARTESIAN_POINT ( 'NONE',  ( -2.515127511734718713, 1421.311320163850723, 184.3934076788736434 ) ) ;
#35007 = CARTESIAN_POINT ( 'NONE',  ( 7.840108726700000474, 1425.497406979299967, 211.6543916462389916 ) ) ;
#35008 = CARTESIAN_POINT ( 'NONE',  ( 19.03958014020000178, 1453.804227313890124, 200.7927590370090059 ) ) ;
#35009 = CARTESIAN_POINT ( 'NONE',  ( 7.817147024559999657, 1507.298328921630173, 182.8873992191979880 ) ) ;
#35010 = CARTESIAN_POINT ( 'NONE',  ( 3.686666017499999892, 1448.977420087960127, 184.1966211689980071 ) ) ;
#35011 = CARTESIAN_POINT ( 'NONE',  ( 8.001480734926794014, 1364.923464046118625, 209.6218459617148824 ) ) ;
#35013 = ORIENTED_EDGE ( 'NONE', *, *, #85004, .F. ) ;
#35012 = CARTESIAN_POINT ( 'NONE',  ( -3.350338079455601026, 1523.604703353109699, 242.0808062845893289 ) ) ;
#35014 = ORIENTED_EDGE ( 'NONE', *, *, #3285, .T. ) ;
#35015 = VECTOR ( 'NONE', #99228, 999.9999999999998863 ) ;
#35016 = CARTESIAN_POINT ( 'NONE',  ( -40.27000727579999761, 1443.958079488249950, 137.1320871855979817 ) ) ;
#35017 = CIRCLE ( 'NONE', #43987, 3.000000000000002665 ) ;
#35018 = CARTESIAN_POINT ( 'NONE',  ( 7.550503318189189628, 1510.480349263560129, 203.5706572562480119 ) ) ;
#35019 = CARTESIAN_POINT ( 'NONE',  ( -0.9513828761539999679, 1471.786836300230107, 269.8654945467980042 ) ) ;
#35020 = CARTESIAN_POINT ( 'NONE',  ( 8.055079858170127949, 1500.429113765004331, 201.0492220431988812 ) ) ;
#35021 = CARTESIAN_POINT ( 'NONE',  ( -120.1712171740600326, 1306.483669372790246, 310.9930631313191043 ) ) ;
#35022 = CARTESIAN_POINT ( 'NONE',  ( -31.87600794503257617, 1525.042337199240364, 202.1059339849676917 ) ) ;
#35023 = CARTESIAN_POINT ( 'NONE',  ( -2.617907763213700001, 1475.116115922490053, 197.9881756648049986 ) ) ;
#35024 = CARTESIAN_POINT ( 'NONE',  ( -36.40679663865240201, 1451.403536159749819, 134.6865063755689960 ) ) ;
#35025 = B_SPLINE_SURFACE_WITH_KNOTS ( 'NONE', 5, 5, ( 
 ( #89956, #3234, #13230, #4844, #73168, #30606 ),
 ( #37918, #22173, #71562, #72099, #59137, #100555 ),
 ( #15982, #23835, #15435, #93259, #41213, #65881 ),
 ( #75385, #23290, #49627, #108415, #33343, #109522 ),
 ( #32798, #50183, #110617, #76464, #16523, #24927 ),
 ( #33900, #67538, #58027, #74829, #14888, #68095 ),
 ( #49079, #50714, #84844, #74285, #8144, #92162 ),
 ( #84310, #25488, #100002, #24392, #83761, #59679 ),
 ( #58577, #101638, #66982, #42310, #108973, #110067 ) ),
 .UNSPECIFIED., .F., .F., .F.,
 ( 6, 3, 6 ),
 ( 6, 6 ),
 ( 21.34407477379999918, 25.74311937130000061, 30.14216396890000027 ),
 ( 0.000000000000000000, 2.000000000000000000 ),
 .UNSPECIFIED. ) ;
#35026 = CARTESIAN_POINT ( 'NONE',  ( -18.88069888589999934, 1519.913060387329779, 196.2596006804980107 ) ) ;
#35027 = CARTESIAN_POINT ( 'NONE',  ( 10.10760548029105621, 1367.483665353111974, 210.6218459617030021 ) ) ;
#35028 = CARTESIAN_POINT ( 'NONE',  ( 7.143284666917959491, 1409.162509384609848, 195.2043232230670071 ) ) ;
#35029 = CARTESIAN_POINT ( 'NONE',  ( -12.08854166899370064, 1407.246857854960126, 268.9879536978270380 ) ) ;
#35030 = CARTESIAN_POINT ( 'NONE',  ( -14.14290945506900066, 1435.350905828940085, 149.5435571626070157 ) ) ;
#35031 = ORIENTED_EDGE ( 'NONE', *, *, #20683, .T. ) ;
#35032 = CARTESIAN_POINT ( 'NONE',  ( -11.86614525289999911, 1432.349253981700031, 150.3971727848980038 ) ) ;
#35033 = CARTESIAN_POINT ( 'NONE',  ( 13.24057533709999923, 1444.706717224920112, 187.3823346222980035 ) ) ;
#35034 = ORIENTED_EDGE ( 'NONE', *, *, #93207, .F. ) ;
#35035 = ORIENTED_EDGE ( 'NONE', *, *, #86810, .T. ) ;
#35036 = EDGE_CURVE ( 'NONE', #80080, #99658, #24229, .T. ) ;
#35037 = CARTESIAN_POINT ( 'NONE',  ( 5.011594840860459144, 1423.113943537101932, 184.3785993670394987 ) ) ;
#35038 = DIRECTION ( 'NONE',  ( 9.156846217086110244E-47, -1.000000000000000000, 1.836970198721029688E-16 ) ) ;
#35039 = ADVANCED_FACE ( 'NONE', ( #109468 ), #110011, .T. ) ;
#35040 = CARTESIAN_POINT ( 'NONE',  ( -0.7360974767499980365, 1517.045004075700035, 213.1642344714070134 ) ) ;
#35041 = CARTESIAN_POINT ( 'NONE',  ( -8.249097597409999594, 1485.477655575529980, 184.2734846816980223 ) ) ;
#35042 = ORIENTED_EDGE ( 'NONE', *, *, #24827, .T. ) ;
#35043 = DIRECTION ( 'NONE',  ( -5.980589973904019347E-17, 1.000000000000000000, -1.736889445713099699E-16 ) ) ;
#35044 = AXIS2_PLACEMENT_3D ( 'NONE', #33910, #347, #24936 ) ;
#35045 = CARTESIAN_POINT ( 'NONE',  ( -105.9558246502879939, 1378.913060387299993, 303.0503163561330098 ) ) ;
#35046 = CARTESIAN_POINT ( 'NONE',  ( 5.001338628314999646, 1516.911981270829983, 203.3378372969070256 ) ) ;
#35047 = EDGE_CURVE ( 'NONE', #30629, #2493, #12348, .T. ) ;
#35048 = CARTESIAN_POINT ( 'NONE',  ( -28.70345826739999850, 1509.590240598730134, 207.9949817522079911 ) ) ;
#35049 = CARTESIAN_POINT ( 'NONE',  ( -7.722579826676089887, 1517.051704428850144, 208.6871515679729896 ) ) ;
#35050 = CARTESIAN_POINT ( 'NONE',  ( -46.09131934240000561, 1385.005100670120100, 219.0267588369590044 ) ) ;
#35051 = CARTESIAN_POINT ( 'NONE',  ( -53.44135509795150085, 1384.636011670080052, 231.0131721128049662 ) ) ;
#35052 = CARTESIAN_POINT ( 'NONE',  ( -14.53473304376390018, 1379.710786975620067, 208.2794084638009906 ) ) ;
#35053 = B_SPLINE_CURVE_WITH_KNOTS ( 'NONE', 3,
 ( #26691, #53027, #973, #79324, #95562, #94435, #1517, #44066, #35098, #18832 ),
 .UNSPECIFIED., .F., .F.,
 ( 4, 2, 2, 2, 4 ),
 ( 0.000000000000000000, 0.2500000000000000000, 0.5000000000000000000, 0.7500000000000000000, 1.000000000000000000 ),
 .UNSPECIFIED. ) ;
#35054 = CARTESIAN_POINT ( 'NONE',  ( -25.74664715480469823, 1449.922850843729975, 208.7294647506780052 ) ) ;
#35056 = VERTEX_POINT ( 'NONE', #5900 ) ;
#35055 = CARTESIAN_POINT ( 'NONE',  ( -10.72653838659999970, 1445.370122805119991, 185.5580616574980013 ) ) ;
#35057 = CARTESIAN_POINT ( 'NONE',  ( 12.55308716756742626, 1426.311334306029721, 201.5587213662597037 ) ) ;
#35058 = CARTESIAN_POINT ( 'NONE',  ( 27.70206559570000238, 1508.130759166529742, 212.2772318986179982 ) ) ;
#35059 = CARTESIAN_POINT ( 'NONE',  ( 10.70400544403340071, 1460.361839742069833, 206.9582489332520083 ) ) ;
#35060 = CARTESIAN_POINT ( 'NONE',  ( -24.06699603970000112, 1435.344051288429910, 136.8276718557980018 ) ) ;
#35061 = CARTESIAN_POINT ( 'NONE',  ( 3.461360093275000160, 1516.874084700499907, 212.3753080308970311 ) ) ;
#35062 = B_SPLINE_CURVE_WITH_KNOTS ( 'NONE', 3,
 ( #56255, #99331, #41098, #22058, #65767, #24287, #15869, #23736, #15328, #23183, #22605, #13662, #31590, #66337, #74722, #40548, #75277, #39997, #57384, #90946, #109424, #32701, #92056, #66881, #7498, #31037, #91510 ),
 .UNSPECIFIED., .F., .F.,
 ( 4, 2, 2, 1, 1, 1, 1, 2, 2, 2, 2, 1, 1, 1, 2, 2, 4 ),
 ( 0.000000000000000000, 0.06250000000001224021, 0.09375000000001836031, 0.1093750000000226485, 0.1171875000000235367, 0.1210937500000230094, 0.1230468750000218020, 0.1240234375000221212, 0.1250000000000224265, 0.1875000000000156541, 0.2500000000000088818, 0.3749999999999950040, 0.4374999999999895639, 0.4687499999999868994, 0.4843749999999868439, 0.4999999999999867883, 1.000000000000000000 ),
 .UNSPECIFIED. ) ;
#35063 = CARTESIAN_POINT ( 'NONE',  ( -68.56795313739999642, 1379.747562649819884, 279.6372059696590213 ) ) ;
#35064 = B_SPLINE_CURVE_WITH_KNOTS ( 'NONE', 5,
 ( #96037, #53510, #103885, #62480, #27186, #104994, #69201, #52952, #54075 ),
 .UNSPECIFIED., .F., .F.,
 ( 6, 3, 6 ),
 ( 0.000000000000000000, 0.5333467950542268854, 1.000000000000000000 ),
 .UNSPECIFIED. ) ;
#35065 = FACE_OUTER_BOUND ( 'NONE', #36151, .T. ) ;
#35066 = CARTESIAN_POINT ( 'NONE',  ( -29.30029655192924665, 1525.907212628473644, 221.3719603026177367 ) ) ;
#35067 = ADVANCED_FACE ( 'NONE', ( #108357 ), #64266, .F. ) ;
#35068 = CARTESIAN_POINT ( 'NONE',  ( 7.332063939445000678, 1516.939491476980038, 209.1111146381379911 ) ) ;
#35069 = ORIENTED_EDGE ( 'NONE', *, *, #33530, .F. ) ;
#35070 = CARTESIAN_POINT ( 'NONE',  ( -1.873189676845119944, 1451.938853521590090, 184.2960223139319851 ) ) ;
#35071 = CARTESIAN_POINT ( 'NONE',  ( -4.146148586359999832, 1410.300477727830184, 232.1600599902980093 ) ) ;
#35072 = CARTESIAN_POINT ( 'NONE',  ( -43.08084643290000315, 1384.773678278489797, 247.5054735941590138 ) ) ;
#35073 = ADVANCED_FACE ( 'NONE', ( #72984 ), #24963, .T. ) ;
#35074 = EDGE_LOOP ( 'NONE', ( #66808, #80245, #70423, #81989, #48589 ) ) ;
#35075 = CARTESIAN_POINT ( 'NONE',  ( -9.652326224251600806, 1385.312451791279727, 218.7068224263840079 ) ) ;
#35076 = CARTESIAN_POINT ( 'NONE',  ( -3.492373078290000432, 1428.790505188590032, 200.8458585022190164 ) ) ;
#35077 = CARTESIAN_POINT ( 'NONE',  ( 12.44490648448620007, 1434.392432424140225, 149.5192106900200031 ) ) ;
#35078 = CARTESIAN_POINT ( 'NONE',  ( 15.33254751237830149, 1488.407451439539955, 231.1339900686130022 ) ) ;
#35079 = CARTESIAN_POINT ( 'NONE',  ( -23.80940814504779723, 1509.710483542359952, 225.5335122003920105 ) ) ;
#35080 = CARTESIAN_POINT ( 'NONE',  ( -2.242235177520000011, 1409.158574251030132, 187.0303599566979926 ) ) ;
#35081 = CARTESIAN_POINT ( 'NONE',  ( 0.4392564578464259739, 1517.051704408389924, 201.5953311768700189 ) ) ;
#35082 = CARTESIAN_POINT ( 'NONE',  ( 4.240088984218660428, 1441.444059629489857, 162.8289912679279894 ) ) ;
#35083 = EDGE_CURVE ( 'NONE', #57779, #90117, #16399, .T. ) ;
#35085 = CARTESIAN_POINT ( 'NONE',  ( 16.42420380379999756, 1507.212883763329955, 193.5443561786979956 ) ) ;
#35084 = CARTESIAN_POINT ( 'NONE',  ( -1.705466448594999962, 1517.120861839400050, 214.1360410720469929 ) ) ;
#35086 = CARTESIAN_POINT ( 'NONE',  ( -8.862914948930789905, 1385.109572092439976, 218.6788282648730046 ) ) ;
#35087 = CARTESIAN_POINT ( 'NONE',  ( 7.329925222404999552, 1516.833976295079992, 216.8387248732070134 ) ) ;
#35088 = ORIENTED_EDGE ( 'NONE', *, *, #45953, .F. ) ;
#35089 = CARTESIAN_POINT ( 'NONE',  ( 5.004475574535000248, 1517.026025493960105, 201.3999380438669959 ) ) ;
#35090 = CARTESIAN_POINT ( 'NONE',  ( -0.7275771281559999526, 1495.113783641829968, 181.2733469408979943 ) ) ;
#35091 = ORIENTED_EDGE ( 'NONE', *, *, #62581, .T. ) ;
#35092 = CARTESIAN_POINT ( 'NONE',  ( 3.797937935320000236, 1421.119554740329932, 185.2659206367980005 ) ) ;
#35093 = EDGE_CURVE ( 'NONE', #39742, #89306, #37721, .T. ) ;
#35094 = CARTESIAN_POINT ( 'NONE',  ( -17.28313798789999822, 1509.292373661990041, 209.6576118363560113 ) ) ;
#35095 = FACE_OUTER_BOUND ( 'NONE', #64487, .T. ) ;
#35096 = CARTESIAN_POINT ( 'NONE',  ( 2.975355613810000133, 1441.383001986190038, 218.5845790346389776 ) ) ;
#35097 = CARTESIAN_POINT ( 'NONE',  ( -29.52630424919052388, 1525.661275128775515, 196.5237685151092819 ) ) ;
#35098 = CARTESIAN_POINT ( 'NONE',  ( -16.04005855938789793, 1409.473190815148428, 192.8190731777143583 ) ) ;
#35099 = CARTESIAN_POINT ( 'NONE',  ( 17.77615777719999812, 1415.140114695929924, 210.2708809818280145 ) ) ;
#35100 = CARTESIAN_POINT ( 'NONE',  ( 31.41104781486818354, 1512.187213306747481, 202.3296363711535264 ) ) ;
#35101 = CARTESIAN_POINT ( 'NONE',  ( 9.529616216263738337, 1459.343410895429997, 203.7689765404180093 ) ) ;
#35102 = CARTESIAN_POINT ( 'NONE',  ( -8844.044327685292956, -2339.359351152911131, 3014.028579042705587 ) ) ;
#35103 = DIRECTION ( 'NONE',  ( 0.000000000000000000, 0.000000000000000000, -1.000000000000000000 ) ) ;
#35105 = CARTESIAN_POINT ( 'NONE',  ( -4.993214560040000194, 1391.653934889589891, 203.5347113830289913 ) ) ;
#35104 = CARTESIAN_POINT ( 'NONE',  ( -14.75778311606660154, 1417.788083049279976, 203.2704335446259734 ) ) ;
#35106 = CARTESIAN_POINT ( 'NONE',  ( 2.682480990172567026, 1524.330813522192102, 241.8675070349544001 ) ) ;
#35107 = VERTEX_POINT ( 'NONE', #3048 ) ;
#35108 = CARTESIAN_POINT ( 'NONE',  ( -8.308282170169999148, 1508.515045414190126, 219.1793389093990072 ) ) ;
#35109 = CARTESIAN_POINT ( 'NONE',  ( 24.50139030460000100, 1449.832840726370023, 206.9640024934579969 ) ) ;
#35110 = EDGE_CURVE ( 'NONE', #40565, #50666, #37535, .T. ) ;
#35111 = CARTESIAN_POINT ( 'NONE',  ( -24.35760840280000039, 1442.387172707180298, 212.1777659041080142 ) ) ;
#35112 = CARTESIAN_POINT ( 'NONE',  ( 7.492276228816673544, 1410.547776690462115, 187.3898987111521706 ) ) ;
#35113 = DIRECTION ( 'NONE',  ( -0.000000000000000000, -1.000000000000000000, -0.000000000000000000 ) ) ;
#35114 = EDGE_CURVE ( 'NONE', #35478, #54360, #55314, .T. ) ;
#35115 = CARTESIAN_POINT ( 'NONE',  ( 28.62766089293167227, 1526.344110814219221, 220.1997210292020952 ) ) ;
#35116 = CARTESIAN_POINT ( 'NONE',  ( -8.324963436393932881, 1511.468585895425122, 214.5031578665083600 ) ) ;
#35118 = VECTOR ( 'NONE', #97170, 1000.000000000000114 ) ;
#35117 = CARTESIAN_POINT ( 'NONE',  ( -3.522358130609859916, 1488.738444080139971, 219.4891182003030110 ) ) ;
#35119 = CARTESIAN_POINT ( 'NONE',  ( -9.573037224950001089, 1423.427965722019962, 192.3355728592989919 ) ) ;
#35120 = CIRCLE ( 'NONE', #83386, 2.500000000000002220 ) ;
#35121 = CARTESIAN_POINT ( 'NONE',  ( -59.44742613381180263, 1383.797447908259983, 279.6660484894090359 ) ) ;
#35122 = LINE ( 'NONE', #59791, #62496 ) ;
#35123 = DIRECTION ( 'NONE',  ( 0.4978433412588624818, 0.000000000000000000, -0.8672669759446693938 ) ) ;
#35124 = CARTESIAN_POINT ( 'NONE',  ( -1.713660193710039970, 1516.545910801970194, 201.4125102895399948 ) ) ;
#35126 = VERTEX_POINT ( 'NONE', #36616 ) ;
#35125 = CARTESIAN_POINT ( 'NONE',  ( 24.69959934959999970, 1509.552027989230055, 195.6047229538980048 ) ) ;
#35127 = CARTESIAN_POINT ( 'NONE',  ( -18.41935412833382202, 1458.939734570434439, 227.7070353066069401 ) ) ;
#35128 = CARTESIAN_POINT ( 'NONE',  ( -68.60662485189999416, 1380.998604106370067, 291.0269659081590135 ) ) ;
#35129 = CARTESIAN_POINT ( 'NONE',  ( 30.31940284292418752, 1523.456872492435195, 222.4933038710543372 ) ) ;
#35130 = ORIENTED_EDGE ( 'NONE', *, *, #1154, .F. ) ;
#35131 = ORIENTED_EDGE ( 'NONE', *, *, #56222, .T. ) ;
#35132 = CARTESIAN_POINT ( 'NONE',  ( 12.96054471030000066, 1446.716588664140090, 188.5511171461979814 ) ) ;
#35133 = CARTESIAN_POINT ( 'NONE',  ( 33.36586802512172767, 1511.187213306747708, 201.9069332299488622 ) ) ;
#35134 = CARTESIAN_POINT ( 'NONE',  ( 39.22710209691519623, 1440.047129195570051, 136.7325733605709956 ) ) ;
#35135 = VECTOR ( 'NONE', #23045, 1000.000000000000000 ) ;
#35137 = CARTESIAN_POINT ( 'NONE',  ( -35.25149193259999691, 1460.997979651529931, 264.2529779472980067 ) ) ;
#35136 = CARTESIAN_POINT ( 'NONE',  ( 19.13335938739999875, 1434.810047171419910, 209.3864841450680103 ) ) ;
#35138 = PLANE ( 'NONE',  #76903 ) ;
#35139 = CARTESIAN_POINT ( 'NONE',  ( -108.6520057740000027, 1383.101129953369991, 297.5200802490589922 ) ) ;
#35140 = LINE ( 'NONE', #17195, #15961 ) ;
#35141 = CARTESIAN_POINT ( 'NONE',  ( -20.11941513109999846, 1485.685652062829831, 190.9455850217979958 ) ) ;
#35142 = CARTESIAN_POINT ( 'NONE',  ( 1.987580315000000208, 1408.982468221330009, 186.9241478344979726 ) ) ;
#35143 = CARTESIAN_POINT ( 'NONE',  ( 1.443775278116770089, 1486.508325946929972, 197.2873345197639878 ) ) ;
#35144 = CARTESIAN_POINT ( 'NONE',  ( -110.0629084955440078, 1384.909053975289908, 296.9513011978259556 ) ) ;
#35145 = CARTESIAN_POINT ( 'NONE',  ( -9.127884186257210430, 1449.574596975079885, 210.1377844312270042 ) ) ;
#35146 = CARTESIAN_POINT ( 'NONE',  ( -15.39552638457469946, 1421.149667150770028, 203.4478981028480007 ) ) ;
#35147 = CARTESIAN_POINT ( 'NONE',  ( 0.02753318172129999575, 1452.474300612129809, 153.7510498093980118 ) ) ;
#35148 = CARTESIAN_POINT ( 'NONE',  ( -1.906499846882070084E-08, 1517.051704408389924, 201.3992656178269840 ) ) ;
#35149 = VERTEX_POINT ( 'NONE', #104929 ) ;
#35150 = CARTESIAN_POINT ( 'NONE',  ( -18.64618896866739561, 1416.835806635407607, 208.5595417920155512 ) ) ;
#35151 = CARTESIAN_POINT ( 'NONE',  ( -3.041881798304169937, 1470.651976562600112, 187.4038384089669762 ) ) ;
#35152 = CARTESIAN_POINT ( 'NONE',  ( -43.33646147129999804, 1450.475004575490175, 269.7148345228980020 ) ) ;
#35153 = CARTESIAN_POINT ( 'NONE',  ( -113.4000000000000057, 1390.913060387289988, 304.2218459572590064 ) ) ;
#35154 = CARTESIAN_POINT ( 'NONE',  ( 17.71298018430000099, 1410.454334487929827, 223.4084641196980101 ) ) ;
#35155 = DIRECTION ( 'NONE',  ( 0.4794255386042041711, 0.000000000000000000, 0.8775825618903720926 ) ) ;
#35156 = CARTESIAN_POINT ( 'NONE',  ( 4.159508860199999880, 1408.913060387329779, 191.2895657749980103 ) ) ;
#35157 = CARTESIAN_POINT ( 'NONE',  ( -20.53092383730000137, 1484.406264705989997, 211.0952521839789711 ) ) ;
#35158 = CARTESIAN_POINT ( 'NONE',  ( -1.343523894720000111, 1416.547221147930031, 228.0666963329979922 ) ) ;
#35159 = CARTESIAN_POINT ( 'NONE',  ( -5.212293933520000699, 1418.055166734629893, 234.1958690057979879 ) ) ;
#35160 = CARTESIAN_POINT ( 'NONE',  ( 23.10442895610000136, 1411.095127645030061, 207.3185325968580059 ) ) ;
#35161 = CARTESIAN_POINT ( 'NONE',  ( 1.748848150589999983, 1360.440694539920059, 207.6218459616989946 ) ) ;
#35162 = CARTESIAN_POINT ( 'NONE',  ( -45.86418412298019831, 1439.840857331170128, 266.4129133962819651 ) ) ;
#35163 = CARTESIAN_POINT ( 'NONE',  ( -3.602258143659999856, 1434.225543709759904, 185.6459190021979850 ) ) ;
#35164 = ORIENTED_EDGE ( 'NONE', *, *, #38008, .T. ) ;
#35165 = CARTESIAN_POINT ( 'NONE',  ( -8.375770438119999994, 1423.465221721570060, 210.4663274327489830 ) ) ;
#35166 = VERTEX_POINT ( 'NONE', #20351 ) ;
#35167 = CARTESIAN_POINT ( 'NONE',  ( -6.550870182235000172, 1516.727502608469877, 209.8762341530540141 ) ) ;
#35168 = EDGE_CURVE ( 'NONE', #26765, #88934, #95086, .T. ) ;
#35169 = CARTESIAN_POINT ( 'NONE',  ( -5.386823041269999557, 1432.449279870900000, 154.6099110731979920 ) ) ;
#35170 = B_SPLINE_CURVE_WITH_KNOTS ( 'NONE', 5,
 ( #14010, #40325, #73946, #16203, #7280, #49849, #14565, #83980, #32490 ),
 .UNSPECIFIED., .F., .F.,
 ( 6, 3, 6 ),
 ( 0.000000000000000000, 0.4794969076149564469, 1.000000000000000000 ),
 .UNSPECIFIED. ) ;
#35171 = CARTESIAN_POINT ( 'NONE',  ( 0.000000000000000000, 1512.187213306747481, 209.1218459616979999 ) ) ;
#35172 = CARTESIAN_POINT ( 'NONE',  ( 7.529301028092720394, 1425.491244692560031, 212.1922084480190165 ) ) ;
#35173 = AXIS2_PLACEMENT_3D ( 'NONE', #79074, #62280, #61727 ) ;
#35174 = CARTESIAN_POINT ( 'NONE',  ( -26.28577179630749683, 1450.928187855339957, 136.5329518447099986 ) ) ;
#35175 = EDGE_LOOP ( 'NONE', ( #45018, #24140, #53250, #20472, #73625 ) ) ;
#35176 = CARTESIAN_POINT ( 'NONE',  ( 19.42898398440000207, 1429.237499567630039, 213.0284083449880086 ) ) ;
#35178 = CARTESIAN_POINT ( 'NONE',  ( 14.83581816709999934, 1470.804162801829989, 194.6684007568979666 ) ) ;
#35177 = CARTESIAN_POINT ( 'NONE',  ( -2.865544263339262265, 1525.651286436460623, 177.1364475444147502 ) ) ;
#35179 = CARTESIAN_POINT ( 'NONE',  ( 2.115993288544910200, 1487.070543772652172, 219.7330506709243707 ) ) ;
#35180 = CARTESIAN_POINT ( 'NONE',  ( -17.46391305203579947, 1508.455563235159843, 212.6812038778440126 ) ) ;
#35181 = EDGE_CURVE ( 'NONE', #8387, #109101, #96935, .T. ) ;
#35182 = CARTESIAN_POINT ( 'NONE',  ( 1.818941110869999989, 1460.558667203089954, 228.6206250013989916 ) ) ;
#35183 = CARTESIAN_POINT ( 'NONE',  ( -9.096589177653610747, 1440.282626970159754, 206.1069680632970176 ) ) ;
#35184 = ORIENTED_EDGE ( 'NONE', *, *, #69186, .T. ) ;
#35185 = CARTESIAN_POINT ( 'NONE',  ( -1.826910925121480123, 1409.229992614159983, 270.3712872650569921 ) ) ;
#35186 = CARTESIAN_POINT ( 'NONE',  ( -5.788691363644999477, 1517.157901477309906, 207.9987443536870160 ) ) ;
#35187 = CARTESIAN_POINT ( 'NONE',  ( 12.53400550999920071, 1420.773202801019806, 231.1418645745110041 ) ) ;
#35188 = CARTESIAN_POINT ( 'NONE',  ( -18.80269612420000058, 1449.648705166280024, 192.8065731388979884 ) ) ;
#35189 = EDGE_CURVE ( 'NONE', #23187, #53058, #45496, .T. ) ;
#35191 = ORIENTED_EDGE ( 'NONE', *, *, #31203, .F. ) ;
#35190 = CARTESIAN_POINT ( 'NONE',  ( -6.559525637288459166, 1366.137815543844226, 209.6218459617148824 ) ) ;
#35192 = ORIENTED_EDGE ( 'NONE', *, *, #65155, .T. ) ;
#35193 = DIRECTION ( 'NONE',  ( -0.7414773880254650340, -0.000000000000000000, -0.6709778558543747495 ) ) ;
#35194 = CARTESIAN_POINT ( 'NONE',  ( -1.234663454762129797, 1409.459554532440052, 185.7565115510559792 ) ) ;
#35195 = DIRECTION ( 'NONE',  ( 0.000000000000000000, -0.000000000000000000, 1.000000000000000000 ) ) ;
#35196 = CARTESIAN_POINT ( 'NONE',  ( -12.08749531470011718, 1407.203987194673573, 266.9030444376613787 ) ) ;
#35197 = CARTESIAN_POINT ( 'NONE',  ( -18.94560849849241535, 1436.391938629627930, 146.5415713983334456 ) ) ;
#35198 = CARTESIAN_POINT ( 'NONE',  ( -23.20503365730000311, 1430.784771651529809, 213.5757909921379962 ) ) ;
#35199 = CARTESIAN_POINT ( 'NONE',  ( 28.14007468020770020, 1467.874185183969985, 269.3927133897410044 ) ) ;
#35200 = CARTESIAN_POINT ( 'NONE',  ( -1.923414284749828562, 1466.968210799180270, 235.2882593390983459 ) ) ;
#35201 = CARTESIAN_POINT ( 'NONE',  ( -4.736739505650000126, 1428.640587360089967, 202.0925030146489974 ) ) ;
#35202 = CARTESIAN_POINT ( 'NONE',  ( 1.119717716265000051, 1517.038650117239968, 205.6590103047369951 ) ) ;
#35203 = VERTEX_POINT ( 'NONE', #93067 ) ;
#35204 = CARTESIAN_POINT ( 'NONE',  ( 10.96966286673369950, 1432.359740019160199, 151.7701370213850112 ) ) ;
#35205 = CARTESIAN_POINT ( 'NONE',  ( -4.752602823847894342, 1516.784510156630176, 203.3028915219003636 ) ) ;
#35206 = CARTESIAN_POINT ( 'NONE',  ( 23.02649207640000029, 1409.822863297029926, 208.4031441088459928 ) ) ;
#35207 = VERTEX_POINT ( 'NONE', #22531 ) ;
#35208 = CARTESIAN_POINT ( 'NONE',  ( -0.7233576412608461181, 1457.980924837309885, 229.7067188217370131 ) ) ;
#35209 = ADVANCED_FACE ( 'NONE', ( #65690 ), #101857, .F. ) ;
#35210 = CARTESIAN_POINT ( 'NONE',  ( 26.14323217959369927, 1451.983980635410035, 135.2537540905360061 ) ) ;
#35211 = CARTESIAN_POINT ( 'NONE',  ( -4.973792553552699225, 1508.551704408389924, 211.8808810681379953 ) ) ;
#35212 = CARTESIAN_POINT ( 'NONE',  ( -3.078458293700000237, 1385.332091261079995, 218.5458417419390003 ) ) ;
#35213 = ADVANCED_FACE ( 'NONE', ( #74640 ), #41583, .F. ) ;
#35214 = CARTESIAN_POINT ( 'NONE',  ( 18.30580500820000012, 1410.476084872329920, 194.0322744968979976 ) ) ;
#35215 = CARTESIAN_POINT ( 'NONE',  ( 11.76014420379719994, 1479.338752705380102, 208.6264958516850072 ) ) ;
#35216 = CARTESIAN_POINT ( 'NONE',  ( 2.895653292560566250, 1439.669445174284419, 183.9645025138850372 ) ) ;
#35218 = CARTESIAN_POINT ( 'NONE',  ( -18.60031629480377902, 1424.402109664954878, 224.8720212759178878 ) ) ;
#35217 = CARTESIAN_POINT ( 'NONE',  ( -1.285566754106051146, 1444.251790938402337, 217.9819968700315940 ) ) ;
#35219 = CARTESIAN_POINT ( 'NONE',  ( -16.48487881372712494, 1525.795403621571268, 181.7735847721916684 ) ) ;
#35220 = EDGE_CURVE ( 'NONE', #17819, #1407, #48666, .T. ) ;
#35221 = CIRCLE ( 'NONE', #51360, 1.000000000000000888 ) ;
#35222 = DIRECTION ( 'NONE',  ( 0.000000000000000000, 0.000000000000000000, -1.000000000000000000 ) ) ;
#35223 = CARTESIAN_POINT ( 'NONE',  ( -7.769784805680000517, 1383.283764732429972, 218.8591787099389876 ) ) ;
#35224 = CARTESIAN_POINT ( 'NONE',  ( -9.849896899200842881, 1512.913060387330006, 185.5490084180013923 ) ) ;
#35225 = VERTEX_POINT ( 'NONE', #73544 ) ;
#35226 = CARTESIAN_POINT ( 'NONE',  ( -1.191524307911311809, 1526.382868172863937, 179.0083900503167911 ) ) ;
#35227 = CARTESIAN_POINT ( 'NONE',  ( 13.74310390781900004, 1517.051704408389924, 217.0905615615409943 ) ) ;
#35228 = CARTESIAN_POINT ( 'NONE',  ( -0.2839359186375919886, 1408.939684095860002, 231.9819584528090104 ) ) ;
#35229 = EDGE_CURVE ( 'NONE', #87953, #30631, #64332, .T. ) ;
#35230 = CARTESIAN_POINT ( 'NONE',  ( -11.41905458360000125, 1390.240470065509953, 203.8447139951190081 ) ) ;
#35231 = CARTESIAN_POINT ( 'NONE',  ( 1.647872562449680167, 1421.485654266244183, 193.8027845224808914 ) ) ;
#35232 = CARTESIAN_POINT ( 'NONE',  ( -10.81837133496780012, 1462.844907795940117, 206.8474244494269954 ) ) ;
#35233 = CARTESIAN_POINT ( 'NONE',  ( -9.145222436810001909, 1453.522154064730103, 214.3676144192479853 ) ) ;
#35234 = CARTESIAN_POINT ( 'NONE',  ( -1.935345215820309939, 1458.401398452629792, 184.0842910492330304 ) ) ;
#35235 = CARTESIAN_POINT ( 'NONE',  ( 11.71656231259999892, 1433.390345078600149, 150.8916009587979943 ) ) ;
#35236 = CARTESIAN_POINT ( 'NONE',  ( 19.80583385279999931, 1445.467019039670049, 219.6133835737980178 ) ) ;
#35237 = AXIS2_PLACEMENT_3D ( 'NONE', #48041, #5478, #45991 ) ;
#35238 = CARTESIAN_POINT ( 'NONE',  ( 12.65294384001390071, 1415.935475482089942, 196.4577491575730050 ) ) ;
#35239 = CARTESIAN_POINT ( 'NONE',  ( 18.32584553287430040, 1429.337180726220140, 201.2167037691079940 ) ) ;
#35240 = EDGE_CURVE ( 'NONE', #72871, #23842, #16019, .T. ) ;
#35241 = CARTESIAN_POINT ( 'NONE',  ( 22.93376428353750285, 1507.619498552430059, 210.5433103207220142 ) ) ;
#35242 = CARTESIAN_POINT ( 'NONE',  ( 23.69434222019999936, 1435.324930578030035, 137.3226534152980207 ) ) ;
#35243 = CARTESIAN_POINT ( 'NONE',  ( -7.020681098499999884, 1486.251198431629973, 182.5489229859979901 ) ) ;
#35244 = CARTESIAN_POINT ( 'NONE',  ( 0.000000000000000000, 1508.913060387330006, 209.1218459616979999 ) ) ;
#35245 = CARTESIAN_POINT ( 'NONE',  ( -7.437115572297779309, 1509.172770186120033, 238.4311077084169881 ) ) ;
#35246 = EDGE_CURVE ( 'NONE', #66491, #46370, #102957, .T. ) ;
#35247 = CARTESIAN_POINT ( 'NONE',  ( 24.70281711890000054, 1449.797141322859943, 213.6739267561380018 ) ) ;
#35248 = AXIS2_PLACEMENT_3D ( 'NONE', #103162, #85829, #34873 ) ;
#35249 = CARTESIAN_POINT ( 'NONE',  ( -0.5646469274638281632, 1477.536569817737927, 198.7333153465972373 ) ) ;
#35250 = CARTESIAN_POINT ( 'NONE',  ( 26.03716339960346104, 1436.680109442058892, 136.9403589541479107 ) ) ;
#35251 = CARTESIAN_POINT ( 'NONE',  ( 3.298919637249711379, 1508.340401136613082, 219.9739890455120985 ) ) ;
#35252 = CARTESIAN_POINT ( 'NONE',  ( -18.29179382875269866, 1466.060301896490046, 217.7541515181700049 ) ) ;
#35253 = EDGE_CURVE ( 'NONE', #34958, #48781, #43228, .T. ) ;
#35254 = CARTESIAN_POINT ( 'NONE',  ( 6.947377783174999877, 1517.009964551830080, 213.7374907746170152 ) ) ;
#35255 = CARTESIAN_POINT ( 'NONE',  ( -14.88318523122000059, 1421.206373356060112, 205.0325180053320082 ) ) ;
#35256 = CARTESIAN_POINT ( 'NONE',  ( 0.1629390172021479843, 1484.504367874960053, 181.9008776530140210 ) ) ;
#35257 = ORIENTED_EDGE ( 'NONE', *, *, #11938, .F. ) ;
#35258 = CARTESIAN_POINT ( 'NONE',  ( 0.000000000000000000, 1442.773887286369927, 126.8032249175980155 ) ) ;
#35259 = CARTESIAN_POINT ( 'NONE',  ( -9.584235951726055802, 1389.063355496089798, 201.2627618223007744 ) ) ;
#35260 = CARTESIAN_POINT ( 'NONE',  ( -4.629662637760000088, 1475.320779598089985, 199.7646424499390037 ) ) ;
#35262 = EDGE_LOOP ( 'NONE', ( #29717, #15528, #19442, #101187, #18203, #55302 ) ) ;
#35261 = CARTESIAN_POINT ( 'NONE',  ( -35.14989576446389918, 1451.591923343860117, 134.0999999983660018 ) ) ;
#35263 = CARTESIAN_POINT ( 'NONE',  ( -3.818868948821170228, 1508.551704408389924, 219.8880244334079919 ) ) ;
#35264 = ORIENTED_EDGE ( 'NONE', *, *, #4899, .T. ) ;
#35265 = CARTESIAN_POINT ( 'NONE',  ( 0.4116874139510000585, 1416.851343894929869, 190.6255312621979954 ) ) ;
#35266 = B_SPLINE_CURVE_WITH_KNOTS ( 'NONE', 5,
 ( #108988, #75399, #32811, #44412, #19161, #94228 ),
 .UNSPECIFIED., .F., .F.,
 ( 6, 6 ),
 ( 0.000000000000000000, 1.000000000000000000 ),
 .UNSPECIFIED. ) ;
#35267 = DIRECTION ( 'NONE',  ( -1.000000000000000000, 0.000000000000000000, 0.000000000000000000 ) ) ;
#35268 = CARTESIAN_POINT ( 'NONE',  ( -14.27054084439999926, 1415.934222462129810, 221.2887574511979949 ) ) ;
#35269 = DIRECTION ( 'NONE',  ( -5.053215498073659967E-16, -1.000000000000000000, -2.442490654180000246E-15 ) ) ;
#35270 = CARTESIAN_POINT ( 'NONE',  ( -2.835036738194454564, 1367.791076339870415, 208.6398238693165297 ) ) ;
#35271 = CARTESIAN_POINT ( 'NONE',  ( -1.191415256510000020, 1432.303667401890152, 218.5821185343490072 ) ) ;
#35272 = CARTESIAN_POINT ( 'NONE',  ( -11.11751878483429934, 1471.394268115599971, 206.7642780669090143 ) ) ;
#35273 = AXIS2_PLACEMENT_3D ( 'NONE', #105877, #72824, #63345 ) ;
#35274 = CARTESIAN_POINT ( 'NONE',  ( -3.350338079455601026, 1523.604703353109699, 242.0808062845893289 ) ) ;
#35275 = CARTESIAN_POINT ( 'NONE',  ( -11.87927758770000075, 1391.913060425439880, 209.7224555632550107 ) ) ;
#35276 = CARTESIAN_POINT ( 'NONE',  ( -85.67243720148771047, 1385.178525901309968, 289.3562383022049858 ) ) ;
#35277 = CARTESIAN_POINT ( 'NONE',  ( -17.39452685740000248, 1413.991076397230017, 192.1659084337979948 ) ) ;
#35278 = DIRECTION ( 'NONE',  ( 1.984846884490000055E-13, 0.000000000000000000, -1.000000000000000000 ) ) ;
#35279 = ORIENTED_EDGE ( 'NONE', *, *, #21508, .T. ) ;
#35280 = CARTESIAN_POINT ( 'NONE',  ( -15.71169620265270161, 1410.111862918789939, 226.5238431294280019 ) ) ;
#35282 = ORIENTED_EDGE ( 'NONE', *, *, #7124, .T. ) ;
#35281 = DIRECTION ( 'NONE',  ( -5.980589973904019347E-17, 1.000000000000000000, -1.736889445713099699E-16 ) ) ;
#35283 = FACE_OUTER_BOUND ( 'NONE', #4636, .T. ) ;
#35284 = ORIENTED_EDGE ( 'NONE', *, *, #35393, .T. ) ;
#35285 = CARTESIAN_POINT ( 'NONE',  ( 26.37059714170000291, 1509.833941931429990, 221.6204849630979936 ) ) ;
#35286 = CARTESIAN_POINT ( 'NONE',  ( -8.910387285865079221, 1362.858511851195999, 210.6218459616987957 ) ) ;
#35287 = CARTESIAN_POINT ( 'NONE',  ( -11.59964765079999971, 1491.341587899690012, 206.7829323850089907 ) ) ;
#35288 = CARTESIAN_POINT ( 'NONE',  ( 39.55840597086309884, 1451.233580783764637, 269.6025367666410375 ) ) ;
#35289 = CARTESIAN_POINT ( 'NONE',  ( 12.41707514731779938, 1427.120553744379777, 206.8353885506759866 ) ) ;
#35290 = CARTESIAN_POINT ( 'NONE',  ( 19.23317556650448523, 1438.816174030696629, 212.7465897691410817 ) ) ;
#35291 = CARTESIAN_POINT ( 'NONE',  ( -9108.204429824800172, -2340.220200558880151, -1569.808522337019895 ) ) ;
#35292 = CARTESIAN_POINT ( 'NONE',  ( -5.651514362218461152, 1516.808499252805632, 214.0555898242563444 ) ) ;
#35293 = CARTESIAN_POINT ( 'NONE',  ( -21.34331888389999676, 1507.003414196590029, 212.5301348003789883 ) ) ;
#35294 = CARTESIAN_POINT ( 'NONE',  ( -10.07915732761907712, 1367.514362519412089, 210.6218459617030021 ) ) ;
#35295 = CARTESIAN_POINT ( 'NONE',  ( 0.3001670315860009430, 1456.850937440089865, 199.4793357935189988 ) ) ;
#35296 = CARTESIAN_POINT ( 'NONE',  ( 2.476450664134999702, 1516.843453247299749, 206.8221896160070230 ) ) ;
#35297 = CIRCLE ( 'NONE', #13856, 0.9999999999999952260 ) ;
#35298 = CARTESIAN_POINT ( 'NONE',  ( -13.02211328169330073, 1434.883360788459868, 149.7670459028529990 ) ) ;
#35299 = CARTESIAN_POINT ( 'NONE',  ( 849.7329242730789929, 1438.581626214380094, 209.1374421084189805 ) ) ;
#35300 = CARTESIAN_POINT ( 'NONE',  ( -2.580029938729999639, 1497.232914682590035, 198.1414743728990118 ) ) ;
#35302 = ORIENTED_EDGE ( 'NONE', *, *, #19892, .T. ) ;
#35301 = CARTESIAN_POINT ( 'NONE',  ( -3.216334032309999813, 1497.139726794089711, 221.0989039285990145 ) ) ;
#35303 = CARTESIAN_POINT ( 'NONE',  ( -120.0391016774570403, 1391.913060387289988, 305.8779575274093077 ) ) ;
#35304 = EDGE_LOOP ( 'NONE', ( #66636, #23949, #14099, #3676 ) ) ;
#35305 = CARTESIAN_POINT ( 'NONE',  ( 40.57811333989999980, 1433.211871387559995, 261.6156834470980357 ) ) ;
#35306 = CARTESIAN_POINT ( 'NONE',  ( -25.10029913840000049, 1449.799429884400070, 205.9286887820979928 ) ) ;
#35308 = CARTESIAN_POINT ( 'NONE',  ( 16.25665712022090048, 1409.489020141060109, 192.9910857566509890 ) ) ;
#35307 = CARTESIAN_POINT ( 'NONE',  ( -11.67404807818740053, 1426.321468137869942, 139.7108783720840108 ) ) ;
#35309 = CARTESIAN_POINT ( 'NONE',  ( 2.492443650904999863, 1516.793978928989873, 212.3737347995770222 ) ) ;
#35310 = B_SPLINE_CURVE_WITH_KNOTS ( 'NONE', 5,
 ( #18404, #79452, #79995, #11152, #88937, #88396, #29047, #44760, #12228 ),
 .UNSPECIFIED., .F., .F.,
 ( 6, 3, 6 ),
 ( 0.8631819992775470185, 2.053866004900000153, 3.194082035662300090 ),
 .UNSPECIFIED. ) ;
#35311 = CARTESIAN_POINT ( 'NONE',  ( 28.15539526923029001, 1510.007817771240298, 198.7357687764576895 ) ) ;
#35312 = CARTESIAN_POINT ( 'NONE',  ( -19.44845634420000025, 1435.008643399710081, 208.5507817201369960 ) ) ;
#35313 = CARTESIAN_POINT ( 'NONE',  ( -43.50118323360000261, 1440.913060407490093, 263.8966221483980235 ) ) ;
#35314 = CARTESIAN_POINT ( 'NONE',  ( -13.18655059090340131, 1379.448246895369948, 208.4926571931940202 ) ) ;
#35315 = CARTESIAN_POINT ( 'NONE',  ( 31.82246047982030390, 1465.839548924079509, 269.9247166951640224 ) ) ;
#35316 = CARTESIAN_POINT ( 'NONE',  ( 4.301866786085239980, 1508.551704408389924, 213.3279396115709687 ) ) ;
#35317 = CARTESIAN_POINT ( 'NONE',  ( -38.22481880452640013, 1438.834491510689986, 136.6247642330480119 ) ) ;
#35318 = ORIENTED_EDGE ( 'NONE', *, *, #54487, .T. ) ;
#35319 = CARTESIAN_POINT ( 'NONE',  ( 10.73158195967269890, 1397.616005728979871, 200.3871790473220074 ) ) ;
#35320 = CARTESIAN_POINT ( 'NONE',  ( 9.404417543028079862, 1461.021834069670149, 206.2633287157840130 ) ) ;
#35321 = CARTESIAN_POINT ( 'NONE',  ( -17.10148908190000228, 1459.927071089530045, 228.3592279236980005 ) ) ;
#35322 = ORIENTED_EDGE ( 'NONE', *, *, #16119, .T. ) ;
#35323 = ORIENTED_EDGE ( 'NONE', *, *, #105278, .F. ) ;
#35324 = AXIS2_PLACEMENT_3D ( 'NONE', #84669, #58941, #57850 ) ;
#35325 = DIRECTION ( 'NONE',  ( -1.755985294532469921E-16, 1.000000000000000000, -1.338183447452831989E-16 ) ) ;
#35326 = DIRECTION ( 'NONE',  ( 0.3090169943749382919, 0.000000000000000000, 0.9510565162951565288 ) ) ;
#35327 = ORIENTED_EDGE ( 'NONE', *, *, #100700, .T. ) ;
#35328 = CARTESIAN_POINT ( 'NONE',  ( -7.526713224480260145, 1508.370997529450051, 219.6556564864339975 ) ) ;
#35329 = CARTESIAN_POINT ( 'NONE',  ( -14.72917304848470010, 1508.551704408389924, 210.3587638926149737 ) ) ;
#35330 = CARTESIAN_POINT ( 'NONE',  ( -12.53380580351000084, 1442.773887400870080, 185.9733686700720057 ) ) ;
#35331 = AXIS2_PLACEMENT_3D ( 'NONE', #94342, #77025, #76456 ) ;
#35332 = CARTESIAN_POINT ( 'NONE',  ( -9.342819160739999518, 1461.186629906429971, 232.5279129794980122 ) ) ;
#35333 = CARTESIAN_POINT ( 'NONE',  ( 0.8412646513084379718, 1420.713512048480197, 182.8900134064909935 ) ) ;
#35334 = CARTESIAN_POINT ( 'NONE',  ( 9.279213122865108687, 1450.852794977289932, 207.7366403636850123 ) ) ;
#35335 = CARTESIAN_POINT ( 'NONE',  ( 19.22058768450000343, 1456.859121009089904, 206.3396914917290133 ) ) ;
#35336 = CARTESIAN_POINT ( 'NONE',  ( -92.68261419228250020, 1384.848981413319962, 293.9963934270520554 ) ) ;
#35337 = ORIENTED_EDGE ( 'NONE', *, *, #74428, .T. ) ;
#35338 =( BOUNDED_CURVE ( )  B_SPLINE_CURVE ( 3, ( #41654, #67983, #35455, #227 ),
 .UNSPECIFIED., .F., .T. ) 
 B_SPLINE_CURVE_WITH_KNOTS ( ( 4, 4 ),
 ( 5.600235996204509625, 5.892581600017769539 ),
 .UNSPECIFIED. ) 
 CURVE ( )  GEOMETRIC_REPRESENTATION_ITEM ( )  RATIONAL_B_SPLINE_CURVE ( ( 1.000000000000000000, 0.9928905095994882135, 0.9928905095994882135, 1.000000000000000000 ) ) 
 REPRESENTATION_ITEM ( '' )  );
#35339 = CARTESIAN_POINT ( 'NONE',  ( 2.483322453895000059, 1517.139039350860003, 202.5585910412470128 ) ) ;
#35340 = CARTESIAN_POINT ( 'NONE',  ( -4.618583430005000601, 1516.939762005280045, 209.1349059721700030 ) ) ;
#35341 = VERTEX_POINT ( 'NONE', #76280 ) ;
#35342 = CARTESIAN_POINT ( 'NONE',  ( 11.83526461542720121, 1430.237649493160006, 149.5707587408450081 ) ) ;
#35343 = CARTESIAN_POINT ( 'NONE',  ( 5.513435558552499671, 1508.603735221732222, 201.8522301334030544 ) ) ;
#35344 = ORIENTED_EDGE ( 'NONE', *, *, #90309, .F. ) ;
#35345 = DIRECTION ( 'NONE',  ( 0.6742693640212139572, -4.299109996486529694E-13, 0.7384854939282339270 ) ) ;
#35346 = EDGE_CURVE ( 'NONE', #49664, #7555, #35376, .T. ) ;
#35347 = CARTESIAN_POINT ( 'NONE',  ( -13.51812398686054451, 1443.913060387329324, 169.4008117781592375 ) ) ;
#35348 = CARTESIAN_POINT ( 'NONE',  ( -2.860413922163684841, 1367.970058130527377, 208.1452275469912649 ) ) ;
#35349 = CARTESIAN_POINT ( 'NONE',  ( -10.56724066066260015, 1462.360737918739915, 208.4611404715059848 ) ) ;
#35350 = CARTESIAN_POINT ( 'NONE',  ( -5.116133894400000770, 1420.946959116729886, 186.4728714752979783 ) ) ;
#35351 = CARTESIAN_POINT ( 'NONE',  ( 2.316388767259710324, 1408.277175035590062, 270.3918176960409596 ) ) ;
#35352 = DIRECTION ( 'NONE',  ( 0.9417419115949053898, -0.3363363969979660806, -9.559255346349042767E-16 ) ) ;
#35353 = CARTESIAN_POINT ( 'NONE',  ( -5.592037798779999846, 1474.580918538189962, 199.9913374685289966 ) ) ;
#35354 = CARTESIAN_POINT ( 'NONE',  ( 10.51054125589999977, 1491.593346108490096, 212.4262192567589693 ) ) ;
#35355 = CARTESIAN_POINT ( 'NONE',  ( -14.17772861709999965, 1379.591530681489985, 207.8208986663090059 ) ) ;
#35356 = DIRECTION ( 'NONE',  ( -0.8775825618903734249, -0.000000000000000000, -0.4794255386042018952 ) ) ;
#35358 = CARTESIAN_POINT ( 'NONE',  ( 14.72777576890000084, 1453.165958253430063, 195.2129441428980101 ) ) ;
#35357 = CARTESIAN_POINT ( 'NONE',  ( 17.96021206210000187, 1457.749394617429971, 229.4559061194979961 ) ) ;
#35359 = CARTESIAN_POINT ( 'NONE',  ( -68.71629745417266122, 1379.747847503009552, 280.3053889065544126 ) ) ;
#35360 = TOROIDAL_SURFACE ( 'NONE', #10263, 3.250000000000000000, 0.5000000000000000000 ) ;
#35361 = CARTESIAN_POINT ( 'NONE',  ( 17.72240587385099886, 1414.657222584279907, 224.9178048682000224 ) ) ;
#35362 = FACE_OUTER_BOUND ( 'NONE', #89831, .T. ) ;
#35363 = ORIENTED_EDGE ( 'NONE', *, *, #35846, .T. ) ;
#35364 = CARTESIAN_POINT ( 'NONE',  ( 28.81649562247350360, 1526.349689584397083, 198.1982788008647276 ) ) ;
#35365 = ADVANCED_FACE ( 'NONE', ( #78490 ), #39693, .T. ) ;
#35366 = CARTESIAN_POINT ( 'NONE',  ( -18.02257621027615997, 1526.382868172863937, 182.8951942368373977 ) ) ;
#35367 = CARTESIAN_POINT ( 'NONE',  ( -2.946552187109835241, 1485.285160343432153, 182.9853163874463462 ) ) ;
#35368 = CARTESIAN_POINT ( 'NONE',  ( 0.000000000000000000, 1512.913060387330006, 209.1218459616979999 ) ) ;
#35370 = ORIENTED_EDGE ( 'NONE', *, *, #33532, .F. ) ;
#35369 = CARTESIAN_POINT ( 'NONE',  ( -0.6118612317751669361, 1515.137305168459989, 204.7942959869070023 ) ) ;
#35371 = CARTESIAN_POINT ( 'NONE',  ( -15.65670116826264113, 1415.721358585960843, 209.6507542426478494 ) ) ;
#35372 = CARTESIAN_POINT ( 'NONE',  ( 20.14609246460000236, 1475.555345410090013, 207.1883922094089883 ) ) ;
#35373 = CARTESIAN_POINT ( 'NONE',  ( -10.93704887400000025, 1430.005839323029932, 151.3915896504979912 ) ) ;
#35374 = FACE_OUTER_BOUND ( 'NONE', #48977, .T. ) ;
#35375 = CARTESIAN_POINT ( 'NONE',  ( -11.03553767863800061, 1462.348513829580043, 209.1377274935910009 ) ) ;
#35376 = LINE ( 'NONE', #33707, #2161 ) ;
#35377 = CARTESIAN_POINT ( 'NONE',  ( -9.783936650027678539, 1438.409968310599879, 210.7790528106160082 ) ) ;
#35378 = CARTESIAN_POINT ( 'NONE',  ( -15.31485522056499882, 1513.484013041540038, 223.6897698068669911 ) ) ;
#35379 = CARTESIAN_POINT ( 'NONE',  ( 14.58335259939999951, 1410.403800467930068, 227.7087990198979810 ) ) ;
#35380 = CARTESIAN_POINT ( 'NONE',  ( -8.049345161460001563, 1477.536138853090051, 215.9441310019589935 ) ) ;
#35382 = CARTESIAN_POINT ( 'NONE',  ( -16.17567356680000046, 1459.146941997929844, 230.7169173512979796 ) ) ;
#35381 = AXIS2_PLACEMENT_3D ( 'NONE', #2667, #36793, #70985 ) ;
#35383 = CARTESIAN_POINT ( 'NONE',  ( 2.864972116015000125, 1516.859514182039902, 206.2412530031170093 ) ) ;
#35384 = CARTESIAN_POINT ( 'NONE',  ( 31.40639260020000023, 1415.744722567929784, 269.1485073036980111 ) ) ;
#35385 = B_SPLINE_CURVE_WITH_KNOTS ( 'NONE', 3,
 ( #109284, #83501, #100316, #51023, #75136, #23602, #33643, #16822, #48840, #67839, #82964, #40404, #74581, #49924, #84061, #85158, #84607, #109823, #99750, #7358, #92450, #8444, #76770, #6257, #32568, #15723, #84, #66742, #24678, #100845, #33103, #65634, #41523, #24136, #23040, #58875, #93007, #58326, #57244, #7899, #91373, #42071, #85710, #61111, #78429, #17378, #51577, #69501, #86266, #61645, #94667, #103624, #9005, #77331, #43180, #1184 ),
 .UNSPECIFIED., .F., .F.,
 ( 4, 2, 2, 1, 1, 1, 1, 1, 2, 2, 2, 1, 1, 1, 1, 2, 2, 2, 2, 2, 2, 2, 1, 1, 1, 1, 2, 2, 2, 2, 1, 1, 1, 2, 2, 4 ),
 ( 0.000000000000000000, 0.2500000000126188504, 0.3750000000189228633, 0.4375000000220682916, 0.4687500000236474174, 0.4843750000244362308, 0.4921875000248307486, 0.4960937500250203747, 0.4980468750251229593, 0.5000000000252254884, 0.6250000000316919824, 0.6875000000349166251, 0.7187500000365378838, 0.7343750000373484577, 0.7421875000377536891, 0.7460937500379563048, 0.7500000000381589205, 0.8125000000413759027, 0.8437500000429742908, 0.8750000000445727899, 0.8906250000453606042, 0.8984375000457649474, 0.9023437500459566829, 0.9042968750460645966, 0.9052734375461291005, 0.9057617187961615191, 0.9060058594211788385, 0.9062500000461961580, 0.9218750000388737931, 0.9296875000352123886, 0.9335937500333889583, 0.9355468750324835714, 0.9365234375320303783, 0.9370117187817978976, 0.9375000000315654169, 1.000000000000000000 ),
 .UNSPECIFIED. ) ;
#35386 = ADVANCED_FACE ( 'NONE', ( #103684 ), #394, .T. ) ;
#35387 = CARTESIAN_POINT ( 'NONE',  ( 0.5800809713973276160, 1465.108713975482033, 238.1055978074999757 ) ) ;
#35388 = CARTESIAN_POINT ( 'NONE',  ( 24.29813646699999907, 1449.724010015529984, 206.4560171053380202 ) ) ;
#35389 = CARTESIAN_POINT ( 'NONE',  ( -23.60070384349999983, 1435.435992124709855, 213.5551618677380077 ) ) ;
#35390 = DIRECTION ( 'NONE',  ( 0.000000000000000000, -0.8505177418130608347, 0.5259463573989380247 ) ) ;
#35391 = CARTESIAN_POINT ( 'NONE',  ( 17.78793056501380931, 1523.919943579690425, 237.8334796938502791 ) ) ;
#35392 = CARTESIAN_POINT ( 'NONE',  ( -1.280362373440000034, 1451.774120662730184, 183.7183834658980004 ) ) ;
#35393 = EDGE_CURVE ( 'NONE', #103755, #1788, #6777, .T. ) ;
#35394 = CARTESIAN_POINT ( 'NONE',  ( -15.81201443571409904, 1506.433683733589987, 193.8503163142329981 ) ) ;
#35395 = CARTESIAN_POINT ( 'NONE',  ( -15.57670388880000090, 1415.694330284400166, 209.2552609234499812 ) ) ;
#35396 = CARTESIAN_POINT ( 'NONE',  ( -16.56043081341401901, 1409.526309863062124, 193.4350318160313122 ) ) ;
#35397 = CARTESIAN_POINT ( 'NONE',  ( -17.23446452470000168, 1453.313060387329870, 219.9051549417980027 ) ) ;
#35398 = CARTESIAN_POINT ( 'NONE',  ( -32.74366364859999834, 1436.969577990789730, 136.5975034958979961 ) ) ;
#35399 = FACE_OUTER_BOUND ( 'NONE', #73423, .T. ) ;
#35400 = ORIENTED_EDGE ( 'NONE', *, *, #102331, .F. ) ;
#35401 = CARTESIAN_POINT ( 'NONE',  ( -2.766744960634999639, 1511.930588878439949, 201.4376028569870130 ) ) ;
#35402 = CARTESIAN_POINT ( 'NONE',  ( -14.54001393154930000, 1409.420808862239937, 212.5391509058709971 ) ) ;
#35403 = AXIS2_PLACEMENT_3D ( 'NONE', #96552, #77134, #97649 ) ;
#35404 = CARTESIAN_POINT ( 'NONE',  ( -2.478238621609999637, 1439.208302790359994, 157.7515629680979998 ) ) ;
#35405 = CARTESIAN_POINT ( 'NONE',  ( -18.18436572850000132, 1472.598912338130049, 269.3834208221979338 ) ) ;
#35406 = DIRECTION ( 'NONE',  ( -0.05326577277506865798, 0.03591581246945392547, 0.9979342723172373031 ) ) ;
#35407 = CIRCLE ( 'NONE', #55333, 1.000000000000002442 ) ;
#35408 = CARTESIAN_POINT ( 'NONE',  ( -4.517196230222680242, 1517.151704408390060, 190.6118719775071781 ) ) ;
#35409 = CARTESIAN_POINT ( 'NONE',  ( -24.34971616191185007, 1444.638322005277587, 211.2124739967878213 ) ) ;
#35410 = CARTESIAN_POINT ( 'NONE',  ( -61.96637076363960261, 1384.688313717450228, 284.1926743991750186 ) ) ;
#35411 = CARTESIAN_POINT ( 'NONE',  ( -24.54314185457210229, 1384.958787300020049, 203.0891551377700068 ) ) ;
#35412 = CARTESIAN_POINT ( 'NONE',  ( 17.55069790844339650, 1424.280160729299951, 227.8786989819499809 ) ) ;
#35413 = CARTESIAN_POINT ( 'NONE',  ( 20.61376621259999808, 1508.366577482129969, 227.7668722788980062 ) ) ;
#35414 = CIRCLE ( 'NONE', #3313, 2.458500000000000352 ) ;
#35415 = CARTESIAN_POINT ( 'NONE',  ( -3.218260492609999801, 1432.346960983880081, 155.4230413404980027 ) ) ;
#35416 = CARTESIAN_POINT ( 'NONE',  ( 2.499999999999999556, 1411.429641636930000, 137.0999999980979851 ) ) ;
#35417 = CARTESIAN_POINT ( 'NONE',  ( 4.282693164180000345, 1515.349926011190064, 208.0213331141290212 ) ) ;
#35418 = CARTESIAN_POINT ( 'NONE',  ( -7.999195660609999869, 1509.131454673530015, 180.7515949602980072 ) ) ;
#35419 = AXIS2_PLACEMENT_3D ( 'NONE', #31053, #57395, #65234 ) ;
#35420 = CARTESIAN_POINT ( 'NONE',  ( -23.22374811570000119, 1411.084293947430069, 205.4313518788480053 ) ) ;
#35421 = CARTESIAN_POINT ( 'NONE',  ( 16.81460438480000263, 1415.425433635630043, 203.9301085955280257 ) ) ;
#35422 = CARTESIAN_POINT ( 'NONE',  ( 3.910001326520000209, 1486.362971887289859, 219.1796580760989741 ) ) ;
#35423 = CARTESIAN_POINT ( 'NONE',  ( 10.91379151888849819, 1479.765342082039979, 208.3165719332679942 ) ) ;
#35424 = CARTESIAN_POINT ( 'NONE',  ( -4.425709718559999041E-15, 1434.541746329560056, 150.4759714514979976 ) ) ;
#35425 = CARTESIAN_POINT ( 'NONE',  ( 20.78241041049849969, 1455.840303560959910, 207.1559588098690199 ) ) ;
#35426 = CARTESIAN_POINT ( 'NONE',  ( -5.513207816801510397, 1508.731180391289854, 216.5668095923579983 ) ) ;
#35427 = CARTESIAN_POINT ( 'NONE',  ( 19.12715434814980142, 1496.834837383639979, 222.0421819497279898 ) ) ;
#35429 = CARTESIAN_POINT ( 'NONE',  ( -9.171139168049998958, 1384.273561242960113, 200.0050165398689899 ) ) ;
#35428 = CARTESIAN_POINT ( 'NONE',  ( -22.76038230680000041, 1410.633847100929870, 211.2989740808880015 ) ) ;
#35430 = CARTESIAN_POINT ( 'NONE',  ( -5.026419929959999422, 1391.797186054590156, 203.6610981513489946 ) ) ;
#35431 = CARTESIAN_POINT ( 'NONE',  ( 9.803321272836790001, 1435.322606278559988, 208.6575614323569994 ) ) ;
#35432 = CARTESIAN_POINT ( 'NONE',  ( -10.69044905890000052, 1491.561357479690059, 211.7988311077089918 ) ) ;
#35433 = CARTESIAN_POINT ( 'NONE',  ( 10.16318987985490097, 1451.293190031329914, 206.5284763887880217 ) ) ;
#35434 = CARTESIAN_POINT ( 'NONE',  ( 3.829620113550000315, 1515.551704408389924, 206.7917118356089929 ) ) ;
#35435 = CARTESIAN_POINT ( 'NONE',  ( 2.286446325635000054, 1517.042661899400173, 204.4961520670869959 ) ) ;
#35436 = CARTESIAN_POINT ( 'NONE',  ( -7.980985505873261054, 1398.150102696605018, 219.3836182790206237 ) ) ;
#35437 = CARTESIAN_POINT ( 'NONE',  ( 0.000000000000000000, 1511.187213306747708, 209.1218459616979999 ) ) ;
#35438 = FACE_BOUND ( 'NONE', #11961, .T. ) ;
#35439 = CARTESIAN_POINT ( 'NONE',  ( -19.65671673259999963, 1468.978988229229799, 193.1983232643979704 ) ) ;
#35440 = DIRECTION ( 'NONE',  ( 0.000000000000000000, -0.02617694830788830015, 0.9996573249755569268 ) ) ;
#35441 = CARTESIAN_POINT ( 'NONE',  ( -11.53006918210525278, 1506.266512897565917, 207.3910517571966068 ) ) ;
#35443 = ORIENTED_EDGE ( 'NONE', *, *, #6434, .F. ) ;
#35442 = CARTESIAN_POINT ( 'NONE',  ( -65.41331928280889940, 1379.741107854490110, 275.4574184064960036 ) ) ;
#35444 = ORIENTED_EDGE ( 'NONE', *, *, #25315, .T. ) ;
#35445 = CARTESIAN_POINT ( 'NONE',  ( 11.20527203278069805, 1434.214488751450062, 151.6116235837919817 ) ) ;
#35446 = CARTESIAN_POINT ( 'NONE',  ( 21.35000886514773555, 1525.163527997504843, 183.8373093396160982 ) ) ;
#35447 = ORIENTED_EDGE ( 'NONE', *, *, #83922, .T. ) ;
#35448 = CARTESIAN_POINT ( 'NONE',  ( 18.66420869458043796, 1526.382868172863937, 185.4599087859680537 ) ) ;
#35449 = CARTESIAN_POINT ( 'NONE',  ( -21.03123196400000339, 1507.789098030929836, 192.1781279194979959 ) ) ;
#35450 = CARTESIAN_POINT ( 'NONE',  ( -7.767752774649999914, 1385.091807982149930, 218.9133695865889990 ) ) ;
#35452 = CARTESIAN_POINT ( 'NONE',  ( 13.54190757295939918, 1453.249853630250072, 224.6401645295789820 ) ) ;
#35451 = CARTESIAN_POINT ( 'NONE',  ( -1.393816646507350487, 1511.187213306747708, 243.1385343369520342 ) ) ;
#35453 = CARTESIAN_POINT ( 'NONE',  ( 17.16377242769999967, 1507.812853982129809, 231.0448963225979924 ) ) ;
#35454 = CARTESIAN_POINT ( 'NONE',  ( 12.21796603489999988, 1507.632479711529868, 184.8478369543980193 ) ) ;
#35455 = CARTESIAN_POINT ( 'NONE',  ( 10.11864553081269058, 1509.266411275488053, 236.5980910735531779 ) ) ;
#35456 = DIRECTION ( 'NONE',  ( 1.755985294532469921E-16, -1.000000000000000000, 1.338183447452831989E-16 ) ) ;
#35457 =( LENGTH_UNIT ( ) NAMED_UNIT ( * ) SI_UNIT ( .MILLI., .METRE. ) );
#35458 = CARTESIAN_POINT ( 'NONE',  ( -2.282915221395000138, 1516.876240617270014, 211.6158662526670184 ) ) ;
#35459 = CARTESIAN_POINT ( 'NONE',  ( 38.01446494478440030, 1436.977963747790000, 134.0999999969440069 ) ) ;
#35460 = CARTESIAN_POINT ( 'NONE',  ( -9.110776130009609730, 1423.030562184250130, 209.7485040796009912 ) ) ;
#35461 = CARTESIAN_POINT ( 'NONE',  ( 7.641097577974999666, 1512.520476835130012, 202.3618328102370185 ) ) ;
#35462 = VERTEX_POINT ( 'NONE', #18005 ) ;
#35463 = CARTESIAN_POINT ( 'NONE',  ( 13.54853135755140059, 1434.978863808960114, 149.0925490114800027 ) ) ;
#35464 =( NAMED_UNIT ( * ) SI_UNIT ( $, .STERADIAN. ) SOLID_ANGLE_UNIT ( ) );
#35465 = ORIENTED_EDGE ( 'NONE', *, *, #5484, .T. ) ;
#35466 = ORIENTED_EDGE ( 'NONE', *, *, #88999, .F. ) ;
#35467 = CARTESIAN_POINT ( 'NONE',  ( -7.284055456385000404, 1511.816633140279919, 215.8034048803770020 ) ) ;
#35468 = CARTESIAN_POINT ( 'NONE',  ( -1.229676403839999876, 1465.032347023129887, 236.8197607516979986 ) ) ;
#35469 = CARTESIAN_POINT ( 'NONE',  ( -8.142296919120433074, 1474.791439460570473, 202.8386750668462923 ) ) ;
#35470 = CARTESIAN_POINT ( 'NONE',  ( -2.872836660654999985, 1517.158319634930194, 216.8472181024670249 ) ) ;
#35471 = CARTESIAN_POINT ( 'NONE',  ( -0.7542027323512070502, 1465.241414061940077, 198.1437931916329944 ) ) ;
#35472 = CARTESIAN_POINT ( 'NONE',  ( 11.25476890810059949, 1422.124858124740058, 210.3410537449459810 ) ) ;
#35473 = CARTESIAN_POINT ( 'NONE',  ( -32.99886885496665911, 1379.635068102732703, 216.1939695130954249 ) ) ;
#35474 = CARTESIAN_POINT ( 'NONE',  ( 3.238415943299999711, 1465.057015839789983, 199.8093003563689933 ) ) ;
#35475 = CARTESIAN_POINT ( 'NONE',  ( -0.06018804149849999591, 1508.906897381529916, 238.6255503046979811 ) ) ;
#35476 = ORIENTED_EDGE ( 'NONE', *, *, #41765, .T. ) ;
#35477 = CARTESIAN_POINT ( 'NONE',  ( 6.546302742015000398, 1516.577434278289957, 206.6347425125669872 ) ) ;
#35478 = VERTEX_POINT ( 'NONE', #8505 ) ;
#35479 = CARTESIAN_POINT ( 'NONE',  ( 23.27833603578599764, 1440.913060387330006, 232.8848930007430056 ) ) ;
#35480 = CARTESIAN_POINT ( 'NONE',  ( -19.58834071409999922, 1508.062712279529933, 229.4587154835980130 ) ) ;
#35481 = VERTEX_POINT ( 'NONE', #9072 ) ;
#35482 = CARTESIAN_POINT ( 'NONE',  ( -6.455481540323650513, 1508.551704606160001, 202.2941615582640225 ) ) ;
#35483 = CARTESIAN_POINT ( 'NONE',  ( -14.50832503429999853, 1410.792323590329943, 190.4765598033980041 ) ) ;
#35484 = CARTESIAN_POINT ( 'NONE',  ( -24.38537946479999974, 1441.549228787309858, 211.3644968983080048 ) ) ;
#35485 = CARTESIAN_POINT ( 'NONE',  ( 1.044682716639319997, 1423.188007962369966, 192.5288407937300121 ) ) ;
#35486 = CARTESIAN_POINT ( 'NONE',  ( 0.0002643472464120411708, 1396.497912824548848, 196.7090272551392616 ) ) ;
#35487 = DIRECTION ( 'NONE',  ( -5.145681809797982184E-09, 0.03085823632287491500, -0.9995237712285994780 ) ) ;
#35488 = DIRECTION ( 'NONE',  ( 5.980589973904019347E-17, -1.000000000000000000, 1.736889445713099699E-16 ) ) ;
#35489 = CARTESIAN_POINT ( 'NONE',  ( 15.36997683531480874, 1435.038989812052023, 147.5081740258111722 ) ) ;
#35491 = CARTESIAN_POINT ( 'NONE',  ( 9.327651199099038948, 1434.415569083649871, 206.2244204008570136 ) ) ;
#35490 = CARTESIAN_POINT ( 'NONE',  ( -26.49915054198219622, 1499.844595131229880, 212.0142546687440301 ) ) ;
#35492 = AXIS2_PLACEMENT_3D ( 'NONE', #91047, #38443, #5955 ) ;
#35493 = CARTESIAN_POINT ( 'NONE',  ( 6.557909882634999299, 1516.908489800550115, 214.8995913655070069 ) ) ;
#35494 = TOROIDAL_SURFACE ( 'NONE', #3382, 14.90133124319999780, 0.5000000000000000000 ) ;
#35495 = CARTESIAN_POINT ( 'NONE',  ( -2.646857175475319846, 1429.116376473109995, 200.1321371505179911 ) ) ;
#35496 = DIRECTION ( 'NONE',  ( -0.7494985254689902066, 0.08460605218640301906, 0.6565773193259429874 ) ) ;
#35497 = EDGE_CURVE ( 'NONE', #69002, #64952, #102009, .T. ) ;
#35498 = AXIS2_PLACEMENT_3D ( 'NONE', #84105, #50527, #7405 ) ;
#35499 = CARTESIAN_POINT ( 'NONE',  ( 28.91076426840000124, 1509.890507619829805, 207.1524129226179980 ) ) ;
#35500 = CARTESIAN_POINT ( 'NONE',  ( -7.708770045145000083, 1516.524310051880093, 211.4128934593470035 ) ) ;
#35501 = CARTESIAN_POINT ( 'NONE',  ( -11.85130961024979968, 1482.142199958030233, 208.1561019704090256 ) ) ;
#35502 = CARTESIAN_POINT ( 'NONE',  ( -15.82940463150903732, 1486.087625934943844, 186.8622631807861012 ) ) ;
#35504 = ORIENTED_EDGE ( 'NONE', *, *, #29302, .T. ) ;
#35503 = CARTESIAN_POINT ( 'NONE',  ( -89.66056332210000335, 1386.526336894989981, 308.7176818193590293 ) ) ;
#35505 = CARTESIAN_POINT ( 'NONE',  ( 42.47353201039999959, 1448.912604704790056, 263.9447844666980245 ) ) ;
#35506 = EDGE_CURVE ( 'NONE', #90113, #58583, #88961, .T. ) ;
#35507 = CARTESIAN_POINT ( 'NONE',  ( -8.598884509784999963, 1512.314860040240092, 211.3567694112070114 ) ) ;
#35508 = CARTESIAN_POINT ( 'NONE',  ( 38.64637139974560398, 1443.913060387190171, 137.1864063390110005 ) ) ;
#35509 = CARTESIAN_POINT ( 'NONE',  ( -7.746307814384410406, 1509.115590816079930, 236.8131461681879841 ) ) ;
#35510 = CARTESIAN_POINT ( 'NONE',  ( -22.52134604649999972, 1451.600229533030188, 219.4799338534979825 ) ) ;
#35512 = CARTESIAN_POINT ( 'NONE',  ( 17.95636871770980036, 1410.547909248580027, 222.9459090208920031 ) ) ;
#35511 = CARTESIAN_POINT ( 'NONE',  ( 11.31015084829999928, 1432.869298927259933, 151.5208831616980092 ) ) ;
#35513 = CARTESIAN_POINT ( 'NONE',  ( 0.2676492203279999815, 1452.807100928730051, 189.1997072006980147 ) ) ;
#35514 = CARTESIAN_POINT ( 'NONE',  ( -108.5976781527699870, 1382.685102817129973, 310.7253367639360704 ) ) ;
#35515 = AXIS2_PLACEMENT_3D ( 'NONE', #22874, #73873, #97553 ) ;
#35516 = ORIENTED_EDGE ( 'NONE', *, *, #49464, .T. ) ;
#35517 = CARTESIAN_POINT ( 'NONE',  ( 6.937965660314999283, 1516.732530461250008, 204.1161457306970135 ) ) ;
#35518 = CARTESIAN_POINT ( 'NONE',  ( 0.5592746378849999811, 1405.719121701330096, 267.8539144989980514 ) ) ;
#35519 = LINE ( 'NONE', #60753, #73217 ) ;
#35520 = CARTESIAN_POINT ( 'NONE',  ( 12.64570686159999902, 1428.691483912829881, 223.9482794350980157 ) ) ;
#35521 = DIRECTION ( 'NONE',  ( 0.000000000000000000, 0.000000000000000000, -1.000000000000000000 ) ) ;
#35522 = CARTESIAN_POINT ( 'NONE',  ( 3.317744430799999922, 1467.314064772389884, 218.6468771502790105 ) ) ;
#35523 = CARTESIAN_POINT ( 'NONE',  ( 5.981720629350000706, 1449.156460935289942, 207.4142490612589995 ) ) ;
#35524 = CARTESIAN_POINT ( 'NONE',  ( -36.21648822516259969, 1440.913060387389805, 253.2446230051280054 ) ) ;
#35525 = DIRECTION ( 'NONE',  ( -0.6736849260863841948, 0.000000000000000000, 0.7390186874254148774 ) ) ;
#35526 = CARTESIAN_POINT ( 'NONE',  ( -1.453744412873089864, 1450.692426123599944, 154.2448216411129920 ) ) ;
#35527 = DIRECTION ( 'NONE',  ( -0.9996573249754487911, 0.02617694831201757000, 1.257327575352784523E-11 ) ) ;
#35528 = CARTESIAN_POINT ( 'NONE',  ( 10.50869459094269942, 1481.949074847140082, 210.5032414321599958 ) ) ;
#35529 = CARTESIAN_POINT ( 'NONE',  ( 3.005897003519999888, 1505.999189604289995, 221.1413980816990090 ) ) ;
#35530 = CARTESIAN_POINT ( 'NONE',  ( -8.557209110492459914, 1448.617779613390212, 212.3361752075699940 ) ) ;
#35531 = ORIENTED_EDGE ( 'NONE', *, *, #73425, .T. ) ;
#35532 = CARTESIAN_POINT ( 'NONE',  ( 20.39146254758223265, 1526.073434386618828, 185.1130326267048645 ) ) ;
#35533 = CARTESIAN_POINT ( 'NONE',  ( -1.273841231818057862, 1450.738619355563060, 181.8035796647308757 ) ) ;
#35534 = CARTESIAN_POINT ( 'NONE',  ( 9.755929852662839963, 1468.207539460409862, 206.7555844597239911 ) ) ;
#35535 = CARTESIAN_POINT ( 'NONE',  ( 11.10627834194573538, 1425.149160823644024, 138.4707484690964634 ) ) ;
#35536 = FACE_OUTER_BOUND ( 'NONE', #72105, .T. ) ;
#35537 = CARTESIAN_POINT ( 'NONE',  ( -29.52080282280000034, 1509.954550902929896, 211.0554093484379905 ) ) ;
#35538 = CARTESIAN_POINT ( 'NONE',  ( 7.721630276590000008, 1426.874396221100142, 211.9998969879490289 ) ) ;
#35539 = CARTESIAN_POINT ( 'NONE',  ( -13.59805687866929880, 1384.880812014989942, 219.1775672781149922 ) ) ;
#35540 = B_SPLINE_SURFACE_WITH_KNOTS ( 'NONE', 5, 1, ( 
 ( #85340, #84252 ),
 ( #84791, #101585 ),
 ( #76405, #8637 ),
 ( #75862, #66928 ),
 ( #42813, #51775 ),
 ( #23782, #59078 ) ),
 .UNSPECIFIED., .F., .F., .F.,
 ( 6, 6 ),
 ( 2, 2 ),
 ( 0.000000000000000000, 16.39065553909999906 ),
 ( 0.000000000000000000, 14.00000000000000000 ),
 .UNSPECIFIED. ) ;
#35541 = CARTESIAN_POINT ( 'NONE',  ( 19.53786426059019021, 1512.187213306747481, 181.5239794925693388 ) ) ;
#35542 = CARTESIAN_POINT ( 'NONE',  ( -9.721170047090000210, 1481.243685225789932, 204.9479232781289966 ) ) ;
#35543 = CARTESIAN_POINT ( 'NONE',  ( 18.89959486413309975, 1416.839692127159879, 210.6687135792209915 ) ) ;
#35544 = CARTESIAN_POINT ( 'NONE',  ( -10.18694299370419998, 1396.268796277229967, 204.7956743315450012 ) ) ;
#35545 = ORIENTED_EDGE ( 'NONE', *, *, #45772, .F. ) ;
#35546 = CARTESIAN_POINT ( 'NONE',  ( -16.83005542020710266, 1409.747738274599897, 225.5715775287220026 ) ) ;
#35547 = CARTESIAN_POINT ( 'NONE',  ( 4.906228319039999342, 1433.447543843880112, 150.0987928807979870 ) ) ;
#35548 = VERTEX_POINT ( 'NONE', #35941 ) ;
#35549 = ORIENTED_EDGE ( 'NONE', *, *, #68125, .T. ) ;
#35550 = CARTESIAN_POINT ( 'NONE',  ( 4.900006679340000559, 1499.255191946190052, 229.7873568473989963 ) ) ;
#35551 = FACE_OUTER_BOUND ( 'NONE', #13015, .T. ) ;
#35553 = CARTESIAN_POINT ( 'NONE',  ( 0.9724418386591719976, 1456.734366788370153, 219.6981812980549762 ) ) ;
#35552 = CARTESIAN_POINT ( 'NONE',  ( 10.38444639019999904, 1425.403467236129927, 94.99627158069790767 ) ) ;
#35554 = DIRECTION ( 'NONE',  ( 0.000000000000000000, 0.000000000000000000, 1.000000000000000000 ) ) ;
#35555 = CARTESIAN_POINT ( 'NONE',  ( -11.81044603969999862, 1433.053321433509836, 150.5679240076979966 ) ) ;
#35556 = CARTESIAN_POINT ( 'NONE',  ( -2.790873196810775614, 1419.912297037458984, 186.1247558487485776 ) ) ;
#35557 = CONICAL_SURFACE ( 'NONE', #81993, 6.911399307709998219, 0.04363323129990067523 ) ;
#35558 = CARTESIAN_POINT ( 'NONE',  ( 7.526645696320000134, 1425.452156459670050, 212.1942742985490042 ) ) ;
#35559 = CARTESIAN_POINT ( 'NONE',  ( -3.005245951399999615, 1450.300005596989877, 188.5532306447990152 ) ) ;
#35560 = CARTESIAN_POINT ( 'NONE',  ( 7.722835720109999080, 1509.114495076129970, 181.4225071154979787 ) ) ;
#35561 = CARTESIAN_POINT ( 'NONE',  ( 3.416038303169999679, 1449.507431040339952, 184.0497570492980230 ) ) ;
#35562 = CARTESIAN_POINT ( 'NONE',  ( 9.813910351400000565, 1364.017814053650000, 207.6218459616989946 ) ) ;
#35564 = ORIENTED_EDGE ( 'NONE', *, *, #64522, .T. ) ;
#35563 = CARTESIAN_POINT ( 'NONE',  ( 7.016154481710000113, 1454.841981631690032, 216.5674988146290048 ) ) ;
#35565 = ORIENTED_EDGE ( 'NONE', *, *, #4126, .T. ) ;
#35566 = CARTESIAN_POINT ( 'NONE',  ( 18.18137294690000161, 1507.608465324829922, 188.5297611294979845 ) ) ;
#35567 = AXIS2_PLACEMENT_3D ( 'NONE', #53292, #79048, #80120 ) ;
#35568 = EDGE_CURVE ( 'NONE', #85936, #32175, #10173, .T. ) ;
#35569 = CARTESIAN_POINT ( 'NONE',  ( 13.77266209894789917, 1517.151704408390060, 201.2043266506040027 ) ) ;
#35570 = CARTESIAN_POINT ( 'NONE',  ( -0.4870700791739999702, 1473.589435998730096, 270.3925729411980114 ) ) ;
#35571 = CARTESIAN_POINT ( 'NONE',  ( 7.253697669526002478, 1500.197240720463924, 200.3293451155131493 ) ) ;
#35572 = CARTESIAN_POINT ( 'NONE',  ( -120.1712171740599473, 1306.483669372790928, 302.4928703550302203 ) ) ;
#35573 = B_SPLINE_CURVE_WITH_KNOTS ( 'NONE', 3,
 ( #60592, #27508, #94712, #102541, #61695, #17988, #26969, #16324, #50525, #86314, #25834, #77919, #1226 ),
 .UNSPECIFIED., .F., .F.,
 ( 4, 2, 2, 1, 2, 2, 4 ),
 ( 0.000000000000000000, 0.2500000000000023870, 0.3750000000000035527, 0.4375000000000029421, 0.4687500000000018319, 0.5000000000000006661, 1.000000000000000000 ),
 .UNSPECIFIED. ) ;
#35575 = EDGE_CURVE ( 'NONE', #37122, #20697, #23528, .T. ) ;
#35574 = CARTESIAN_POINT ( 'NONE',  ( -32.21733215213330936, 1523.844782250843309, 201.4553020982646387 ) ) ;
#35576 = CARTESIAN_POINT ( 'NONE',  ( 0.5358887729754751028, 1475.906136617699985, 197.6669786481479889 ) ) ;
#35577 = CARTESIAN_POINT ( 'NONE',  ( -33.93389098834200013, 1451.576030851350197, 135.5842732458419846 ) ) ;
#35578 = ADVANCED_FACE ( 'NONE', ( #59495 ), #33934, .T. ) ;
#35579 = SURFACE_STYLE_USAGE ( .BOTH. , #60817 ) ;
#35580 = CARTESIAN_POINT ( 'NONE',  ( -2.500000000000529798, 1448.894380907979894, 155.6080925131469996 ) ) ;
#35581 = CARTESIAN_POINT ( 'NONE',  ( 7.979399411837515999, 1369.012103654667044, 210.6218459617030021 ) ) ;
#35582 = CARTESIAN_POINT ( 'NONE',  ( 12.63607377350000149, 1408.833611601630082, 216.0564899030879928 ) ) ;
#35583 = CARTESIAN_POINT ( 'NONE',  ( -0.7664924707717509778, 1406.506770649930104, 269.4987574733809765 ) ) ;
#35584 = CARTESIAN_POINT ( 'NONE',  ( -14.41479079490409987, 1436.126800610740020, 149.9515762605120131 ) ) ;
#35585 = EDGE_LOOP ( 'NONE', ( #82727, #101837, #20281, #17507, #99184 ) ) ;
#35586 = CARTESIAN_POINT ( 'NONE',  ( -10.96892109859999920, 1432.312127186730095, 151.7701099962980038 ) ) ;
#35587 = CARTESIAN_POINT ( 'NONE',  ( 13.22002162090000077, 1442.920576605979932, 188.2908536790980065 ) ) ;
#35588 = ORIENTED_EDGE ( 'NONE', *, *, #12098, .T. ) ;
#35589 = VERTEX_POINT ( 'NONE', #108499 ) ;
#35590 = DIRECTION ( 'NONE',  ( 1.755985294532464991E-16, -1.000000000000000000, 1.338183447452830017E-16 ) ) ;
#35591 = CARTESIAN_POINT ( 'NONE',  ( -8.622403150219998480, 1362.632156860360055, 207.6218459616989946 ) ) ;
#35592 = CIRCLE ( 'NONE', #96342, 0.5000000000000000000 ) ;
#35593 = CARTESIAN_POINT ( 'NONE',  ( -1.120543735785000106, 1517.073005577650065, 213.1661658574570026 ) ) ;
#35594 = CARTESIAN_POINT ( 'NONE',  ( 3.853756123904999775, 1510.775363762149937, 216.6800758355570053 ) ) ;
#35595 = ORIENTED_EDGE ( 'NONE', *, *, #60421, .F. ) ;
#35596 = CARTESIAN_POINT ( 'NONE',  ( -73.44525057620001007, 1375.641846743739961, 283.9849195986590189 ) ) ;
#35597 = CARTESIAN_POINT ( 'NONE',  ( 7.388977406289999550, 1415.087797054229895, 224.7253375031980056 ) ) ;
#35598 = CARTESIAN_POINT ( 'NONE',  ( 1.706797785944999868, 1517.164987839469859, 203.3324512698969784 ) ) ;
#35599 = CARTESIAN_POINT ( 'NONE',  ( -27.59699679970000119, 1509.623160989430062, 202.9201204474879887 ) ) ;
#35600 = CARTESIAN_POINT ( 'NONE',  ( -1.514732356010000114, 1507.625766696930214, 232.0393368578980073 ) ) ;
#35601 = CARTESIAN_POINT ( 'NONE',  ( 11.41977518000482128, 1433.011620482430772, 151.3551162631975728 ) ) ;
#35602 = CARTESIAN_POINT ( 'NONE',  ( -66.36363792712158727, 1384.713802119680167, 258.0891102980660321 ) ) ;
#35603 = CARTESIAN_POINT ( 'NONE',  ( -7.271052316819551109, 1517.151704408390060, 225.3404165491008371 ) ) ;
#35604 = CARTESIAN_POINT ( 'NONE',  ( -10.16240527536719895, 1472.558926193989919, 209.8189312950259762 ) ) ;
#35605 = ORIENTED_EDGE ( 'NONE', *, *, #93254, .T. ) ;
#35606 = LINE ( 'NONE', #96634, #42226 ) ;
#35607 = CARTESIAN_POINT ( 'NONE',  ( 30.31940284292420174, 1512.187213306747481, 222.4933038710543087 ) ) ;
#35608 = CARTESIAN_POINT ( 'NONE',  ( 20.07779891821229867, 1477.280519013530011, 225.0994067720200178 ) ) ;
#35609 = CARTESIAN_POINT ( 'NONE',  ( -25.36277544819999719, 1435.571748013670003, 136.4218649723979979 ) ) ;
#35610 = CARTESIAN_POINT ( 'NONE',  ( 7.724732408895000013, 1517.133889586189980, 212.3822030989969960 ) ) ;
#35611 = CONICAL_SURFACE ( 'NONE', #33772, 7.500000000000000000, 0.02617993877989872875 ) ;
#35612 = CARTESIAN_POINT ( 'NONE',  ( -68.36902399430000798, 1379.746974201359990, 279.2217794733590495 ) ) ;
#35613 = DIRECTION ( 'NONE',  ( -1.000000000000000000, 0.000000000000000000, 0.000000000000000000 ) ) ;
#35614 = CARTESIAN_POINT ( 'NONE',  ( -12.98226561589999939, 1414.913060387329779, 219.9156672276980089 ) ) ;
#35615 = CARTESIAN_POINT ( 'NONE',  ( -21.51338411143810347, 1505.551551846900111, 209.1218200089510333 ) ) ;
#35616 = CARTESIAN_POINT ( 'NONE',  ( -5.788691363644999477, 1517.157901477309906, 207.9987443536870160 ) ) ;
#35617 = VERTEX_POINT ( 'NONE', #101733 ) ;
#35618 = CARTESIAN_POINT ( 'NONE',  ( 2.500000000000000000, 1434.635760835609972, 157.5644327210980293 ) ) ;
#35619 = CARTESIAN_POINT ( 'NONE',  ( 3.018077178498919544, 1440.716223221779728, 157.2134753452489804 ) ) ;
#35620 = CARTESIAN_POINT ( 'NONE',  ( -43.07689360599999873, 1384.903938649839802, 247.5074275424589985 ) ) ;
#35621 = EDGE_LOOP ( 'NONE', ( #88782, #36241, #23209, #99049, #4664 ) ) ;
#35622 = CARTESIAN_POINT ( 'NONE',  ( -16.85980286139739803, 1385.288128647810026, 219.8538196921649899 ) ) ;
#35623 = AXIS2_PLACEMENT_3D ( 'NONE', #95335, #29234, #61760 ) ;
#35624 = CARTESIAN_POINT ( 'NONE',  ( -11.82942659101509975, 1491.433867479470109, 205.8513465834750207 ) ) ;
#35625 = CARTESIAN_POINT ( 'NONE',  ( 12.20245528595089901, 1434.091338913249956, 149.6907156280659876 ) ) ;
#35626 = EDGE_CURVE ( 'NONE', #76715, #27116, #57587, .T. ) ;
#35627 = B_SPLINE_SURFACE_WITH_KNOTS ( 'NONE', 5, 5, ( 
 ( #42139, #34829, #102565, #70136, #42689, #26422 ),
 ( #1247, #52209, #69016, #34281, #86335, #60059 ),
 ( #69574, #103693, #26993, #61182, #18560, #95299 ),
 ( #61721, #95843, #50548, #55510, #54967, #63383 ),
 ( #54427, #45473, #97499, #11305, #106449, #79615 ),
 ( #81231, #2919, #46567, #28087, #88560, #37037 ),
 ( #38136, #4011, #79069, #11843, #96403, #70686 ),
 ( #20767, #89093, #106990, #29732, #98033, #20226 ),
 ( #10751, #38680, #46015, #80145, #96961, #104799 ),
 ( #53885, #44922, #2374, #105353, #36490, #62274 ),
 ( #71231, #3464, #37593, #28644, #71794, #19680 ),
 ( #12380, #105913, #29193, #72318, #88021, #21305 ),
 ( #80701, #62847, #63918, #89638, #12925, #47105 ),
 ( #4547, #72856, #30278, #64471, #19111, #53314 ),
 ( #87456, #65006, #438, #7699, #90176, #33435 ) ),
 .UNSPECIFIED., .F., .F., .F.,
 ( 6, 3, 3, 3, 6 ),
 ( 6, 6 ),
 ( 14.45298335000000023, 21.98568536959999875, 27.70858623979999891, 30.13845758540000119, 37.41853765350000316 ),
 ( 0.000000000000000000, 1.621616996280000000 ),
 .UNSPECIFIED. ) ;
#35628 = CARTESIAN_POINT ( 'NONE',  ( 18.15210693040249978, 1469.010815795120152, 228.4209498636830062 ) ) ;
#35629 = CARTESIAN_POINT ( 'NONE',  ( -23.50962832835050165, 1509.033178799369807, 224.0176340712529850 ) ) ;
#35630 = CARTESIAN_POINT ( 'NONE',  ( -2.431089449619999954, 1409.932888510029898, 186.5211211122979762 ) ) ;
#35631 = CARTESIAN_POINT ( 'NONE',  ( 0.05606136413419999381, 1409.080515703730043, 232.6633760207980117 ) ) ;
#35632 = CARTESIAN_POINT ( 'NONE',  ( -19.63722818156799832, 1522.051704408389924, 200.0074286628000095 ) ) ;
#35634 = CARTESIAN_POINT ( 'NONE',  ( -2.900970950180000063, 1421.449121440929957, 184.2745271147979906 ) ) ;
#35633 = CARTESIAN_POINT ( 'NONE',  ( -6.939219520934999608, 1516.783701990830195, 214.9027072062869763 ) ) ;
#35635 = CARTESIAN_POINT ( 'NONE',  ( 19.35070455179999982, 1509.010601610729964, 188.1735489204979785 ) ) ;
#35636 = CARTESIAN_POINT ( 'NONE',  ( 2.872700517194999748, 1516.559109716219837, 216.8315272385270021 ) ) ;
#35637 = ORIENTED_EDGE ( 'NONE', *, *, #42012, .F. ) ;
#35638 = CARTESIAN_POINT ( 'NONE',  ( -11.22551998621869807, 1414.913060387399810, 197.5794005584399997 ) ) ;
#35639 = CARTESIAN_POINT ( 'NONE',  ( -20.21023357682352994, 1526.107880201381477, 184.5539505003309841 ) ) ;
#35640 = ORIENTED_EDGE ( 'NONE', *, *, #47344, .F. ) ;
#35641 = AXIS2_PLACEMENT_3D ( 'NONE', #8238, #107542, #41857 ) ;
#35642 = CARTESIAN_POINT ( 'NONE',  ( 4.401092509980000678, 1420.174153530429976, 185.7217844323980103 ) ) ;
#35643 = AXIS2_PLACEMENT_3D ( 'NONE', #95567, #69845, #79329 ) ;
#35644 =( BOUNDED_SURFACE ( )  B_SPLINE_SURFACE ( 3, 2, ( 
 ( #86340, #2926, #71236 ),
 ( #17451, #94181, #95304 ),
 ( #85789, #11310, #9625 ),
 ( #44927, #36496, #96410 ) ),
 .UNSPECIFIED., .F., .F., .F. ) 
 B_SPLINE_SURFACE_WITH_KNOTS ( ( 4, 4 ),
 ( 3, 3 ),
 ( 0.000000000000000000, 0.0002960034161023851105 ),
 ( 0.000000000000000000, 1.000000000000000000 ),
 .UNSPECIFIED. ) 
 GEOMETRIC_REPRESENTATION_ITEM ( )  RATIONAL_B_SPLINE_SURFACE ( (
 ( 1.000000000000000000, 0.8070209408750127489, 1.000000000000000000),
 ( 1.000000000000000000, 0.8071723757218264295, 1.000000000000000000),
 ( 1.000000000000000000, 0.8072480346917805250, 1.000000000000000000),
 ( 1.000000000000000000, 0.8072480644198094524, 1.000000000000000000) ) ) 
 REPRESENTATION_ITEM ( '' )  SURFACE ( )  );
#35645 = CARTESIAN_POINT ( 'NONE',  ( -8.169799973510000868, 1501.392344667289990, 208.3166649180830063 ) ) ;
#35646 = CARTESIAN_POINT ( 'NONE',  ( 7.395102123895940238, 1511.068351247050032, 202.7464954504410173 ) ) ;
#35647 = UNCERTAINTY_MEASURE_WITH_UNIT (LENGTH_MEASURE( 1.000000000000000082E-05 ), #229, 'distance_accuracy_value', 'NONE');
#35648 = CARTESIAN_POINT ( 'NONE',  ( 3.745877440767119815, 1424.347276005310050, 191.5446012222820116 ) ) ;
#35649 = CARTESIAN_POINT ( 'NONE',  ( -30.04019103850641770, 1524.756004293092019, 195.9352227457331139 ) ) ;
#35650 = CARTESIAN_POINT ( 'NONE',  ( 230.7985005798999794, 11216.44053380570040, -1757.088479869530147 ) ) ;
#35651 = CARTESIAN_POINT ( 'NONE',  ( 17.38235991649999690, 1414.983773854429955, 210.5633853152779977 ) ) ;
#35652 = CARTESIAN_POINT ( 'NONE',  ( -17.95544320140000139, 1424.506778464429999, 226.1749991304979801 ) ) ;
#35653 = CARTESIAN_POINT ( 'NONE',  ( -19.60102139359999995, 1435.996833568079865, 145.7756697456979964 ) ) ;
#35654 = CARTESIAN_POINT ( 'NONE',  ( -9.788350359310001636, 1441.600846913620217, 148.8293326998980035 ) ) ;
#35655 = CARTESIAN_POINT ( 'NONE',  ( -11.78824854703250047, 1522.051704408389924, 206.8304425649369875 ) ) ;
#35657 = CARTESIAN_POINT ( 'NONE',  ( -19.08445480129999794, 1440.913060387330006, 209.8212738029720299 ) ) ;
#35656 = CARTESIAN_POINT ( 'NONE',  ( 1.052431931509999918, 1415.163755984130148, 191.3800010946980024 ) ) ;
#35658 = CARTESIAN_POINT ( 'NONE',  ( 6.036759152895515790, 1509.035273823006037, 201.6612097352038120 ) ) ;
#35659 = ORIENTED_EDGE ( 'NONE', *, *, #81716, .F. ) ;
#35660 = CARTESIAN_POINT ( 'NONE',  ( 1.556370309037290012, 1414.996442620790276, 191.7142051069610034 ) ) ;
#35661 = CARTESIAN_POINT ( 'NONE',  ( 24.83969286159999967, 1449.817299431849960, 207.3631499707580019 ) ) ;
#35662 = ADVANCED_FACE ( 'NONE', ( #59223 ), #8833, .F. ) ;
#35663 = CARTESIAN_POINT ( 'NONE',  ( -23.87982329980000173, 1436.855522858850236, 211.6538958347979928 ) ) ;
#35664 = CARTESIAN_POINT ( 'NONE',  ( 9.651066088509999474, 1425.440658930580184, 195.4941615409990163 ) ) ;
#35665 = VECTOR ( 'NONE', #66914, 1000.000000000000000 ) ;
#35666 = CARTESIAN_POINT ( 'NONE',  ( -18.28985832939523348, 1522.051704408389924, 198.5293912879491529 ) ) ;
#35667 = B_SPLINE_SURFACE_WITH_KNOTS ( 'NONE', 5, 5, ( 
 ( #32775, #91025, #73709, #15411, #66959, #74802, #24365, #58551, #50157 ),
 ( #110042, #56344, #32234, #5933, #65304, #22694, #40079, #13751, #66414 ),
 ( #107834, #57462, #91588, #14312, #48503, #14863, #52913, #16499, #42843 ),
 ( #59108, #60205, #18172, #44505, #18717, #59654, #87045, #43950, #311 ),
 ( #26576, #101613, #69730, #77005, #17602, #26008, #61333, #78652, #68611 ),
 ( #50688, #60773, #10333, #25459, #9784, #94898, #94324, #103849, #1395 ) ),
 .UNSPECIFIED., .F., .F., .F.,
 ( 6, 6 ),
 ( 6, 3, 6 ),
 ( 25.36855762109999901, 27.09121026449999903 ),
 ( 0.000000000000000000, 1.000000000000000000, 2.000000000000000000 ),
 .UNSPECIFIED. ) ;
#35668 = CARTESIAN_POINT ( 'NONE',  ( 29.13898522073297315, 1526.069472839380978, 221.1027213634262409 ) ) ;
#35669 = CARTESIAN_POINT ( 'NONE',  ( -11.39266988268109948, 1470.664952754889782, 209.5618712138449951 ) ) ;
#35670 = DIRECTION ( 'NONE',  ( 0.000000000000000000, 0.000000000000000000, -1.000000000000000000 ) ) ;
#35671 = CARTESIAN_POINT ( 'NONE',  ( -8.627771016562100215, 1437.492617161759881, 228.3379561119689924 ) ) ;
#35672 = CARTESIAN_POINT ( 'NONE',  ( -98.51084969631571653, 1383.764957257319793, 310.4650094518850096 ) ) ;
#35673 = B_SPLINE_CURVE_WITH_KNOTS ( 'NONE', 3,
 ( #77215, #24007, #94535, #32446, #35752, #61529, #105166, #78301, #28457, #70491, #3280, #10551, #71044, #105730 ),
 .UNSPECIFIED., .F., .F.,
 ( 4, 2, 1, 1, 1, 1, 2, 2, 4 ),
 ( 0.000000000000000000, 0.2499999999998150368, 0.3749999999997225553, 0.4374999999996475597, 0.4687499999995786149, 0.4843749999995755062, 0.4921874999995717870, 0.4999999999995680677, 1.000000000000000000 ),
 .UNSPECIFIED. ) ;
#35674 = CARTESIAN_POINT ( 'NONE',  ( 16.60876200430000083, 1451.097362684130076, 149.1934168744979843 ) ) ;
#35675 = CARTESIAN_POINT ( 'NONE',  ( -0.8265242355799999885, 1408.941923249630008, 187.0792671738979891 ) ) ;
#35677 = ORIENTED_EDGE ( 'NONE', *, *, #711, .T. ) ;
#35676 = CARTESIAN_POINT ( 'NONE',  ( 23.19217488219999979, 1509.011520754329922, 193.6160623652979780 ) ) ;
#35678 = CARTESIAN_POINT ( 'NONE',  ( -1.547463840030000037, 1414.913060387329779, 225.9340782259980074 ) ) ;
#35679 = CARTESIAN_POINT ( 'NONE',  ( -67.57883611510000321, 1382.334558834929794, 291.7886434181590403 ) ) ;
#35680 = CARTESIAN_POINT ( 'NONE',  ( -14.72209156862839841, 1419.171754436449874, 213.6412557114610138 ) ) ;
#35681 = ORIENTED_EDGE ( 'NONE', *, *, #12765, .T. ) ;
#35682 = ORIENTED_EDGE ( 'NONE', *, *, #23915, .F. ) ;
#35683 = CARTESIAN_POINT ( 'NONE',  ( 20.30812341819380151, 1509.558769329250026, 230.1713298670660208 ) ) ;
#35684 = CARTESIAN_POINT ( 'NONE',  ( 9.698064461892839105, 1462.705242386489999, 208.0596150282290182 ) ) ;
#35685 = CARTESIAN_POINT ( 'NONE',  ( 40.17126634324269929, 1442.450104387399733, 136.9828420844469861 ) ) ;
#35687 = CARTESIAN_POINT ( 'NONE',  ( -12.45246145670000004, 1471.374038867429817, 259.9010043778980048 ) ) ;
#35686 = FACE_BOUND ( 'NONE', #108423, .T. ) ;
#35688 = B_SPLINE_CURVE_WITH_KNOTS ( 'NONE', 4,
 ( #76692, #15113, #49303, #83428, #68877, #24603, #100770, #50954, #75061 ),
 .UNSPECIFIED., .F., .F.,
 ( 5, 4, 5 ),
 ( 0.000000000000000000, 0.9999834295456402344, 1.000000000000000000 ),
 .UNSPECIFIED. ) ;
#35689 = CARTESIAN_POINT ( 'NONE',  ( -4.535936068263819898, 1495.192894671210070, 197.6626227834830161 ) ) ;
#35690 = CARTESIAN_POINT ( 'NONE',  ( -108.3255562700000070, 1381.229067324740072, 298.1483132478589937 ) ) ;
#35691 = CARTESIAN_POINT ( 'NONE',  ( 25.60002290280000281, 1509.583810695030024, 197.6050161354980048 ) ) ;
#35692 = CARTESIAN_POINT ( 'NONE',  ( -20.57706974239999909, 1485.807236340330064, 191.5873737050980026 ) ) ;
#35693 = EDGE_CURVE ( 'NONE', #13874, #237, #8225, .T. ) ;
#35694 = CARTESIAN_POINT ( 'NONE',  ( 2.241718320410000409, 1410.369684904329915, 185.5035919006979839 ) ) ;
#35695 = CARTESIAN_POINT ( 'NONE',  ( 6.301535050710000085, 1423.297843521130062, 186.2731961210980103 ) ) ;
#35696 = CARTESIAN_POINT ( 'NONE',  ( -6.823170074189999212, 1439.352238415810007, 154.2706163447979861 ) ) ;
#35697 = CARTESIAN_POINT ( 'NONE',  ( -9.204027750931148333, 1450.286637959580048, 208.6661583415359758 ) ) ;
#35698 = CARTESIAN_POINT ( 'NONE',  ( -16.40172556159690131, 1420.659342363810083, 203.2854767675109997 ) ) ;
#35699 = CARTESIAN_POINT ( 'NONE',  ( -3.134276369640000226, 1452.365440490629908, 153.7789987939979994 ) ) ;
#35700 = CARTESIAN_POINT ( 'NONE',  ( 3.195005116169999937, 1472.592485613090048, 218.8132852216689912 ) ) ;
#35701 = ORIENTED_EDGE ( 'NONE', *, *, #65823, .F. ) ;
#35702 = FACE_OUTER_BOUND ( 'NONE', #56549, .T. ) ;
#35703 = EDGE_CURVE ( 'NONE', #77632, #95724, #84932, .T. ) ;
#35704 = CARTESIAN_POINT ( 'NONE',  ( 18.25820950609999826, 1474.753073108990066, 194.7346205266990182 ) ) ;
#35705 = CARTESIAN_POINT ( 'NONE',  ( -39.05686162770000180, 1453.566290948429923, 270.0278499002980084 ) ) ;
#35706 = CARTESIAN_POINT ( 'NONE',  ( -26.51885021291319688, 1446.534126691539996, 137.5835072909900134 ) ) ;
#35707 = CARTESIAN_POINT ( 'NONE',  ( 9.443064477949999258, 1434.540978515130064, 153.1670680800980051 ) ) ;
#35708 = ADVANCED_FACE ( 'NONE', ( #75474 ), #58660, .T. ) ;
#35709 = DIRECTION ( 'NONE',  ( -0.2054769195713296581, 0.000000000000000000, -0.9786619618251632957 ) ) ;
#35710 = VECTOR ( 'NONE', #68500, 1000.000000000000227 ) ;
#35711 = CARTESIAN_POINT ( 'NONE',  ( 7.612906430609999830, 1431.113060387329824, 191.6937606090980069 ) ) ;
#35712 = CARTESIAN_POINT ( 'NONE',  ( 2.901685312356649948, 1409.503309903549962, 231.2713400696559916 ) ) ;
#35713 = FACE_OUTER_BOUND ( 'NONE', #82849, .T. ) ;
#35714 = CARTESIAN_POINT ( 'NONE',  ( -3.251704830740000052, 1417.670526751729994, 234.4799080884979787 ) ) ;
#35715 = EDGE_CURVE ( 'NONE', #98535, #88625, #56178, .T. ) ;
#35716 = CARTESIAN_POINT ( 'NONE',  ( -1.076831829273358521, 1484.840516514630508, 182.1570766342005072 ) ) ;
#35717 = CARTESIAN_POINT ( 'NONE',  ( -6.359819428916967610, 1360.120001944986825, 210.6218459617030021 ) ) ;
#35718 = CARTESIAN_POINT ( 'NONE',  ( -45.92274223606419525, 1438.266996619100155, 266.6811736395359844 ) ) ;
#35719 = DIRECTION ( 'NONE',  ( -0.9531156431133573914, 0.2972425205391840963, 0.05672261309322752798 ) ) ;
#35720 = AXIS2_PLACEMENT_3D ( 'NONE', #44554, #10951, #61931 ) ;
#35721 = VERTEX_POINT ( 'NONE', #75999 ) ;
#35722 = CARTESIAN_POINT ( 'NONE',  ( 23.61230825720000226, 1435.322028862560046, 137.2857987807979896 ) ) ;
#35723 = EDGE_CURVE ( 'NONE', #104032, #42951, #44299, .T. ) ;
#35724 = VERTEX_POINT ( 'NONE', #96108 ) ;
#35725 = CARTESIAN_POINT ( 'NONE',  ( 5.013429356055000063, 1517.123342927159911, 210.2437967141769946 ) ) ;
#35726 = CARTESIAN_POINT ( 'NONE',  ( -6.694418385159999652, 1473.791160286789818, 199.7891180969089930 ) ) ;
#35727 = CARTESIAN_POINT ( 'NONE',  ( -27.46336423809769656, 1441.403115911309897, 137.3061811715859903 ) ) ;
#35728 = CARTESIAN_POINT ( 'NONE',  ( -11.07444842074230174, 1415.954755714380099, 195.9645819946510130 ) ) ;
#35729 = TOROIDAL_SURFACE ( 'NONE', #8854, 1.000000000000000000, 1.000000000000000000 ) ;
#35730 = CARTESIAN_POINT ( 'NONE',  ( -2.128846521502799849, 1496.797177652799974, 221.3100224611679891 ) ) ;
#35731 = ORIENTED_EDGE ( 'NONE', *, *, #78858, .F. ) ;
#35732 = CARTESIAN_POINT ( 'NONE',  ( -14.53241430329999773, 1470.815019615729852, 194.7137864531979972 ) ) ;
#35734 = CARTESIAN_POINT ( 'NONE',  ( 13.61940320949999972, 1452.819910076330189, 194.9772319796979900 ) ) ;
#35733 = CARTESIAN_POINT ( 'NONE',  ( 27.68253994085160130, 1507.989615297080036, 207.6661388942010262 ) ) ;
#35735 = EDGE_CURVE ( 'NONE', #57941, #98890, #3912, .T. ) ;
#35736 = CARTESIAN_POINT ( 'NONE',  ( 1.804213551060599885, 1410.351307734219972, 232.1928989352460064 ) ) ;
#35737 = CARTESIAN_POINT ( 'NONE',  ( -11.47928298387556012, 1425.866406702411268, 139.0912110491933333 ) ) ;
#35738 = CARTESIAN_POINT ( 'NONE',  ( -22.98659938915999845, 1452.110350648670192, 138.7940535307059804 ) ) ;
#35739 = EDGE_CURVE ( 'NONE', #36610, #104032, #53586, .T. ) ;
#35740 = CARTESIAN_POINT ( 'NONE',  ( -9.731514810505409230, 1440.165830278139993, 206.7233373073800067 ) ) ;
#35741 = ORIENTED_EDGE ( 'NONE', *, *, #7683, .T. ) ;
#35742 = CARTESIAN_POINT ( 'NONE',  ( -1.222390855309730018, 1409.214342690750073, 270.3713430301190215 ) ) ;
#35743 = CARTESIAN_POINT ( 'NONE',  ( 6.935801261535000428, 1516.621991115350056, 207.9918434378369909 ) ) ;
#35744 = CARTESIAN_POINT ( 'NONE',  ( 8.888454490430000021, 1417.713827340430043, 230.5629018249979652 ) ) ;
#35745 = CARTESIAN_POINT ( 'NONE',  ( -9.833393186232889605, 1517.051704408389924, 212.5077547680540135 ) ) ;
#35747 = EDGE_LOOP ( 'NONE', ( #70987, #79939, #30361, #29790, #10706 ) ) ;
#35746 = CARTESIAN_POINT ( 'NONE',  ( -7.408371670602375225, 1365.603856542280710, 209.6218459617148824 ) ) ;
#35748 = EDGE_LOOP ( 'NONE', ( #87195, #31911, #17268, #50597 ) ) ;
#35749 = ADVANCED_FACE ( 'NONE', ( #17712 ), #41050, .T. ) ;
#35750 = CARTESIAN_POINT ( 'NONE',  ( -23.77291164573799875, 1410.729768559269814, 210.1269042920389722 ) ) ;
#35751 = CARTESIAN_POINT ( 'NONE',  ( -4.653283256210000829, 1425.827074144530116, 186.2156745063980168 ) ) ;
#35752 = CARTESIAN_POINT ( 'NONE',  ( -11.33168998458564936, 1437.952585642965687, 152.0540813750432676 ) ) ;
#35753 = VECTOR ( 'NONE', #25981, 1000.000000000000000 ) ;
#35754 = CARTESIAN_POINT ( 'NONE',  ( 2.372478608332516892, 1522.382868172863937, 174.8996806668726549 ) ) ;
#35755 = EDGE_CURVE ( 'NONE', #87953, #104164, #109725, .T. ) ;
#35756 = CARTESIAN_POINT ( 'NONE',  ( -20.98880188002820191, 1506.431317093110010, 192.2210660023540072 ) ) ;
#35757 = CARTESIAN_POINT ( 'NONE',  ( -17.75051042830000014, 1425.821874560129800, 226.3520932680980025 ) ) ;
#35758 = CARTESIAN_POINT ( 'NONE',  ( 36.69248205205470015, 1461.665376385029958, 269.0208840940840105 ) ) ;
#35759 = CARTESIAN_POINT ( 'NONE',  ( -8.798117652420820889, 1465.157268619798060, 232.9151898438935575 ) ) ;
#35760 = CARTESIAN_POINT ( 'NONE',  ( 8.723378431209999562, 1446.953229722669903, 186.0446995693979773 ) ) ;
#35761 = CARTESIAN_POINT ( 'NONE',  ( 1.119439089684999944, 1517.026534522949987, 205.8528207963470038 ) ) ;
#35762 = ORIENTED_EDGE ( 'NONE', *, *, #76649, .F. ) ;
#35763 = CARTESIAN_POINT ( 'NONE',  ( 19.03319670683364606, 1457.114807116183783, 226.2774458981556052 ) ) ;
#35764 = CARTESIAN_POINT ( 'NONE',  ( 1.529023292565329761, 1453.102415013690006, 183.4720393914749934 ) ) ;
#35765 = CARTESIAN_POINT ( 'NONE',  ( 22.68092815790000216, 1409.705069317929883, 208.9674978898780182 ) ) ;
#35766 = VERTEX_POINT ( 'NONE', #57985 ) ;
#35768 = AXIS2_PLACEMENT_3D ( 'NONE', #34193, #68933, #52117 ) ;
#35767 = CARTESIAN_POINT ( 'NONE',  ( -0.8815214275217030382, 1457.995828996750106, 229.7940963460050057 ) ) ;
#35769 = CARTESIAN_POINT ( 'NONE',  ( 25.44620943400289903, 1452.008651903540112, 135.5281762852589793 ) ) ;
#35770 = CARTESIAN_POINT ( 'NONE',  ( -14.26080844802509873, 1456.560644424450174, 195.3871132866240146 ) ) ;
#35771 = CARTESIAN_POINT ( 'NONE',  ( -3.078458299170000245, 1388.638918953580060, 216.9987451616589738 ) ) ;
#35772 = CARTESIAN_POINT ( 'NONE',  ( 7.406484258469999915, 1423.002001740159812, 195.5970099228989909 ) ) ;
#35774 = B_SPLINE_SURFACE_WITH_KNOTS ( 'NONE', 5, 5, ( 
 ( #32174, #59594, #23208, #23759, #50096, #51187, #58493, #50638, #31614 ),
 ( #108881, #91533, #92078, #14811, #92619, #93710, #57408, #57946, #83671 ),
 ( #6427, #24311, #67456, #41122, #65791, #5877, #68012, #66358, #33267 ),
 ( #6968, #15896, #75302, #33820, #109990, #99913, #32725, #48998, #101557 ),
 ( #100477, #16442, #49546, #66905, #24848, #102122, #40021, #74199, #101012 ),
 ( #109445, #84223, #108331, #8066, #83131, #7523, #41681, #25401, #75841 ) ),
 .UNSPECIFIED., .F., .F., .F.,
 ( 6, 6 ),
 ( 6, 3, 6 ),
 ( 0.4666582265040000177, 2.797885342376539963 ),
 ( -1.082960654485929847E-05, 1.000000000000000000, 2.000000000000000000 ),
 .UNSPECIFIED. ) ;
#35773 = CARTESIAN_POINT ( 'NONE',  ( 18.15046249250000088, 1410.043460838129931, 194.1297086120979998 ) ) ;
#35775 = CARTESIAN_POINT ( 'NONE',  ( -3.980933278039999745, 1495.557870970189924, 197.8745908229989823 ) ) ;
#35776 = CARTESIAN_POINT ( 'NONE',  ( 2.962028108840362162, 1439.673284367522001, 184.0494181787074979 ) ) ;
#35778 = CARTESIAN_POINT ( 'NONE',  ( -18.88466409699455539, 1424.778541419677822, 224.4175826655136632 ) ) ;
#35777 = CARTESIAN_POINT ( 'NONE',  ( 0.3313159878120000013, 1417.263519912130050, 235.9102102634980156 ) ) ;
#35779 = CARTESIAN_POINT ( 'NONE',  ( 14.12491358549999987, 1409.406313238730036, 226.3524348291979891 ) ) ;
#35780 = CARTESIAN_POINT ( 'NONE',  ( -0.2739194539550000029, 1497.016984061830044, 230.9805001397980107 ) ) ;
#35781 = CARTESIAN_POINT ( 'NONE',  ( -9.129809187350000244, 1383.863787716160004, 218.5279288458490043 ) ) ;
#35782 = CARTESIAN_POINT ( 'NONE',  ( -6.936398393775000670, 1516.667393516340098, 213.1585948090369698 ) ) ;
#35783 = CARTESIAN_POINT ( 'NONE',  ( 3.237130272123891928, 1524.843178112495480, 241.7217292875349415 ) ) ;
#35784 = EDGE_LOOP ( 'NONE', ( #52540, #89701, #83693, #54550 ) ) ;
#35785 = CARTESIAN_POINT ( 'NONE',  ( -16.95354638770000122, 1417.269256936009924, 207.1959995758089974 ) ) ;
#35786 = CARTESIAN_POINT ( 'NONE',  ( 21.41029105011577727, 1526.329757971583831, 234.0206363886036343 ) ) ;
#35787 = CARTESIAN_POINT ( 'NONE',  ( -6.736062857916709667, 1484.563701159229822, 199.3070513110980073 ) ) ;
#35788 = CARTESIAN_POINT ( 'NONE',  ( 9816.840209715130186, 50.13405481578730161, 1424.308828391600173 ) ) ;
#35789 = ADVANCED_FACE ( 'NONE', ( #101052 ), #74128, .T. ) ;
#35790 = CARTESIAN_POINT ( 'NONE',  ( -34.38848389989589549, 1450.406366866479857, 136.2345448457099906 ) ) ;
#35791 = CARTESIAN_POINT ( 'NONE',  ( -4.328122124485859423, 1515.115455661490159, 208.2045458931170003 ) ) ;
#35792 = CARTESIAN_POINT ( 'NONE',  ( -25.52872276659999784, 1450.634754193449908, 248.0989693021979861 ) ) ;
#35793 = VECTOR ( 'NONE', #73502, 1000.000000000000000 ) ;
#35794 = CARTESIAN_POINT ( 'NONE',  ( -28.70874162694016007, 1526.306647125541986, 197.9001931917368893 ) ) ;
#35795 = CARTESIAN_POINT ( 'NONE',  ( -12.31782664275830008, 1378.331050523219801, 209.6139402054469940 ) ) ;
#35796 = CARTESIAN_POINT ( 'NONE',  ( 19.00000000000000000, 1442.955095612160221, 209.1218459616979999 ) ) ;
#35797 = B_SPLINE_SURFACE_WITH_KNOTS ( 'NONE', 5, 5, ( 
 ( #57746, #91866, #85112, #7856, #40910, #15140 ),
 ( #49330, #110322, #33596, #67791, #109239, #102459 ),
 ( #48792, #6206, #6751, #25193, #59396, #32523 ),
 ( #93507, #66695, #16779, #50983, #8400, #26877 ),
 ( #45359, #43133, #103575, #96287, #34716, #79498 ),
 ( #8962, #77291, #94618, #53770, #19564, #95183 ) ),
 .UNSPECIFIED., .F., .F., .F.,
 ( 6, 6 ),
 ( 6, 6 ),
 ( 0.5468448937290000256, 9.215064474420000096 ),
 ( 0.000000000000000000, 20.00000000000000000 ),
 .UNSPECIFIED. ) ;
#35798 = CARTESIAN_POINT ( 'NONE',  ( -17.99954540876850118, 1410.904693920620048, 195.2564682659330231 ) ) ;
#35799 =( BOUNDED_CURVE ( )  B_SPLINE_CURVE ( 3, ( #31089, #75327, #40598, #5901 ),
 .UNSPECIFIED., .F., .F. ) 
 B_SPLINE_CURVE_WITH_KNOTS ( ( 4, 4 ),
 ( 1.441033914288156303, 1.936717213009869099 ),
 .UNSPECIFIED. ) 
 CURVE ( )  GEOMETRIC_REPRESENTATION_ITEM ( )  RATIONAL_B_SPLINE_CURVE ( ( 1.000000000000000000, 0.9796294326414420883, 0.9796294326414420883, 1.000000000000000000 ) ) 
 REPRESENTATION_ITEM ( '' )  );
#35800 = CARTESIAN_POINT ( 'NONE',  ( -9.760330733150000881, 1424.207526998040066, 192.3956767351990038 ) ) ;
#35801 = AXIS2_PLACEMENT_3D ( 'NONE', #92433, #66182, #100832 ) ;
#35802 = CARTESIAN_POINT ( 'NONE',  ( -30.51231035492526900, 1526.382868172863937, 200.0858385050243555 ) ) ;
#35803 = CARTESIAN_POINT ( 'NONE',  ( 13.89554995500000167, 1452.733480491630189, 223.3956528723979886 ) ) ;
#35804 = EDGE_CURVE ( 'NONE', #43307, #21837, #85926, .T. ) ;
#35805 = CARTESIAN_POINT ( 'NONE',  ( -9.618017228990000334, 1486.043860324930165, 183.5224656496979776 ) ) ;
#35806 = CARTESIAN_POINT ( 'NONE',  ( -7.112124026466545068, 1509.032357789247726, 202.3798027825555153 ) ) ;
#35807 = CARTESIAN_POINT ( 'NONE',  ( -25.97046449806400048, 1509.898002744609812, 192.9853469788230029 ) ) ;
#35808 = AXIS2_PLACEMENT_3D ( 'NONE', #32938, #59826, #92849 ) ;
#35809 = CARTESIAN_POINT ( 'NONE',  ( 24.95209251429999853, 1469.238639853630048, 215.5966609727680066 ) ) ;
#35810 = CARTESIAN_POINT ( 'NONE',  ( -16.62238355811029322, 1420.074002544102314, 208.4323893795217089 ) ) ;
#35811 = PLANE ( 'NONE',  #28980 ) ;
#35812 = CARTESIAN_POINT ( 'NONE',  ( -33.61606591832439506, 1383.837376072390043, 232.0323804794959983 ) ) ;
#35813 = CARTESIAN_POINT ( 'NONE',  ( 19.12715430460800192, 1496.834837051899967, 222.0421819869680178 ) ) ;
#35814 = CARTESIAN_POINT ( 'NONE',  ( -4.029572678834999699, 1516.858649670339901, 213.1633184439769764 ) ) ;
#35815 = DIRECTION ( 'NONE',  ( 1.000000000000000000, 0.000000000000000000, 0.000000000000000000 ) ) ;
#35816 = CARTESIAN_POINT ( 'NONE',  ( 0.1597472590855660013, 1486.419116074489921, 181.8185966615969846 ) ) ;
#35818 = EDGE_LOOP ( 'NONE', ( #56301, #8528, #74461, #103376 ) ) ;
#35817 = SPHERICAL_SURFACE ( 'NONE', #51500, 2.000000000660000055 ) ;
#35819 = CARTESIAN_POINT ( 'NONE',  ( -1.925297170580940076, 1519.551704408389924, 187.5582988486569889 ) ) ;
#35820 = ADVANCED_FACE ( 'NONE', ( #61867 ), #84880, .F. ) ;
#35821 = CARTESIAN_POINT ( 'NONE',  ( -1.094146225179760032E-15, 1380.165560287059861, 203.1907195691389916 ) ) ;
#35822 = CARTESIAN_POINT ( 'NONE',  ( -4.376458691559999892, 1474.728570106689858, 198.9952830931989922 ) ) ;
#35824 = ORIENTED_EDGE ( 'NONE', *, *, #47629, .F. ) ;
#35823 = CARTESIAN_POINT ( 'NONE',  ( -32.21733187660822040, 1523.844789899202397, 216.7883882218984013 ) ) ;
#35825 = CARTESIAN_POINT ( 'NONE',  ( -4.661699225921780432, 1508.551704408389924, 219.7406003995500043 ) ) ;
#35826 = ORIENTED_EDGE ( 'NONE', *, *, #54205, .T. ) ;
#35827 = DIRECTION ( 'NONE',  ( -8.596382804469569442E-17, 1.000000000000000000, 0.000000000000000000 ) ) ;
#35828 = DIRECTION ( 'NONE',  ( -0.05651223375311825725, 0.3161865716976207663, -0.9470123649215663741 ) ) ;
#35829 =( NAMED_UNIT ( * ) SI_UNIT ( $, .STERADIAN. ) SOLID_ANGLE_UNIT ( ) );
#35830 = EDGE_CURVE ( 'NONE', #86670, #22363, #108337, .T. ) ;
#35831 = CARTESIAN_POINT ( 'NONE',  ( -2.876093934609688763, 1368.080635615046049, 208.1320087752549455 ) ) ;
#35832 = CARTESIAN_POINT ( 'NONE',  ( 0.7162863658319988946, 1429.709265593189912, 217.4063670190490143 ) ) ;
#35833 = VECTOR ( 'NONE', #68473, 1000.000000000000000 ) ;
#35834 = CARTESIAN_POINT ( 'NONE',  ( 4.487249753905000027, 1509.038615934239942, 209.1727295022979831 ) ) ;
#35835 = CARTESIAN_POINT ( 'NONE',  ( 14.72140900422560073, 1409.427143317539958, 211.6119428930840343 ) ) ;
#35836 = CARTESIAN_POINT ( 'NONE',  ( -11.45492292490000175, 1391.035318004910096, 204.4802647352790075 ) ) ;
#35837 = CARTESIAN_POINT ( 'NONE',  ( -90.33759372070990423, 1385.193793571259903, 292.7742252942939558 ) ) ;
#35838 = CARTESIAN_POINT ( 'NONE',  ( -17.51214883540000145, 1417.728543787030048, 192.0614060638979765 ) ) ;
#35839 = CARTESIAN_POINT ( 'NONE',  ( -32.86802468386297704, 1523.382868172864164, 201.0396662540046577 ) ) ;
#35840 = ORIENTED_EDGE ( 'NONE', *, *, #46991, .F. ) ;
#35841 = CARTESIAN_POINT ( 'NONE',  ( 17.22623662315568893, 1443.913060387331598, 162.9225832754749490 ) ) ;
#35843 = VERTEX_POINT ( 'NONE', #9767 ) ;
#35842 = CARTESIAN_POINT ( 'NONE',  ( 17.68237282055029880, 1522.051704408389924, 212.5589510568480023 ) ) ;
#35844 = CARTESIAN_POINT ( 'NONE',  ( 7.492689511757870235, 1466.181183281610174, 215.6096703809890016 ) ) ;
#35845 = ORIENTED_EDGE ( 'NONE', *, *, #94018, .T. ) ;
#35846 = EDGE_CURVE ( 'NONE', #17997, #79550, #91488, .T. ) ;
#35847 = CARTESIAN_POINT ( 'NONE',  ( 24.90415728650000204, 1509.109212994030031, 220.8332857727979786 ) ) ;
#35848 = CARTESIAN_POINT ( 'NONE',  ( -8.421179885235224205, 1364.068242571890096, 210.6218459617142003 ) ) ;
#35849 = CARTESIAN_POINT ( 'NONE',  ( 2.433505161638750192, 1497.103005101570034, 196.9591516541469787 ) ) ;
#35850 = EDGE_CURVE ( 'NONE', #25072, #12462, #32180, .T. ) ;
#35851 = CARTESIAN_POINT ( 'NONE',  ( 35.04905840024694896, 1457.721304834078865, 269.5321777411671178 ) ) ;
#35852 = CARTESIAN_POINT ( 'NONE',  ( 11.68966055026420037, 1427.510905538520092, 209.0456480543080033 ) ) ;
#35853 = CARTESIAN_POINT ( 'NONE',  ( 3.412736717740000092, 1396.032235779629900, 220.0203514156980020 ) ) ;
#35854 = CARTESIAN_POINT ( 'NONE',  ( 20.18543375162190046, 1451.730034569789950, 209.6998159054799942 ) ) ;
#35855 = CARTESIAN_POINT ( 'NONE',  ( 4.233304266720000264, 1446.747982731589900, 200.2615130837390041 ) ) ;
#35856 = CARTESIAN_POINT ( 'NONE',  ( -118.1581044363824731, 1309.112692017089103, 296.2006505458993502 ) ) ;
#35857 = CARTESIAN_POINT ( 'NONE',  ( -9.316240760817720457, 1369.171982693950895, 209.6218459617033432 ) ) ;
#35858 = FACE_OUTER_BOUND ( 'NONE', #4964, .T. ) ;
#35859 = CARTESIAN_POINT ( 'NONE',  ( 10.75856251613272718, 1424.957327209176810, 140.6161141926336029 ) ) ;
#35860 = EDGE_CURVE ( 'NONE', #26041, #48957, #20363, .T. ) ;
#35861 = CARTESIAN_POINT ( 'NONE',  ( 4.995725969715000048, 1516.651306816259876, 206.8263604310569690 ) ) ;
#35862 = CARTESIAN_POINT ( 'NONE',  ( -13.08019506225550010, 1434.911011336890169, 149.7358237173160092 ) ) ;
#35863 = LINE ( 'NONE', #10663, #76578 ) ;
#35864 = CARTESIAN_POINT ( 'NONE',  ( 44.92382427260000100, 1446.402585538819949, 269.6913831871979710 ) ) ;
#35866 = EDGE_LOOP ( 'NONE', ( #70268, #12351, #34776, #47598 ) ) ;
#35865 = CARTESIAN_POINT ( 'NONE',  ( 1.375364450349999990, 1495.360691154489814, 220.6206533883990062 ) ) ;
#35867 = EDGE_CURVE ( 'NONE', #86830, #61012, #62980, .T. ) ;
#35868 = CARTESIAN_POINT ( 'NONE',  ( 40.30319224264979994, 1444.187662185900081, 137.0996438307940082 ) ) ;
#35869 = EDGE_LOOP ( 'NONE', ( #31414, #6032, #26353, #8218, #33295 ) ) ;
#35870 = CARTESIAN_POINT ( 'NONE',  ( 3.468905163120000072E-10, 1405.830928045030078, 267.2558864325980039 ) ) ;
#35871 = CARTESIAN_POINT ( 'NONE',  ( -26.43941341069999851, 1488.684867474930115, 204.4673947574779902 ) ) ;
#35873 = CARTESIAN_POINT ( 'NONE',  ( 16.58590676013170295, 1409.592623960390029, 192.7795323272440271 ) ) ;
#35872 = CARTESIAN_POINT ( 'NONE',  ( -10.67358497261050054, 1425.014385072390269, 135.2576413182610224 ) ) ;
#35874 = CARTESIAN_POINT ( 'NONE',  ( -4.027051443935000030, 1516.733363207009916, 211.6130343286269806 ) ) ;
#35875 = AXIS2_PLACEMENT_3D ( 'NONE', #51593, #60564, #94684 ) ;
#35876 = DIRECTION ( 'NONE',  ( -0.4794255386042000078, 8.806904269216944428E-17, 0.8775825618903743131 ) ) ;
#35877 = CARTESIAN_POINT ( 'NONE',  ( -31.95512683489999617, 1440.913060381139985, 244.1805851169980031 ) ) ;
#35878 = CARTESIAN_POINT ( 'NONE',  ( 18.68655961963949963, 1509.584487903890022, 232.0746350300250072 ) ) ;
#35879 = CARTESIAN_POINT ( 'NONE',  ( 28.25086641300000068, 1508.135711190629991, 209.3856964555159834 ) ) ;
#35880 = CARTESIAN_POINT ( 'NONE',  ( -5.222641443459999699, 1391.931189958289906, 214.6468068300290213 ) ) ;
#35881 = DIRECTION ( 'NONE',  ( 0.8234232003240999909, -0.5674277338727967690, -0.000000000000000000 ) ) ;
#35882 = ORIENTED_EDGE ( 'NONE', *, *, #18644, .T. ) ;
#35883 = CARTESIAN_POINT ( 'NONE',  ( 5.639071283312759419, 1396.170382753050035, 219.3208655836849914 ) ) ;
#35884 = CARTESIAN_POINT ( 'NONE',  ( 10.64147525944390082, 1460.268832998469861, 206.6760994863940084 ) ) ;
#35885 = EDGE_CURVE ( 'NONE', #323, #28577, #80789, .T. ) ;
#35886 = CARTESIAN_POINT ( 'NONE',  ( -16.40067627780000237, 1459.015013897929975, 229.6400837563979849 ) ) ;
#35887 = ORIENTED_EDGE ( 'NONE', *, *, #18277, .T. ) ;
#35888 = ORIENTED_EDGE ( 'NONE', *, *, #25408, .F. ) ;
#35889 = CARTESIAN_POINT ( 'NONE',  ( 9.894842273953122103, 1453.125045676060154, 211.4470279248059796 ) ) ;
#35890 = CARTESIAN_POINT ( 'NONE',  ( 8.453089846490000170, 1424.727987169319931, 195.6886735564989976 ) ) ;
#35891 = EDGE_LOOP ( 'NONE', ( #81713, #64444, #57029, #41431 ) ) ;
#35892 = CARTESIAN_POINT ( 'NONE',  ( -1.080623904679999914, 1417.487791310030161, 185.0156185439980163 ) ) ;
#35893 = CARTESIAN_POINT ( 'NONE',  ( -2.409034624560000282, 1512.051704408390151, 213.5301952362090105 ) ) ;
#35894 = ADVANCED_FACE ( 'NONE', ( #47792 ), #101051, .T. ) ;
#35895 = CIRCLE ( 'NONE', #101964, 1.999999999999997780 ) ;
#35896 = CARTESIAN_POINT ( 'NONE',  ( -12.01638156518240130, 1440.881463477919851, 187.8051726210379968 ) ) ;
#35897 = CARTESIAN_POINT ( 'NONE',  ( -7.249244512309999777, 1470.477750770629882, 233.8384446450980079 ) ) ;
#35898 = CARTESIAN_POINT ( 'NONE',  ( 6.120117875752820957, 1508.729257035799947, 201.6787668059709802 ) ) ;
#35899 = SURFACE_STYLE_USAGE ( .BOTH. , #18507 ) ;
#35900 = CARTESIAN_POINT ( 'NONE',  ( -14.17232384770000131, 1420.119835273649869, 215.1506258166890007 ) ) ;
#35901 = CARTESIAN_POINT ( 'NONE',  ( -99.99820827492719388, 1384.874182120719979, 296.2685436471570029 ) ) ;
#35902 = CARTESIAN_POINT ( 'NONE',  ( -6.556651409415000131, 1516.858146885269889, 202.5689485651570010 ) ) ;
#35903 = CARTESIAN_POINT ( 'NONE',  ( 4.044319887224999910, 1517.073005577650065, 210.2423896678870108 ) ) ;
#35904 = VERTEX_POINT ( 'NONE', #46168 ) ;
#35905 = CARTESIAN_POINT ( 'NONE',  ( 11.86577998873609907, 1432.313618685340089, 149.9823692228469838 ) ) ;
#35906 = CARTESIAN_POINT ( 'NONE',  ( 13.19964874196263338, 1444.708229313989477, 187.3105044755715767 ) ) ;
#35907 = VERTEX_POINT ( 'NONE', #89239 ) ;
#35908 = CARTESIAN_POINT ( 'NONE',  ( 30.44527832718689808, 1526.211523310372513, 201.0917162105438933 ) ) ;
#35909 = CYLINDRICAL_SURFACE ( 'NONE', #9107, 1.000000000000000888 ) ;
#35910 = CARTESIAN_POINT ( 'NONE',  ( 2.982314100249999989, 1508.959213791230013, 237.3237166239979956 ) ) ;
#35911 = AXIS2_PLACEMENT_3D ( 'NONE', #86242, #85686, #9533 ) ;
#35912 = CARTESIAN_POINT ( 'NONE',  ( -9.346796821772709762, 1471.356213985179920, 213.0927830673160202 ) ) ;
#35913 = CARTESIAN_POINT ( 'NONE',  ( -5.436853854820000720, 1424.722442587329851, 186.3690072748979958 ) ) ;
#35914 = CARTESIAN_POINT ( 'NONE',  ( 3.472351607788480177, 1409.306382308760021, 270.3710068956600026 ) ) ;
#35915 = CARTESIAN_POINT ( 'NONE',  ( 9.181100887863649973, 1450.964097471789955, 210.1935140534000084 ) ) ;
#35916 = CARTESIAN_POINT ( 'NONE',  ( -7.009441893950000058, 1474.031553669390178, 201.0250566641990133 ) ) ;
#35917 = CARTESIAN_POINT ( 'NONE',  ( 10.76609234380000046, 1492.646438831789965, 213.2464151773390029 ) ) ;
#35918 = CARTESIAN_POINT ( 'NONE',  ( -18.85193010680000114, 1379.597462637329954, 208.8881565698789871 ) ) ;
#35919 = CARTESIAN_POINT ( 'NONE',  ( 0.03158484996424502922, 1410.294062402277405, 233.2218019618084099 ) ) ;
#35921 = LINE ( 'NONE', #62244, #36582 ) ;
#35920 = CARTESIAN_POINT ( 'NONE',  ( -19.14812029890000034, 1505.318613837190014, 209.0594768593419985 ) ) ;
#35922 = CARTESIAN_POINT ( 'NONE',  ( -68.54407940728098936, 1379.747756885784611, 280.1275194419689001 ) ) ;
#35923 = CIRCLE ( 'NONE', #98478, 3.750000000000000000 ) ;
#35924 = CARTESIAN_POINT ( 'NONE',  ( -9.959708506167800124, 1439.533817592069909, 208.3028740885160062 ) ) ;
#35925 = CARTESIAN_POINT ( 'NONE',  ( -5.544570429734849704, 1422.963021390169843, 111.4258773807360114 ) ) ;
#35926 = ORIENTED_EDGE ( 'NONE', *, *, #26071, .F. ) ;
#35927 = CARTESIAN_POINT ( 'NONE',  ( 26.42714721250000309, 1437.883259618699867, 243.9198229428980085 ) ) ;
#35928 = CARTESIAN_POINT ( 'NONE',  ( 13.55396217860879915, 1434.957544704839847, 148.7506959228599897 ) ) ;
#35929 = CARTESIAN_POINT ( 'NONE',  ( -20.71343476518021731, 1522.906561336852974, 179.9059455038230908 ) ) ;
#35930 = CARTESIAN_POINT ( 'NONE',  ( 4.944374238289999113, 1505.309208253089992, 220.4536355099990033 ) ) ;
#35931 = CARTESIAN_POINT ( 'NONE',  ( -14.47420009890000081, 1416.181292664740113, 214.4142689833190047 ) ) ;
#35933 = ORIENTED_EDGE ( 'NONE', *, *, #39179, .T. ) ;
#35932 = CARTESIAN_POINT ( 'NONE',  ( 1.548360550803739910, 1515.071586600679893, 204.7925750858499896 ) ) ;
#35934 = CARTESIAN_POINT ( 'NONE',  ( 4.781276783620000081, 1452.020048942890071, 190.5513815401990030 ) ) ;
#35935 = AXIS2_PLACEMENT_3D ( 'NONE', #108776, #40467, #76281 ) ;
#35936 = CARTESIAN_POINT ( 'NONE',  ( -7.545020141288169668, 1384.905783179920036, 219.0876432115910006 ) ) ;
#35937 = CARTESIAN_POINT ( 'NONE',  ( -16.52551917950000160, 1417.103176096179823, 208.5467600217809832 ) ) ;
#35938 = CARTESIAN_POINT ( 'NONE',  ( 19.37133922758618354, 1456.941101056772595, 224.5491805723401626 ) ) ;
#35939 = CARTESIAN_POINT ( 'NONE',  ( 1.007052846431199411, 1444.164410995541857, 218.0138153337278482 ) ) ;
#35940 = DIRECTION ( 'NONE',  ( 0.7074300732606700892, 0.02470400251916599760, -0.7063514732099990256 ) ) ;
#35941 = CARTESIAN_POINT ( 'NONE',  ( -2.170627987649289992, 1485.611815795640041, 197.4219879416550327 ) ) ;
#35942 = CARTESIAN_POINT ( 'NONE',  ( 31.12456774391177206, 1525.960063244516959, 217.0912716842394730 ) ) ;
#35943 = CARTESIAN_POINT ( 'NONE',  ( -16.21241003196499975, 1514.452905717119847, 224.0491558541669974 ) ) ;
#35944 = CARTESIAN_POINT ( 'NONE',  ( 12.50842520650000012, 1415.079606268429870, 228.9876709444980065 ) ) ;
#35945 = CARTESIAN_POINT ( 'NONE',  ( -11.39043170617670064, 1482.032881333110026, 208.0372395411779962 ) ) ;
#35946 = CARTESIAN_POINT ( 'NONE',  ( -15.69219286469999908, 1459.328416987729952, 229.9957181814980061 ) ) ;
#35947 = CARTESIAN_POINT ( 'NONE',  ( -2.880592967115000125, 1516.859514182039902, 206.2568738160869941 ) ) ;
#35948 = CARTESIAN_POINT ( 'NONE',  ( 21.96192329710000379, 1409.941828261930141, 267.3321697500979894 ) ) ;
#35949 = CARTESIAN_POINT ( 'NONE',  ( -33.28034951413919629, 1522.382868172863937, 217.4407153818824554 ) ) ;
#35950 = FACE_OUTER_BOUND ( 'NONE', #4203, .T. ) ;
#35951 = CARTESIAN_POINT ( 'NONE',  ( 20.68893471149999996, 1469.156827144430054, 193.1476934458979997 ) ) ;
#35952 = CARTESIAN_POINT ( 'NONE',  ( -23.46657084150000117, 1435.066155488599861, 213.1839366923280181 ) ) ;
#35953 = CARTESIAN_POINT ( 'NONE',  ( 2.768651645099999836, 1478.720412810289872, 229.3713484223989951 ) ) ;
#35954 = CARTESIAN_POINT ( 'NONE',  ( -14.97307836811019932, 1417.870019438920053, 203.2001793081319931 ) ) ;
#35955 = CARTESIAN_POINT ( 'NONE',  ( -1.342311606190000006, 1451.734940660029906, 183.7820431827979633 ) ) ;
#35956 = CARTESIAN_POINT ( 'NONE',  ( -20.19282075723703684, 1506.569407720561458, 200.1490527362905425 ) ) ;
#35957 = CARTESIAN_POINT ( 'NONE',  ( -15.88408514909999880, 1416.392489341679948, 208.4668446563049997 ) ) ;
#35958 = CARTESIAN_POINT ( 'NONE',  ( -13.17579405299999884, 1442.542553075959859, 187.8823243441979969 ) ) ;
#35959 = CARTESIAN_POINT ( 'NONE',  ( -7.766930450867759461, 1383.293315432029885, 218.8617756867199944 ) ) ;
#35960 = CARTESIAN_POINT ( 'NONE',  ( -29.17526201480000125, 1435.517118628549952, 135.6494733468979916 ) ) ;
#35961 = CARTESIAN_POINT ( 'NONE',  ( -7.271061757791160929, 1456.602686919181451, 227.6850874585875601 ) ) ;
#35962 = VERTEX_POINT ( 'NONE', #88703 ) ;
#35963 = CYLINDRICAL_SURFACE ( 'NONE', #43909, 1.000000000000001110 ) ;
#35964 = CARTESIAN_POINT ( 'NONE',  ( -14.79665290848370063, 1409.429770892780198, 207.1251313586369918 ) ) ;
#35965 = CARTESIAN_POINT ( 'NONE',  ( 11.63974220683948779, 1435.319261371113043, 224.2611706537471719 ) ) ;
#35966 = DIRECTION ( 'NONE',  ( -0.3090169943749582204, 0.000000000000000000, -0.9510565162951499785 ) ) ;
#35967 = CARTESIAN_POINT ( 'NONE',  ( -45.67178295499999763, 1445.962966203089991, 266.1885921243979851 ) ) ;
#35968 = CARTESIAN_POINT ( 'NONE',  ( -30.16747994869158944, 1524.964230758882877, 196.5181873855272272 ) ) ;
#35969 = CARTESIAN_POINT ( 'NONE',  ( 16.67046851633390148, 1516.551188146170034, 222.1952932998519827 ) ) ;
#35970 = DIRECTION ( 'NONE',  ( 0.7074300732601481734, -0.02470400263378330630, 0.7063514732065131474 ) ) ;
#35971 = CARTESIAN_POINT ( 'NONE',  ( -69.45404346786109784, 1384.664049648719811, 294.4447972851179429 ) ) ;
#35972 = CARTESIAN_POINT ( 'NONE',  ( 19.02974679407714120, 1457.003061607406380, 225.9956790813866974 ) ) ;
#35973 = COLOUR_RGB ( '', 0.40784314, 0.44705882, 0.49803922) ;
#35974 = CARTESIAN_POINT ( 'NONE',  ( -5.013264356492538099, 1375.413060387289761, 214.7179447576738482 ) ) ;
#35975 = CARTESIAN_POINT ( 'NONE',  ( 13.74428069839999900, 1415.087818611729972, 219.0809107912880052 ) ) ;
#35976 = FACE_OUTER_BOUND ( 'NONE', #49784, .T. ) ;
#35977 = CARTESIAN_POINT ( 'NONE',  ( -11.03352569490000157, 1462.446813036689946, 208.7213868678359745 ) ) ;
#35978 = CARTESIAN_POINT ( 'NONE',  ( 4.329448813750000014, 1515.064791442790010, 207.6699222060090051 ) ) ;
#35979 = CARTESIAN_POINT ( 'NONE',  ( -9.883703466890001010, 1508.498109722830122, 182.1694905005979876 ) ) ;
#35980 = CARTESIAN_POINT ( 'NONE',  ( -23.93955323720000194, 1410.670994470229971, 208.0781342075679845 ) ) ;
#35981 = CLOSED_SHELL ( 'NONE', ( #98514, #70721, #25522, #77445, #41435, #1499, #99311, #25106, #56976, #22443, #89036, #42049, #57866, #14526 ) ) ;
#35982 = CARTESIAN_POINT ( 'NONE',  ( 16.44108920490000258, 1415.931669658029932, 201.4407812804579976 ) ) ;
#35983 = EDGE_CURVE ( 'NONE', #29937, #50057, #104030, .T. ) ;
#35984 = CARTESIAN_POINT ( 'NONE',  ( -14.20525283303160080, 1416.384016890880048, 203.1489016136929706 ) ) ;
#35985 = CARTESIAN_POINT ( 'NONE',  ( 5.145337980659999921, 1422.426138373190042, 194.5914561771990066 ) ) ;
#35986 = EDGE_CURVE ( 'NONE', #65298, #36309, #54042, .T. ) ;
#35987 = CARTESIAN_POINT ( 'NONE',  ( -106.6249237206099991, 1391.913060387289988, 305.6722210509360025 ) ) ;
#35988 = CARTESIAN_POINT ( 'NONE',  ( -9.913669495620000660, 1449.457131675590063, 190.8767303025989861 ) ) ;
#35989 = CARTESIAN_POINT ( 'NONE',  ( -7.443079168794310085, 1508.729257029040127, 215.2419651647340118 ) ) ;
#35990 = CARTESIAN_POINT ( 'NONE',  ( -12.04602610265449947, 1481.198043685850052, 227.9689298190359921 ) ) ;
#35992 = CARTESIAN_POINT ( 'NONE',  ( -10.06558583579999855, 1380.695348830889998, 201.8564714307489680 ) ) ;
#35991 = CARTESIAN_POINT ( 'NONE',  ( 11.90008666459999986, 1434.920851464509951, 147.6452002888979962 ) ) ;
#35993 = CARTESIAN_POINT ( 'NONE',  ( -5.028436728809999146, 1391.796861381390045, 203.7103736513389833 ) ) ;
#35994 = CARTESIAN_POINT ( 'NONE',  ( 9.796705758833221367, 1435.283077638600162, 208.5591499206929882 ) ) ;
#35995 = CARTESIAN_POINT ( 'NONE',  ( -10.90499273530000046, 1491.392513267690219, 210.6662861634189881 ) ) ;
#35996 = CARTESIAN_POINT ( 'NONE',  ( 8.178501070643639181, 1441.152429762079919, 153.9860758848200248 ) ) ;
#35997 = CARTESIAN_POINT ( 'NONE',  ( -7.811405798880000084, 1367.739269854439954, 210.6218459616991936 ) ) ;
#35998 = CARTESIAN_POINT ( 'NONE',  ( 3.255340926295000159, 1516.962555622980062, 204.4977466407669908 ) ) ;
#35999 =( NAMED_UNIT ( * ) PLANE_ANGLE_UNIT ( ) SI_UNIT ( $, .RADIAN. ) );
#36000 = CARTESIAN_POINT ( 'NONE',  ( -17.41094686896749977, 1485.005976550500236, 188.5081240344379978 ) ) ;
#36001 = CARTESIAN_POINT ( 'NONE',  ( -18.93046898119999710, 1449.653411359970050, 193.5799670889979893 ) ) ;
#36002 = CARTESIAN_POINT ( 'NONE',  ( 10.70119619629079999, 1502.850065394879948, 214.5617076214280132 ) ) ;
#36003 = CARTESIAN_POINT ( 'NONE',  ( -9.434181852818266378, 1422.844516205027048, 210.7101302893215120 ) ) ;
#36005 = ORIENTED_EDGE ( 'NONE', *, *, #89059, .T. ) ;
#36004 = CARTESIAN_POINT ( 'NONE',  ( -66.95006683284590565, 1379.743526258429938, 277.9676770911790413 ) ) ;
#36006 = EDGE_CURVE ( 'NONE', #75020, #69697, #32498, .T. ) ;
#36007 = VERTEX_POINT ( 'NONE', #76294 ) ;
#36008 = CARTESIAN_POINT ( 'NONE',  ( 11.77041528381420044, 1433.833598648250018, 150.9228460987970095 ) ) ;
#36009 = CARTESIAN_POINT ( 'NONE',  ( 20.70484064406382529, 1525.907212628473644, 185.0411015109853565 ) ) ;
#36010 = VERTEX_POINT ( 'NONE', #22546 ) ;
#36011 = CARTESIAN_POINT ( 'NONE',  ( 19.29374783221134138, 1526.349684470114653, 185.0912796807455152 ) ) ;
#36012 = CARTESIAN_POINT ( 'NONE',  ( -22.05719187630000278, 1509.683314500430015, 191.3091005153979722 ) ) ;
#36014 = CARTESIAN_POINT ( 'NONE',  ( -0.06574339172959998978, 1508.965708869629907, 179.3766826782980104 ) ) ;
#36013 = DIRECTION ( 'NONE',  ( 0.9455185755993178454, 0.000000000000000000, -0.3255681544571539243 ) ) ;
#36015 = CARTESIAN_POINT ( 'NONE',  ( 11.89544747750000120, 1434.541746328260160, 147.6465872843980094 ) ) ;
#36016 =( BOUNDED_CURVE ( )  B_SPLINE_CURVE ( 3, ( #27950, #36896, #44210, #35802 ),
 .UNSPECIFIED., .F., .F. ) 
 B_SPLINE_CURVE_WITH_KNOTS ( ( 4, 4 ),
 ( 3.141592653589793116, 4.712388980384689674 ),
 .UNSPECIFIED. ) 
 CURVE ( )  GEOMETRIC_REPRESENTATION_ITEM ( )  RATIONAL_B_SPLINE_CURVE ( ( 1.000000000000000000, 0.8047378541243649375, 0.8047378541243649375, 1.000000000000000000 ) ) 
 REPRESENTATION_ITEM ( '' )  );
#36017 = AXIS2_PLACEMENT_3D ( 'NONE', #89891, #108906, #66925 ) ;
#36018 = B_SPLINE_CURVE_WITH_KNOTS ( 'NONE', 5,
 ( #77188, #83354, #41372, #57641, #42460, #8298, #32948, #49229, #59836 ),
 .UNSPECIFIED., .F., .F.,
 ( 6, 3, 6 ),
 ( 0.000000000000000000, 0.7482103374986269761, 1.000000000000000000 ),
 .UNSPECIFIED. ) ;
#36019 = CARTESIAN_POINT ( 'NONE',  ( -23.84450196390190158, 1452.080391932540124, 136.9869676255979982 ) ) ;
#36020 = CARTESIAN_POINT ( 'NONE',  ( -0.5477602106990010489, 1469.061648626090118, 219.1663329555989890 ) ) ;
#36021 = CARTESIAN_POINT ( 'NONE',  ( -24.59804701143680106, 1444.770899505660054, 210.9018572211569733 ) ) ;
#36022 = CARTESIAN_POINT ( 'NONE',  ( -7.709681306425000713, 1516.559109716219837, 211.9945464874270158 ) ) ;
#36023 = CARTESIAN_POINT ( 'NONE',  ( 35.92423077391850228, 1436.007692230339899, 134.0999999972619889 ) ) ;
#36025 = TOROIDAL_SURFACE ( 'NONE', #53957, 21.40691501530000096, 1.500287545629999997 ) ;
#36024 = CARTESIAN_POINT ( 'NONE',  ( -8.279722129557768540, 1423.369210425909841, 209.8234668683010113 ) ) ;
#36026 = DIRECTION ( 'NONE',  ( -0.9455185755993178454, 0.000000000000000000, 0.3255681544571537578 ) ) ;
#36027 = VERTEX_POINT ( 'NONE', #91987 ) ;
#36028 = CARTESIAN_POINT ( 'NONE',  ( 14.43356177019170161, 1436.105945022930200, 149.9343689364710031 ) ) ;
#36029 = CYLINDRICAL_SURFACE ( 'NONE', #97720, 1.999999999999998668 ) ;
#36030 = ORIENTED_EDGE ( 'NONE', *, *, #1511, .F. ) ;
#36031 = VERTEX_POINT ( 'NONE', #33724 ) ;
#36032 = EDGE_LOOP ( 'NONE', ( #83770, #59613 ) ) ;
#36033 = CYLINDRICAL_SURFACE ( 'NONE', #16118, 0.9999999999999873435 ) ;
#36034 = CARTESIAN_POINT ( 'NONE',  ( -0.7474240596110000023, 1467.090493009529837, 235.5344236438979806 ) ) ;
#36035 = CARTESIAN_POINT ( 'NONE',  ( 22.11924855878987728, 1450.910478644122122, 143.0538365109425456 ) ) ;
#36036 = FACE_OUTER_BOUND ( 'NONE', #30790, .T. ) ;
#36037 = CARTESIAN_POINT ( 'NONE',  ( 0.08355061096887030081, 1465.424449796589897, 198.1142439294760038 ) ) ;
#36038 = EDGE_CURVE ( 'NONE', #59778, #7623, #83041, .T. ) ;
#36039 = VECTOR ( 'NONE', #69284, 1000.000000000000114 ) ;
#36040 = CARTESIAN_POINT ( 'NONE',  ( -19.07402656877554392, 1442.263495886194960, 210.5458490460772225 ) ) ;
#36041 = CARTESIAN_POINT ( 'NONE',  ( -45.68166716313724862, 1379.673069186346083, 231.7062482893097695 ) ) ;
#36042 = DIRECTION ( 'NONE',  ( 1.734723475976998196E-15, -1.000000000000000000, 0.000000000000000000 ) ) ;
#36043 = EDGE_CURVE ( 'NONE', #52385, #45960, #17466, .T. ) ;
#36044 = CARTESIAN_POINT ( 'NONE',  ( 8.651090045271681461, 1437.459470016739942, 208.9048937552290113 ) ) ;
#36045 = ORIENTED_EDGE ( 'NONE', *, *, #37258, .F. ) ;
#36046 = CARTESIAN_POINT ( 'NONE',  ( 4.027697225915000345, 1516.766397346390022, 206.2431526829570032 ) ) ;
#36047 = VERTEX_POINT ( 'NONE', #49455 ) ;
#36048 = CARTESIAN_POINT ( 'NONE',  ( 32.50672632217259661, 1440.913060387330006, 256.8451983435460306 ) ) ;
#36049 = CARTESIAN_POINT ( 'NONE',  ( -17.98937745960000001, 1509.201726663129875, 186.3878134344979856 ) ) ;
#36050 = ORIENTED_EDGE ( 'NONE', *, *, #48013, .F. ) ;
#36051 = CARTESIAN_POINT ( 'NONE',  ( -6.032830782151830107, 1508.551567431860121, 201.9555811633020141 ) ) ;
#36052 = CARTESIAN_POINT ( 'NONE',  ( -14.51206241080000048, 1409.419832773630105, 192.1183054032979953 ) ) ;
#36053 = CARTESIAN_POINT ( 'NONE',  ( -57.65665968917219431, 1379.718748827512627, 261.1525070835933207 ) ) ;
#36054 = CARTESIAN_POINT ( 'NONE',  ( 0.1595995995380000143, 1486.508831850330125, 181.8147405652979671 ) ) ;
#36055 = CARTESIAN_POINT ( 'NONE',  ( -0.2452586311791360163, 1422.882060582030135, 192.4945411992279958 ) ) ;
#36056 = CARTESIAN_POINT ( 'NONE',  ( 0.0001418537954666921350, 1395.950261259293029, 197.6573513283705665 ) ) ;
#36057 = DIRECTION ( 'NONE',  ( -0.7071093782156816498, -3.166819169022306488E-06, -0.7071041841407837980 ) ) ;
#36058 = CARTESIAN_POINT ( 'NONE',  ( -26.79413167943010166, 1436.761919080860025, 136.7821860765010058 ) ) ;
#36059 = CARTESIAN_POINT ( 'NONE',  ( -7.354862284149999319, 1508.833542331989975, 219.0557158588990205 ) ) ;
#36061 = CARTESIAN_POINT ( 'NONE',  ( 8.909957024879078702, 1434.607635241320168, 206.3240561870909744 ) ) ;
#36060 = LINE ( 'NONE', #50645, #105793 ) ;
#36062 = CARTESIAN_POINT ( 'NONE',  ( 2.875850094215000041, 1516.647618671360078, 214.8936433964170192 ) ) ;
#36063 = B_SPLINE_CURVE_WITH_KNOTS ( 'NONE', 3,
 ( #96649, #54118, #3162, #38376, #107795, #99373 ),
 .UNSPECIFIED., .F., .F.,
 ( 4, 2, 4 ),
 ( -0.03810055507010769865, -0.01873955902292570239, 0.000000000000000000 ),
 .UNSPECIFIED. ) ;
#36064 = DIRECTION ( 'NONE',  ( -0.6736849260863837507, 0.000000000000000000, 0.7390186874254154326 ) ) ;
#36065 = CARTESIAN_POINT ( 'NONE',  ( 5.745732791923909843, 1511.535603804869879, 217.7226386876670006 ) ) ;
#36066 = CARTESIAN_POINT ( 'NONE',  ( 27.93158904759999928, 1508.017348895330088, 207.9454904019079891 ) ) ;
#36067 = CARTESIAN_POINT ( 'NONE',  ( 1.716392741775000008, 1516.788317650260069, 211.9856338259669997 ) ) ;
#36068 = CARTESIAN_POINT ( 'NONE',  ( -18.95069757339999938, 1434.818091166690010, 209.0758544139090134 ) ) ;
#36069 = CARTESIAN_POINT ( 'NONE',  ( -17.27977277066755946, 1486.136564927255677, 187.9056138646151055 ) ) ;
#36071 = VERTEX_POINT ( 'NONE', #83577 ) ;
#36070 = CARTESIAN_POINT ( 'NONE',  ( -76.73601434870001015, 1388.129781852509950, 300.4664286386590106 ) ) ;
#36072 = CARTESIAN_POINT ( 'NONE',  ( -16.97881484272415875, 1525.055402519470135, 236.9933241842670100 ) ) ;
#36073 = CARTESIAN_POINT ( 'NONE',  ( -5.623567758859999945E-10, 1466.838857909629951, 244.5742075746979936 ) ) ;
#36074 = CARTESIAN_POINT ( 'NONE',  ( 30.61611611310372894, 1526.069472839377568, 216.5565799337455530 ) ) ;
#36075 = CARTESIAN_POINT ( 'NONE',  ( 19.01706420256806496, 1526.382868172863937, 232.8536233449245287 ) ) ;
#36076 = CARTESIAN_POINT ( 'NONE',  ( -2.809418260625490049, 1508.990990147629873, 238.3402367501120125 ) ) ;
#36077 = CARTESIAN_POINT ( 'NONE',  ( -19.92007499920000058, 1455.402141745330027, 226.0082975429980081 ) ) ;
#36078 = CIRCLE ( 'NONE', #43191, 3.500000000000003109 ) ;
#36080 = CARTESIAN_POINT ( 'NONE',  ( 19.46842866420000107, 1455.664567239729877, 226.2662422576979964 ) ) ;
#36079 = CARTESIAN_POINT ( 'NONE',  ( 11.58636795370000172, 1433.009610628010023, 151.1946776810979713 ) ) ;
#36081 = CARTESIAN_POINT ( 'NONE',  ( 0.1661831847680000085, 1452.811554597430131, 189.3009787847980192 ) ) ;
#36082 = CARTESIAN_POINT ( 'NONE',  ( -106.3539583109999995, 1379.482941952589954, 307.8537995074590299 ) ) ;
#36083 = ORIENTED_EDGE ( 'NONE', *, *, #33990, .T. ) ;
#36084 = CARTESIAN_POINT ( 'NONE',  ( -2.875850132345000087, 1516.647618671360078, 203.3500485059169876 ) ) ;
#36085 = CARTESIAN_POINT ( 'NONE',  ( -8.949166976945781116, 1508.433673422140146, 219.1618437498449907 ) ) ;
#36086 = DIRECTION ( 'NONE',  ( 0.000000000000000000, 0.2733307411301343914, -0.9619201141224000828 ) ) ;
#36087 = CARTESIAN_POINT ( 'NONE',  ( 30.27492243234960156, 1463.607600769530109, 269.7181436845010580 ) ) ;
#36088 = CARTESIAN_POINT ( 'NONE',  ( 5.391625819569999756, 1433.099291512059835, 154.6242831037980068 ) ) ;
#36089 = CARTESIAN_POINT ( 'NONE',  ( -19.82380892210000312, 1467.090503478189930, 209.9302942427229937 ) ) ;
#36090 = CARTESIAN_POINT ( 'NONE',  ( 0.5135905785996027761, 1469.225700524577405, 219.1587014438361223 ) ) ;
#36091 = AXIS2_PLACEMENT_3D ( 'NONE', #15521, #30130, #22815 ) ;
#36092 = CARTESIAN_POINT ( 'NONE',  ( -36.67895744121949519, 1440.913060387330006, 254.0696615155329994 ) ) ;
#36093 = CARTESIAN_POINT ( 'NONE',  ( 34.39105378604129726, 1450.405804220740265, 136.2345510266769963 ) ) ;
#36094 = CARTESIAN_POINT ( 'NONE',  ( 2.500574528909250027, 1448.942056006560051, 154.5733147652059927 ) ) ;
#36095 = CARTESIAN_POINT ( 'NONE',  ( -0.06016446275539899524, 1431.826830952890077, 200.6931156591689955 ) ) ;
#36096 = CARTESIAN_POINT ( 'NONE',  ( -15.85591190879999779, 1415.880081504350073, 209.4912631162540038 ) ) ;
#36097 = CARTESIAN_POINT ( 'NONE',  ( -0.9486860776340020340, 1507.879202551890103, 220.9616002900989997 ) ) ;
#36098 = CARTESIAN_POINT ( 'NONE',  ( 1.582067810090000045E-15, 1508.551704408389924, 209.1218459616989946 ) ) ;
#36099 = DIRECTION ( 'NONE',  ( -0.9455185755993178454, 0.000000000000000000, 0.3255681544571539243 ) ) ;
#36100 = EDGE_LOOP ( 'NONE', ( #76286, #99061, #19882, #94695 ) ) ;
#36101 = CARTESIAN_POINT ( 'NONE',  ( -8.881784197000000993E-16, 1410.951844103529993, 268.3665355202980436 ) ) ;
#36102 = CARTESIAN_POINT ( 'NONE',  ( -0.1560728617379990024, 1485.890437600389760, 197.6029597742989949 ) ) ;
#36103 = CARTESIAN_POINT ( 'NONE',  ( 6.487764263893970096, 1466.799890030109964, 201.2724796736299879 ) ) ;
#36104 = CARTESIAN_POINT ( 'NONE',  ( -0.1078499524459999998, 1475.983410498030025, 267.2349610867980232 ) ) ;
#36105 = DIRECTION ( 'NONE',  ( -1.000000000000000000, 0.000000000000000000, 0.000000000000000000 ) ) ;
#36106 = CARTESIAN_POINT ( 'NONE',  ( -30.51126001304075430, 1526.382868172863937, 198.3878992055731487 ) ) ;
#36107 = CARTESIAN_POINT ( 'NONE',  ( 8.482143754180000883, 1423.325759885000025, 211.9865062201690193 ) ) ;
#36108 = CARTESIAN_POINT ( 'NONE',  ( -22.27559603053860116, 1384.855102641009807, 222.0256361789579955 ) ) ;
#36109 = AXIS2_PLACEMENT_3D ( 'NONE', #12534, #46712, #80842 ) ;
#36110 = CARTESIAN_POINT ( 'NONE',  ( -17.83233393729999960, 1415.128105759529944, 207.7695487697079955 ) ) ;
#36111 = CARTESIAN_POINT ( 'NONE',  ( -10.28192841989999984, 1482.564960466189859, 205.0245988223590246 ) ) ;
#36112 = CARTESIAN_POINT ( 'NONE',  ( 19.00334344017809585, 1416.835288280193936, 210.3100235811058667 ) ) ;
#36113 = CARTESIAN_POINT ( 'NONE',  ( -5.573518479978040396, 1396.107691941430176, 199.5941084161559900 ) ) ;
#36114 = ORIENTED_EDGE ( 'NONE', *, *, #13931, .F. ) ;
#36115 = AXIS2_PLACEMENT_3D ( 'NONE', #91765, #48135, #100709 ) ;
#36116 = CARTESIAN_POINT ( 'NONE',  ( -17.22758722712179846, 1410.459222837350126, 225.8949354550800024 ) ) ;
#36117 = CARTESIAN_POINT ( 'NONE',  ( 22.28175235382923347, 1509.670458318331612, 227.1137651221278020 ) ) ;
#36118 = VERTEX_POINT ( 'NONE', #99824 ) ;
#36119 = CARTESIAN_POINT ( 'NONE',  ( -11.39431203569762552, 1501.174835975778933, 208.1498517562084487 ) ) ;
#36120 = CARTESIAN_POINT ( 'NONE',  ( -13.58681706775159981, 1508.455392534539897, 209.9114426240880107 ) ) ;
#36121 = CARTESIAN_POINT ( 'NONE',  ( 2.963088497139999777, 1449.560975490390092, 190.2511718989990186 ) ) ;
#36123 = CARTESIAN_POINT ( 'NONE',  ( -9.842956191871440552, 1438.561763663640022, 210.4747371474470015 ) ) ;
#36122 = CARTESIAN_POINT ( 'NONE',  ( 10.00814141210000052, 1425.214601638330123, 94.99987188269780347 ) ) ;
#36124 = CARTESIAN_POINT ( 'NONE',  ( 3.156166260290000025, 1466.544008048530031, 236.1241471695980181 ) ) ;
#36125 = CARTESIAN_POINT ( 'NONE',  ( -8.835157404840000339, 1450.736626986090187, 204.9140208344290102 ) ) ;
#36126 = CARTESIAN_POINT ( 'NONE',  ( -109.9742488199109971, 1384.497342733709957, 311.4391987445749805 ) ) ;
#36127 = CARTESIAN_POINT ( 'NONE',  ( 7.774392068240000064, 1425.884050503550270, 211.7695909195089996 ) ) ;
#36128 = CARTESIAN_POINT ( 'NONE',  ( -19.04700360180000374, 1444.155872993190087, 199.5980005317190091 ) ) ;
#36129 = CARTESIAN_POINT ( 'NONE',  ( -23.55087667009999919, 1411.110693366829764, 210.4794020521279947 ) ) ;
#36130 = LINE ( 'NONE', #27720, #23881 ) ;
#36131 = CARTESIAN_POINT ( 'NONE',  ( 2.622224098489999822, 1449.049842484869941, 183.1053685486979816 ) ) ;
#36132 = CARTESIAN_POINT ( 'NONE',  ( 9.671060821812719865, 1366.060403940060041, 210.6218459616987957 ) ) ;
#36134 = ORIENTED_EDGE ( 'NONE', *, *, #13815, .T. ) ;
#36133 = CARTESIAN_POINT ( 'NONE',  ( -15.74154698502330163, 1459.394320999469983, 230.7248352790539911 ) ) ;
#36135 = EDGE_LOOP ( 'NONE', ( #13683, #88034, #40284, #74189 ) ) ;
#36136 = EDGE_CURVE ( 'NONE', #3437, #37815, #101565, .T. ) ;
#36137 = CARTESIAN_POINT ( 'NONE',  ( -40.71369779150000312, 1443.851625732439970, 137.1196992376980006 ) ) ;
#36138 = DIRECTION ( 'NONE',  ( 0.000000000000000000, 1.000000000000000000, 0.000000000000000000 ) ) ;
#36139 = CARTESIAN_POINT ( 'NONE',  ( -10.06709464454669956, 1499.964826402849894, 247.9768189705859811 ) ) ;
#36140 = CARTESIAN_POINT ( 'NONE',  ( 6.271138058716076991, 1499.936577760534874, 199.6202075728144507 ) ) ;
#36141 = CARTESIAN_POINT ( 'NONE',  ( -106.3607387814725911, 1309.112692017088648, 308.0674118875946874 ) ) ;
#36142 = CARTESIAN_POINT ( 'NONE',  ( -31.56778878607243044, 1525.408337840050308, 202.0372949643508491 ) ) ;
#36143 = CARTESIAN_POINT ( 'NONE',  ( 2.239840163258520089, 1476.242923025720074, 197.8476420570929974 ) ) ;
#36144 = EDGE_CURVE ( 'NONE', #77609, #25815, #82943, .T. ) ;
#36145 = CARTESIAN_POINT ( 'NONE',  ( -34.91175744441260065, 1450.402292434889887, 136.2167050401169774 ) ) ;
#36146 = CARTESIAN_POINT ( 'NONE',  ( -2.500000000000000000, 1448.457353036769973, 161.2531520594690164 ) ) ;
#36147 = CARTESIAN_POINT ( 'NONE',  ( 9.510490888398619447, 1396.245174050119886, 214.7739347511380004 ) ) ;
#36148 = CARTESIAN_POINT ( 'NONE',  ( 9.336575772837418796, 1408.712768855870081, 198.5035178465510057 ) ) ;
#36149 = CARTESIAN_POINT ( 'NONE',  ( -5.339443612929020588, 1406.221089105190003, 266.9497679340149716 ) ) ;
#36150 = CARTESIAN_POINT ( 'NONE',  ( -13.76119476942800013, 1434.988040804719958, 148.8304954868820005 ) ) ;
#36151 = EDGE_LOOP ( 'NONE', ( #73537, #31971, #38492, #42862 ) ) ;
#36152 = CARTESIAN_POINT ( 'NONE',  ( 3.709769364390000490, 1425.443954302430029, 185.2607701543980170 ) ) ;
#36153 = CARTESIAN_POINT ( 'NONE',  ( 13.37712129999999888, 1445.815448238960016, 188.8332726567979876 ) ) ;
#36154 = VERTEX_POINT ( 'NONE', #57320 ) ;
#36155 = ORIENTED_EDGE ( 'NONE', *, *, #49415, .F. ) ;
#36156 = CARTESIAN_POINT ( 'NONE',  ( -3.205906119050000225, 1454.493865833489963, 199.5427769187489844 ) ) ;
#36157 = CARTESIAN_POINT ( 'NONE',  ( -9.351945459739999578, 1366.519103298159735, 207.6218459616989946 ) ) ;
#36158 = CARTESIAN_POINT ( 'NONE',  ( 3.458526497885000328, 1516.742629295279812, 214.1194197574270106 ) ) ;
#36159 = CARTESIAN_POINT ( 'NONE',  ( 4.827505427815000694, 1511.354819475749991, 217.2927421938970269 ) ) ;
#36160 = ORIENTED_EDGE ( 'NONE', *, *, #35220, .T. ) ;
#36161 = CARTESIAN_POINT ( 'NONE',  ( -77.77200720220001529, 1374.656469663290181, 291.9281914796590058 ) ) ;
#36162 = CARTESIAN_POINT ( 'NONE',  ( 9.839466250099999201, 1415.426091369430196, 224.2613875613980099 ) ) ;
#36163 = CARTESIAN_POINT ( 'NONE',  ( 2.480813884984999884, 1517.051603658920158, 204.1089070683270279 ) ) ;
#36164 = AXIS2_PLACEMENT_3D ( 'NONE', #52624, #36907, #71669 ) ;
#36165 = CARTESIAN_POINT ( 'NONE',  ( -13.70772824027479864, 1507.648153509909889, 184.2587339175119894 ) ) ;
#36166 = CARTESIAN_POINT ( 'NONE',  ( -2.564633821555000193, 1511.308638870219966, 201.5496530815769916 ) ) ;
#36167 = CARTESIAN_POINT ( 'NONE',  ( 11.21203837860620922, 1433.014098020969641, 151.5746018212971364 ) ) ;
#36168 = CARTESIAN_POINT ( 'NONE',  ( -54.02940655686400362, 1384.639031856270094, 232.0758257302100276 ) ) ;
#36169 = CARTESIAN_POINT ( 'NONE',  ( 9.213513262295309758, 1461.925794281050003, 206.0128988621550263 ) ) ;
#36170 = CARTESIAN_POINT ( 'NONE',  ( -5.999476885900000056, 1410.056533633429808, 231.4736029180979813 ) ) ;
#36172 = VERTEX_POINT ( 'NONE', #66816 ) ;
#36171 = CARTESIAN_POINT ( 'NONE',  ( -8.921414208959999925, 1447.268111543890200, 186.2693290151980250 ) ) ;
#36173 = CARTESIAN_POINT ( 'NONE',  ( -14.58073495223914051, 1436.114484106691634, 149.8442567287235363 ) ) ;
#36174 = CARTESIAN_POINT ( 'NONE',  ( -12.02051104499999923, 1491.153688735689911, 206.6632163132790083 ) ) ;
#36175 = DIRECTION ( 'NONE',  ( 0.4794255386042041156, -2.935634756405673411E-17, -0.8775825618903722036 ) ) ;
#36176 = CARTESIAN_POINT ( 'NONE',  ( 15.62326149577455325, 1506.535970895669379, 224.7081918935420219 ) ) ;
#36177 = CARTESIAN_POINT ( 'NONE',  ( -25.34185429560000102, 1436.460898709450021, 137.3540916501980291 ) ) ;
#36178 = CARTESIAN_POINT ( 'NONE',  ( -2.864972154145000172, 1516.859514182039902, 212.0024388992169975 ) ) ;
#36179 = VECTOR ( 'NONE', #27524, 1000.000000000000000 ) ;
#36180 = CARTESIAN_POINT ( 'NONE',  ( -65.37434784279999178, 1379.739354356529930, 273.2054369558589997 ) ) ;
#36181 = CARTESIAN_POINT ( 'NONE',  ( 0.008364224685127532796, 1508.450927448398261, 237.9449321159623594 ) ) ;
#36182 = CARTESIAN_POINT ( 'NONE',  ( 13.69810584925325259, 1494.139388547490398, 192.1978378177635705 ) ) ;
#36183 = CARTESIAN_POINT ( 'NONE',  ( 20.22198891407199994, 1410.979504948318208, 197.8698230559548108 ) ) ;
#36184 = CARTESIAN_POINT ( 'NONE',  ( 0.007128837152181529378, 1517.006509894990131, 209.8686634857439799 ) ) ;
#36185 = ORIENTED_EDGE ( 'NONE', *, *, #71695, .T. ) ;
#36186 = CARTESIAN_POINT ( 'NONE',  ( 2.500000000000000000, 1432.484228967709896, 157.4989653737979722 ) ) ;
#36187 = CARTESIAN_POINT ( 'NONE',  ( 5.457743877670670152, 1440.715679535709796, 154.7912908120740099 ) ) ;
#36188 = CARTESIAN_POINT ( 'NONE',  ( -62.07030651009999644, 1385.055139444880069, 284.7661505247589844 ) ) ;
#36189 = ORIENTED_EDGE ( 'NONE', *, *, #32715, .T. ) ;
#36190 = DIRECTION ( 'NONE',  ( -7.460783098696655896E-07, -0.9583089388702578093, 0.2857341031112730634 ) ) ;
#36191 = LINE ( 'NONE', #21014, #101340 ) ;
#36192 = CARTESIAN_POINT ( 'NONE',  ( 12.51168921360669906, 1434.575074074980193, 150.0969845919200054 ) ) ;
#36193 = CARTESIAN_POINT ( 'NONE',  ( 13.20134068419620021, 1478.703343677790144, 231.7406313773049931 ) ) ;
#36194 = CARTESIAN_POINT ( 'NONE',  ( -24.18231958401429793, 1509.512723376200029, 223.7027743721939999 ) ) ;
#36195 = CARTESIAN_POINT ( 'NONE',  ( -1.899659233539999992, 1408.979397949530039, 187.8524191995979891 ) ) ;
#36196 = CARTESIAN_POINT ( 'NONE',  ( -15.12003195112067111, 1517.151704408390060, 218.5174026476448432 ) ) ;
#36197 = CARTESIAN_POINT ( 'NONE',  ( 0.02480326138201020131, 1420.444607191170007, 182.6734921983770050 ) ) ;
#36199 = CARTESIAN_POINT ( 'NONE',  ( -4.319145982190000232, 1421.270721987530123, 186.1375689550980042 ) ) ;
#36198 = CARTESIAN_POINT ( 'NONE',  ( -2.288357445734999995, 1517.116049120239950, 214.9102823043970147 ) ) ;
#36200 = CARTESIAN_POINT ( 'NONE',  ( -7.722580352405000070, 1517.051704408389924, 209.1218459511669892 ) ) ;
#36201 = CARTESIAN_POINT ( 'NONE',  ( 2.291047489114999891, 1516.524310051880093, 216.8306159772470210 ) ) ;
#36202 = VERTEX_POINT ( 'NONE', #41030 ) ;
#36203 = CARTESIAN_POINT ( 'NONE',  ( -12.78353013627570078, 1416.221314539589912, 196.4153621971449866 ) ) ;
#36204 = DIRECTION ( 'NONE',  ( -0.01594118961724027769, -0.9969860201949399814, -0.07592597717146752634 ) ) ;
#36205 = VERTEX_POINT ( 'NONE', #75207 ) ;
#36206 = LINE ( 'NONE', #43510, #23162 ) ;
#36207 = CARTESIAN_POINT ( 'NONE',  ( 9.275190821709212941, 1436.622319119972872, 152.9610493690184683 ) ) ;
#36208 = CARTESIAN_POINT ( 'NONE',  ( 8.553070074608509543, 1511.487400615810202, 203.5546195846039836 ) ) ;
#36209 = CARTESIAN_POINT ( 'NONE',  ( 2.736568218950000020, 1441.973427766389932, 217.9247250662190254 ) ) ;
#36210 = CARTESIAN_POINT ( 'NONE',  ( -3.271538019026510202, 1454.292002138270163, 199.1638778078030043 ) ) ;
#36211 = CARTESIAN_POINT ( 'NONE',  ( -21.54890432409634116, 1524.816846803860926, 234.5807495618499559 ) ) ;
#36212 = CARTESIAN_POINT ( 'NONE',  ( 17.35267690140000241, 1414.988017870030035, 210.4487656687780088 ) ) ;
#36213 = CARTESIAN_POINT ( 'NONE',  ( -18.54624378429999965, 1425.206167962729978, 225.2666202254980021 ) ) ;
#36214 = CARTESIAN_POINT ( 'NONE',  ( -21.38425910549999998, 1436.475178973239963, 143.9724053363979976 ) ) ;
#36215 = CARTESIAN_POINT ( 'NONE',  ( -0.5805478584864469660, 1457.956445091640035, 229.5817085807559863 ) ) ;
#36216 = CARTESIAN_POINT ( 'NONE',  ( 17.09566487500000065, 1418.986537885430153, 191.5701185073980071 ) ) ;
#36218 = CARTESIAN_POINT ( 'NONE',  ( 0.5779700330962650456, 1451.730245120970039, 188.9364029278959833 ) ) ;
#36217 = CARTESIAN_POINT ( 'NONE',  ( -34.18677586421173231, 1522.382868172863937, 219.7932833225216882 ) ) ;
#36219 = CARTESIAN_POINT ( 'NONE',  ( 11.73811278442431139, 1433.731505864096334, 150.9439206914117619 ) ) ;
#36220 = ORIENTED_EDGE ( 'NONE', *, *, #99547, .T. ) ;
#36221 = CARTESIAN_POINT ( 'NONE',  ( 1.556453189349229937, 1415.124054205860148, 191.3769848897780150 ) ) ;
#36222 = CARTESIAN_POINT ( 'NONE',  ( 23.97240591419999944, 1430.440342350430001, 207.3418792401980113 ) ) ;
#36223 = CARTESIAN_POINT ( 'NONE',  ( -11.87682050080051788, 1433.080539119526748, 149.9786770413036265 ) ) ;
#36224 = DIRECTION ( 'NONE',  ( -0.9993908270190955401, -0.03489949670250328678, 0.000000000000000000 ) ) ;
#36225 = CARTESIAN_POINT ( 'NONE',  ( -18.63433789430000331, 1508.246382728430035, 229.7323350256980063 ) ) ;
#36226 = CARTESIAN_POINT ( 'NONE',  ( -10.43765270066229967, 1479.571382516360018, 210.2075621104870038 ) ) ;
#36227 = CARTESIAN_POINT ( 'NONE',  ( -22.86388141493510062, 1452.114636054849825, 134.0999999999999943 ) ) ;
#36228 = CARTESIAN_POINT ( 'NONE',  ( -18.68121726845560104, 1509.578614484549917, 185.5942095029820109 ) ) ;
#36229 = CARTESIAN_POINT ( 'NONE',  ( -4.376494698527389815, 1488.973636533830131, 219.1697672411899873 ) ) ;
#36230 = CARTESIAN_POINT ( 'NONE',  ( -0.3862383889521530111, 1500.063189114229999, 233.1571762794760048 ) ) ;
#36231 = CARTESIAN_POINT ( 'NONE',  ( -75.94647945793420263, 1383.780046445180005, 300.6252629312149907 ) ) ;
#36232 = CARTESIAN_POINT ( 'NONE',  ( -109.2888349613960060, 1384.560112836649978, 311.2476446514990016 ) ) ;
#36233 = CARTESIAN_POINT ( 'NONE',  ( -113.4000000000000057, 1384.913060387289988, 304.2218459572590064 ) ) ;
#36234 = CARTESIAN_POINT ( 'NONE',  ( -1.764278193548540097, 1516.541781377969983, 201.4126184223130167 ) ) ;
#36236 = VERTEX_POINT ( 'NONE', #91447 ) ;
#36235 = DIRECTION ( 'NONE',  ( -1.000000000000000000, 0.000000000000000000, 0.000000000000000000 ) ) ;
#36237 = CARTESIAN_POINT ( 'NONE',  ( -18.05523222188424270, 1459.620137051063921, 227.9958600545465970 ) ) ;
#36238 = CARTESIAN_POINT ( 'NONE',  ( -85.62072771500000101, 1379.320813475580053, 297.8911852074589888 ) ) ;
#36239 = CARTESIAN_POINT ( 'NONE',  ( 20.18524465598390094, 1509.340777616249852, 229.9812346231060189 ) ) ;
#36240 = VERTEX_POINT ( 'NONE', #74657 ) ;
#36241 = ORIENTED_EDGE ( 'NONE', *, *, #98660, .T. ) ;
#36242 = CARTESIAN_POINT ( 'NONE',  ( 29.40443212115383531, 1511.187213306747708, 196.1539082851714966 ) ) ;
#36243 = CARTESIAN_POINT ( 'NONE',  ( 18.52260186970000433, 1425.593317732829973, 225.5454236923980034 ) ) ;
#36244 = CARTESIAN_POINT ( 'NONE',  ( 13.45445143672208843, 1443.535890046601253, 169.3629104747118959 ) ) ;
#36246 = CARTESIAN_POINT ( 'NONE',  ( -40.44435938619999860, 1454.056667761929930, 264.0385842768980069 ) ) ;
#36245 = CARTESIAN_POINT ( 'NONE',  ( 12.91599431494240946, 1411.873776468889218, 269.3566367870338922 ) ) ;
#36247 = CARTESIAN_POINT ( 'NONE',  ( 8.754875282535529379, 1436.430644587890129, 208.9268862815009982 ) ) ;
#36248 = CARTESIAN_POINT ( 'NONE',  ( -11.81090838280000099, 1433.647990716570121, 150.7603589772980115 ) ) ;
#36249 = CARTESIAN_POINT ( 'NONE',  ( 0.1543026821579989993, 1487.992631772989853, 217.2489902802990116 ) ) ;
#36250 = CARTESIAN_POINT ( 'NONE',  ( -20.06661625339999944, 1486.017343259630252, 190.5747571216979850 ) ) ;
#36251 = CARTESIAN_POINT ( 'NONE',  ( 11.16746684139999957, 1409.469218647829848, 189.9183212870979958 ) ) ;
#36252 = CARTESIAN_POINT ( 'NONE',  ( 5.192738225420000298, 1422.609109026029955, 185.4141380594979864 ) ) ;
#36253 = CARTESIAN_POINT ( 'NONE',  ( -7.539474871700000413, 1438.620589098819892, 153.9375992959979840 ) ) ;
#36254 = CARTESIAN_POINT ( 'NONE',  ( -9.204572690731579243, 1450.041973421969942, 209.1554608508139950 ) ) ;
#36255 = CARTESIAN_POINT ( 'NONE',  ( -2.714057680736050138, 1440.141560261370159, 155.9947301247320013 ) ) ;
#36256 = CARTESIAN_POINT ( 'NONE',  ( -6.137775026819999979, 1452.698724561930021, 152.5573369345979984 ) ) ;
#36257 = ORIENTED_EDGE ( 'NONE', *, *, #7650, .T. ) ;
#36258 = CARTESIAN_POINT ( 'NONE',  ( -3.224549562455830021, 1508.551704408489968, 213.9552827710969893 ) ) ;
#36259 = CARTESIAN_POINT ( 'NONE',  ( 9.992014340670891670, 1491.422427633320012, 188.4943361087159985 ) ) ;
#36260 = CARTESIAN_POINT ( 'NONE',  ( -38.83547189680000145, 1453.431358638529900, 269.8277507654979672 ) ) ;
#36261 = CARTESIAN_POINT ( 'NONE',  ( -24.11880918795291606, 1435.788364753321275, 210.9889112370256044 ) ) ;
#36262 = CARTESIAN_POINT ( 'NONE',  ( 6.733046173459999117, 1443.913060387330006, 154.8821828340979891 ) ) ;
#36263 = DIRECTION ( 'NONE',  ( -0.6736849260863841948, 0.000000000000000000, 0.7390186874254148774 ) ) ;
#36264 = FACE_OUTER_BOUND ( 'NONE', #29989, .T. ) ;
#36265 = CARTESIAN_POINT ( 'NONE',  ( 2.923521462801879967, 1410.394928839790055, 231.6309329194170061 ) ) ;
#36266 = CARTESIAN_POINT ( 'NONE',  ( -1.556584322539999787, 1415.163755998629995, 226.9904013962980116 ) ) ;
#36267 = CARTESIAN_POINT ( 'NONE',  ( -4.185496514609999608, 1416.327449659429931, 232.4314624903980189 ) ) ;
#36268 = CARTESIAN_POINT ( 'NONE',  ( 7.281762805592231658, 1360.709910169842260, 207.6218459616987673 ) ) ;
#36269 = CARTESIAN_POINT ( 'NONE',  ( -44.07818812065350045, 1430.685783913769910, 266.7420579915649910 ) ) ;
#36270 = CARTESIAN_POINT ( 'NONE',  ( -2.695125831749999978, 1436.928758190210146, 184.7684663464980019 ) ) ;
#36271 = VERTEX_POINT ( 'NONE', #67916 ) ;
#36272 = CARTESIAN_POINT ( 'NONE',  ( -8.782009155840000858, 1423.187680728870191, 210.2326933490990086 ) ) ;
#36273 = VERTEX_POINT ( 'NONE', #108793 ) ;
#36274 = CARTESIAN_POINT ( 'NONE',  ( 1.133653140995000141, 1516.978425811520083, 209.8592968530090275 ) ) ;
#36275 = CARTESIAN_POINT ( 'NONE',  ( 7.012921545474999796, 1508.551704408389924, 203.6084103740869864 ) ) ;
#36276 = CARTESIAN_POINT ( 'NONE',  ( -20.61546995249999981, 1508.365016819329867, 190.3615313952979875 ) ) ;
#36277 = CARTESIAN_POINT ( 'NONE',  ( -14.19908403099999994, 1410.402768462430004, 190.3287729933980188 ) ) ;
#36278 = DIRECTION ( 'NONE',  ( 0.9999994573234139983, 9.540975887252238799E-32, -0.001041802705676339504 ) ) ;
#36279 = ORIENTED_EDGE ( 'NONE', *, *, #64845, .F. ) ;
#36280 = CARTESIAN_POINT ( 'NONE',  ( -49.24962907673571522, 1526.382868172863937, 10.34030387146701813 ) ) ;
#36282 = FACE_OUTER_BOUND ( 'NONE', #19556, .T. ) ;
#36281 = FACE_OUTER_BOUND ( 'NONE', #18497, .T. ) ;
#36283 = CARTESIAN_POINT ( 'NONE',  ( 11.60004869885203682, 1424.919886225515711, 136.4495339943606211 ) ) ;
#36284 = CARTESIAN_POINT ( 'NONE',  ( -16.32084964895840073, 1508.551704408389924, 213.4499384416680243 ) ) ;
#36285 = CARTESIAN_POINT ( 'NONE',  ( 9.986106302860001449, 1472.420748959189950, 214.7747459013789921 ) ) ;
#36286 = CARTESIAN_POINT ( 'NONE',  ( -9.105587270462899951, 1439.161147590870087, 208.1449012116760002 ) ) ;
#36287 = ORIENTED_EDGE ( 'NONE', *, *, #72591, .F. ) ;
#36288 = CARTESIAN_POINT ( 'NONE',  ( -16.87533949840419822, 1410.935239512470162, 270.3978791998690099 ) ) ;
#36289 = CARTESIAN_POINT ( 'NONE',  ( -5.789394700334999477, 1517.164987839469859, 207.4150481461570052 ) ) ;
#36290 = CARTESIAN_POINT ( 'NONE',  ( -28.12789902060000102, 1435.479491205339855, 135.2461919473980174 ) ) ;
#36291 = CARTESIAN_POINT ( 'NONE',  ( 8.899191358356040027, 1435.476522257870101, 207.7847561027849963 ) ) ;
#36293 = ORIENTED_EDGE ( 'NONE', *, *, #38046, .T. ) ;
#36292 = CARTESIAN_POINT ( 'NONE',  ( -6.371134682384000492, 1368.423166410931799, 210.6218459616987957 ) ) ;
#36294 = ORIENTED_EDGE ( 'NONE', *, *, #104202, .F. ) ;
#36295 = DIRECTION ( 'NONE',  ( -0.6709778558543747495, 0.000000000000000000, 0.7414773880254650340 ) ) ;
#36296 = EDGE_CURVE ( 'NONE', #38904, #43913, #109359, .T. ) ;
#36297 = CARTESIAN_POINT ( 'NONE',  ( -1.138272880244320051, 1409.887086923559764, 185.4055134639719995 ) ) ;
#36298 = CARTESIAN_POINT ( 'NONE',  ( 3.659006180651771967, 1425.028668711506043, 184.9642397768932938 ) ) ;
#36299 = LINE ( 'NONE', #71613, #100205 ) ;
#36300 = CARTESIAN_POINT ( 'NONE',  ( -19.89499272040000122, 1430.791176822330044, 223.1073517981980103 ) ) ;
#36301 = CARTESIAN_POINT ( 'NONE',  ( 5.279745845456099929, 1475.319256162549891, 269.4988495444229670 ) ) ;
#36302 = CARTESIAN_POINT ( 'NONE',  ( -11.66658784013729999, 1391.913060387289988, 209.7120188154370339 ) ) ;
#36303 = CARTESIAN_POINT ( 'NONE',  ( 10.27269517170000057, 1447.035794548080048, 186.9035346276980079 ) ) ;
#36304 =( BOUNDED_CURVE ( )  B_SPLINE_CURVE ( 3, ( #58825, #24630, #67244, #86221 ),
 .UNSPECIFIED., .F., .T. ) 
 B_SPLINE_CURVE_WITH_KNOTS ( ( 4, 4 ),
 ( 1.191031352841563917, 1.212284566114525841 ),
 .UNSPECIFIED. ) 
 CURVE ( )  GEOMETRIC_REPRESENTATION_ITEM ( )  RATIONAL_B_SPLINE_CURVE ( ( 1.000000000000000000, 0.9999623587646855327, 0.9999623587646855327, 1.000000000000000000 ) ) 
 REPRESENTATION_ITEM ( '' )  );
#36305 = CARTESIAN_POINT ( 'NONE',  ( 6.547556931335000385, 1516.633288330999903, 205.8595812817970057 ) ) ;
#36306 = EDGE_LOOP ( 'NONE', ( #9288, #66009, #44678, #89397 ) ) ;
#36307 = CARTESIAN_POINT ( 'NONE',  ( 19.03110457515579768, 1457.047041246000163, 226.1578386336209974 ) ) ;
#36308 = CARTESIAN_POINT ( 'NONE',  ( 1.472146761774899781, 1484.510777100460018, 182.0990331927370107 ) ) ;
#36309 = VERTEX_POINT ( 'NONE', #57858 ) ;
#36310 = CARTESIAN_POINT ( 'NONE',  ( 4.545982209787698736, 1508.783371651607240, 212.6094383991669474 ) ) ;
#36311 = CARTESIAN_POINT ( 'NONE',  ( 26.21478449920509846, 1450.935004627359831, 136.5697675719979713 ) ) ;
#36312 = CARTESIAN_POINT ( 'NONE',  ( -15.81201443571409904, 1506.433683733589987, 193.8503163142329981 ) ) ;
#36313 = CARTESIAN_POINT ( 'NONE',  ( -31.35957567500000209, 1388.283776034970060, 207.2672171163289931 ) ) ;
#36314 = CARTESIAN_POINT ( 'NONE',  ( 7.571416214730000149, 1423.019345440409779, 195.7264161940989879 ) ) ;
#36315 = CARTESIAN_POINT ( 'NONE',  ( 17.68757587670000220, 1410.455303309029887, 192.9846075591979968 ) ) ;
#36316 = CARTESIAN_POINT ( 'NONE',  ( -4.037927790559999508, 1496.698780035289928, 198.6284372844990003 ) ) ;
#36317 = CARTESIAN_POINT ( 'NONE',  ( 2.601738789480323000, 1439.644030142424072, 183.4006585331323720 ) ) ;
#36319 = CARTESIAN_POINT ( 'NONE',  ( -23.64337456402409998, 1435.765682558080016, 212.0350035351450231 ) ) ;
#36318 = CARTESIAN_POINT ( 'NONE',  ( -9.094910673856409389, 1384.931050598509955, 199.9427862989620053 ) ) ;
#36320 = CARTESIAN_POINT ( 'NONE',  ( 2.175409717514719593E-31, 1397.551704408390151, 209.1218459616989946 ) ) ;
#36321 = CARTESIAN_POINT ( 'NONE',  ( 29.02628104525710029, 1509.926680456929944, 206.2525988547419900 ) ) ;
#36322 = CARTESIAN_POINT ( 'NONE',  ( 3.264778779384999829, 1516.727068157269969, 214.1190961241369735 ) ) ;
#36323 = FACE_OUTER_BOUND ( 'NONE', #20511, .T. ) ;
#36324 = VERTEX_POINT ( 'NONE', #32639 ) ;
#36325 = DIRECTION ( 'NONE',  ( -0.3090169943749516146, 0.000000000000000000, -0.9510565162951523099 ) ) ;
#36326 = CARTESIAN_POINT ( 'NONE',  ( 21.61975802670987790, 1524.130440953581001, 234.4879735737363831 ) ) ;
#36327 = CARTESIAN_POINT ( 'NONE',  ( -0.5016765698272009910, 1409.762109374920101, 233.0393131857059927 ) ) ;
#36328 = ADVANCED_FACE ( 'NONE', ( #15795 ), #4352, .F. ) ;
#36329 = CARTESIAN_POINT ( 'NONE',  ( 1232.316865285700032, 2833.596074015789782, -9639.481875267569194 ) ) ;
#36330 = EDGE_CURVE ( 'NONE', #101391, #52522, #52228, .T. ) ;
#36331 = CARTESIAN_POINT ( 'NONE',  ( -1.288421119806714588, 1420.729263807338157, 193.7694644859544724 ) ) ;
#36332 = EDGE_CURVE ( 'NONE', #46325, #28853, #25358, .T. ) ;
#36333 = CARTESIAN_POINT ( 'NONE',  ( 19.41976554590000248, 1457.605858504690104, 210.0668255001349962 ) ) ;
#36334 = CARTESIAN_POINT ( 'NONE',  ( -8.518323187880001868, 1460.717990423530182, 243.9198229205979942 ) ) ;
#36335 = CARTESIAN_POINT ( 'NONE',  ( 15.79259708711904686, 1474.064254307462761, 266.8744062780497757 ) ) ;
#36336 = EDGE_CURVE ( 'NONE', #105303, #49707, #20023, .T. ) ;
#36337 = CARTESIAN_POINT ( 'NONE',  ( 11.87682525570000003, 1433.080808133479877, 149.9786264939980072 ) ) ;
#36338 = CARTESIAN_POINT ( 'NONE',  ( 4.163336342339999869E-15, 1416.181292664740113, 209.1218459616989946 ) ) ;
#36340 = EDGE_CURVE ( 'NONE', #103319, #47969, #33543, .T. ) ;
#36339 = CARTESIAN_POINT ( 'NONE',  ( -10.82576510151410076, 1461.830236086719879, 211.0839844832650272 ) ) ;
#36341 = B_SPLINE_SURFACE_WITH_KNOTS ( 'NONE', 5, 1, ( 
 ( #53733, #96253 ),
 ( #55367, #62691 ),
 ( #96813, #29585 ),
 ( #55918, #72183 ),
 ( #98445, #63770 ),
 ( #80002, #44767 ),
 ( #27945, #20084 ),
 ( #81092, #54818 ),
 ( #88943, #87871 ),
 ( #71084, #21714 ),
 ( #11161, #21160 ),
 ( #64323, #104648 ),
 ( #12236, #19528 ),
 ( #78918, #89499 ),
 ( #2224, #72714 ),
 ( #97886, #54277 ),
 ( #45322, #106837 ),
 ( #12792, #88402 ),
 ( #3325, #106302 ),
 ( #3873, #79460 ),
 ( #46970, #37450 ),
 ( #30131, #10596 ),
 ( #11695, #38536 ),
 ( #46425, #36891 ) ),
 .UNSPECIFIED., .F., .F., .F.,
 ( 6, 3, 3, 3, 3, 3, 3, 6 ),
 ( 2, 2 ),
 ( -1.071643382647970112E-05, 1.787098717269999915, 3.575031044529999757, 7.150895699039999442, 35.35713560909999842, 55.42405856439999923, 74.38977909560000512, 84.36278581140000199 ),
 ( 2.018281005271230111, 3.029715956260000009 ),
 .UNSPECIFIED. ) ;
#36342 = CARTESIAN_POINT ( 'NONE',  ( -9.385734277025909122, 1422.648365155559986, 192.2754659541220121 ) ) ;
#36343 = VERTEX_POINT ( 'NONE', #25309 ) ;
#36344 = DIRECTION ( 'NONE',  ( 0.7071067811860475283, 0.000000000000000000, 0.7071067811870476172 ) ) ;
#36345 = CARTESIAN_POINT ( 'NONE',  ( 24.09734436609999975, 1435.413501786879806, 137.5049309707980001 ) ) ;
#36346 = CARTESIAN_POINT ( 'NONE',  ( -12.16611854289999961, 1486.038279009429971, 184.6517507125980160 ) ) ;
#36347 = CARTESIAN_POINT ( 'NONE',  ( 7.982414096761766942, 1398.150145363782258, 198.8611880334231330 ) ) ;
#36348 = CARTESIAN_POINT ( 'NONE',  ( -4.925340228020513855, 1491.207026113694155, 188.8237031222513451 ) ) ;
#36349 = CARTESIAN_POINT ( 'NONE',  ( 25.18172488799999797, 1449.799985342450100, 212.0110979567280083 ) ) ;
#36350 = CARTESIAN_POINT ( 'NONE',  ( -16.47688868883378888, 1420.112172641060852, 208.7131226723711848 ) ) ;
#36351 = CARTESIAN_POINT ( 'NONE',  ( -15.46915279469999938, 1508.458298799929935, 231.5778441731980024 ) ) ;
#36352 = CARTESIAN_POINT ( 'NONE',  ( -20.17056002823349914, 1383.853403695010002, 220.8314763200619950 ) ) ;
#36353 = CARTESIAN_POINT ( 'NONE',  ( 20.04224800140000085, 1476.152569352130058, 225.0639570481980059 ) ) ;
#36354 = CARTESIAN_POINT ( 'NONE',  ( 2.499941270706060426, 1419.920042689079992, 110.8944432325759948 ) ) ;
#36355 = ADVANCED_FACE ( 'NONE', ( #17452 ), #83061, .T. ) ;
#36356 = CARTESIAN_POINT ( 'NONE',  ( -7.211935934568223239, 1522.051704408389924, 193.5679467272088345 ) ) ;
#36357 = CARTESIAN_POINT ( 'NONE',  ( 0.1656846011524400197, 1482.872822838080083, 181.9709779989089782 ) ) ;
#36359 = VERTEX_POINT ( 'NONE', #21857 ) ;
#36358 = CARTESIAN_POINT ( 'NONE',  ( 3.626340809789999842, 1441.877721644789972, 217.3328878409490130 ) ) ;
#36360 = CARTESIAN_POINT ( 'NONE',  ( -0.4725090650170000184, 1450.961208915830184, 181.9239884144979840 ) ) ;
#36361 = CARTESIAN_POINT ( 'NONE',  ( -5.380564766416549850E-17, 1384.485850024879937, 199.6505477045689929 ) ) ;
#36362 = CARTESIAN_POINT ( 'NONE',  ( -20.24816999180000110, 1507.884035326030016, 189.2341655923979999 ) ) ;
#36364 = VERTEX_POINT ( 'NONE', #5085 ) ;
#36363 = CARTESIAN_POINT ( 'NONE',  ( -32.18357971100785875, 1524.059663615500540, 216.7473357175133231 ) ) ;
#36365 = CARTESIAN_POINT ( 'NONE',  ( 18.38166776770140132, 1428.164217240339894, 201.4944361684150067 ) ) ;
#36366 = VERTEX_POINT ( 'NONE', #104805 ) ;
#36367 = ADVANCED_FACE ( 'NONE', ( #28093 ), #62856, .T. ) ;
#36368 = CARTESIAN_POINT ( 'NONE',  ( -12.25109094605330107, 1392.007944422769924, 210.6850267857309973 ) ) ;
#36369 = CARTESIAN_POINT ( 'NONE',  ( -16.06428786779999740, 1414.913060387329779, 209.3174441332850222 ) ) ;
#36370 = CARTESIAN_POINT ( 'NONE',  ( -2.487935123020000194, 1508.551704408389924, 214.1089243778970115 ) ) ;
#36371 = EDGE_CURVE ( 'NONE', #77376, #68723, #101020, .T. ) ;
#36372 = AXIS2_PLACEMENT_3D ( 'NONE', #69037, #33189, #60633 ) ;
#36373 = CARTESIAN_POINT ( 'NONE',  ( -3.007104530145896515, 1369.004598681105563, 207.6218459616999894 ) ) ;
#36374 = CARTESIAN_POINT ( 'NONE',  ( -0.6139455675770010279, 1430.723786662589873, 217.4810676936089919 ) ) ;
#36375 = CARTESIAN_POINT ( 'NONE',  ( -10.28050713296510033, 1472.193390648910054, 207.1071822515270071 ) ) ;
#36376 = CARTESIAN_POINT ( 'NONE',  ( 10.49013805814599998, 1409.279384075129883, 219.7750123596210017 ) ) ;
#36377 = CARTESIAN_POINT ( 'NONE',  ( -112.2014361534894817, 1347.163060387289988, 302.0278895525330540 ) ) ;
#36378 = CARTESIAN_POINT ( 'NONE',  ( -99.28926058784159636, 1385.219051903349964, 296.1397385972409779 ) ) ;
#36379 = CARTESIAN_POINT ( 'NONE',  ( -18.01683494470000113, 1424.194020404830098, 193.0485151117980251 ) ) ;
#36380 = CARTESIAN_POINT ( 'NONE',  ( -3.657993755839999750, 1474.872004365689918, 218.7367895275489786 ) ) ;
#36381 = ORIENTED_EDGE ( 'NONE', *, *, #18672, .F. ) ;
#36382 = ADVANCED_FACE ( 'NONE', ( #3472 ), #105920, .F. ) ;
#36383 = CARTESIAN_POINT ( 'NONE',  ( -0.7133045362011090074, 1467.033258661540003, 237.5733310560259781 ) ) ;
#36385 = EDGE_LOOP ( 'NONE', ( #11917, #21793, #12652, #43343 ) ) ;
#36384 = FACE_OUTER_BOUND ( 'NONE', #8856, .T. ) ;
#36386 = ORIENTED_EDGE ( 'NONE', *, *, #41240, .T. ) ;
#36387 = CARTESIAN_POINT ( 'NONE',  ( 28.15442102719999795, 1509.896234434229882, 217.4026611133980111 ) ) ;
#36388 = CARTESIAN_POINT ( 'NONE',  ( -3.792994181805666276, 1361.742475207348207, 207.6218459616988241 ) ) ;
#36389 = CARTESIAN_POINT ( 'NONE',  ( 1.887268207041509882, 1496.992342273679924, 196.8733779563050064 ) ) ;
#36390 = CARTESIAN_POINT ( 'NONE',  ( 29.51859446050732316, 1509.963736870992079, 211.6832300364890500 ) ) ;
#36391 = CARTESIAN_POINT ( 'NONE',  ( 21.58938658888978779, 1409.666978379882949, 207.8232565829630119 ) ) ;
#36392 = CARTESIAN_POINT ( 'NONE',  ( -28.27930516629999858, 1508.150008668130113, 209.2731387451690068 ) ) ;
#36393 = CARTESIAN_POINT ( 'NONE',  ( 32.48417584039749784, 1524.659802833172535, 201.1732701908057379 ) ) ;
#36394 = CARTESIAN_POINT ( 'NONE',  ( -5.931260097829800237, 1516.766044797163204, 213.7134053296210823 ) ) ;
#36395 = CARTESIAN_POINT ( 'NONE',  ( -0.1714601298129999896, 1471.143170311029962, 182.4338783372979833 ) ) ;
#36396 = CARTESIAN_POINT ( 'NONE',  ( -5.499060144977048203, 1369.740687513229432, 207.6218459616987673 ) ) ;
#36397 = CARTESIAN_POINT ( 'NONE',  ( -5.788436372295000076, 1517.116049120239950, 206.8334885244969712 ) ) ;
#36398 = CARTESIAN_POINT ( 'NONE',  ( -2.469101154908970308, 1524.816548299036640, 175.8588282813664705 ) ) ;
#36399 = CARTESIAN_POINT ( 'NONE',  ( 6.160531803039999588, 1422.363866332430007, 133.5160842810979887 ) ) ;
#36400 = CARTESIAN_POINT ( 'NONE',  ( -0.3821804589910179906, 1506.433683733660018, 187.1424611576989889 ) ) ;
#36401 = CARTESIAN_POINT ( 'NONE',  ( -2.697707841769999781, 1496.152875393589966, 220.1550137170989956 ) ) ;
#36402 = CARTESIAN_POINT ( 'NONE',  ( 41.46340468307529648, 1444.106639930779920, 136.3851283920170090 ) ) ;
#36403 = ORIENTED_EDGE ( 'NONE', *, *, #81129, .F. ) ;
#36404 = CARTESIAN_POINT ( 'NONE',  ( 45.67178422140000293, 1440.913060379869876, 266.1886048774979940 ) ) ;
#36405 = CARTESIAN_POINT ( 'NONE',  ( -24.95209251639999692, 1469.238639858829856, 202.6470309557579981 ) ) ;
#36407 = CARTESIAN_POINT ( 'NONE',  ( 16.22603119529000182, 1409.504885741160024, 192.8289540260319939 ) ) ;
#36406 = CARTESIAN_POINT ( 'NONE',  ( -10.78182592408190033, 1425.674068949819912, 99.91377539918158845 ) ) ;
#36408 = CARTESIAN_POINT ( 'NONE',  ( 3.461995158685000185, 1516.906233342200039, 211.9877574868770012 ) ) ;
#36409 = FACE_OUTER_BOUND ( 'NONE', #35585, .T. ) ;
#36410 = CARTESIAN_POINT ( 'NONE',  ( -22.15551762850000017, 1489.466917449829907, 208.0059448184480004 ) ) ;
#36411 = CARTESIAN_POINT ( 'NONE',  ( -24.64758684779999953, 1426.171069946930174, 240.2509105751980201 ) ) ;
#36412 = CARTESIAN_POINT ( 'NONE',  ( 3.347837012790000344, 1485.651792710489872, 219.4796433975990055 ) ) ;
#36413 = CARTESIAN_POINT ( 'NONE',  ( 29.15335220830669982, 1509.735908697959758, 209.5818691752959921 ) ) ;
#36414 = DIRECTION ( 'NONE',  ( 0.9072248115955994230, -0.3865001137603080728, -0.1660144671063280564 ) ) ;
#36415 = CARTESIAN_POINT ( 'NONE',  ( 20.59684415428669979, 1507.762623717989982, 227.6602567528719874 ) ) ;
#36416 = ORIENTED_EDGE ( 'NONE', *, *, #96154, .T. ) ;
#36417 = CARTESIAN_POINT ( 'NONE',  ( -6.531167973260559201, 1517.151704408390060, 216.7070295963201829 ) ) ;
#36418 = CARTESIAN_POINT ( 'NONE',  ( 15.00581739583218521, 1514.742486326955941, 225.2136390995225383 ) ) ;
#36419 = CARTESIAN_POINT ( 'NONE',  ( 37.77042218360499959, 1442.790213541490175, 137.1073832719119991 ) ) ;
#36420 = ORIENTED_EDGE ( 'NONE', *, *, #105597, .T. ) ;
#36421 = ORIENTED_EDGE ( 'NONE', *, *, #85304, .F. ) ;
#36422 = CARTESIAN_POINT ( 'NONE',  ( 8.853608006785520956, 1452.164931631960144, 211.9660445263369866 ) ) ;
#36423 = CARTESIAN_POINT ( 'NONE',  ( 8.607172403139999872, 1425.024168402240093, 195.3267954577989940 ) ) ;
#36424 = EDGE_CURVE ( 'NONE', #54363, #67527, #73654, .T. ) ;
#36425 = ORIENTED_EDGE ( 'NONE', *, *, #82003, .T. ) ;
#36426 = CARTESIAN_POINT ( 'NONE',  ( 13.37406854550570046, 1507.496451373729997, 233.0472692220099873 ) ) ;
#36427 = CARTESIAN_POINT ( 'NONE',  ( -6.349477754588637168, 1419.387435849262829, 195.0908289166754059 ) ) ;
#36428 = CARTESIAN_POINT ( 'NONE',  ( -9.862951377749247683, 1517.151704408390060, 228.3939896778649654 ) ) ;
#36429 = CARTESIAN_POINT ( 'NONE',  ( -11.43754841480000017, 1461.185958034129953, 231.4422348057979946 ) ) ;
#36430 = CARTESIAN_POINT ( 'NONE',  ( 7.443079130664420617, 1508.729257029040127, 203.0017267375970107 ) ) ;
#36431 = CARTESIAN_POINT ( 'NONE',  ( -11.84966374040000048, 1391.913060387289988, 210.3228853754790180 ) ) ;
#36432 = CARTESIAN_POINT ( 'NONE',  ( 0.2576823252080000515, 1419.224537961029910, 184.6439154818979773 ) ) ;
#36433 = ORIENTED_EDGE ( 'NONE', *, *, #10580, .T. ) ;
#36434 = CARTESIAN_POINT ( 'NONE',  ( -2.874588960795000148, 1516.606339319019980, 202.5748942495170013 ) ) ;
#36435 = CARTESIAN_POINT ( 'NONE',  ( -2.868112169295000236, 1516.855632454399938, 209.8795095036720113 ) ) ;
#36436 = ORIENTED_EDGE ( 'NONE', *, *, #106284, .F. ) ;
#36437 = CARTESIAN_POINT ( 'NONE',  ( 11.86064628478500005, 1431.955178181789961, 149.9690613615080110 ) ) ;
#36438 = EDGE_CURVE ( 'NONE', #73608, #26364, #99128, .T. ) ;
#36439 = CARTESIAN_POINT ( 'NONE',  ( 5.513435558552499671, 1509.038615934029849, 201.6090957240569992 ) ) ;
#36440 = VERTEX_POINT ( 'NONE', #49312 ) ;
#36441 = DIRECTION ( 'NONE',  ( 0.000000000000000000, -1.000000000000000000, 0.000000000000000000 ) ) ;
#36442 = CARTESIAN_POINT ( 'NONE',  ( -6.558694315301119460, 1508.421471884069888, 219.8384412560889984 ) ) ;
#36443 = CARTESIAN_POINT ( 'NONE',  ( -2.813822098188480059, 1367.641464703512383, 209.1220808600859300 ) ) ;
#36444 =( BOUNDED_SURFACE ( )  B_SPLINE_SURFACE ( 1, 2, ( 
 ( #39295, #21363, #5139, #13518, #37648, #29247, #38735 ),
 ( #71853, #73467, #28141, #29791, #62332, #2975, #89695 ) ),
 .UNSPECIFIED., .F., .F., .T. ) 
 B_SPLINE_SURFACE_WITH_KNOTS ( ( 2, 2 ),
 ( 3, 2, 2, 3 ),
 ( -10000.00000000000000, 10000.00000000000000 ),
 ( 2.609770915052339824, 3.141592653589790007, 4.712388980384689674, 5.770213224332369606 ),
 .UNSPECIFIED. ) 
 GEOMETRIC_REPRESENTATION_ITEM ( )  RATIONAL_B_SPLINE_SURFACE ( (
 ( 0.8688191111210129547, 0.9008356601183090673, 1.000000000000000000, 0.7071067811865480168, 1.000000000000000000, 0.8027563838394459195, 0.8711730262106620604),
 ( 0.8688191111210129547, 0.9008356601183090673, 1.000000000000000000, 0.7071067811865480168, 1.000000000000000000, 0.8027563838394459195, 0.8711730262106620604) ) ) 
 REPRESENTATION_ITEM ( '' )  SURFACE ( )  );
#36445 = CARTESIAN_POINT ( 'NONE',  ( -4.824314178002369502, 1468.483533977829893, 219.2782425545100011 ) ) ;
#36446 = CARTESIAN_POINT ( 'NONE',  ( -4.746427511560000312, 1423.669336908029891, 184.8320719503979888 ) ) ;
#36447 = CARTESIAN_POINT ( 'NONE',  ( 4.188705820677620650, 1409.351545472750104, 270.3708454374540224 ) ) ;
#36448 = DIRECTION ( 'NONE',  ( -0.1403878024439498828, 0.9900965937346509760, 0.000000000000000000 ) ) ;
#36449 = DIRECTION ( 'NONE',  ( -0.000000000000000000, -1.000000000000000000, -0.000000000000000000 ) ) ;
#36450 = CARTESIAN_POINT ( 'NONE',  ( -2.449516837986489559, 1422.315028397099923, 192.7719440642819961 ) ) ;
#36451 = CARTESIAN_POINT ( 'NONE',  ( -42.01596790420000360, 1379.656258535449979, 226.0503548403590059 ) ) ;
#36452 = CIRCLE ( 'NONE', #86485, 3.994150673153873399 ) ;
#36453 = CARTESIAN_POINT ( 'NONE',  ( 7.443246446248299009, 1423.092341332710021, 195.6161848952980051 ) ) ;
#36455 = DIRECTION ( 'NONE',  ( 0.000000000000000000, 0.7071067811865474617, 0.7071067811865474617 ) ) ;
#36454 = CARTESIAN_POINT ( 'NONE',  ( -20.30540503779999995, 1505.205473082589833, 209.2397414641690148 ) ) ;
#36456 = CARTESIAN_POINT ( 'NONE',  ( -65.44977854107980875, 1379.747342584464377, 275.4353169227350691 ) ) ;
#36457 = CARTESIAN_POINT ( 'NONE',  ( -9.932527294720630451, 1439.673512841460024, 207.9640247163430047 ) ) ;
#36458 = CARTESIAN_POINT ( 'NONE',  ( -6.479185156475000262, 1511.503799556569902, 201.7413190995169998 ) ) ;
#36459 = EDGE_LOOP ( 'NONE', ( #87173, #13435, #83509, #63033 ) ) ;
#36460 = CARTESIAN_POINT ( 'NONE',  ( 14.73695825489999933, 1419.186926028530252, 255.3819207742980097 ) ) ;
#36461 = AXIS2_PLACEMENT_3D ( 'NONE', #68616, #1400, #94903 ) ;
#36462 = CARTESIAN_POINT ( 'NONE',  ( 21.83550407203906119, 1523.678648413191468, 183.2743720722706655 ) ) ;
#36464 = CARTESIAN_POINT ( 'NONE',  ( -68.45946465731660169, 1385.029717728800051, 293.2748923492039808 ) ) ;
#36463 = B_SPLINE_CURVE_WITH_KNOTS ( 'NONE', 3,
 ( #50010, #41606, #26438, #93093, #16909, #67928, #16364, #51114, #15804, #77958, #717, #109907, #59518, #9099, #100929, #34295 ),
 .UNSPECIFIED., .F., .F.,
 ( 4, 3, 3, 3, 3, 4 ),
 ( -7.690120649562800281, -7.200842779664780480, -6.186030432389340028, -5.174050502141839480, -4.163300565000019660, -3.154256035599999564 ),
 .UNSPECIFIED. ) ;
#36465 = B_SPLINE_SURFACE_WITH_KNOTS ( 'NONE', 5, 5, ( 
 ( #44788, #78938, #36360, #70551, #104670, #90615, #21734, #73278, #5519 ),
 ( #47531, #29607, #81652, #13339, #89518, #81113, #13895, #107416, #30712 ),
 ( #64898, #99006, #30151, #63258, #63793, #22281, #56484, #4957, #54841 ),
 ( #48081, #4430, #99558, #73842, #82215, #39101, #90056, #39674, #97907 ),
 ( #12256, #46445, #107969, #54298, #31266, #80577, #46989, #3892, #65448 ),
 ( #106324, #64342, #98465, #88965, #38023, #38556, #55386, #72202, #105792 ),
 ( #88427, #21178, #72734, #106860, #37470, #11717, #55937, #45888, #80025 ),
 ( #3346, #97367, #20639, #12809, #71673, #29074, #59251, #74401, #83323 ),
 ( #66006, #84429, #83870, #6067, #14996, #109635, #40220, #93369, #76030 ) ),
 .UNSPECIFIED., .F., .F., .F.,
 ( 6, 3, 6 ),
 ( 6, 3, 6 ),
 ( 1.581906524000000092, 2.897190900920000090, 4.210865504630000089 ),
 ( 0.000000000000000000, 1.000000000000000000, 2.000000000000000000 ),
 .UNSPECIFIED. ) ;
#36466 = CARTESIAN_POINT ( 'NONE',  ( -16.68062049856758122, 1526.382868172863937, 181.4122394607865942 ) ) ;
#36467 = ADVANCED_FACE ( 'NONE', ( #65012 ), #15122, .T. ) ;
#36468 = CARTESIAN_POINT ( 'NONE',  ( 5.123510356189999726, 1506.385164154990207, 219.6030550502989911 ) ) ;
#36469 = CARTESIAN_POINT ( 'NONE',  ( -12.81436613661749924, 1447.032455685610103, 185.6742731520540133 ) ) ;
#36471 = ORIENTED_EDGE ( 'NONE', *, *, #105916, .F. ) ;
#36470 = CARTESIAN_POINT ( 'NONE',  ( -1.700207153400070004, 1515.066230056300128, 204.7924348194040078 ) ) ;
#36472 = CARTESIAN_POINT ( 'NONE',  ( 18.18137294690000161, 1507.608465325429734, 188.5297611294979845 ) ) ;
#36473 = CARTESIAN_POINT ( 'NONE',  ( -24.22142878869999905, 1443.578504641800009, 212.3984149774479988 ) ) ;
#36474 = CARTESIAN_POINT ( 'NONE',  ( -15.89685123880000006, 1415.918798422770124, 209.5438913505039977 ) ) ;
#36475 = CARTESIAN_POINT ( 'NONE',  ( -6.436826263860000452, 1460.741096996990109, 209.1237132485140080 ) ) ;
#36476 = CARTESIAN_POINT ( 'NONE',  ( 12.04512424413499971, 1511.810036768419877, 224.5882503546669682 ) ) ;
#36477 = CARTESIAN_POINT ( 'NONE',  ( 3.855903220025218125, 1370.345307389557092, 209.9425081570149985 ) ) ;
#36478 = CARTESIAN_POINT ( 'NONE',  ( 28.12945447419999923, 1510.024089002930168, 194.4010711305979839 ) ) ;
#36479 = CIRCLE ( 'NONE', #47207, 95.87929217111340563 ) ;
#36480 = DIRECTION ( 'NONE',  ( 0.000000000000000000, 1.000000000000000000, 0.000000000000000000 ) ) ;
#36481 = CARTESIAN_POINT ( 'NONE',  ( -5.386185223340929973, 1432.347042777500064, 154.6076275972019971 ) ) ;
#36482 = CARTESIAN_POINT ( 'NONE',  ( 5.914165527020000646, 1417.414484838129965, 231.4237124127979826 ) ) ;
#36483 = ADVANCED_FACE ( 'NONE', ( #5654 ), #83438, .T. ) ;
#36484 = CARTESIAN_POINT ( 'NONE',  ( -4.652798870049999813, 1476.958451974490117, 219.7229608691989995 ) ) ;
#36485 = CARTESIAN_POINT ( 'NONE',  ( -15.94730198739999949, 1459.284216063530039, 229.6241229289979913 ) ) ;
#36486 = CARTESIAN_POINT ( 'NONE',  ( 6.546302742015000398, 1516.577434278289957, 206.6347425125669872 ) ) ;
#36487 = CARTESIAN_POINT ( 'NONE',  ( 39.48010127979999595, 1422.408814482829939, 266.8920267569980069 ) ) ;
#36489 = DIRECTION ( 'NONE',  ( -1.000000000000000000, 0.000000000000000000, 0.000000000000000000 ) ) ;
#36488 = AXIS2_PLACEMENT_3D ( 'NONE', #28167, #67017, #34908 ) ;
#36490 = CARTESIAN_POINT ( 'NONE',  ( 18.94140730250000004, 1435.974603093500036, 146.3778792160980231 ) ) ;
#36491 = CARTESIAN_POINT ( 'NONE',  ( 21.17607668140000143, 1469.155376887830016, 194.0056914575980329 ) ) ;
#36492 = EDGE_CURVE ( 'NONE', #37425, #73065, #92551, .T. ) ;
#36493 = CARTESIAN_POINT ( 'NONE',  ( 5.386185205460879644, 1432.347042709529887, 154.6076275981190236 ) ) ;
#36494 = CARTESIAN_POINT ( 'NONE',  ( -1.197716701820000118, 1479.406703890490007, 229.6030852470990169 ) ) ;
#36495 = CARTESIAN_POINT ( 'NONE',  ( -31.50880186010000017, 1466.258756145929965, 266.5723332967979786 ) ) ;
#36497 = B_SPLINE_CURVE_WITH_KNOTS ( 'NONE', 3,
 ( #57460, #55250, #4813, #108389, #80983, #91587, #23262, #21048, #89382, #38959 ),
 .UNSPECIFIED., .F., .F.,
 ( 4, 2, 2, 2, 4 ),
 ( 3.469446951953613804E-18, 0.0007403986298595397093, 0.001480797259719075949, 0.002221195889578612189, 0.002961594519438148429 ),
 .UNSPECIFIED. ) ;
#36496 = CARTESIAN_POINT ( 'NONE',  ( 32.23393008313279040, 1523.382868172864164, 216.8400319010852400 ) ) ;
#36498 = CARTESIAN_POINT ( 'NONE',  ( 18.83903520582832414, 1477.219481574037900, 217.3633840002517843 ) ) ;
#36499 = CARTESIAN_POINT ( 'NONE',  ( -6.448255163698850545, 1408.606950372470010, 197.2260920424329811 ) ) ;
#36500 = DIRECTION ( 'NONE',  ( 2.775557561562888827E-14, 0.000000000000000000, 1.000000000000000000 ) ) ;
#36501 = CARTESIAN_POINT ( 'NONE',  ( -13.57767673750000093, 1442.998007393829994, 188.1052366738979913 ) ) ;
#36502 = CARTESIAN_POINT ( 'NONE',  ( -27.79335146049099947, 1508.202759685119872, 210.4818766450680130 ) ) ;
#36503 = CARTESIAN_POINT ( 'NONE',  ( -33.91369295919999871, 1437.010537939619780, 136.5611922338979696 ) ) ;
#36504 = CARTESIAN_POINT ( 'NONE',  ( -10.16993673199276671, 1455.367861617207382, 226.0916021546657646 ) ) ;
#36505 = ORIENTED_EDGE ( 'NONE', *, *, #61441, .F. ) ;
#36506 = FACE_OUTER_BOUND ( 'NONE', #20977, .T. ) ;
#36507 = CARTESIAN_POINT ( 'NONE',  ( -14.45571664180179994, 1409.417865136020055, 212.8813991959680152 ) ) ;
#36508 = ORIENTED_EDGE ( 'NONE', *, *, #4504, .F. ) ;
#36509 = EDGE_CURVE ( 'NONE', #70768, #67802, #72454, .T. ) ;
#36510 = CARTESIAN_POINT ( 'NONE',  ( -13.59448967766789806, 1507.983772107289951, 209.3963046402899977 ) ) ;
#36511 = FACE_OUTER_BOUND ( 'NONE', #104395, .T. ) ;
#36512 = CARTESIAN_POINT ( 'NONE',  ( -31.62532717830000095, 1466.392620420529965, 268.6459143616979759 ) ) ;
#36513 = CARTESIAN_POINT ( 'NONE',  ( -17.13990208540000282, 1503.228774872230133, 224.1177471422980148 ) ) ;
#36514 = CARTESIAN_POINT ( 'NONE',  ( 0.2707015808795459888, 1419.455472800460029, 184.4597787253470074 ) ) ;
#36515 = ADVANCED_FACE ( 'NONE', ( #15658 ), #75949, .F. ) ;
#36516 = CARTESIAN_POINT ( 'NONE',  ( 20.53760542139786693, 1525.821544997590308, 233.5223198772804949 ) ) ;
#36517 = CARTESIAN_POINT ( 'NONE',  ( -61.62836627276490020, 1384.689555943140022, 283.6559180833200458 ) ) ;
#36518 = CARTESIAN_POINT ( 'NONE',  ( -45.28208375225440818, 1385.003918354740108, 218.6697845988200015 ) ) ;
#36519 = CARTESIAN_POINT ( 'NONE',  ( 16.60890868733800119, 1423.045925081060204, 227.3707771178220014 ) ) ;
#36520 = CARTESIAN_POINT ( 'NONE',  ( 20.61484677210000171, 1508.366076579829951, 227.7402271394979891 ) ) ;
#36521 = CARTESIAN_POINT ( 'NONE',  ( 14.29966752569999855, 1463.297110392330069, 223.2977952946979769 ) ) ;
#36522 = CARTESIAN_POINT ( 'NONE',  ( -10.63631708518249752, 1493.561200479843819, 205.8325361800690132 ) ) ;
#36523 = CARTESIAN_POINT ( 'NONE',  ( 3.984081798389999651, 1515.551704150889918, 207.2788819995389815 ) ) ;
#36524 = CARTESIAN_POINT ( 'NONE',  ( -9.094536456969999350, 1384.945384211949886, 199.9428478864389831 ) ) ;
#36525 = CARTESIAN_POINT ( 'NONE',  ( -23.07071866700000129, 1409.718707635629926, 208.5793258069899707 ) ) ;
#36526 = CARTESIAN_POINT ( 'NONE',  ( 18.05542495199999919, 1416.825784011830137, 208.7596466302789793 ) ) ;
#36527 = CARTESIAN_POINT ( 'NONE',  ( -12.60360202350000058, 1416.535385209630022, 194.9281104267980140 ) ) ;
#36528 = CARTESIAN_POINT ( 'NONE',  ( 2.021030077200000274, 1421.580652348860212, 193.8043510613990179 ) ) ;
#36529 = CARTESIAN_POINT ( 'NONE',  ( 23.01976738670000344, 1409.881403417030015, 211.5932151611179961 ) ) ;
#36530 = CARTESIAN_POINT ( 'NONE',  ( -11.95607891459999905, 1433.549464727329905, 149.8823818600980076 ) ) ;
#36531 = CARTESIAN_POINT ( 'NONE',  ( 18.90005065560000119, 1456.739796555589919, 200.1223556290190118 ) ) ;
#36532 = DIRECTION ( 'NONE',  ( -0.02616798426500960631, 0.9993150019883682011, -0.02616798426500970345 ) ) ;
#36534 = DIRECTION ( 'NONE',  ( 0.000000000000000000, 1.000000000000000000, -0.000000000000000000 ) ) ;
#36533 = DIRECTION ( 'NONE',  ( -0.8775825618903734249, -0.000000000000000000, -0.4794255386042018952 ) ) ;
#36535 = CARTESIAN_POINT ( 'NONE',  ( -0.1139762647940000123, 1411.657414646530015, 233.3213770427979910 ) ) ;
#36536 = CARTESIAN_POINT ( 'NONE',  ( -0.4151546846821903003, 1512.187213306747481, 242.9330574173806951 ) ) ;
#36537 = CARTESIAN_POINT ( 'NONE',  ( -11.95245250920000046, 1489.692386819589956, 211.6783199228790124 ) ) ;
#36538 = CARTESIAN_POINT ( 'NONE',  ( -23.10158782639999941, 1411.031839777530195, 210.9252372482680187 ) ) ;
#36539 = AXIS2_PLACEMENT_3D ( 'NONE', #24552, #58740, #5016 ) ;
#36540 = CARTESIAN_POINT ( 'NONE',  ( -9.505471540889999460, 1363.500209798500009, 210.6218459616991936 ) ) ;
#36541 = CARTESIAN_POINT ( 'NONE',  ( -0.7560907659159991079, 1516.770163853809890, 204.1215159365669933 ) ) ;
#36542 = CARTESIAN_POINT ( 'NONE',  ( -18.99822365203170094, 1485.804394114710021, 189.5286731071130077 ) ) ;
#36543 = CARTESIAN_POINT ( 'NONE',  ( 7.287626706846419999, 1504.670790707109973, 218.7321252575409858 ) ) ;
#36544 = CARTESIAN_POINT ( 'NONE',  ( -4.256729589579360429, 1441.274763077670059, 159.9751555247389945 ) ) ;
#36545 = VECTOR ( 'NONE', #79500, 1000.000000000000114 ) ;
#36547 = EDGE_LOOP ( 'NONE', ( #106812, #9182, #38429, #105124 ) ) ;
#36546 = CARTESIAN_POINT ( 'NONE',  ( -67.13862316386790496, 1379.745831551899983, 278.1727330697519847 ) ) ;
#36548 = ORIENTED_EDGE ( 'NONE', *, *, #25867, .T. ) ;
#36549 = CARTESIAN_POINT ( 'NONE',  ( 11.39672343189880088, 1433.938446316660020, 151.4312701205349754 ) ) ;
#36550 = CARTESIAN_POINT ( 'NONE',  ( 21.80586012576933541, 1523.954924407801855, 183.3405100316582832 ) ) ;
#36551 = ORIENTED_EDGE ( 'NONE', *, *, #91840, .F. ) ;
#36552 = CARTESIAN_POINT ( 'NONE',  ( -2.401759440763739040, 1456.579829547543568, 199.9421882610167245 ) ) ;
#36553 = CARTESIAN_POINT ( 'NONE',  ( 11.07826983750000061, 1500.667907230989840, 205.8218841770989798 ) ) ;
#36555 = CARTESIAN_POINT ( 'NONE',  ( 4.823778297959999684, 1426.859560269130043, 144.1938086916980239 ) ) ;
#36554 = CARTESIAN_POINT ( 'NONE',  ( 15.86818584750560035, 1417.144054420810107, 191.3226642558889807 ) ) ;
#36556 = DIRECTION ( 'NONE',  ( 1.000000000000000000, 0.000000000000000000, 0.000000000000000000 ) ) ;
#36557 = CARTESIAN_POINT ( 'NONE',  ( -33.93019615848960768, 1522.382868172863937, 197.6607374646001176 ) ) ;
#36558 = CARTESIAN_POINT ( 'NONE',  ( 0.03360429821169879511, 1468.905055714589935, 219.1740298947989913 ) ) ;
#36559 = CARTESIAN_POINT ( 'NONE',  ( -24.08412280772440184, 1444.795065662000070, 211.8316922065289987 ) ) ;
#36560 =( NAMED_UNIT ( * ) PLANE_ANGLE_UNIT ( ) SI_UNIT ( $, .RADIAN. ) );
#36561 = PRODUCT_DEFINITION_SHAPE ( 'NONE', 'NONE',  #25390 ) ;
#36562 = CARTESIAN_POINT ( 'NONE',  ( -4.027697264044999947, 1516.766397346390022, 212.0005392193770035 ) ) ;
#36563 = CARTESIAN_POINT ( 'NONE',  ( 13.81908124298479912, 1415.258594621350085, 197.5028968623049934 ) ) ;
#36564 = CARTESIAN_POINT ( 'NONE',  ( -12.95799293189999979, 1421.417920776069877, 210.6553815501089844 ) ) ;
#36565 = FACE_OUTER_BOUND ( 'NONE', #32153, .T. ) ;
#36566 = VERTEX_POINT ( 'NONE', #28511 ) ;
#36567 = CARTESIAN_POINT ( 'NONE',  ( 13.51024008597019943, 1434.958051702800049, 149.0116953593919789 ) ) ;
#36568 = CARTESIAN_POINT ( 'NONE',  ( -12.14766904159599825, 1440.691551917680044, 223.4139461185880009 ) ) ;
#36569 = VERTEX_POINT ( 'NONE', #29069 ) ;
#36570 = EDGE_LOOP ( 'NONE', ( #85162, #21755, #796, #29439, #109141 ) ) ;
#36571 = VERTEX_POINT ( 'NONE', #54834 ) ;
#36572 = CARTESIAN_POINT ( 'NONE',  ( -8.375502483594999603, 1512.383155430640045, 215.8646805558269932 ) ) ;
#36573 = CARTESIAN_POINT ( 'NONE',  ( 15.90990255763500016, 1512.830284628050094, 198.1616908427670296 ) ) ;
#36574 = EDGE_CURVE ( 'NONE', #49356, #34770, #12452, .T. ) ;
#36575 = DIRECTION ( 'NONE',  ( 0.9455185755993178454, 0.000000000000000000, -0.3255681544571537578 ) ) ;
#36576 = CARTESIAN_POINT ( 'NONE',  ( -8.023209542600000077, 1384.926838732019860, 218.7874811480190260 ) ) ;
#36577 = CARTESIAN_POINT ( 'NONE',  ( 9.870105591850000692, 1461.985261895689973, 208.8208347412080172 ) ) ;
#36578 = CARTESIAN_POINT ( 'NONE',  ( -18.40330103019589814, 1508.551701338139992, 210.4131062939880223 ) ) ;
#36579 = CARTESIAN_POINT ( 'NONE',  ( -59.10074528520486581, 1379.721676241261093, 259.3488587256716187 ) ) ;
#36580 = CARTESIAN_POINT ( 'NONE',  ( 4.223239625950419907, 1446.235523347980006, 167.1961359861499830 ) ) ;
#36581 = LINE ( 'NONE', #70780, #66455 ) ;
#36582 = VECTOR ( 'NONE', #70653, 1000.000000000000000 ) ;
#36583 = ORIENTED_EDGE ( 'NONE', *, *, #48129, .T. ) ;
#36584 = CARTESIAN_POINT ( 'NONE',  ( 2.864043418315000089, 1516.811292230880099, 206.8228319013669818 ) ) ;
#36585 = ORIENTED_EDGE ( 'NONE', *, *, #97878, .F. ) ;
#36586 = CARTESIAN_POINT ( 'NONE',  ( 24.64606047185390025, 1440.913060387330006, 237.9243720522470085 ) ) ;
#36587 = EDGE_CURVE ( 'NONE', #109446, #58146, #104642, .T. ) ;
#36588 = CARTESIAN_POINT ( 'NONE',  ( -17.69367671410000398, 1508.290913714329918, 186.8003383294980040 ) ) ;
#36589 = ORIENTED_EDGE ( 'NONE', *, *, #50187, .F. ) ;
#36590 = CARTESIAN_POINT ( 'NONE',  ( -6.081362942748859801, 1508.610509101569960, 201.8017925879439929 ) ) ;
#36591 = CARTESIAN_POINT ( 'NONE',  ( -15.18679397699999889, 1410.815794815029903, 190.8549424428979933 ) ) ;
#36592 = CARTESIAN_POINT ( 'NONE',  ( -57.28860159201197177, 1379.717568064870875, 260.4116547525887881 ) ) ;
#36594 = DIRECTION ( 'NONE',  ( 0.03489949670075159077, -0.9993908270191568244, -1.181473170880211640E-10 ) ) ;
#36593 = CARTESIAN_POINT ( 'NONE',  ( -24.38625746622182433, 1440.079494890380602, 212.0144860022579678 ) ) ;
#36595 = CARTESIAN_POINT ( 'NONE',  ( -11.06583617882839832, 1414.913527292460003, 196.0153757934279781 ) ) ;
#36596 = CARTESIAN_POINT ( 'NONE',  ( 26.07583925208389886, 1441.264734006110075, 138.1452381084750130 ) ) ;
#36597 = CARTESIAN_POINT ( 'NONE',  ( -12.06095611880000007, 1433.903655509099963, 149.2721377443980089 ) ) ;
#36598 = CARTESIAN_POINT ( 'NONE',  ( 21.17685425119999820, 1435.236150072139935, 141.6298919720979939 ) ) ;
#36600 = CARTESIAN_POINT ( 'NONE',  ( -0.8415958139899989421, 1498.413741156690094, 200.5784037818789898 ) ) ;
#36599 = CARTESIAN_POINT ( 'NONE',  ( 6.115264850039999978, 1465.022781530429938, 233.8169749081980058 ) ) ;
#36601 = B_SPLINE_SURFACE_WITH_KNOTS ( 'NONE', 5, 5, ( 
 ( #22076, #90402, #55746, #73640, #81445, #73079, #63598, #46793, #107770 ),
 ( #99348, #80922, #63063, #55192, #88775, #12057, #106660, #29950, #3690 ),
 ( #38351, #64144, #98262, #21531, #18586, #86917, #71264, #10775, #37068 ),
 ( #28673, #69601, #78529, #63412, #52781, #45503, #43820, #19709, #62879 ),
 ( #10209, #44385, #1840, #35975, #37621, #87488, #52235, #44947, #29223 ),
 ( #54454, #9645, #53912, #104277, #97527, #27564, #105385, #79094, #95870 ) ),
 .UNSPECIFIED., .F., .F., .F.,
 ( 6, 6 ),
 ( 6, 3, 6 ),
 ( 39.30566966140000318, 56.26181215439999761 ),
 ( 0.000000000000000000, 1.000000000000000000, 2.000000000000000000 ),
 .UNSPECIFIED. ) ;
#36602 = CARTESIAN_POINT ( 'NONE',  ( 1.130607463874999885, 1516.632821972880038, 215.6700465578769865 ) ) ;
#36603 = CARTESIAN_POINT ( 'NONE',  ( -0.06914114004050241069, 1462.882045625689898, 228.8295648571990171 ) ) ;
#36604 = CARTESIAN_POINT ( 'NONE',  ( -26.27875192360060197, 1507.830998981459970, 209.1491001731010044 ) ) ;
#36605 = CARTESIAN_POINT ( 'NONE',  ( 27.96976559109999982, 1509.201555290129818, 207.5796322881679998 ) ) ;
#36606 = CARTESIAN_POINT ( 'NONE',  ( -2.864972154145000172, 1516.859514182039902, 212.0024388992169975 ) ) ;
#36607 = CARTESIAN_POINT ( 'NONE',  ( -11.49316453475270094, 1482.710248906200150, 206.0058552507379943 ) ) ;
#36608 = CARTESIAN_POINT ( 'NONE',  ( -18.97219799319119815, 1486.246528605739741, 189.3000344508529906 ) ) ;
#36610 = VERTEX_POINT ( 'NONE', #98459 ) ;
#36609 = CARTESIAN_POINT ( 'NONE',  ( -92.02227936059999536, 1390.573016258800180, 301.9656767862589959 ) ) ;
#36611 = CARTESIAN_POINT ( 'NONE',  ( -0.9518847404100000409, 1415.296882282229944, 227.0497707501980074 ) ) ;
#36612 = CARTESIAN_POINT ( 'NONE',  ( 27.24390625040000202, 1454.605078681330042, 244.3119004044979761 ) ) ;
#36613 = ADVANCED_FACE ( 'NONE', ( #36905 ), #45338, .F. ) ;
#36614 = CARTESIAN_POINT ( 'NONE',  ( 30.68434753607487764, 1526.000688113786737, 216.8500914425656845 ) ) ;
#36615 = CARTESIAN_POINT ( 'NONE',  ( -14.31200009510000015, 1415.739699867260015, 203.9225122001990087 ) ) ;
#36616 = CARTESIAN_POINT ( 'NONE',  ( 4.363122647530000009, 1416.108409730630001, 162.4768476156980057 ) ) ;
#36617 = EDGE_CURVE ( 'NONE', #49524, #38319, #92063, .T. ) ;
#36618 = CARTESIAN_POINT ( 'NONE',  ( -18.72510712869999949, 1457.176800226130126, 227.4990798502979885 ) ) ;
#36619 = CIRCLE ( 'NONE', #43732, 2.000000000052873261 ) ;
#36620 = ADVANCED_FACE ( 'NONE', ( #2240 ), #14188, .T. ) ;
#36622 = CARTESIAN_POINT ( 'NONE',  ( 5.360339899599590119, 1422.243068060369978, 144.1383403130810166 ) ) ;
#36621 = CARTESIAN_POINT ( 'NONE',  ( 11.86937491419999979, 1432.581104674459993, 149.9818612858980202 ) ) ;
#36623 = CARTESIAN_POINT ( 'NONE',  ( -9.466486982440619258, 1449.314193870430017, 207.5699851590599962 ) ) ;
#36624 = CARTESIAN_POINT ( 'NONE',  ( -105.9692983431669973, 1380.841777212760235, 308.5995165648880629 ) ) ;
#36625 = ORIENTED_EDGE ( 'NONE', *, *, #105132, .F. ) ;
#36626 = CARTESIAN_POINT ( 'NONE',  ( 2.287084270065000258, 1517.068517094990057, 204.1085709707169826 ) ) ;
#36627 = CARTESIAN_POINT ( 'NONE',  ( 1.328042612950000034, 1406.002643151530037, 266.9604903208979749 ) ) ;
#36628 = AXIS2_PLACEMENT_3D ( 'NONE', #21429, #30402, #72436 ) ;
#36629 = CARTESIAN_POINT ( 'NONE',  ( 1.842963219479999859, 1515.064792519189950, 213.4512947472589985 ) ) ;
#36630 = AXIS2_PLACEMENT_3D ( 'NONE', #101749, #25037, #59239 ) ;
#36631 = EDGE_CURVE ( 'NONE', #105296, #98890, #53420, .T. ) ;
#36632 = CARTESIAN_POINT ( 'NONE',  ( 6.399316741296109612, 1471.586156901340019, 269.6149390625339493 ) ) ;
#36633 =( BOUNDED_SURFACE ( )  B_SPLINE_SURFACE ( 3, 2, ( 
 ( #48594, #83276, #6574 ),
 ( #40722, #74894, #103935 ),
 ( #53563, #25550, #2057 ),
 ( #949, #59742, #95537 ) ),
 .UNSPECIFIED., .F., .F., .T. ) 
 B_SPLINE_SURFACE_WITH_KNOTS ( ( 4, 4 ),
 ( 3, 3 ),
 ( 0.000000000000000000, 0.0002960034161023848936 ),
 ( 0.000000000000000000, 1.000000000000000000 ),
 .UNSPECIFIED. ) 
 GEOMETRIC_REPRESENTATION_ITEM ( )  RATIONAL_B_SPLINE_SURFACE ( (
 ( 1.000000000000000000, 0.8070209408750060875, 1.000000000000000000),
 ( 1.000000000000000000, 0.8071723757218383088, 1.000000000000000000),
 ( 1.000000000000000000, 0.8072480346917747518, 1.000000000000000000),
 ( 1.000000000000000000, 0.8072480644198177790, 1.000000000000000000) ) ) 
 REPRESENTATION_ITEM ( '' )  SURFACE ( )  );
#36634 = CARTESIAN_POINT ( 'NONE',  ( 5.440910205060000671, 1437.356219380560105, 154.7142170579979847 ) ) ;
#36635 = CARTESIAN_POINT ( 'NONE',  ( 3.135857944719999679, 1466.984112378690043, 218.9566967715590238 ) ) ;
#36636 = CARTESIAN_POINT ( 'NONE',  ( -39.22252855717829334, 1440.913060397279878, 258.1633042160279388 ) ) ;
#36637 = CARTESIAN_POINT ( 'NONE',  ( 37.66833179081890393, 1449.093331502820092, 136.3452658211859898 ) ) ;
#36638 = DIRECTION ( 'NONE',  ( -0.1481527700395769420, 0.3686965082634817703, 0.9176675005272424412 ) ) ;
#36639 = CARTESIAN_POINT ( 'NONE',  ( 0.4140934722930009748, 1432.034230537489975, 200.6936621557090064 ) ) ;
#36640 = CARTESIAN_POINT ( 'NONE',  ( 9.183393462700504273, 1463.661249169792200, 215.2717992091796475 ) ) ;
#36641 = CARTESIAN_POINT ( 'NONE',  ( 0.7301356836779989701, 1507.011728406289876, 221.2028043055989883 ) ) ;
#36642 = CARTESIAN_POINT ( 'NONE',  ( -18.60492040140000114, 1442.815685133389934, 206.3625141719689964 ) ) ;
#36643 = ORIENTED_EDGE ( 'NONE', *, *, #23070, .T. ) ;
#36644 = FACE_OUTER_BOUND ( 'NONE', #42901, .T. ) ;
#36645 = DIRECTION ( 'NONE',  ( 0.000000000000000000, 0.000000000000000000, -1.000000000000000000 ) ) ;
#36646 = CARTESIAN_POINT ( 'NONE',  ( 4.498205314171340952, 1465.056958170999906, 200.2655687005689913 ) ) ;
#36647 = CARTESIAN_POINT ( 'NONE',  ( -0.5524668390069999990, 1475.317206268129894, 269.4985896541979855 ) ) ;
#36648 = DIRECTION ( 'NONE',  ( -0.02952616936612191892, 0.9995640069543085815, 3.638695136259567707E-05 ) ) ;
#36649 = CARTESIAN_POINT ( 'NONE',  ( -29.99620953741503371, 1526.382868172863937, 198.4974435154502999 ) ) ;
#36650 = EDGE_CURVE ( 'NONE', #94190, #71731, #76022, .T. ) ;
#36651 = LINE ( 'NONE', #38836, #59265 ) ;
#36652 = CARTESIAN_POINT ( 'NONE',  ( -10.65556547286379896, 1384.888491042710257, 218.8119669670159908 ) ) ;
#36653 = CARTESIAN_POINT ( 'NONE',  ( -17.64235773549999919, 1415.063410501330054, 207.5649593417179801 ) ) ;
#36654 = CARTESIAN_POINT ( 'NONE',  ( -10.43759599350000045, 1482.453041218790077, 205.4625892378089986 ) ) ;
#36655 = CARTESIAN_POINT ( 'NONE',  ( 26.57374339968509958, 1436.576538602379969, 136.7711906959450232 ) ) ;
#36656 = AXIS2_PLACEMENT_3D ( 'NONE', #85424, #58604, #17658 ) ;
#36658 = ADVANCED_FACE ( 'NONE', ( #66000 ), #83971, .T. ) ;
#36657 = CARTESIAN_POINT ( 'NONE',  ( -8.408055307214409524, 1396.206676148849965, 216.3013428204890261 ) ) ;
#36659 =( BOUNDED_CURVE ( )  B_SPLINE_CURVE ( 3, ( #103168, #26470, #1295, #60664 ),
 .UNSPECIFIED., .F., .T. ) 
 B_SPLINE_CURVE_WITH_KNOTS ( ( 4, 4 ),
 ( 1.006279808626920014, 2.135312847049839924 ),
 .UNSPECIFIED. ) 
 CURVE ( )  GEOMETRIC_REPRESENTATION_ITEM ( )  RATIONAL_B_SPLINE_CURVE ( ( 1.000000000000000000, 0.8965649099742322159, 0.8965649099742322159, 1.000000000000000000 ) ) 
 REPRESENTATION_ITEM ( '' )  );
#36660 = CARTESIAN_POINT ( 'NONE',  ( -2.825661703002820158, 1508.551704408389924, 204.1562177343460007 ) ) ;
#36661 = CARTESIAN_POINT ( 'NONE',  ( -16.29312086328269871, 1409.507180582139881, 225.3571590951270025 ) ) ;
#36662 = CARTESIAN_POINT ( 'NONE',  ( 11.89544747750000120, 1434.541746328260160, 147.6465872843980094 ) ) ;
#36663 = VERTEX_POINT ( 'NONE', #94753 ) ;
#36664 = CARTESIAN_POINT ( 'NONE',  ( -11.37084677945475164, 1501.461804469615572, 207.7930807248614258 ) ) ;
#36665 = CARTESIAN_POINT ( 'NONE',  ( -13.58041510073769942, 1508.551704408389924, 210.3416170870220014 ) ) ;
#36666 = VECTOR ( 'NONE', #43878, 1000.000000000000000 ) ;
#36667 = CARTESIAN_POINT ( 'NONE',  ( -11.74015294769649920, 1428.979986577860018, 144.1937977377450011 ) ) ;
#36669 = DIRECTION ( 'NONE',  ( -7.229590540988901841E-06, 0.03108153742028734942, -0.9995168522737994943 ) ) ;
#36668 = CARTESIAN_POINT ( 'NONE',  ( 10.12215235309999883, 1425.175395598030036, 101.9133589526980046 ) ) ;
#36670 = CARTESIAN_POINT ( 'NONE',  ( -16.16285233240872188, 1409.477476458355795, 225.0537141666407592 ) ) ;
#36671 = DIRECTION ( 'NONE',  ( -0.9455185755993167351, 0.000000000000000000, 0.3255681544571568109 ) ) ;
#36672 = CARTESIAN_POINT ( 'NONE',  ( 6.942354273414999888, 1516.905946377369901, 201.4030824261969883 ) ) ;
#36673 = CARTESIAN_POINT ( 'NONE',  ( 7.539740262130000481, 1425.605416228270087, 212.1797667491989898 ) ) ;
#36674 = CARTESIAN_POINT ( 'NONE',  ( -9.838224505759999516, 1462.268909614690074, 227.9668215275989667 ) ) ;
#36675 = CARTESIAN_POINT ( 'NONE',  ( 6.811012384640000583, 1507.262578865030036, 182.5160571543979984 ) ) ;
#36676 = CARTESIAN_POINT ( 'NONE',  ( 0.2612772751870610088, 1416.851343895820037, 190.7759414009450154 ) ) ;
#36677 = CARTESIAN_POINT ( 'NONE',  ( -113.4000000000000057, 1379.413060386290226, 304.2217751689950092 ) ) ;
#36678 = CARTESIAN_POINT ( 'NONE',  ( 8.654519645408177198, 1365.419269571389577, 210.6218459617142003 ) ) ;
#36680 = ORIENTED_EDGE ( 'NONE', *, *, #38125, .T. ) ;
#36679 = CARTESIAN_POINT ( 'NONE',  ( 8.040162348720000907, 1454.435424808689959, 215.4819357908390316 ) ) ;
#36681 = EDGE_LOOP ( 'NONE', ( #48848, #36030, #53598, #106424 ) ) ;
#36682 = CARTESIAN_POINT ( 'NONE',  ( -40.71507211770000367, 1443.618860023849948, 137.1015985469979910 ) ) ;
#36683 = CARTESIAN_POINT ( 'NONE',  ( -0.2985181081541919967, 1490.954057054879968, 236.6328081109120092 ) ) ;
#36684 = CARTESIAN_POINT ( 'NONE',  ( 0.000000000000000000, 1524.090675761330203, 232.8211094035767985 ) ) ;
#36685 = CARTESIAN_POINT ( 'NONE',  ( -7.558229903455000454, 1510.775363762149937, 212.9756020941370309 ) ) ;
#36687 = CARTESIAN_POINT ( 'NONE',  ( 21.13734888319999783, 1496.938803861589804, 209.1218459616989946 ) ) ;
#36686 = CARTESIAN_POINT ( 'NONE',  ( -107.1062838689999950, 1390.174440383410001, 309.0839720245589888 ) ) ;
#36688 = CARTESIAN_POINT ( 'NONE',  ( -32.36539586358053810, 1523.843263703803586, 202.1341903664009294 ) ) ;
#36689 = CARTESIAN_POINT ( 'NONE',  ( 12.41437396263700066, 1421.386826425689833, 223.7211383651710150 ) ) ;
#36690 =( NAMED_UNIT ( * ) SI_UNIT ( $, .STERADIAN. ) SOLID_ANGLE_UNIT ( ) );
#36691 = CARTESIAN_POINT ( 'NONE',  ( 35.15277841134140147, 1435.727150378580063, 135.4689313601830065 ) ) ;
#36692 = CARTESIAN_POINT ( 'NONE',  ( 29.68682906300000113, 1435.534167576209938, 135.1977161657979991 ) ) ;
#36693 = CARTESIAN_POINT ( 'NONE',  ( 13.66950429799999966, 1409.390409995830169, 216.6296730155279988 ) ) ;
#36694 = CARTESIAN_POINT ( 'NONE',  ( -0.7719351484700760491, 1406.066357371350023, 269.0457477767660066 ) ) ;
#36695 = CARTESIAN_POINT ( 'NONE',  ( 40.71369707939999927, 1443.851488934740019, 137.1197025281979904 ) ) ;
#36696 = ORIENTED_EDGE ( 'NONE', *, *, #30850, .T. ) ;
#36697 = CARTESIAN_POINT ( 'NONE',  ( -11.76903983939999954, 1432.302179094919893, 150.8119321882979875 ) ) ;
#36698 = CARTESIAN_POINT ( 'NONE',  ( 13.04724490819999971, 1442.955582623249938, 187.2795607120979753 ) ) ;
#36699 = VERTEX_POINT ( 'NONE', #28101 ) ;
#36700 = ORIENTED_EDGE ( 'NONE', *, *, #26824, .F. ) ;
#36701 = CARTESIAN_POINT ( 'NONE',  ( -3.668914018200000182, 1454.923457869790127, 200.3099103192890027 ) ) ;
#36702 = CARTESIAN_POINT ( 'NONE',  ( -9.516636888329999877, 1366.309137899869938, 207.6218459616989946 ) ) ;
#36703 = CARTESIAN_POINT ( 'NONE',  ( -2.480813923114999930, 1517.051603658920158, 214.1347848340070072 ) ) ;
#36704 = CARTESIAN_POINT ( 'NONE',  ( 2.698112791424999823, 1512.326491219019999, 216.8133626242469916 ) ) ;
#36705 = EDGE_LOOP ( 'NONE', ( #86180, #82828, #53326, #43853, #97973 ) ) ;
#36706 = FACE_OUTER_BOUND ( 'NONE', #1192, .T. ) ;
#36707 = CARTESIAN_POINT ( 'NONE',  ( -88.16707049670000629, 1374.885509058189882, 298.5681932088589861 ) ) ;
#36708 = AXIS2_PLACEMENT_3D ( 'NONE', #35133, #69875, #104549 ) ;
#36709 = B_SPLINE_CURVE_WITH_KNOTS ( 'NONE', 3,
 ( #71268, #44950, #1843, #88594, #28677, #79097, #53915, #11335 ),
 .UNSPECIFIED., .F., .F.,
 ( 4, 2, 2, 4 ),
 ( 0.0001365944327631960203, 0.003338885444831087533, 0.004940030950865032314, 0.006541176456898977962 ),
 .UNSPECIFIED. ) ;
#36710 = CARTESIAN_POINT ( 'NONE',  ( -106.8013500654249981, 1378.913060387289988, 301.4297679048889904 ) ) ;
#36711 = CARTESIAN_POINT ( 'NONE',  ( -2.297085753945000253, 1516.718889242609976, 205.0950684461469962 ) ) ;
#36712 = B_SPLINE_CURVE_WITH_KNOTS ( 'NONE', 5,
 ( #105970, #63437, #38191, #96456, #97555, #37093, #20829, #55024, #105408, #28701, #53937, #62906, #97017, #106502, #89151 ),
 .UNSPECIFIED., .F., .F.,
 ( 6, 3, 3, 3, 6 ),
 ( 0.000000000000000000, 0.2761287575458264421, 0.5540238061273354830, 0.8350199265002417048, 1.000000000000000000 ),
 .UNSPECIFIED. ) ;
#36713 = CARTESIAN_POINT ( 'NONE',  ( 2.330134126090000368, 1515.551704408389924, 212.9514660752490158 ) ) ;
#36714 = B_SPLINE_SURFACE_WITH_KNOTS ( 'NONE', 5, 5, ( 
 ( #19091, #45452, #79594, #20747, #54944, #10730, #2897, #2352, #44901 ),
 ( #108628, #81757, #108068, #66107, #72838, #40317, #30812, #64449, #31915 ),
 ( #64989, #39777, #5626, #89617, #22946, #74499, #82869, #99107, #48189 ),
 ( #65546, #15098, #31363, #106971, #49290, #98565, #23511, #21834, #73936 ),
 ( #22384, #13440, #90718, #5062, #99655, #100232, #30258, #57704, #56583 ),
 ( #91820, #83418, #14002, #57151, #91276, #12908, #14556, #6714, #6163 ),
 ( #82327, #48746, #40869, #75046, #109198, #56032, #32482, #90159, #66654 ),
 ( #21284, #4529, #55492, #47087, #47630, #81213, #38662, #39209, #73386 ),
 ( #107521, #41436, #50942, #68862, #77792, #67198, #8914, #43089, #26265 ),
 ( #25702, #100756, #34123, #41984, #101296, #43640, #68312, #101858, #76679 ),
 ( #60454, #25151, #1101, #35230, #85614, #58239, #9476, #83972, #110274 ),
 ( #33011, #93463, #24046, #86184, #16196, #92363, #550, #77250, #15636 ),
 ( #24592, #8357, #58785, #94572, #50397, #17845, #59355, #51484, #92924 ),
 ( #84526, #34674, #94025, #42523, #17288, #110830, #16735, #67748, #102421 ),
 ( #85067, #49842, #59904, #7814, #7272, #76133, #102966, #52048, #75602 ) ),
 .UNSPECIFIED., .F., .F., .F.,
 ( 6, 3, 3, 3, 6 ),
 ( 6, 3, 6 ),
 ( 8.074854476129999625, 11.27964861890000137, 15.06487702990000166, 20.05826248609999851, 31.54355322360000002 ),
 ( 0.000000000000000000, 1.000000000000000000, 2.000000000000000000 ),
 .UNSPECIFIED. ) ;
#36715 = CARTESIAN_POINT ( 'NONE',  ( -89.15855235860000505, 1384.953912536200050, 292.2553702161590081 ) ) ;
#36716 = CARTESIAN_POINT ( 'NONE',  ( 4.616899834755000320, 1517.050041317280147, 201.3993091674070115 ) ) ;
#36717 = CARTESIAN_POINT ( 'NONE',  ( -5.244631414159999672, 1410.030825445330038, 231.7638218180980232 ) ) ;
#36719 = ORIENTED_EDGE ( 'NONE', *, *, #20651, .T. ) ;
#36718 = CARTESIAN_POINT ( 'NONE',  ( -12.19576576879999941, 1445.284189276100051, 186.5171162045979827 ) ) ;
#36720 = DIRECTION ( 'NONE',  ( 0.000000000000000000, 0.000000000000000000, -1.000000000000000000 ) ) ;
#36721 = CARTESIAN_POINT ( 'NONE',  ( -24.99421969891459838, 1440.913060486799850, 216.0048573796309768 ) ) ;
#36722 = CARTESIAN_POINT ( 'NONE',  ( -19.17520157370000078, 1384.525909681719895, 220.5202403064590158 ) ) ;
#36723 = CARTESIAN_POINT ( 'NONE',  ( -4.460976907891178733, 1441.968611084702388, 201.4736981887971865 ) ) ;
#36724 = CARTESIAN_POINT ( 'NONE',  ( -25.04882088009999919, 1436.150498452359898, 137.5238809139979992 ) ) ;
#36725 = CARTESIAN_POINT ( 'NONE',  ( 34.96986345050569867, 1422.094637478340019, 270.1431711936880333 ) ) ;
#36726 = CARTESIAN_POINT ( 'NONE',  ( 5.786837678925000006, 1517.040132827679827, 212.3790665729270017 ) ) ;
#36727 = CARTESIAN_POINT ( 'NONE',  ( -67.28931209470000852, 1379.745217898479950, 277.1039849055590594 ) ) ;
#36728 = CARTESIAN_POINT ( 'NONE',  ( 0.01932857556553018927, 1507.377889191095164, 237.3808053707595604 ) ) ;
#36729 = CARTESIAN_POINT ( 'NONE',  ( 16.37089355035010030, 1427.986872975570122, 201.3297975146790009 ) ) ;
#36731 = CARTESIAN_POINT ( 'NONE',  ( 9.738306733412100513, 1493.400156934610095, 188.2659883396410123 ) ) ;
#36730 = VECTOR ( 'NONE', #73825, 1000.000000000000000 ) ;
#36732 = CARTESIAN_POINT ( 'NONE',  ( -2.292217048824999992, 1516.941178807709775, 209.1350424789999920 ) ) ;
#36733 = ORIENTED_EDGE ( 'NONE', *, *, #40371, .T. ) ;
#36734 = CARTESIAN_POINT ( 'NONE',  ( 12.27615406349190152, 1509.341753133656539, 182.5553123939410227 ) ) ;
#36735 = CARTESIAN_POINT ( 'NONE',  ( -3.618106369209999951, 1415.374423376830009, 232.5614439549979977 ) ) ;
#36736 = CARTESIAN_POINT ( 'NONE',  ( -43.08024461549999273, 1385.034280802249896, 247.5058162161589905 ) ) ;
#36737 = ORIENTED_EDGE ( 'NONE', *, *, #46016, .F. ) ;
#36738 = CARTESIAN_POINT ( 'NONE',  ( -24.35956345089839914, 1385.258544084970026, 223.2439328304530193 ) ) ;
#36739 = DIRECTION ( 'NONE',  ( 0.4770263929449307105, 0.7067418228238977473, 0.5224574779879248565 ) ) ;
#36740 = EDGE_CURVE ( 'NONE', #27006, #43749, #994, .T. ) ;
#36741 = CARTESIAN_POINT ( 'NONE',  ( 16.37204142619090064, 1469.006598734869840, 229.5670462769519986 ) ) ;
#36742 = AXIS2_PLACEMENT_3D ( 'NONE', #57265, #81317, #65099 ) ;
#36743 = CARTESIAN_POINT ( 'NONE',  ( -22.70684900021230135, 1509.410791795379964, 226.2783582751810059 ) ) ;
#36744 = CARTESIAN_POINT ( 'NONE',  ( -2.825023821920000344, 1409.011712393730022, 187.6092908591980120 ) ) ;
#36745 = CARTESIAN_POINT ( 'NONE',  ( -0.3610188369850000356, 1409.865909257629937, 233.1896167169979890 ) ) ;
#36746 = CARTESIAN_POINT ( 'NONE',  ( -20.92767404034479028, 1512.187213306747481, 235.3888156262297571 ) ) ;
#36748 = CARTESIAN_POINT ( 'NONE',  ( 15.09400015716100008, 1464.825201970499847, 194.8529889085539821 ) ) ;
#36747 = CARTESIAN_POINT ( 'NONE',  ( -4.615017365965000451, 1516.987478262539980, 215.6816440265270103 ) ) ;
#36749 = CARTESIAN_POINT ( 'NONE',  ( 19.06709222750000166, 1507.978133761729850, 188.5708093027980112 ) ) ;
#36750 = CARTESIAN_POINT ( 'NONE',  ( 10.94246130620789970, 1470.964434095790239, 209.6243324065490015 ) ) ;
#36751 = EDGE_LOOP ( 'NONE', ( #4776, #49360, #65267, #85096, #41527 ) ) ;
#36752 = CARTESIAN_POINT ( 'NONE',  ( -11.48654377540849936, 1414.913057860449953, 197.4148903956670154 ) ) ;
#36753 = FACE_OUTER_BOUND ( 'NONE', #15600, .T. ) ;
#36754 = VERTEX_POINT ( 'NONE', #78517 ) ;
#36755 = DIRECTION ( 'NONE',  ( -0.6736849260863841948, 0.000000000000000000, 0.7390186874254148774 ) ) ;
#36756 = ADVANCED_FACE ( 'NONE', ( #36506 ), #35963, .T. ) ;
#36757 = CARTESIAN_POINT ( 'NONE',  ( 4.629464564640000113, 1426.297974515259966, 211.0805667635490011 ) ) ;
#36758 = CARTESIAN_POINT ( 'NONE',  ( 7.536818026188599973, 1511.326458810320219, 202.9508713580690085 ) ) ;
#36759 = CARTESIAN_POINT ( 'NONE',  ( 3.149572309329999875, 1442.624013563290191, 217.4256031491790111 ) ) ;
#36760 = CARTESIAN_POINT ( 'NONE',  ( -33.05665451062068172, 1523.390106123591067, 200.9313857523611375 ) ) ;
#36761 = CARTESIAN_POINT ( 'NONE',  ( -21.32681782946734828, 1525.211473355384896, 234.3841091294584373 ) ) ;
#36762 = B_SPLINE_CURVE_WITH_KNOTS ( 'NONE', 5,
 ( #2330, #104755, #19636, #53838, #87977, #90137, #99634, #99086, #90693 ),
 .UNSPECIFIED., .F., .F.,
 ( 6, 3, 6 ),
 ( 0.000000000000000000, 0.5437164176757826040, 1.000000000000000000 ),
 .UNSPECIFIED. ) ;
#36763 = CARTESIAN_POINT ( 'NONE',  ( 18.08041632129999954, 1415.296882296330068, 210.6774151550479814 ) ) ;
#36764 = CARTESIAN_POINT ( 'NONE',  ( -28.27139721233033143, 1526.382868172863937, 219.5606225550389752 ) ) ;
#36765 = CARTESIAN_POINT ( 'NONE',  ( -16.07930208289999996, 1436.295294290089942, 148.8862706138980059 ) ) ;
#36766 = EDGE_CURVE ( 'NONE', #56739, #64419, #73433, .T. ) ;
#36767 = CARTESIAN_POINT ( 'NONE',  ( -2.446787376320000096, 1432.353341358199941, 150.2884730787980061 ) ) ;
#36768 = CARTESIAN_POINT ( 'NONE',  ( 16.16809600799999913, 1413.530257726130003, 191.4342317662980122 ) ) ;
#36770 = CARTESIAN_POINT ( 'NONE',  ( 0.5884825575569611056, 1477.920118691090011, 187.7824158287019998 ) ) ;
#36769 = CARTESIAN_POINT ( 'NONE',  ( -17.69507376908103424, 1521.951704408389787, 216.2288492090250998 ) ) ;
#36771 = CARTESIAN_POINT ( 'NONE',  ( -30.25425994616995240, 1522.382868172863937, 218.9520509131593258 ) ) ;
#36772 = VERTEX_POINT ( 'NONE', #63399 ) ;
#36773 = CARTESIAN_POINT ( 'NONE',  ( 1.556350644722900078, 1415.152886232740002, 191.3166872668830081 ) ) ;
#36774 = CARTESIAN_POINT ( 'NONE',  ( 25.13460091010000141, 1469.176458824629890, 206.2207530469580092 ) ) ;
#36775 = CARTESIAN_POINT ( 'NONE',  ( -11.88526718636376067, 1433.193527212150912, 149.9682077723181806 ) ) ;
#36776 = CARTESIAN_POINT ( 'NONE',  ( -3.428557866510000274, 1483.455582133289909, 199.0092266202990174 ) ) ;
#36777 = CARTESIAN_POINT ( 'NONE',  ( -16.42371717981465906, 1417.596043028402619, 205.5727573974847076 ) ) ;
#36778 = CARTESIAN_POINT ( 'NONE',  ( -2.038646110889595242, 1525.960063244516959, 241.1857569150894562 ) ) ;
#36779 = CARTESIAN_POINT ( 'NONE',  ( 19.31623058889999811, 1475.513060387329915, 217.5297674309880165 ) ) ;
#36780 = CARTESIAN_POINT ( 'NONE',  ( 26.80766065159997069, 1436.328454115282284, 136.7303795916004390 ) ) ;
#36781 = CARTESIAN_POINT ( 'NONE',  ( -11.24888976860679968, 1470.384811285099886, 210.8887443170019935 ) ) ;
#36782 = CARTESIAN_POINT ( 'NONE',  ( -7.501016434054790238, 1489.462053520290056, 217.1422798885779741 ) ) ;
#36783 = CARTESIAN_POINT ( 'NONE',  ( -0.03315926146910300187, 1502.038558776489936, 233.2541124319990047 ) ) ;
#36784 = CARTESIAN_POINT ( 'NONE',  ( -84.17015566942070848, 1383.774096447810052, 306.0826382659470255 ) ) ;
#36785 = CARTESIAN_POINT ( 'NONE',  ( -109.7475505361389878, 1384.114406720439774, 311.3182628089780337 ) ) ;
#36786 = CARTESIAN_POINT ( 'NONE',  ( 10.81518794224679958, 1424.921099295370141, 144.1705737284439977 ) ) ;
#36788 = EDGE_CURVE ( 'NONE', #32282, #46630, #70719, .T. ) ;
#36787 = CARTESIAN_POINT ( 'NONE',  ( -1.606066254855309960, 1516.556413965820184, 201.4122352545150250 ) ) ;
#36790 = ORIENTED_EDGE ( 'NONE', *, *, #96767, .F. ) ;
#36789 = CARTESIAN_POINT ( 'NONE',  ( 21.40470761700000324, 1507.840874668130027, 191.1187993005979990 ) ) ;
#36791 = FACE_OUTER_BOUND ( 'NONE', #87344, .T. ) ;
#36792 = CARTESIAN_POINT ( 'NONE',  ( -75.49415276370000072, 1384.770980541030212, 276.6885382114589902 ) ) ;
#36793 = DIRECTION ( 'NONE',  ( 0.8090169943749551118, 0.000000000000000000, 0.5877852522924624790 ) ) ;
#36794 = EDGE_LOOP ( 'NONE', ( #22379, #14530, #23470, #62530 ) ) ;
#36795 = ORIENTED_EDGE ( 'NONE', *, *, #96189, .T. ) ;
#36796 = CARTESIAN_POINT ( 'NONE',  ( 18.33918424680000214, 1416.543503932829935, 209.3898435056050005 ) ) ;
#36797 = CARTESIAN_POINT ( 'NONE',  ( -109.3494501450000058, 1384.931116597319942, 297.1385459540589977 ) ) ;
#36798 = CARTESIAN_POINT ( 'NONE',  ( 12.61676916276099725, 1442.788706415137540, 169.4674284520042988 ) ) ;
#36800 = CARTESIAN_POINT ( 'NONE',  ( -1.577671622059999856E-08, 1474.725719134630026, 264.8986983836979903 ) ) ;
#36799 = CARTESIAN_POINT ( 'NONE',  ( 35.03707096594791892, 1424.091692757612918, 269.5320251267563094 ) ) ;
#36801 = CARTESIAN_POINT ( 'NONE',  ( -5.187859588409159173, 1494.961024232720092, 197.9425774163800327 ) ) ;
#36802 = CARTESIAN_POINT ( 'NONE',  ( -11.28694401269999936, 1433.836412287389976, 151.5342276279979785 ) ) ;
#36803 = B_SPLINE_CURVE_WITH_KNOTS ( 'NONE', 3,
 ( #7277, #67753, #24597, #85620, #76685, #34680, #100763, #110282, #50947, #50405, #86188, #102426, #52053, #41442, #17294, #8920, #109737, #75607, #68868, #25157, #109203, #84531, #40875, #75053, #42531, #32488, #15641, #44312 ),
 .UNSPECIFIED., .F., .F.,
 ( 4, 3, 3, 3, 3, 3, 3, 3, 3, 4 ),
 ( -27.07213034072810132, -26.96001054729109825, -26.59046874310789832, -26.18598420665719928, -25.74274519917580051, -25.56107395287200035, -25.09940057177660222, -24.72598341592859938, -24.42045415469999980, -24.41308947359999948 ),
 .UNSPECIFIED. ) ;
#36804 = CARTESIAN_POINT ( 'NONE',  ( -0.6387392339020010468, 1488.293180997690115, 217.2118250028790101 ) ) ;
#36805 = CARTESIAN_POINT ( 'NONE',  ( 11.69034591517040056, 1426.726663316670056, 140.8301495756180088 ) ) ;
#36806 = CARTESIAN_POINT ( 'NONE',  ( 5.689812125580000490, 1409.111753005129913, 187.6973877038979879 ) ) ;
#36807 = CARTESIAN_POINT ( 'NONE',  ( 6.251976625090000184, 1423.636347555029943, 186.2373219085980054 ) ) ;
#36808 = CARTESIAN_POINT ( 'NONE',  ( -1.694729585588290011, 1515.066341861390129, 213.4512541762859996 ) ) ;
#36809 = CARTESIAN_POINT ( 'NONE',  ( 9.836119452340000180, 1438.961854673600101, 152.9388124017980317 ) ) ;
#36810 = CARTESIAN_POINT ( 'NONE',  ( -9.641170858363588891, 1424.230922240009932, 204.6135712703660090 ) ) ;
#36811 = CARTESIAN_POINT ( 'NONE',  ( 2.857351367441036238, 1525.661276915132476, 241.0960470690656052 ) ) ;
#36812 = LINE ( 'NONE', #71003, #12195 ) ;
#36813 = ORIENTED_EDGE ( 'NONE', *, *, #92471, .T. ) ;
#36814 = CARTESIAN_POINT ( 'NONE',  ( -11.93942137219999999, 1507.056495409390209, 208.6096073126149975 ) ) ;
#36815 = AXIS2_PLACEMENT_3D ( 'NONE', #91170, #14448, #60910 ) ;
#36816 = CARTESIAN_POINT ( 'NONE',  ( -5.659004368249999750, 1491.641286619889797, 185.8655773011990107 ) ) ;
#36817 = CARTESIAN_POINT ( 'NONE',  ( -42.54899106340000259, 1442.425395630990124, 270.0692087720980226 ) ) ;
#36818 = DIRECTION ( 'NONE',  ( 0.9455185755993166241, -1.675808339056839216E-14, -0.3255681544571569219 ) ) ;
#36819 = CARTESIAN_POINT ( 'NONE',  ( 3.346415545340000186, 1442.759383208520148, 155.7539078627980018 ) ) ;
#36820 = CARTESIAN_POINT ( 'NONE',  ( -15.46960593179999854, 1495.922518723830080, 224.3507688835979934 ) ) ;
#36821 = CARTESIAN_POINT ( 'NONE',  ( 4.328991615394299330, 1515.082251143320036, 210.4834250158149871 ) ) ;
#36822 = CARTESIAN_POINT ( 'NONE',  ( -11.51310730920000047, 1420.345402828329952, 230.4603701114980083 ) ) ;
#36823 = AXIS2_PLACEMENT_3D ( 'NONE', #49419, #9050, #77372 ) ;
#36824 = CARTESIAN_POINT ( 'NONE',  ( -6.802668042220000544, 1459.333277144890189, 216.9857242932490067 ) ) ;
#36825 = CARTESIAN_POINT ( 'NONE',  ( 9.643569501056903803, 1360.898780757513578, 209.6218459617033432 ) ) ;
#36826 = CARTESIAN_POINT ( 'NONE',  ( -45.62046377349849990, 1437.139006798159926, 266.4203617035300340 ) ) ;
#36827 = CARTESIAN_POINT ( 'NONE',  ( -2.500000000000000000, 1436.878463555260169, 183.6520988947980015 ) ) ;
#36828 = ORIENTED_EDGE ( 'NONE', *, *, #85737, .T. ) ;
#36829 = CARTESIAN_POINT ( 'NONE',  ( 24.88936805819999876, 1435.366663778739849, 135.7839653261980004 ) ) ;
#36830 = ORIENTED_EDGE ( 'NONE', *, *, #70186, .F. ) ;
#36831 = CARTESIAN_POINT ( 'NONE',  ( -7.332063977575000280, 1516.939491476980038, 209.1325772641960157 ) ) ;
#36832 = CARTESIAN_POINT ( 'NONE',  ( -5.898813458170000246, 1474.065724237490031, 199.2881457417290108 ) ) ;
#36833 = CARTESIAN_POINT ( 'NONE',  ( -3.313501335607589748, 1397.551704408390151, 203.0565224509919915 ) ) ;
#36834 = CARTESIAN_POINT ( 'NONE',  ( -12.73441983819999912, 1425.415068379630156, 188.8640771564980128 ) ) ;
#36835 = CARTESIAN_POINT ( 'NONE',  ( -27.02393216510709806, 1451.035700111990081, 136.3598584798200193 ) ) ;
#36836 = ORIENTED_EDGE ( 'NONE', *, *, #92004, .T. ) ;
#36837 = CARTESIAN_POINT ( 'NONE',  ( 3.775314256393730084, 1507.374707593759922, 220.2027404254530154 ) ) ;
#36838 = CARTESIAN_POINT ( 'NONE',  ( 3.827327205999999205, 1409.546157813759464, 137.0999999980979851 ) ) ;
#36839 = CARTESIAN_POINT ( 'NONE',  ( -18.51989805858369920, 1508.551704408389924, 210.2057868587989731 ) ) ;
#36840 = DIRECTION ( 'NONE',  ( 0.7074300732573280959, 0.02470400251971145017, -0.7063514732133270302 ) ) ;
#36841 = CARTESIAN_POINT ( 'NONE',  ( -9.510122433503239492, 1439.432175621480155, 208.1922871124760093 ) ) ;
#36842 = ORIENTED_EDGE ( 'NONE', *, *, #51525, .T. ) ;
#36843 = CARTESIAN_POINT ( 'NONE',  ( -26.80401541404379984, 1414.781986674270001, 270.2830222979230257 ) ) ;
#36844 = CARTESIAN_POINT ( 'NONE',  ( 7.713648834184999359, 1516.710624944440042, 208.3691743819339877 ) ) ;
#36845 = CARTESIAN_POINT ( 'NONE',  ( -0.7625704858929999164, 1427.674934138829940, 112.4493539157979995 ) ) ;
#36846 = CARTESIAN_POINT ( 'NONE',  ( 17.68237282055029880, 1517.051704408389924, 212.5589510568480023 ) ) ;
#36848 = ORIENTED_EDGE ( 'NONE', *, *, #48798, .T. ) ;
#36847 = CARTESIAN_POINT ( 'NONE',  ( -7.004779464842641801, 1367.034864359649873, 207.6218459616988241 ) ) ;
#36849 = EDGE_LOOP ( 'NONE', ( #95781, #76655, #74366, #33588 ) ) ;
#36850 = CARTESIAN_POINT ( 'NONE',  ( 45.07050412730048805, 1446.292603878223190, 268.9905583915053171 ) ) ;
#36851 = CARTESIAN_POINT ( 'NONE',  ( 2.324366880823700132, 1466.792378440680068, 219.9346284353489978 ) ) ;
#36852 = CARTESIAN_POINT ( 'NONE',  ( 3.657938333797013719, 1424.289973031273348, 184.1667673033518895 ) ) ;
#36853 = DIRECTION ( 'NONE',  ( 0.000000000000000000, 0.000000000000000000, -1.000000000000000000 ) ) ;
#36854 = CARTESIAN_POINT ( 'NONE',  ( -18.70785252105190111, 1416.073666489629886, 207.5722946701860110 ) ) ;
#36855 = CARTESIAN_POINT ( 'NONE',  ( -19.46569100160000332, 1425.812900638729843, 223.4663329973979842 ) ) ;
#36856 = AXIS2_PLACEMENT_3D ( 'NONE', #1198, #9568, #26937 ) ;
#36857 = CARTESIAN_POINT ( 'NONE',  ( 5.332756758680099907, 1475.983341725180026, 267.2347467959210121 ) ) ;
#36858 = CARTESIAN_POINT ( 'NONE',  ( -11.62269725585159996, 1391.913060387140149, 208.4322474913049916 ) ) ;
#36859 = CARTESIAN_POINT ( 'NONE',  ( 5.766269470360000149, 1446.073093314650123, 183.5047901106979964 ) ) ;
#36860 = CARTESIAN_POINT ( 'NONE',  ( 6.933879402874999265, 1516.560253536979872, 206.6353711893569880 ) ) ;
#36861 = ORIENTED_EDGE ( 'NONE', *, *, #46016, .T. ) ;
#36862 = CARTESIAN_POINT ( 'NONE',  ( -14.26333330936780008, 1452.396687514240057, 223.0069981058830137 ) ) ;
#36863 = CARTESIAN_POINT ( 'NONE',  ( 1.484957073209509870, 1474.597282977839996, 182.5315330437460091 ) ) ;
#36864 = ORIENTED_EDGE ( 'NONE', *, *, #62570, .F. ) ;
#36865 = CARTESIAN_POINT ( 'NONE',  ( 3.116127822634939815, 1509.034536885679927, 204.6344861955039960 ) ) ;
#36866 = CARTESIAN_POINT ( 'NONE',  ( 25.56660996036589850, 1451.956732796869801, 135.7427434114759990 ) ) ;
#36867 = CARTESIAN_POINT ( 'NONE',  ( -13.10606021074817207, 1519.551704408389924, 192.4222450282478292 ) ) ;
#36868 = CARTESIAN_POINT ( 'NONE',  ( -23.42580017550000093, 1388.535583196000061, 220.7761725842590010 ) ) ;
#36869 = LINE ( 'NONE', #87278, #43140 ) ;
#36870 = CARTESIAN_POINT ( 'NONE',  ( 17.84430285039999831, 1410.460570803829796, 193.2432472200979987 ) ) ;
#36871 = DIRECTION ( 'NONE',  ( 0.000000000000000000, 1.000000000000000000, 0.000000000000000000 ) ) ;
#36872 = CARTESIAN_POINT ( 'NONE',  ( 16.63042445450000173, 1409.493807611130023, 225.0072295868980063 ) ) ;
#36873 = CARTESIAN_POINT ( 'NONE',  ( -19.40238068805140870, 1425.501152276447101, 223.5497471931373923 ) ) ;
#36874 = CARTESIAN_POINT ( 'NONE',  ( 0.8680289119235070627, 1450.932674612510027, 182.0391449964180310 ) ) ;
#36875 = CARTESIAN_POINT ( 'NONE',  ( 27.68253994085160130, 1507.989615297080036, 207.6661388942010262 ) ) ;
#36876 = CARTESIAN_POINT ( 'NONE',  ( -7.713117841115000317, 1516.690345681169902, 214.1262880092169780 ) ) ;
#36877 = CARTESIAN_POINT ( 'NONE',  ( 26.20934030730460407, 1446.264570522150279, 137.9472260036899911 ) ) ;
#36878 = VERTEX_POINT ( 'NONE', #29748 ) ;
#36879 = CARTESIAN_POINT ( 'NONE',  ( -17.01462653269999947, 1417.417567022180037, 207.6637925360890051 ) ) ;
#36880 = CARTESIAN_POINT ( 'NONE',  ( 22.03465957474240255, 1522.644714754858114, 235.4136513321555810 ) ) ;
#36881 = CARTESIAN_POINT ( 'NONE',  ( -7.637723194635209545, 1484.320820859400101, 199.9856414351459932 ) ) ;
#36882 = CIRCLE ( 'NONE', #83384, 2.000000000000003553 ) ;
#36883 = EDGE_CURVE ( 'NONE', #96481, #660, #33340, .T. ) ;
#36884 = CARTESIAN_POINT ( 'NONE',  ( 11040.89558201060572, 2833.596074015790236, -8386.665009981872572 ) ) ;
#36885 = CARTESIAN_POINT ( 'NONE',  ( -39.03741743653520047, 1447.683443756730185, 136.5404196528269836 ) ) ;
#36886 = CARTESIAN_POINT ( 'NONE',  ( -3.968827103576990201, 1519.551704408389924, 229.5396913781519856 ) ) ;
#36887 = CARTESIAN_POINT ( 'NONE',  ( -21.34957048430000270, 1448.971257407479925, 234.3916895749979687 ) ) ;
#36888 = CARTESIAN_POINT ( 'NONE',  ( -22.52609268272879817, 1509.699688877640028, 190.9355248210520131 ) ) ;
#36889 = CARTESIAN_POINT ( 'NONE',  ( 11.86794208260000083, 1433.007090817639892, 150.2053038657979869 ) ) ;
#36890 = EDGE_CURVE ( 'NONE', #98602, #36878, #31958, .T. ) ;
#36891 = CARTESIAN_POINT ( 'NONE',  ( -45.63734427819910167, 1440.913053513229897, 268.9745364329980362 ) ) ;
#36892 = CARTESIAN_POINT ( 'NONE',  ( 24.79030299087470013, 1440.913060396060018, 214.6803157916720295 ) ) ;
#36893 = CARTESIAN_POINT ( 'NONE',  ( -109.7179997069999899, 1385.165587680520048, 297.0932178332590183 ) ) ;
#36894 = CARTESIAN_POINT ( 'NONE',  ( 13.16547634019999968, 1429.085800465429884, 222.6599709325980143 ) ) ;
#36895 = VERTEX_POINT ( 'NONE', #5666 ) ;
#36896 = CARTESIAN_POINT ( 'NONE',  ( -34.18677586421193837, 1524.726013923371283, 198.4504086008750505 ) ) ;
#36897 = CARTESIAN_POINT ( 'NONE',  ( 9.576461961311400373, 1463.549209214470011, 211.2185630534640097 ) ) ;
#36898 = CARTESIAN_POINT ( 'NONE',  ( -3.527569048100000160, 1486.518325592330029, 181.8541486797979871 ) ) ;
#36899 = CARTESIAN_POINT ( 'NONE',  ( -7.512705432752817991, 1509.036904581754015, 203.3466808530631909 ) ) ;
#36900 = CARTESIAN_POINT ( 'NONE',  ( -19.06177932457689295, 1488.336581673826686, 199.7544505207700070 ) ) ;
#36901 = CARTESIAN_POINT ( 'NONE',  ( 24.66781776970000095, 1430.359786436929880, 210.6510114860680289 ) ) ;
#36902 = DIRECTION ( 'NONE',  ( 1.000000000000000000, 0.000000000000000000, 0.000000000000000000 ) ) ;
#36903 = CARTESIAN_POINT ( 'NONE',  ( -16.93884357239999972, 1507.634939734329919, 230.1482611379979915 ) ) ;
#36904 = CARTESIAN_POINT ( 'NONE',  ( -22.97691509383379938, 1383.850362194360059, 222.2151806931460385 ) ) ;
#36905 = FACE_OUTER_BOUND ( 'NONE', #62660, .T. ) ;
#36906 = CARTESIAN_POINT ( 'NONE',  ( 5.764290840147539896, 1423.363971970169814, 93.10623776433179444 ) ) ;
#36907 = DIRECTION ( 'NONE',  ( -1.755985294532469921E-16, 1.000000000000000000, -1.338183447452831989E-16 ) ) ;
#36908 = CARTESIAN_POINT ( 'NONE',  ( 8.781724162916820120, 1451.721506209049949, 212.1163246891099732 ) ) ;
#36910 = VERTEX_POINT ( 'NONE', #46583 ) ;
#36909 = DIRECTION ( 'NONE',  ( 1.000000000000000000, 0.000000000000000000, 0.000000000000000000 ) ) ;
#36911 = CARTESIAN_POINT ( 'NONE',  ( -0.9042085446950000049, 1416.833018185029914, 228.0293392571980178 ) ) ;
#36912 = B_SPLINE_CURVE_WITH_KNOTS ( 'NONE', 3,
 ( #32062, #100895, #24192, #57301, #6311, #67343, #74085, #40457, #84110, #32620, #57837, #6847, #108214, #66795, #58379, #75731, #91427, #109875, #50532, #33154, #58928, #93059, #16333, #42123, #31502, #110420, #67894, #102001, #65682, #59488, #93598, #17996, #17429, #18544 ),
 .UNSPECIFIED., .F., .F.,
 ( 4, 3, 3, 3, 3, 3, 3, 3, 3, 3, 3, 4 ),
 ( -2.000000000000000000, -1.872502022310899905, -1.688267240139549985, -1.501795031034689920, -1.314134592350729935, -1.125010883417350005, -0.9354619354659259312, -0.7459537259483131066, -0.5569474984532378770, -0.3696240495077129928, -0.1838865046504070122, 0.000000000000000000 ),
 .UNSPECIFIED. ) ;
#36913 = CARTESIAN_POINT ( 'NONE',  ( -8.350980490578317372, 1386.945100721060726, 199.8923438227050724 ) ) ;
#36914 = CARTESIAN_POINT ( 'NONE',  ( -20.13638283970000131, 1507.886205248129954, 189.0953426691980042 ) ) ;
#36916 = ORIENTED_EDGE ( 'NONE', *, *, #2284, .F. ) ;
#36915 = CARTESIAN_POINT ( 'NONE',  ( -38.54572101790750338, 1450.058425145499996, 134.0999999982749955 ) ) ;
#36917 = CARTESIAN_POINT ( 'NONE',  ( 18.28862841063420319, 1430.119204692329959, 201.0315373977480249 ) ) ;
#36918 = ORIENTED_EDGE ( 'NONE', *, *, #110319, .T. ) ;
#36919 = CARTESIAN_POINT ( 'NONE',  ( -11.37528348128880040, 1389.803332359200112, 215.0420196902499868 ) ) ;
#36920 = CARTESIAN_POINT ( 'NONE',  ( 33.28034951413924603, 1501.977400791986611, 200.8029765415137433 ) ) ;
#36921 = CARTESIAN_POINT ( 'NONE',  ( -2.866593677795437056, 1368.013634267723319, 210.0441101397873922 ) ) ;
#36922 = CYLINDRICAL_SURFACE ( 'NONE', #89345, 1.999999999999999556 ) ;
#36923 = CARTESIAN_POINT ( 'NONE',  ( -12.31314964446622362, 1377.826519118230408, 208.9131911094586940 ) ) ;
#36924 = CARTESIAN_POINT ( 'NONE',  ( 13.76570265589420039, 1409.393769314739984, 214.9243204603270101 ) ) ;
#36925 = CARTESIAN_POINT ( 'NONE',  ( 4.044941532578454790, 1419.921549897504519, 137.0999999980980135 ) ) ;
#36926 = CARTESIAN_POINT ( 'NONE',  ( -93.07006015126680154, 1385.202033573790004, 294.1823754421509989 ) ) ;
#36927 = CARTESIAN_POINT ( 'NONE',  ( -10.08173109987140137, 1391.913060387289988, 214.3435508543619790 ) ) ;
#36928 = CARTESIAN_POINT ( 'NONE',  ( -40.26396455803409680, 1444.186530478750001, 137.1012301494149881 ) ) ;
#36929 = CARTESIAN_POINT ( 'NONE',  ( 10.97962301462450085, 1490.622470617079898, 207.3477770736940045 ) ) ;
#36931 = EDGE_LOOP ( 'NONE', ( #98561, #102843, #59595, #96669 ) ) ;
#36930 = DIRECTION ( 'NONE',  ( 1.000000000000000000, 0.000000000000000000, 0.000000000000000000 ) ) ;
#36932 = ORIENTED_EDGE ( 'NONE', *, *, #21299, .F. ) ;
#36933 = CARTESIAN_POINT ( 'NONE',  ( -18.73498386431730012, 1442.071135603129960, 209.6995629687959877 ) ) ;
#36934 = CARTESIAN_POINT ( 'NONE',  ( 2.391961498639229688, 1497.094853944359784, 196.9517835458970012 ) ) ;
#36935 = CARTESIAN_POINT ( 'NONE',  ( 29.70209480455160289, 1509.984357653646612, 210.2261402311804659 ) ) ;
#36936 = CARTESIAN_POINT ( 'NONE',  ( 11.84247987984260142, 1427.444780555890020, 208.6785203155049828 ) ) ;
#36937 = CARTESIAN_POINT ( 'NONE',  ( 1.250005296159999890, 1397.324124807030103, 222.0664063312979692 ) ) ;
#36938 = CARTESIAN_POINT ( 'NONE',  ( 31.54873523816509362, 1525.317349363550193, 201.5741525441649742 ) ) ;
#36939 = CARTESIAN_POINT ( 'NONE',  ( 3.279726742559999852, 1445.963864114290118, 200.3213863680089730 ) ) ;
#36940 = CARTESIAN_POINT ( 'NONE',  ( -0.5154891906340001162, 1455.056769859629867, 183.1589657396980044 ) ) ;
#36941 = CARTESIAN_POINT ( 'NONE',  ( -10.26707792444094736, 1367.299349508571595, 210.6218459617030021 ) ) ;
#36942 = DIRECTION ( 'NONE',  ( -0.6709778558543776361, 0.000000000000000000, -0.7414773880254624805 ) ) ;
#36943 = CARTESIAN_POINT ( 'NONE',  ( -2.881222795715000284, 1516.891731298979948, 206.6444723262370076 ) ) ;
#36944 = CARTESIAN_POINT ( 'NONE',  ( -13.02075094452810156, 1434.790641786380093, 149.2531060708759867 ) ) ;
#36945 = DIRECTION ( 'NONE',  ( 1.000000000000000000, 1.810374147724000060E-32, 1.224646799147351975E-16 ) ) ;
#36946 = CARTESIAN_POINT ( 'NONE',  ( 2.475018574370000390, 1497.111080388990104, 196.9667223758990247 ) ) ;
#36947 = CARTESIAN_POINT ( 'NONE',  ( -20.11389898556769751, 1487.601351896439837, 204.1067778117269995 ) ) ;
#36948 = AXIS2_PLACEMENT_3D ( 'NONE', #74013, #14637, #56660 ) ;
#36949 = CARTESIAN_POINT ( 'NONE',  ( 41.07185139426759690, 1444.167090557440133, 136.8192919370380025 ) ) ;
#36950 = ORIENTED_EDGE ( 'NONE', *, *, #105003, .T. ) ;
#36951 = CARTESIAN_POINT ( 'NONE',  ( 6.814834853189999819, 1407.100401533429931, 264.8986986396980114 ) ) ;
#36952 = ADVANCED_FACE ( 'NONE', ( #38154 ), #57150, .T. ) ;
#36953 = CARTESIAN_POINT ( 'NONE',  ( -26.41621169419999759, 1469.246811866430107, 207.9181783895880073 ) ) ;
#36955 = FACE_OUTER_BOUND ( 'NONE', #20303, .T. ) ;
#36954 = CARTESIAN_POINT ( 'NONE',  ( -10.65149325124349922, 1425.724702697329803, 91.14980580301869395 ) ) ;
#36956 = EDGE_CURVE ( 'NONE', #97580, #23634, #97533, .T. ) ;
#36957 = CARTESIAN_POINT ( 'NONE',  ( 0.7576635334400020350, 1516.855632454399938, 211.9899581013969794 ) ) ;
#36958 =( BOUNDED_CURVE ( )  B_SPLINE_CURVE ( 3, ( #8863, #44152, #25107, #8315 ),
 .UNSPECIFIED., .F., .F. ) 
 B_SPLINE_CURVE_WITH_KNOTS ( ( 4, 4 ),
 ( 5.766256096902659500, 6.404609662640440071 ),
 .UNSPECIFIED. ) 
 CURVE ( )  GEOMETRIC_REPRESENTATION_ITEM ( )  RATIONAL_B_SPLINE_CURVE ( ( 1.000000000000000000, 0.9663293686618639189, 0.9663293686618639189, 1.000000000000000000 ) ) 
 REPRESENTATION_ITEM ( '' )  );
#36959 = CARTESIAN_POINT ( 'NONE',  ( -4.026786250540000722, 1408.413060387330006, 137.0999999980979851 ) ) ;
#36960 = CARTESIAN_POINT ( 'NONE',  ( -15.89627787769999934, 1415.668893196430190, 250.4785789484980114 ) ) ;
#36961 = CARTESIAN_POINT ( 'NONE',  ( 20.30091062346680175, 1509.661473013709838, 230.8308773693809997 ) ) ;
#36962 = EDGE_CURVE ( 'NONE', #76097, #60628, #84956, .T. ) ;
#36963 = CARTESIAN_POINT ( 'NONE',  ( -26.31479228349999744, 1435.423696365460046, 135.4819446036979684 ) ) ;
#36964 = ADVANCED_FACE ( 'NONE', ( #82909 ), #85106, .T. ) ;
#36965 = CARTESIAN_POINT ( 'NONE',  ( 2.738648607395533841, 1448.013770983326594, 154.7581944341845599 ) ) ;
#36966 = DIRECTION ( 'NONE',  ( -9.992007221626410836E-16, -0.7071067811865470176, -0.7071067811865480168 ) ) ;
#36967 = EDGE_LOOP ( 'NONE', ( #85440, #107074 ) ) ;
#36968 = LINE ( 'NONE', #12311, #30358 ) ;
#36969 = FACE_OUTER_BOUND ( 'NONE', #12314, .T. ) ;
#36970 = DIRECTION ( 'NONE',  ( 0.4794255386042031719, 0.000000000000000000, 0.8775825618903726477 ) ) ;
#36971 = ORIENTED_EDGE ( 'NONE', *, *, #43571, .F. ) ;
#36972 = VERTEX_POINT ( 'NONE', #108664 ) ;
#36973 = CARTESIAN_POINT ( 'NONE',  ( 9.993125864493370258, 1452.958822306690081, 210.9634216041149841 ) ) ;
#36974 = CARTESIAN_POINT ( 'NONE',  ( 4.993613116619998848, 1423.332947890779906, 194.3851836586989918 ) ) ;
#36975 = ORIENTED_EDGE ( 'NONE', *, *, #100788, .T. ) ;
#36976 = CARTESIAN_POINT ( 'NONE',  ( -0.2621966296400000118, 1421.807807218729977, 227.6850737390979873 ) ) ;
#36977 = DIRECTION ( 'NONE',  ( -1.755985294532469921E-16, 1.000000000000000000, -1.338183447452831989E-16 ) ) ;
#36978 = CARTESIAN_POINT ( 'NONE',  ( -2.854534533760000325, 1489.061586880230152, 236.0493179470980181 ) ) ;
#36979 = CARTESIAN_POINT ( 'NONE',  ( 7.266079630789520571, 1509.032014039220030, 202.3522229272149957 ) ) ;
#36980 = EDGE_LOOP ( 'NONE', ( #95214, #78557, #106595, #54488 ) ) ;
#36981 = CARTESIAN_POINT ( 'NONE',  ( 45.85445186496249903, 1440.912968281529857, 268.7564834733289558 ) ) ;
#36982 = DIRECTION ( 'NONE',  ( -2.220446049250000002E-16, -1.000000000000000000, 2.220446049250000002E-16 ) ) ;
#36983 = ADVANCED_FACE ( 'NONE', ( #75635 ), #58242, .F. ) ;
#36984 = CARTESIAN_POINT ( 'NONE',  ( 13.89849120039999875, 1452.828749846529945, 224.0454814765980132 ) ) ;
#36985 = ORIENTED_EDGE ( 'NONE', *, *, #91975, .T. ) ;
#36986 = CARTESIAN_POINT ( 'NONE',  ( 3.449777315724999571, 1516.974592746400049, 204.1104779853070283 ) ) ;
#36987 = ORIENTED_EDGE ( 'NONE', *, *, #13146, .T. ) ;
#36988 = CARTESIAN_POINT ( 'NONE',  ( 11.86362456902309859, 1432.162991587550096, 149.9796059917460127 ) ) ;
#36989 = CARTESIAN_POINT ( 'NONE',  ( 13.40902307454580722, 1444.400031499317947, 187.7555987698363538 ) ) ;
#36990 = ORIENTED_EDGE ( 'NONE', *, *, #54917, .T. ) ;
#36991 = ORIENTED_EDGE ( 'NONE', *, *, #13717, .F. ) ;
#36992 = CARTESIAN_POINT ( 'NONE',  ( 5.851689954866730048, 1422.502855755774817, 139.1417834163787575 ) ) ;
#36993 = CARTESIAN_POINT ( 'NONE',  ( -13.51702042466202158, 1443.501467202830327, 169.3754641244113373 ) ) ;
#36994 = CARTESIAN_POINT ( 'NONE',  ( -2.823657736881381997, 1367.710836537829891, 208.5987421069861796 ) ) ;
#36995 = AXIS2_PLACEMENT_3D ( 'NONE', #75726, #100365, #7950 ) ;
#36996 = EDGE_CURVE ( 'NONE', #47062, #98891, #45691, .T. ) ;
#36997 = CARTESIAN_POINT ( 'NONE',  ( -9.702159690257650126, 1471.556315755829928, 212.0784607202180041 ) ) ;
#36998 = CARTESIAN_POINT ( 'NONE',  ( 16.34988667148460095, 1452.342109763679900, 146.8430469853310001 ) ) ;
#36999 = CARTESIAN_POINT ( 'NONE',  ( 3.068142017777439889, 1410.113784448680008, 269.8661674101820154 ) ) ;
#37000 = CARTESIAN_POINT ( 'NONE',  ( -109.1645132478509908, 1384.901512804259937, 297.1326343494729940 ) ) ;
#37001 = CARTESIAN_POINT ( 'NONE',  ( -12.74742477238099880, 1502.424001303030082, 209.9689629893190101 ) ) ;
#37002 = CARTESIAN_POINT ( 'NONE',  ( 10.81377540340000110, 1493.463431426289844, 215.2021047779490175 ) ) ;
#37003 = CARTESIAN_POINT ( 'NONE',  ( 0.000000000000000000, 1523.409940573003951, 209.1218459616979999 ) ) ;
#37004 = CARTESIAN_POINT ( 'NONE',  ( 8.507717558044577189, 1424.620342978096460, 195.7232110867650192 ) ) ;
#37006 = DIRECTION ( 'NONE',  ( 1.000000000000000000, 0.000000000000000000, 0.000000000000000000 ) ) ;
#37005 = CARTESIAN_POINT ( 'NONE',  ( -17.70257496129999808, 1504.298185088789978, 209.2114294917570021 ) ) ;
#37007 = CYLINDRICAL_SURFACE ( 'NONE', #86198, 1.999999999999999556 ) ;
#37008 = CARTESIAN_POINT ( 'NONE',  ( -9.965372901819408824, 1439.491959218489910, 208.4032164217179854 ) ) ;
#37009 = CARTESIAN_POINT ( 'NONE',  ( -8.118882966355000619, 1514.642928591840018, 202.5872254880569869 ) ) ;
#37010 = ORIENTED_EDGE ( 'NONE', *, *, #11224, .F. ) ;
#37011 = CARTESIAN_POINT ( 'NONE',  ( 37.18025143530000065, 1432.092747987069970, 265.6112251771979800 ) ) ;
#37012 = CARTESIAN_POINT ( 'NONE',  ( 13.42933457559999866, 1434.933251406229829, 148.8497112766980308 ) ) ;
#37013 = CIRCLE ( 'NONE', #94229, 2.000000000000001776 ) ;
#37014 = CARTESIAN_POINT ( 'NONE',  ( -75.37352950217560021, 1385.006855903410042, 300.3767631137689591 ) ) ;
#37015 = CARTESIAN_POINT ( 'NONE',  ( -17.43739734485818005, 1526.178928173327449, 180.7274168163475281 ) ) ;
#37016 = CARTESIAN_POINT ( 'NONE',  ( 5.466273243599998999, 1504.965088730989919, 220.6538119101990105 ) ) ;
#37017 = CARTESIAN_POINT ( 'NONE',  ( -15.51438564200000059, 1415.734451527310057, 210.2992275438789989 ) ) ;
#37019 = ORIENTED_EDGE ( 'NONE', *, *, #101435, .T. ) ;
#37018 = CARTESIAN_POINT ( 'NONE',  ( 12.60620919525579886, 1421.114752853880191, 203.4337117396169958 ) ) ;
#37020 = CARTESIAN_POINT ( 'NONE',  ( -15.61900273229925418, 1415.705855514175028, 209.6365545205262890 ) ) ;
#37021 = CARTESIAN_POINT ( 'NONE',  ( -9.803834995107230554, 1522.051704408389924, 196.6215198571080123 ) ) ;
#37022 = CARTESIAN_POINT ( 'NONE',  ( -11.73653109249999993, 1426.280329148629789, 144.1709412064980143 ) ) ;
#37023 = CARTESIAN_POINT ( 'NONE',  ( 4.124127541549999165, 1440.791920158089852, 218.1322488136489994 ) ) ;
#37024 = ADVANCED_FACE ( 'NONE', ( #100269 ), #13496, .F. ) ;
#37025 = CARTESIAN_POINT ( 'NONE',  ( 18.14165090985069995, 1415.439546991589850, 223.1321341251090189 ) ) ;
#37026 = CARTESIAN_POINT ( 'NONE',  ( 5.361911014951845189, 1422.281284793781651, 142.4622902538874314 ) ) ;
#37027 = CARTESIAN_POINT ( 'NONE',  ( 27.47350474782500385, 1509.872456313999919, 194.7471083429309999 ) ) ;
#37028 = DIRECTION ( 'NONE',  ( 0.000000000000000000, -1.000000000000000000, -0.000000000000000000 ) ) ;
#37029 = CARTESIAN_POINT ( 'NONE',  ( -8.010413950200000244, 1453.313060387329870, 227.4940039322979999 ) ) ;
#37030 = CARTESIAN_POINT ( 'NONE',  ( 15.15971965770000018, 1415.085700719130045, 227.6136599590979870 ) ) ;
#37031 = CARTESIAN_POINT ( 'NONE',  ( -4.648405679570000615, 1475.312747251090059, 218.3805770009889784 ) ) ;
#37032 = CARTESIAN_POINT ( 'NONE',  ( -16.32411324169200029, 1459.451818037003932, 228.9510944607559964 ) ) ;
#37033 = CARTESIAN_POINT ( 'NONE',  ( 7.708745647785000266, 1516.523379810429788, 207.4137536659370085 ) ) ;
#37034 = CARTESIAN_POINT ( 'NONE',  ( 39.46828811559999650, 1422.426797802230112, 268.4272099870980242 ) ) ;
#37035 = CARTESIAN_POINT ( 'NONE',  ( -19.24864600659999780, 1410.507820697930129, 222.4474005179980054 ) ) ;
#37036 = AXIS2_PLACEMENT_3D ( 'NONE', #37561, #64436, #38105 ) ;
#37037 = CARTESIAN_POINT ( 'NONE',  ( 21.27861338680000003, 1436.471609301180024, 144.0072822869979916 ) ) ;
#37038 = CARTESIAN_POINT ( 'NONE',  ( 21.90978594049999728, 1508.011557042930008, 191.9201679438979795 ) ) ;
#37039 = CARTESIAN_POINT ( 'NONE',  ( -16.17519662274699854, 1409.477882727519955, 192.6004389500859872 ) ) ;
#37040 = DIRECTION ( 'NONE',  ( 0.5877852522924831291, 0.000000000000000000, 0.8090169943749401238 ) ) ;
#37041 = CARTESIAN_POINT ( 'NONE',  ( -0.2153814148640000037, 1475.836819236129941, 266.9611412552980028 ) ) ;
#37042 = CARTESIAN_POINT ( 'NONE',  ( 17.83486663330506872, 1523.678648413191695, 237.8759530894958800 ) ) ;
#37043 = CARTESIAN_POINT ( 'NONE',  ( -33.91367881351369817, 1435.681798209460112, 135.0664091405390081 ) ) ;
#37044 = CARTESIAN_POINT ( 'NONE',  ( -7.626416753354130051, 1407.838202350920028, 198.4036846208539941 ) ) ;
#37045 = CARTESIAN_POINT ( 'NONE',  ( -18.20160569639999792, 1416.825421875629900, 205.1678409615580279 ) ) ;
#37046 = CARTESIAN_POINT ( 'NONE',  ( -17.60061311809051077, 1410.712255857376476, 193.4350317014313134 ) ) ;
#37047 = CARTESIAN_POINT ( 'NONE',  ( -27.88619979645839919, 1508.695391729820130, 210.5767662318619955 ) ) ;
#37048 = CARTESIAN_POINT ( 'NONE',  ( 3.727273714354999878, 1456.064331771540083, 219.0685001699370105 ) ) ;
#37049 = CARTESIAN_POINT ( 'NONE',  ( -33.92723094509999981, 1436.576986543820112, 136.5095885516980161 ) ) ;
#37050 = CARTESIAN_POINT ( 'NONE',  ( -8.145248142631778876, 1456.245062998393223, 227.2183179010753236 ) ) ;
#37051 = ORIENTED_EDGE ( 'NONE', *, *, #91784, .T. ) ;
#37052 = CARTESIAN_POINT ( 'NONE',  ( -2.698112829555000314, 1512.326491219019999, 201.4303292780870152 ) ) ;
#37053 = CARTESIAN_POINT ( 'NONE',  ( -0.3017417235444129764, 1408.923597440540107, 224.1202794661850248 ) ) ;
#37054 = CARTESIAN_POINT ( 'NONE',  ( 31.76119286153732091, 1522.906363951597314, 196.2959455099801573 ) ) ;
#37055 = VERTEX_POINT ( 'NONE', #101895 ) ;
#37056 = EDGE_CURVE ( 'NONE', #2813, #27462, #22356, .T. ) ;
#37057 = CARTESIAN_POINT ( 'NONE',  ( 17.05938516367379876, 1517.051704408300111, 223.0487112149370148 ) ) ;
#37058 = CARTESIAN_POINT ( 'NONE',  ( -33.43582158959214468, 1442.831169986189025, 154.5919879262729921 ) ) ;
#37059 = VECTOR ( 'NONE', #21710, 1000.000000000000114 ) ;
#37060 = CARTESIAN_POINT ( 'NONE',  ( -37.84955692739999478, 1461.864452344229903, 267.2558694692979770 ) ) ;
#37061 = CARTESIAN_POINT ( 'NONE',  ( -29.86461515634930564, 1525.960063244516959, 197.2746849027939504 ) ) ;
#37062 = CARTESIAN_POINT ( 'NONE',  ( -4.500000000000000000, 1448.210448412289907, 183.1418046154980175 ) ) ;
#37063 = EDGE_CURVE ( 'NONE', #98048, #43851, #83451, .T. ) ;
#37064 = CARTESIAN_POINT ( 'NONE',  ( 19.38211899476526767, 1526.344110814219221, 232.9251177427934181 ) ) ;
#37065 = DIRECTION ( 'NONE',  ( 0.000000000000000000, -1.000000000000000000, 0.000000000000000000 ) ) ;
#37066 = CARTESIAN_POINT ( 'NONE',  ( -38.18457335657470963, 1384.985636250929929, 211.2360860694770111 ) ) ;
#37067 = CARTESIAN_POINT ( 'NONE',  ( -5.013264356663312604, 1375.410824559817684, 214.7179447577057658 ) ) ;
#37068 = CARTESIAN_POINT ( 'NONE',  ( 17.25136325379999747, 1416.823872462129884, 215.4099459140879844 ) ) ;
#37069 = CARTESIAN_POINT ( 'NONE',  ( -28.25550469189699854, 1508.223393722109904, 208.8542599017760040 ) ) ;
#37070 = CARTESIAN_POINT ( 'NONE',  ( -26.96762182225300108, 1508.002311694569926, 211.4841061306140375 ) ) ;
#37071 = CYLINDRICAL_SURFACE ( 'NONE', #25091, 2.000000000000003109 ) ;
#37072 = CARTESIAN_POINT ( 'NONE',  ( -8.371372866679999802, 1384.925069025969833, 199.7749685622990228 ) ) ;
#37073 = DIRECTION ( 'NONE',  ( 5.980589973904019347E-17, -1.000000000000000000, 1.736889445713099699E-16 ) ) ;
#37074 = DIRECTION ( 'NONE',  ( -1.000000000000000000, -0.000000000000000000, -0.000000000000000000 ) ) ;
#37075 = CARTESIAN_POINT ( 'NONE',  ( -11.37414570439999828, 1415.063410501330054, 195.5459300842980213 ) ) ;
#37076 = CARTESIAN_POINT ( 'NONE',  ( 0.5871476172820019324, 1421.209716202029767, 193.6933393547989795 ) ) ;
#37077 = CARTESIAN_POINT ( 'NONE',  ( 23.66327964099999903, 1411.099855206130087, 211.3154122771679795 ) ) ;
#37078 = CARTESIAN_POINT ( 'NONE',  ( -106.5387865765160029, 1391.913060387289988, 305.3438590551860443 ) ) ;
#37079 = CARTESIAN_POINT ( 'NONE',  ( -9.724670062538070425, 1448.677161661070159, 190.8206614882809902 ) ) ;
#37080 = CARTESIAN_POINT ( 'NONE',  ( -16.11028175070000046, 1421.340732576330083, 227.0764403262979840 ) ) ;
#37082 = CARTESIAN_POINT ( 'NONE',  ( -11.59475506509999931, 1379.773093697659988, 204.2227873110190046 ) ) ;
#37081 = DIRECTION ( 'NONE',  ( -0.4794255386042018952, 0.000000000000000000, 0.8775825618903733139 ) ) ;
#37083 = CARTESIAN_POINT ( 'NONE',  ( 0.3077026392289999857, 1413.018417486829776, 233.3704243096979951 ) ) ;
#37084 = DIRECTION ( 'NONE',  ( -0.6742693640212139572, -4.521919481779819710E-17, -0.7384854939282339270 ) ) ;
#37085 = FACE_OUTER_BOUND ( 'NONE', #46932, .T. ) ;
#37086 = CARTESIAN_POINT ( 'NONE',  ( -22.79695488910000378, 1415.997925189830084, 211.7898339411780171 ) ) ;
#37087 = VECTOR ( 'NONE', #32631, 1000.000000000000000 ) ;
#37088 = CARTESIAN_POINT ( 'NONE',  ( -1.368198998969730074, 1419.344532540260161, 185.2221260820999760 ) ) ;
#37089 = CARTESIAN_POINT ( 'NONE',  ( -4.039897316195000698, 1516.787536375099990, 204.1233307748069876 ) ) ;
#37090 = CARTESIAN_POINT ( 'NONE',  ( -10.33691510611295072, 1423.136607578389885, 193.7437805996329416 ) ) ;
#37091 = EDGE_CURVE ( 'NONE', #107129, #109428, #58275, .T. ) ;
#37092 = CARTESIAN_POINT ( 'NONE',  ( -16.45057082148009897, 1486.105697468709877, 187.2873420190170179 ) ) ;
#37093 = CARTESIAN_POINT ( 'NONE',  ( -9.093965512229999604, 1423.880366148619942, 207.4491482849089721 ) ) ;
#37094 = CARTESIAN_POINT ( 'NONE',  ( -14.41017938444479185, 1420.830237651402740, 210.6135021038660966 ) ) ;
#37097 = ORIENTED_EDGE ( 'NONE', *, *, #6660, .T. ) ;
#37096 = CARTESIAN_POINT ( 'NONE',  ( -68.28858713622280163, 1379.746781482150027, 279.8552178119970222 ) ) ;
#37095 = TOROIDAL_SURFACE ( 'NONE', #46075, 2.000000000000000000, 1.000000000000000000 ) ;
#37098 = B_SPLINE_CURVE_WITH_KNOTS ( 'NONE', 3,
 ( #21273, #44890, #63887, #55482, #89607, #44326, #1783, #95813, #19080, #79040, #30802, #23501, #5052, #81745, #47077, #65537, #47620, #107512, #82860, #99643, #57693, #14545, #4519, #83409, #40307, #48734, #6704, #99096 ),
 .UNSPECIFIED., .F., .F.,
 ( 4, 3, 3, 3, 3, 3, 3, 3, 3, 4 ),
 ( -135.3348859266969839, -117.2219614944759911, -82.53340793120000285, -56.13266858090000255, -37.05188947199999916, -35.60956935775467969, -34.16724924350930337, -32.72651312666420154, -31.25859511619860598, -29.73193251775185786 ),
 .UNSPECIFIED. ) ;
#37099 = EDGE_LOOP ( 'NONE', ( #4072, #74777, #87371, #77818, #11449 ) ) ;
#37100 = CARTESIAN_POINT ( 'NONE',  ( 28.15885401449999748, 1509.153812686330184, 211.2508761953780265 ) ) ;
#37101 = ORIENTED_EDGE ( 'NONE', *, *, #86562, .T. ) ;
#37102 = CARTESIAN_POINT ( 'NONE',  ( 0.2886576936755593792, 1457.782815465476006, 199.5840498596436134 ) ) ;
#37103 = ADVANCED_FACE ( 'NONE', ( #6745 ), #15671, .T. ) ;
#37104 = CARTESIAN_POINT ( 'NONE',  ( -109.8256948709999961, 1384.925724839099757, 311.3807902692590233 ) ) ;
#37106 = CARTESIAN_POINT ( 'NONE',  ( 15.75924993152980136, 1409.463370494670244, 192.9545979772890121 ) ) ;
#37105 = CARTESIAN_POINT ( 'NONE',  ( 15.70001310441050002, 1411.351890569249917, 191.5014854339599992 ) ) ;
#37107 = DIRECTION ( 'NONE',  ( -1.000000000000000000, 0.000000000000000000, 0.000000000000000000 ) ) ;
#37108 = CARTESIAN_POINT ( 'NONE',  ( -25.36352536740899666, 1450.980594565270167, 137.3053237213029831 ) ) ;
#37109 = CARTESIAN_POINT ( 'NONE',  ( -0.6482359200730010151, 1468.620574178790093, 219.2670886169990183 ) ) ;
#37110 = CARTESIAN_POINT ( 'NONE',  ( 13.52138341930000109, 1409.385237502129939, 227.1744411764980214 ) ) ;
#37111 =( NAMED_UNIT ( * ) SI_UNIT ( $, .STERADIAN. ) SOLID_ANGLE_UNIT ( ) );
#37112 = CARTESIAN_POINT ( 'NONE',  ( 5.786527562335000319, 1517.025653221279981, 212.5728793591970032 ) ) ;
#37113 = CARTESIAN_POINT ( 'NONE',  ( 40.55649113733859679, 1439.640597909239887, 134.0999999981079895 ) ) ;
#37115 =( BOUNDED_CURVE ( )  B_SPLINE_CURVE ( 3, ( #53974, #3012, #37134, #105447 ),
 .UNSPECIFIED., .F., .T. ) 
 B_SPLINE_CURVE_WITH_KNOTS ( ( 4, 4 ),
 ( 1.969431562482085677E-12, 0.4510268114855934263 ),
 .UNSPECIFIED. ) 
 CURVE ( )  GEOMETRIC_REPRESENTATION_ITEM ( )  RATIONAL_B_SPLINE_CURVE ( ( 1.000000000000000000, 0.9831196230105669898, 0.9831196230105669898, 1.000000000000000000 ) ) 
 REPRESENTATION_ITEM ( '' )  );
#37114 = CARTESIAN_POINT ( 'NONE',  ( -9.200421498919999053, 1422.937291500389847, 210.7384572914190244 ) ) ;
#37116 = CARTESIAN_POINT ( 'NONE',  ( -0.5628230732972099304, 1418.319990097900018, 227.8334187985380197 ) ) ;
#37117 = ORIENTED_EDGE ( 'NONE', *, *, #21249, .F. ) ;
#37118 = CARTESIAN_POINT ( 'NONE',  ( -19.04700360180000374, 1444.155872993190087, 199.5980005317190091 ) ) ;
#37119 = CARTESIAN_POINT ( 'NONE',  ( -2.645191157576220142, 1430.969724324070285, 201.1795969678530014 ) ) ;
#37120 = ORIENTED_EDGE ( 'NONE', *, *, #79567, .F. ) ;
#37121 = ORIENTED_EDGE ( 'NONE', *, *, #70667, .T. ) ;
#37122 = VERTEX_POINT ( 'NONE', #19559 ) ;
#37123 = EDGE_CURVE ( 'NONE', #20110, #86208, #72529, .T. ) ;
#37124 = CARTESIAN_POINT ( 'NONE',  ( 2.309262712061971090, 1512.187213306747481, 217.7723287588028143 ) ) ;
#37125 = CYLINDRICAL_SURFACE ( 'NONE', #70664, 1.500000000000001332 ) ;
#37126 = CARTESIAN_POINT ( 'NONE',  ( -21.62164173379369814, 1517.151704408390060, 210.2163513719069954 ) ) ;
#37127 = AXIS2_PLACEMENT_3D ( 'NONE', #3870, #46422, #48052 ) ;
#37128 = CARTESIAN_POINT ( 'NONE',  ( -8.023381802619999448, 1384.920841448390092, 218.7875057646990058 ) ) ;
#37129 = DIRECTION ( 'NONE',  ( 0.000000000000000000, 0.000000000000000000, 1.000000000000000000 ) ) ;
#37130 = EDGE_CURVE ( 'NONE', #71158, #59489, #18671, .T. ) ;
#37131 = CARTESIAN_POINT ( 'NONE',  ( 11.60004869885203682, 0.000000000000000000, 137.0999999980979851 ) ) ;
#37132 = CARTESIAN_POINT ( 'NONE',  ( -68.45463625549879794, 1379.747337658472588, 279.3853496566876515 ) ) ;
#37133 = CARTESIAN_POINT ( 'NONE',  ( 4.291176059336820003, 1446.971469614359876, 154.7965853925720126 ) ) ;
#37134 = CARTESIAN_POINT ( 'NONE',  ( -4.151444337083049163, 1516.720891557477444, 217.8757000259121810 ) ) ;
#37135 = B_SPLINE_CURVE_WITH_KNOTS ( 'NONE', 3,
 ( #73504, #107639, #66763, #31470, #50502, #5740, #100336, #108737, #32588, #82442, #83522, #75698 ),
 .UNSPECIFIED., .F., .F.,
 ( 4, 2, 2, 2, 2, 4 ),
 ( 0.000000000000000000, 0.0007194225121792582585, 0.001079133768269195789, 0.001438845024359133428, 0.002158267536539008706, 0.002877690048718883550 ),
 .UNSPECIFIED. ) ;
#37136 = ADVANCED_FACE ( 'NONE', ( #17327 ), #100943, .F. ) ;
#37137 = ORIENTED_EDGE ( 'NONE', *, *, #59893, .T. ) ;
#37138 = CARTESIAN_POINT ( 'NONE',  ( 1.700259675955000160, 1516.898441858519845, 207.4036424686470070 ) ) ;
#37139 = ORIENTED_EDGE ( 'NONE', *, *, #4984, .F. ) ;
#37140 = CARTESIAN_POINT ( 'NONE',  ( 31.86551960166520558, 1440.913060387330006, 255.7072771772910187 ) ) ;
#37141 = CARTESIAN_POINT ( 'NONE',  ( -16.69460746589999900, 1509.155873805930014, 185.4220695494979907 ) ) ;
#37142 = ORIENTED_EDGE ( 'NONE', *, *, #53675, .F. ) ;
#37143 = CARTESIAN_POINT ( 'NONE',  ( -5.513261715040130184, 1508.551704609589933, 202.1093729265590184 ) ) ;
#37144 = CARTESIAN_POINT ( 'NONE',  ( -13.81938794709999918, 1409.562354991629945, 190.7366003602979845 ) ) ;
#37145 = CARTESIAN_POINT ( 'NONE',  ( -58.12963253436136313, 1379.720251017925648, 262.1005719551359334 ) ) ;
#37146 = ADVANCED_FACE ( 'NONE', ( #32916 ), #83877, .F. ) ;
#37148 = CARTESIAN_POINT ( 'NONE',  ( 21.84020450222056908, 1501.977400791986611, 234.9798068779740277 ) ) ;
#37147 = CARTESIAN_POINT ( 'NONE',  ( 8.248015215549999724, 1502.411902838189917, 208.8103458818409877 ) ) ;
#37149 = CARTESIAN_POINT ( 'NONE',  ( 22.37294064578369657, 1410.435102231539986, 206.2265387881180061 ) ) ;
#37150 = DIRECTION ( 'NONE',  ( 1.755985294532469921E-16, -1.000000000000000000, 1.338183447452831989E-16 ) ) ;
#37152 = B_SPLINE_CURVE_WITH_KNOTS ( 'NONE', 3,
 ( #18760, #97697, #61925, #20969, #28289, #19313, #79260, #62485, #87091, #29930, #2570, #89298, #12594, #4199, #96605, #87657, #64121, #70886, #19874, #45676, #2011, #54081, #36147, #70331, #79814, #104443, #37248, #27735, #98242, #22055, #90380, #56252, #98793, #83644, #22602, #21512, #56805, #75274, #74173, #100450, #57921, #5290, #13115, #39994, #89843, #90943, #83105, #108301, #30487, #13659, #73057, #23180, #92053, #14229, #55724, #107199, #14787, #91507, #5853, #6399, #40544, #31034, #65216, #49520, #47298, #107751, #23733, #66334, #48973, #74719, #48418, #81422, #99328, #4733, #32146, #108852, #47848, #38876, #6940, #31587, #15325, #65764, #32698, #64676, #41095, #109421, #81982, #39448, #73621, #82561, #99882, #57381, #76921, #100988, #17521, #84743, #102095, #33791, #101530, #109964, #53239, #8040, #87380, #10674, #59569, #24284, #67985, #50611, #110509, #42209, #41657, #44841, #76360, #78995, #2298, #60129, #51162, #25931 ),
 .UNSPECIFIED., .F., .F.,
 ( 4, 3, 3, 3, 3, 3, 3, 3, 3, 3, 3, 3, 3, 3, 3, 3, 3, 3, 3, 3, 3, 3, 3, 3, 3, 3, 3, 3, 3, 3, 3, 3, 3, 3, 3, 3, 3, 3, 3, 4 ),
 ( 0.000000000000000000, 1.208150270900489875, 2.429651893694120268, 3.658664080013049436, 4.894387409778079956, 6.135850761516199903, 7.383699400574919913, 8.633905489600488536, 9.885650277918578865, 10.37921801280000089, 11.62573138507199921, 12.86918051959590059, 14.10827304762559997, 15.34185558769280000, 16.56515402037690166, 17.78190617995440093, 18.98746852701869869, 19.90003809979999971, 21.10030473618510172, 22.30904239636550201, 23.52596673361060198, 24.75067484191579936, 25.98628883277909551, 27.22721929388799822, 28.47521747268259773, 29.42039610570000008, 30.67411275314229968, 31.94530611542449705, 33.20243901502989559, 34.45840916216139505, 35.71192178359849834, 36.99485625054889937, 38.23735636254910020, 39.47464645472779665, 40.70388848455859687, 40.84365965140000299, 42.06598350958260113, 43.28072877285099906, 44.48361342172800192, 45.10384108367830436 ),
 .UNSPECIFIED. ) ;
#37151 = CARTESIAN_POINT ( 'NONE',  ( 27.46336372570400286, 1441.403115843749902, 137.3061811889630235 ) ) ;
#37153 = B_SPLINE_CURVE_WITH_KNOTS ( 'NONE', 5,
 ( #43986, #78122, #19303, #53504, #29369, #107738, #79803, #88745, #38866, #106091, #99317, #4187, #20408, #71435, #64108 ),
 .UNSPECIFIED., .F., .F.,
 ( 6, 3, 3, 3, 6 ),
 ( 0.000000000000000000, 0.1823333780437425278, 0.5255321158878730747, 0.7212967652657603645, 1.000000000000000000 ),
 .UNSPECIFIED. ) ;
#37154 = EDGE_CURVE ( 'NONE', #106272, #49433, #49748, .T. ) ;
#37155 = CARTESIAN_POINT ( 'NONE',  ( -13.19867885639999905, 1434.900411297580149, 148.5640551728980085 ) ) ;
#37156 = CARTESIAN_POINT ( 'NONE',  ( 16.10667611295789570, 1435.057002863770549, 146.9490699512605545 ) ) ;
#37158 = CARTESIAN_POINT ( 'NONE',  ( 17.99277867620000038, 1432.534352819589913, 212.7098897757189775 ) ) ;
#37157 = CARTESIAN_POINT ( 'NONE',  ( 15.69201213754273638, 1410.669748705371148, 191.5225451384409610 ) ) ;
#37159 = CIRCLE ( 'NONE', #99697, 2.000006068106865875 ) ;
#37160 = CARTESIAN_POINT ( 'NONE',  ( -2.483322492024999661, 1517.139039350860003, 215.6851008610869940 ) ) ;
#37161 = EDGE_CURVE ( 'NONE', #5162, #31573, #25055, .T. ) ;
#37162 = CARTESIAN_POINT ( 'NONE',  ( -2.404972330437235684, 1525.211473355384896, 242.0950351792775450 ) ) ;
#37163 = FACE_OUTER_BOUND ( 'NONE', #90384, .T. ) ;
#37164 = CARTESIAN_POINT ( 'NONE',  ( 2.694739704345535891, 1517.051704408389924, 206.1657712119973382 ) ) ;
#37165 = CARTESIAN_POINT ( 'NONE',  ( -1.701729858475000023, 1516.969638403840008, 212.0041719496170174 ) ) ;
#37166 = CARTESIAN_POINT ( 'NONE',  ( -21.49889961270000072, 1488.801231227030030, 208.8489735576630153 ) ) ;
#37167 = CARTESIAN_POINT ( 'NONE',  ( 29.53442096303756159, 1525.651285554130254, 221.7311742728463457 ) ) ;
#37169 = ORIENTED_EDGE ( 'NONE', *, *, #57263, .F. ) ;
#37168 = CARTESIAN_POINT ( 'NONE',  ( -91.60491507549998857, 1389.456972387929909, 296.8809262675589480 ) ) ;
#37170 = FACE_OUTER_BOUND ( 'NONE', #86771, .T. ) ;
#37171 = CARTESIAN_POINT ( 'NONE',  ( 4.804950796049999973, 1465.695272585830025, 240.4142140057979873 ) ) ;
#37172 = CARTESIAN_POINT ( 'NONE',  ( -3.276492809264478723, 1486.691461902717947, 220.6577066230676962 ) ) ;
#37173 = CARTESIAN_POINT ( 'NONE',  ( -1.794934993283609614, 1484.669492803836192, 198.5571763550413209 ) ) ;
#37174 = CARTESIAN_POINT ( 'NONE',  ( -31.33756689035267229, 1523.580203803270933, 196.3415365178086631 ) ) ;
#37175 = CARTESIAN_POINT ( 'NONE',  ( -21.38445639540000087, 1453.349625644829985, 224.4824140897979987 ) ) ;
#37176 = AXIS2_PLACEMENT_3D ( 'NONE', #38009, #46976, #105778 ) ;
#37178 = CARTESIAN_POINT ( 'NONE',  ( 2.500000000000000000, 1419.383414104229814, 144.0748232612980075 ) ) ;
#37177 = CARTESIAN_POINT ( 'NONE',  ( 11.58425270890000114, 1432.866135319230125, 151.1952033301980123 ) ) ;
#37179 = CARTESIAN_POINT ( 'NONE',  ( -9.499594844283979711, 1449.194695334430207, 207.7958694408430063 ) ) ;
#37180 = CARTESIAN_POINT ( 'NONE',  ( -105.5548029506649925, 1381.074381071139896, 308.7453718054549654 ) ) ;
#37181 = ORIENTED_EDGE ( 'NONE', *, *, #46603, .T. ) ;
#37182 = CARTESIAN_POINT ( 'NONE',  ( -3.264778817514999876, 1516.727068157269969, 204.1245957781970048 ) ) ;
#37183 = CARTESIAN_POINT ( 'NONE',  ( 0.8749198469600000250, 1406.783822975030034, 269.6498238079980183 ) ) ;
#37184 = CARTESIAN_POINT ( 'NONE',  ( -1.117126662530000036, 1515.456827602489966, 213.3225888563989940 ) ) ;
#37185 = VECTOR ( 'NONE', #28130, 1000.000000000000000 ) ;
#37186 = EDGE_CURVE ( 'NONE', #72398, #36202, #27482, .T. ) ;
#37187 = TOROIDAL_SURFACE ( 'NONE', #35419, 8.013264357029999729, 0.5000000000000000000 ) ;
#37188 = CARTESIAN_POINT ( 'NONE',  ( 6.659675234235749919, 1473.897714816529970, 270.2927028066139883 ) ) ;
#37189 = ADVANCED_FACE ( 'NONE', ( #99564 ), #32106, .T. ) ;
#37190 = CARTESIAN_POINT ( 'NONE',  ( 2.478907528220000156, 1433.027990083169925, 157.5361285726980043 ) ) ;
#37191 = CARTESIAN_POINT ( 'NONE',  ( 11.60004869885203682, 1424.140514235982437, 136.0100240574817292 ) ) ;
#37192 = CARTESIAN_POINT ( 'NONE',  ( -37.15831699375700481, 1440.913060387739961, 254.8961880939840228 ) ) ;
#37193 = DIRECTION ( 'NONE',  ( 0.000000000000000000, -1.000000000000000000, 0.000000000000000000 ) ) ;
#37194 = CARTESIAN_POINT ( 'NONE',  ( -11.86629850686009924, 1432.349867577580198, 149.9824227077560010 ) ) ;
#37195 = DIRECTION ( 'NONE',  ( -0.4186104444426561599, -0.02615378819618780631, 0.9077892239757592296 ) ) ;
#37196 = FACE_OUTER_BOUND ( 'NONE', #30067, .T. ) ;
#37197 = CARTESIAN_POINT ( 'NONE',  ( 1.871941823660000059, 1506.355489675189801, 221.3883213455989960 ) ) ;
#37198 = CARTESIAN_POINT ( 'NONE',  ( -4.324092179320000007, 1515.269353058490196, 209.4836008490580070 ) ) ;
#37199 = ORIENTED_EDGE ( 'NONE', *, *, #48895, .F. ) ;
#37200 = CARTESIAN_POINT ( 'NONE',  ( -31.32742178079999462, 1437.308404696490015, 255.3819207742980097 ) ) ;
#37201 = EDGE_CURVE ( 'NONE', #50084, #36569, #60159, .T. ) ;
#37202 = CARTESIAN_POINT ( 'NONE',  ( 6.578458372278979560, 1465.931120787709915, 201.5766924354090293 ) ) ;
#37203 = CARTESIAN_POINT ( 'NONE',  ( -1.770636241409999867, 1475.812198116930176, 266.9599394754979471 ) ) ;
#37205 = VECTOR ( 'NONE', #95737, 1000.000000000000000 ) ;
#37204 = CARTESIAN_POINT ( 'NONE',  ( 13.67970179620000160, 1494.136271315190015, 192.1856007679989773 ) ) ;
#37206 = CARTESIAN_POINT ( 'NONE',  ( -32.41382812665801794, 1525.581535527370306, 197.9832485531580630 ) ) ;
#37207 = FACE_OUTER_BOUND ( 'NONE', #75821, .T. ) ;
#37208 = CARTESIAN_POINT ( 'NONE',  ( -29.93716070313080024, 1384.828683197690225, 227.9879461525169972 ) ) ;
#37209 = DIRECTION ( 'NONE',  ( -5.980589973904019347E-17, 1.000000000000000000, -1.736889445713099699E-16 ) ) ;
#37210 = CARTESIAN_POINT ( 'NONE',  ( -10.97570620389999974, 1482.624300749189842, 205.8415958148989944 ) ) ;
#37211 = CARTESIAN_POINT ( 'NONE',  ( 26.68383462467300049, 1435.975862505480109, 136.4814827833579898 ) ) ;
#37212 = CARTESIAN_POINT ( 'NONE',  ( -10.94421840418110037, 1396.295240915489785, 210.8008358220470200 ) ) ;
#37213 = CARTESIAN_POINT ( 'NONE',  ( -14.93588953819999965, 1422.319491557630045, 228.4029780258980225 ) ) ;
#37214 = EDGE_CURVE ( 'NONE', #20317, #86983, #86636, .T. ) ;
#37215 = CARTESIAN_POINT ( 'NONE',  ( -16.62086504976599954, 1410.867400916760062, 226.5111953344219842 ) ) ;
#37216 = CARTESIAN_POINT ( 'NONE',  ( 19.27986066999695680, 1456.016186168368449, 225.1713710279379370 ) ) ;
#37217 = ORIENTED_EDGE ( 'NONE', *, *, #36038, .T. ) ;
#37218 = CARTESIAN_POINT ( 'NONE',  ( -11.49747572423030029, 1414.913060387329779, 197.9009878255399997 ) ) ;
#37219 = CARTESIAN_POINT ( 'NONE',  ( 6.774723932182340036, 1511.035127054690065, 217.4331360664359920 ) ) ;
#37220 = CARTESIAN_POINT ( 'NONE',  ( -18.11608073946016617, 1485.171156873887867, 188.9685297383233262 ) ) ;
#37222 = CARTESIAN_POINT ( 'NONE',  ( -11.28295023116499962, 1512.609537213029853, 192.8912262721669890 ) ) ;
#37221 = CARTESIAN_POINT ( 'NONE',  ( 10.08386706099999941, 1425.185608643229898, 99.60988851169790337 ) ) ;
#37223 = DIRECTION ( 'NONE',  ( 9.120238070098449704E-47, -1.000000000000000000, 1.836970198721029688E-16 ) ) ;
#37224 = ADVANCED_FACE ( 'NONE', ( #458 ), #107156, .T. ) ;
#37225 = CARTESIAN_POINT ( 'NONE',  ( -11.23388613411650105, 1443.913060387330006, 205.3674499604520065 ) ) ;
#37226 = AXIS2_PLACEMENT_3D ( 'NONE', #71714, #54339, #47032 ) ;
#37227 = CARTESIAN_POINT ( 'NONE',  ( 5.779627054084999216, 1516.977993847330026, 201.4011957967969977 ) ) ;
#37228 = CARTESIAN_POINT ( 'NONE',  ( 7.467907613800000455, 1424.983389225890051, 212.2844559904590085 ) ) ;
#37229 = CARTESIAN_POINT ( 'NONE',  ( -4.354856984870000502, 1481.954696296189923, 231.1149923864989830 ) ) ;
#37230 = CARTESIAN_POINT ( 'NONE',  ( 4.179882439260000027, 1508.490740823229999, 181.1834003096979870 ) ) ;
#37231 = CARTESIAN_POINT ( 'NONE',  ( 7.621419120635000155, 1512.021995456199875, 206.5558387662869961 ) ) ;
#37232 = CARTESIAN_POINT ( 'NONE',  ( -83.77787960067068695, 1379.600322909919896, 298.8836558466570636 ) ) ;
#37233 = CARTESIAN_POINT ( 'NONE',  ( 6.912446013178925597, 1366.858127842395334, 210.6218459617142003 ) ) ;
#37235 = VERTEX_POINT ( 'NONE', #77695 ) ;
#37234 = CARTESIAN_POINT ( 'NONE',  ( -22.59589169820000265, 1507.700907224229923, 190.9355247910979756 ) ) ;
#37236 = ORIENTED_EDGE ( 'NONE', *, *, #101696, .F. ) ;
#37237 = LINE ( 'NONE', #89832, #109954 ) ;
#37238 = CARTESIAN_POINT ( 'NONE',  ( -14.51206241080000048, 1409.419832773630105, 192.1183054032979953 ) ) ;
#37239 = CARTESIAN_POINT ( 'NONE',  ( -9.061398245540321028, 1507.228273329460080, 237.0094930597339840 ) ) ;
#37240 = CARTESIAN_POINT ( 'NONE',  ( -7.985842396434999380, 1511.355055856609852, 213.1582267177570031 ) ) ;
#37242 = CARTESIAN_POINT ( 'NONE',  ( -113.4000000000000057, 1309.112692017090239, 312.2430413686190036 ) ) ;
#37241 = CARTESIAN_POINT ( 'NONE',  ( -8.307395124150000143, 1384.509440565790101, 218.6838747432389880 ) ) ;
#37243 = CARTESIAN_POINT ( 'NONE',  ( -32.21030510514562195, 1524.412455883367329, 202.1448083870403138 ) ) ;
#37244 = EDGE_CURVE ( 'NONE', #40573, #48513, #76106, .T. ) ;
#37245 = DIRECTION ( 'NONE',  ( 0.9526631324121143107, 0.2953532403522530769, -0.07210700074307911656 ) ) ;
#37246 = CARTESIAN_POINT ( 'NONE',  ( -37.43491952192539429, 1450.745172276120002, 135.6028198332160173 ) ) ;
#37247 = CARTESIAN_POINT ( 'NONE',  ( -2.500000000000000000, 1448.210404589970040, 167.6157966154659960 ) ) ;
#37248 = CARTESIAN_POINT ( 'NONE',  ( 9.871841148089821161, 1396.257792678529995, 214.1149673374819713 ) ) ;
#37249 = CARTESIAN_POINT ( 'NONE',  ( -26.78805561499009968, 1436.761859905399888, 136.7824057165339866 ) ) ;
#37250 = CARTESIAN_POINT ( 'NONE',  ( -1.472772997237789872, 1415.954755716330055, 226.2562541087189913 ) ) ;
#37251 = CARTESIAN_POINT ( 'NONE',  ( 41.65927937599999353, 1443.915252855300196, 135.6909788338979865 ) ) ;
#37252 = VERTEX_POINT ( 'NONE', #35684 ) ;
#37253 = CARTESIAN_POINT ( 'NONE',  ( 3.837151314420000237, 1425.396477843930143, 185.3020672648979996 ) ) ;
#37254 = CARTESIAN_POINT ( 'NONE',  ( 12.12358720160000125, 1442.555572165430021, 187.1519726473979972 ) ) ;
#37255 = VERTEX_POINT ( 'NONE', #18316 ) ;
#37256 = AXIS2_PLACEMENT_3D ( 'NONE', #6455, #14286, #32206 ) ;
#37257 = ORIENTED_EDGE ( 'NONE', *, *, #105628, .T. ) ;
#37258 = EDGE_CURVE ( 'NONE', #64180, #59778, #61469, .T. ) ;
#37259 = CARTESIAN_POINT ( 'NONE',  ( 1.393816646507355372, 1511.187213306747708, 243.1385343369520342 ) ) ;
#37260 = CARTESIAN_POINT ( 'NONE',  ( 9.093835586129998205, 1363.023136422000107, 207.6218459616989946 ) ) ;
#37261 = AXIS2_PLACEMENT_3D ( 'NONE', #59259, #18317, #16643 ) ;
#37262 = CARTESIAN_POINT ( 'NONE',  ( -1.706797824074999914, 1517.164987839469859, 214.9112406324369999 ) ) ;
#37263 = CARTESIAN_POINT ( 'NONE',  ( 2.625066769795000088, 1511.873873588870083, 216.7407507270369820 ) ) ;
#37264 = AXIS2_PLACEMENT_3D ( 'NONE', #22007, #75222, #90898 ) ;
#37265 = EDGE_CURVE ( 'NONE', #43261, #40565, #70371, .T. ) ;
#37266 = ORIENTED_EDGE ( 'NONE', *, *, #66601, .F. ) ;
#37267 = CARTESIAN_POINT ( 'NONE',  ( 7.916532357550000398, 1425.151355441629903, 211.5881757975789981 ) ) ;
#37268 = CARTESIAN_POINT ( 'NONE',  ( -78.82321740920001218, 1378.727265989730085, 290.9639565884590411 ) ) ;
#37269 = VECTOR ( 'NONE', #89068, 1000.000000000000000 ) ;
#37270 = AXIS2_PLACEMENT_3D ( 'NONE', #35171, #67694, #25094 ) ;
#37271 = CARTESIAN_POINT ( 'NONE',  ( -105.8090605497289971, 1378.913060387299993, 303.7886957086479924 ) ) ;
#37272 = CARTESIAN_POINT ( 'NONE',  ( -5.009478105444999940, 1516.886345593249871, 204.5093386581970094 ) ) ;
#37273 = CARTESIAN_POINT ( 'NONE',  ( -29.61076270571678748, 1526.107880201381477, 220.7510230871936017 ) ) ;
#37274 = CARTESIAN_POINT ( 'NONE',  ( -113.4000000000000057, 1385.026018367459983, 297.2218459572590064 ) ) ;
#37275 = CARTESIAN_POINT ( 'NONE',  ( -6.440516398849998936, 1409.640628502429990, 231.0932606539979872 ) ) ;
#37277 = ORIENTED_EDGE ( 'NONE', *, *, #47370, .T. ) ;
#37276 = CARTESIAN_POINT ( 'NONE',  ( 2.143765237719135186, 1525.848196786131211, 176.8604030897658674 ) ) ;
#37278 = EDGE_CURVE ( 'NONE', #94190, #91380, #67169, .T. ) ;
#37279 = CARTESIAN_POINT ( 'NONE',  ( 33.12914009259999659, 1451.756166416729911, 134.7383383604980054 ) ) ;
#37280 = CARTESIAN_POINT ( 'NONE',  ( -26.31643818619939879, 1440.913060459879944, 223.5219688644119742 ) ) ;
#37281 = CARTESIAN_POINT ( 'NONE',  ( -22.71366063019999970, 1384.180912115839874, 221.9862684950589937 ) ) ;
#37282 = CARTESIAN_POINT ( 'NONE',  ( 16.61610589626278767, 1423.426877523299481, 227.8835257429488195 ) ) ;
#37283 = CONICAL_SURFACE ( 'NONE', #98089, 7.500000000000000000, 0.02617993877989872875 ) ;
#37284 = CARTESIAN_POINT ( 'NONE',  ( 26.02835829290000191, 1413.547636220630011, 269.9886483863980402 ) ) ;
#37285 = EDGE_CURVE ( 'NONE', #37407, #93915, #42684, .T. ) ;
#37286 = CARTESIAN_POINT ( 'NONE',  ( 7.335900995594999863, 1517.068717944079935, 213.1567545299469657 ) ) ;
#37287 = CARTESIAN_POINT ( 'NONE',  ( -67.30421475440000734, 1379.744441735729879, 277.0965467265589837 ) ) ;
#37288 = DIRECTION ( 'NONE',  ( 0.000000000000000000, 0.000000000000000000, 1.000000000000000000 ) ) ;
#37289 = CARTESIAN_POINT ( 'NONE',  ( 6.543292404667510276, 1424.997647815940127, 192.3570860859640277 ) ) ;
#37290 = CARTESIAN_POINT ( 'NONE',  ( 16.66443952165710130, 1492.498711326890088, 193.3249459387799902 ) ) ;
#37291 =( BOUNDED_SURFACE ( )  B_SPLINE_SURFACE ( 4, 2, ( 
 ( #43211, #50513, #7389, #41554, #67321, #17410, #85741 ),
 ( #84636, #42102, #110398, #33678, #118, #67870, #16855 ),
 ( #42649, #76803, #26952, #1212, #94697, #2331, #61679 ),
 ( #95802, #69534, #53840, #53274, #52167, #36993, #62233 ),
 ( #103655, #27492, #105309, #45428, #71187, #19070, #35347 ) ),
 .UNSPECIFIED., .F., .F., .F. ) 
 B_SPLINE_SURFACE_WITH_KNOTS ( ( 5, 5 ),
 ( 3, 2, 2, 3 ),
 ( 1.967616199060000071, 3.613988937050000239 ),
 ( 11.46118682297159985, 11.46128530315550087, 12.56637061435916003, 12.57442343279650032 ),
 .UNSPECIFIED. ) 
 GEOMETRIC_REPRESENTATION_ITEM ( )  RATIONAL_B_SPLINE_SURFACE ( (
 ( 0.8778316440755170591, 0.8778241674203509648, 0.8778166930676719604, 0.7939440089458740246, 1.000000000000000000, 0.9984984584745990599, 0.9970123125050369683),
 ( 0.8778316440755170591, 0.8778241674203509648, 0.8778166930676719604, 0.7939440089458740246, 1.000000000000000000, 0.9984984584745990599, 0.9970123125050369683),
 ( 0.8778316440755170591, 0.8778241674203509648, 0.8778166930676719604, 0.7939440089458740246, 1.000000000000000000, 0.9984984584745990599, 0.9970123125050369683),
 ( 0.8778316440755170591, 0.8778241674203509648, 0.8778166930676719604, 0.7939440089458740246, 1.000000000000000000, 0.9984984584745990599, 0.9970123125050369683),
 ( 0.8778316440755170591, 0.8778241674203509648, 0.8778166930676719604, 0.7939440089458740246, 1.000000000000000000, 0.9984984584745990599, 0.9970123125050369683) ) ) 
 REPRESENTATION_ITEM ( '' )  SURFACE ( )  );
#37292 = CARTESIAN_POINT ( 'NONE',  ( -4.031168805994999715, 1516.805675336850072, 209.8787446699039947 ) ) ;
#37293 = ORIENTED_EDGE ( 'NONE', *, *, #48270, .T. ) ;
#37294 = CARTESIAN_POINT ( 'NONE',  ( 4.275795800415670200, 1421.906489317239902, 184.1737643678170002 ) ) ;
#37295 = CARTESIAN_POINT ( 'NONE',  ( -0.7710674123559999593, 1420.454978029629956, 233.5406515987980072 ) ) ;
#37296 = CARTESIAN_POINT ( 'NONE',  ( 5.360168252066184635, 1422.336953262081352, 139.1415641536600276 ) ) ;
#37297 = ORIENTED_EDGE ( 'NONE', *, *, #14328, .T. ) ;
#37298 = CARTESIAN_POINT ( 'NONE',  ( -36.42513895959979919, 1385.201677668759885, 236.2565189331969862 ) ) ;
#37299 = CARTESIAN_POINT ( 'NONE',  ( 2.694739704345535447, 1522.051704408389924, 206.1657712119973382 ) ) ;
#37300 = CARTESIAN_POINT ( 'NONE',  ( 10.50998152559020049, 1488.402885203860023, 233.3684635021429870 ) ) ;
#37301 = CARTESIAN_POINT ( 'NONE',  ( -20.15451341185540457, 1507.845745166900087, 228.9024278368160026 ) ) ;
#37302 = CARTESIAN_POINT ( 'NONE',  ( -29.37019419317373448, 1526.382868172864164, 217.2592043484932844 ) ) ;
#37303 = CARTESIAN_POINT ( 'NONE',  ( 0.1764129495400000303, 1409.076774902530133, 232.6426639635980109 ) ) ;
#37304 = CARTESIAN_POINT ( 'NONE',  ( -0.04442723591320390381, 1420.445872299549819, 182.6811953437060083 ) ) ;
#37306 = CARTESIAN_POINT ( 'NONE',  ( 10.47511427260239891, 1482.040461736080033, 210.7458695605469927 ) ) ;
#37305 = CARTESIAN_POINT ( 'NONE',  ( 2.875850094215000041, 1516.647618671360078, 214.8936433964170192 ) ) ;
#37307 = FACE_OUTER_BOUND ( 'NONE', #1649, .T. ) ;
#37308 = CARTESIAN_POINT ( 'NONE',  ( 10.52924840420589980, 1470.684170504899839, 209.6686858039719823 ) ) ;
#37309 = ORIENTED_EDGE ( 'NONE', *, *, #52831, .T. ) ;
#37310 = CARTESIAN_POINT ( 'NONE',  ( -12.78749341904959991, 1416.842625005220043, 196.1051283137009875 ) ) ;
#37311 = CARTESIAN_POINT ( 'NONE',  ( -18.66420869458074350, 1526.382868172863937, 185.4599087859683095 ) ) ;
#37312 = ORIENTED_EDGE ( 'NONE', *, *, #78217, .T. ) ;
#37313 = CARTESIAN_POINT ( 'NONE',  ( 11.60004869885203327, 1426.466819648586352, 135.9733978570640716 ) ) ;
#37314 = B_SPLINE_CURVE_WITH_KNOTS ( 'NONE', 5,
 ( #21845, #29724, #13452, #81769, #90729, #39789 ),
 .UNSPECIFIED., .F., .F.,
 ( 6, 6 ),
 ( -1.999999509065029990, -6.779759595954004681E-07 ),
 .UNSPECIFIED. ) ;
#37315 = CARTESIAN_POINT ( 'NONE',  ( 4.824051484379999977, 1425.779874028899940, 210.3687978271890131 ) ) ;
#37316 = CARTESIAN_POINT ( 'NONE',  ( 7.482857888537069790, 1511.023286695659863, 202.9712329530480019 ) ) ;
#37317 = CARTESIAN_POINT ( 'NONE',  ( 2.003345808180000187, 1442.032355148490069, 218.4647324736090184 ) ) ;
#37318 = CARTESIAN_POINT ( 'NONE',  ( -27.42598290503229919, 1509.711393979569948, 201.1186931426829858 ) ) ;
#37319 = CARTESIAN_POINT ( 'NONE',  ( -2.499999992009999783, 1448.405372066850077, 154.5226066568979775 ) ) ;
#37320 = CARTESIAN_POINT ( 'NONE',  ( -17.85044820919999964, 1423.477864059130070, 226.0162590187979959 ) ) ;
#37321 = CARTESIAN_POINT ( 'NONE',  ( -16.53868516720000059, 1435.074985172869901, 146.6152374475979911 ) ) ;
#37322 = CARTESIAN_POINT ( 'NONE',  ( -19.18813880309999931, 1465.797355387890093, 204.3301597990889888 ) ) ;
#37323 = CARTESIAN_POINT ( 'NONE',  ( 17.31877846000000076, 1416.204268826130146, 191.9452355195979862 ) ) ;
#37325 = CARTESIAN_POINT ( 'NONE',  ( -18.93888144065705603, 1438.916806179615605, 210.4257881881777053 ) ) ;
#37324 = CARTESIAN_POINT ( 'NONE',  ( 0.9956485761700990533, 1409.114994398940098, 232.2357569347449839 ) ) ;
#37326 = CARTESIAN_POINT ( 'NONE',  ( -108.6556974451439999, 1383.125878945329987, 312.9723968252589543 ) ) ;
#37327 = ORIENTED_EDGE ( 'NONE', *, *, #1647, .F. ) ;
#37328 = DIRECTION ( 'NONE',  ( 3.740163838737602180E-16, -0.7071067811865475727, -0.7071067811865475727 ) ) ;
#37329 = CARTESIAN_POINT ( 'NONE',  ( -8.954648243350000314, 1508.433707402489972, 219.1777012664989854 ) ) ;
#37330 = CARTESIAN_POINT ( 'NONE',  ( 11.43185072513739797, 1443.913060387330006, 147.9056598087979921 ) ) ;
#37331 = CARTESIAN_POINT ( 'NONE',  ( -16.88275388290000123, 1507.705444072489854, 209.4032267757409898 ) ) ;
#37332 = CARTESIAN_POINT ( 'NONE',  ( -3.520005857620000178, 1483.900612090289997, 199.0196415985990086 ) ) ;
#37333 = CIRCLE ( 'NONE', #53421, 1.999999999999999556 ) ;
#37334 = CARTESIAN_POINT ( 'NONE',  ( -18.53418672730000338, 1507.620785846030003, 229.7143111650979961 ) ) ;
#37335 = CARTESIAN_POINT ( 'NONE',  ( 1.779428962334640207, 1456.357349043589920, 198.6855221538999956 ) ) ;
#37336 = CARTESIAN_POINT ( 'NONE',  ( -17.08684344950000167, 1414.913528139129994, 207.7074066321380030 ) ) ;
#37337 = DIRECTION ( 'NONE',  ( -0.000000000000000000, -1.000000000000000000, -0.000000000000000000 ) ) ;
#37338 = CIRCLE ( 'NONE', #42690, 1.000000000000000888 ) ;
#37339 = CARTESIAN_POINT ( 'NONE',  ( -9.092716900757949361, 1490.074253787619909, 215.3417004495109950 ) ) ;
#37340 = CARTESIAN_POINT ( 'NONE',  ( -20.36852816458540261, 1464.956552523959999, 210.9458084407719980 ) ) ;
#37341 = CARTESIAN_POINT ( 'NONE',  ( -95.02475577813770258, 1383.767157683600090, 309.8628875536620058 ) ) ;
#37342 = CARTESIAN_POINT ( 'NONE',  ( -109.4279020612130040, 1384.328769556499765, 311.2418332238150356 ) ) ;
#37343 = CARTESIAN_POINT ( 'NONE',  ( 7.360592667339999728, 1427.547308638959976, 213.0878291651189897 ) ) ;
#37345 = ORIENTED_EDGE ( 'NONE', *, *, #1786, .F. ) ;
#37344 = CARTESIAN_POINT ( 'NONE',  ( -18.75058736031470019, 1443.878575118040089, 210.7892154803369920 ) ) ;
#37346 = CARTESIAN_POINT ( 'NONE',  ( -79.44287100420000058, 1383.304495963870067, 282.9878770193590185 ) ) ;
#37347 = CARTESIAN_POINT ( 'NONE',  ( -0.8266213562413129434, 1417.364321680721559, 235.5374543686832283 ) ) ;
#37348 = ORIENTED_EDGE ( 'NONE', *, *, #78052, .T. ) ;
#37349 = EDGE_LOOP ( 'NONE', ( #29811, #29080, #75506, #527, #96555, #90999, #47467, #90317, #100578, #12093, #3947, #78139, #8993, #19572, #4956 ) ) ;
#37350 = CARTESIAN_POINT ( 'NONE',  ( 18.34590453789999742, 1416.851343897030119, 209.3831232140299790 ) ) ;
#37351 = CARTESIAN_POINT ( 'NONE',  ( -109.1643463520000097, 1384.912499995879898, 297.1325824111589782 ) ) ;
#37352 = CARTESIAN_POINT ( 'NONE',  ( 13.28748371237506731, 1443.220925009591383, 169.3801757590552768 ) ) ;
#37354 = CARTESIAN_POINT ( 'NONE',  ( -32.79493994620000308, 1447.324624203729854, 248.1152222123979811 ) ) ;
#37353 = CARTESIAN_POINT ( 'NONE',  ( 36.73277783119023354, 1426.075947637769559, 269.5563403403481288 ) ) ;
#37355 = CARTESIAN_POINT ( 'NONE',  ( -20.45323004049999938, 1505.124052112629897, 189.8381095372979814 ) ) ;
#37356 = CARTESIAN_POINT ( 'NONE',  ( -11.91180695089999908, 1433.366504895910111, 149.9330032971979847 ) ) ;
#37357 = CARTESIAN_POINT ( 'NONE',  ( 27.13474198999999842, 1509.190014491130114, 206.1955381244279693 ) ) ;
#37358 = CARTESIAN_POINT ( 'NONE',  ( -18.97220044710000053, 1486.246524106529932, 189.3000240390980196 ) ) ;
#37359 = AXIS2_PLACEMENT_3D ( 'NONE', #74601, #49941, #84079 ) ;
#37360 = CARTESIAN_POINT ( 'NONE',  ( 12.66769394129999959, 1410.724484346930012, 190.2446672170979980 ) ) ;
#37361 = CARTESIAN_POINT ( 'NONE',  ( 5.250757762980000187, 1425.396628029330259, 185.7731830333980270 ) ) ;
#37362 = CARTESIAN_POINT ( 'NONE',  ( -0.6417514479877001188, 1515.135428326259898, 213.4494450834599775 ) ) ;
#37363 = CARTESIAN_POINT ( 'NONE',  ( -18.66420869458074350, 1526.382868172863937, 185.4599087859683095 ) ) ;
#37364 = CARTESIAN_POINT ( 'NONE',  ( -17.60627563539999940, 1410.895669412530196, 209.1303365420520208 ) ) ;
#37365 = CARTESIAN_POINT ( 'NONE',  ( 3.350338079455601026, 1523.604703353109699, 242.0808062845893289 ) ) ;
#37367 = ORIENTED_EDGE ( 'NONE', *, *, #34939, .T. ) ;
#37366 = CARTESIAN_POINT ( 'NONE',  ( 4.221033085759999359, 1472.290285735790121, 218.3905899716789918 ) ) ;
#37368 = ORIENTED_EDGE ( 'NONE', *, *, #98695, .T. ) ;
#37369 = CARTESIAN_POINT ( 'NONE',  ( -2.487923159525530004, 1508.611354624159958, 213.7999901551609980 ) ) ;
#37370 = CARTESIAN_POINT ( 'NONE',  ( -5.221937430894320720, 1489.269441483490027, 185.8916500386229984 ) ) ;
#37371 = CARTESIAN_POINT ( 'NONE',  ( -20.15863288730000136, 1468.575974982129992, 270.0907409689979772 ) ) ;
#37372 = CARTESIAN_POINT ( 'NONE',  ( -23.87637954442272914, 1435.955112056939470, 211.3744525167508641 ) ) ;
#37373 = CARTESIAN_POINT ( 'NONE',  ( 4.551914400959999783E-15, 1438.194204504490017, 155.6035180864980134 ) ) ;
#37374 = CARTESIAN_POINT ( 'NONE',  ( -2.483162210680000204, 1476.934831334089949, 201.9767984825489862 ) ) ;
#37375 = EDGE_CURVE ( 'NONE', #39203, #38027, #43548, .T. ) ;
#37376 = CARTESIAN_POINT ( 'NONE',  ( 4.328546746085200070, 1515.099240016830208, 210.2463711844760041 ) ) ;
#37377 = ADVANCED_FACE ( 'NONE', ( #42427 ), #81443, .F. ) ;
#37378 = CARTESIAN_POINT ( 'NONE',  ( -12.25907712989999965, 1420.080780804629740, 228.9648508334979908 ) ) ;
#37379 = CARTESIAN_POINT ( 'NONE',  ( -6.214213076750000120, 1457.627299019590282, 216.3771072480390103 ) ) ;
#37380 = CARTESIAN_POINT ( 'NONE',  ( 10.06893603924860869, 1361.212982179845767, 209.6218459617033432 ) ) ;
#37381 = CARTESIAN_POINT ( 'NONE',  ( -45.11974237219880735, 1434.479238661079989, 266.4358854948999920 ) ) ;
#37382 = EDGE_LOOP ( 'NONE', ( #13410, #45965, #3687, #39545 ) ) ;
#37383 = CARTESIAN_POINT ( 'NONE',  ( -8.001908350489999933, 1424.415893222990007, 210.2813077655789868 ) ) ;
#37384 = EDGE_LOOP ( 'NONE', ( #29042, #26434, #62567, #91918 ) ) ;
#37385 = CARTESIAN_POINT ( 'NONE',  ( -1.117840124865000062, 1516.949031626070109, 210.8389850543470061 ) ) ;
#37386 = CARTESIAN_POINT ( 'NONE',  ( -9.791236033121871074, 1446.818000420939825, 212.2240223532789969 ) ) ;
#37387 = CARTESIAN_POINT ( 'NONE',  ( 11.60004869885203860, 1428.965959225140750, 137.0999999980979851 ) ) ;
#37388 = CARTESIAN_POINT ( 'NONE',  ( -15.21150735940000054, 1425.420275960830168, 190.1564087504980023 ) ) ;
#37389 = AXIS2_PLACEMENT_3D ( 'NONE', #40265, #82273, #74448 ) ;
#37390 = EDGE_CURVE ( 'NONE', #99485, #59125, #106483, .T. ) ;
#37391 = DIRECTION ( 'NONE',  ( -1.913759484722300243E-19, 1.000000000000000000, -1.836968204960139822E-16 ) ) ;
#37392 = B_SPLINE_SURFACE_WITH_KNOTS ( 'NONE', 5, 5, ( 
 ( #37114, #86962, #27613, #10253, #70215, #78573 ),
 ( #88090, #36024, #79689, #11377, #19755, #44992 ),
 ( #71315, #35460, #104319, #1888, #95920, #45549 ),
 ( #79139, #52834, #2448, #69650, #105429, #28163 ),
 ( #36564, #104873, #62351, #9701, #96475, #28718 ),
 ( #60692, #53956, #26496, #18091, #103771, #94815 ),
 ( #43869, #78012, #27073, #61257, #95372, #18636 ),
 ( #76704, #84550, #33579, #17, #34698, #33038 ),
 ( #67227, #68890, #50965, #69439, #68336, #94596 ),
 ( #103554, #110304, #16220, #9496, #59379, #51509 ),
 ( #101323, #59931, #85642, #17314, #52072, #85093 ),
 ( #86205, #8942, #43115, #43663, #35255, #93491 ),
 ( #25729, #24613, #77274, #58808, #77815, #1124 ),
 ( #34151, #572, #67771, #102443, #94048, #92948 ),
 ( #26857, #102992, #41462, #50424, #16762, #92387 ),
 ( #8384, #42553, #75624, #26289, #60478, #15660 ),
 ( #76156, #17875, #49864, #83998, #7298, #109758 ),
 ( #7839, #42007, #101884, #25175, #32129, #108282 ),
 ( #22583, #98774, #100431, #82540, #100967, #99863 ),
 ( #57899, #73602, #66314, #23714, #90925, #83623 ),
 ( #6920, #92034, #81404, #49498, #15306, #41076 ),
 ( #13097, #57362, #83084, #5270, #109403, #22036 ),
 ( #13641, #91486, #56233, #6377, #90363, #75254 ),
 ( #40523, #31569, #74701, #65197, #23160, #14766 ) ),
 .UNSPECIFIED., .F., .F., .F.,
 ( 6, 3, 3, 3, 3, 3, 3, 6 ),
 ( 6, 6 ),
 ( 7.502205049999999709, 15.58712854470000053, 20.12010233590000041, 26.07035490390000021, 28.80892602879999842, 30.17821159120000019, 30.86285437249999930, 31.55357349654520149 ),
 ( -1.110223024629999900E-16, 53.14935204510580036 ),
 .UNSPECIFIED. ) ;
#37393 = ORIENTED_EDGE ( 'NONE', *, *, #64413, .F. ) ;
#37394 = CARTESIAN_POINT ( 'NONE',  ( -14.45760366698473476, 1416.831922872548603, 221.3918072960863128 ) ) ;
#37395 = CARTESIAN_POINT ( 'NONE',  ( 2.872208710164999790, 1517.145312756229941, 201.7840522196070197 ) ) ;
#37396 = AXIS2_PLACEMENT_3D ( 'NONE', #94209, #67949, #68496 ) ;
#37397 = AXIS2_PLACEMENT_3D ( 'NONE', #58618, #4888, #39029 ) ;
#37398 = LINE ( 'NONE', #95644, #87482 ) ;
#37399 = CARTESIAN_POINT ( 'NONE',  ( -8.831974440303309137, 1439.830871220620111, 206.5957406833990149 ) ) ;
#37400 = ORIENTED_EDGE ( 'NONE', *, *, #711, .F. ) ;
#37401 = CARTESIAN_POINT ( 'NONE',  ( -17.06173606976129875, 1410.334726962669947, 270.2383762330159698 ) ) ;
#37402 = CARTESIAN_POINT ( 'NONE',  ( 2.486220101774999858, 1516.939658295650133, 209.1086089184300079 ) ) ;
#37403 = CARTESIAN_POINT ( 'NONE',  ( -2.329729395510000245, 1427.373795049630189, 123.0297916884979941 ) ) ;
#37404 = FACE_OUTER_BOUND ( 'NONE', #27426, .T. ) ;
#37406 = ORIENTED_EDGE ( 'NONE', *, *, #65961, .F. ) ;
#37405 = CARTESIAN_POINT ( 'NONE',  ( -9.209502321788820112, 1366.683160837849982, 210.6218459616987957 ) ) ;
#37407 = VERTEX_POINT ( 'NONE', #17189 ) ;
#37408 = CARTESIAN_POINT ( 'NONE',  ( 42.05250925581326271, 1454.198947671722181, 269.0743982858291474 ) ) ;
#37409 = CARTESIAN_POINT ( 'NONE',  ( 11.39677682778439838, 1471.132186382680175, 209.6872533683069832 ) ) ;
#37410 = CARTESIAN_POINT ( 'NONE',  ( 3.628297850329112340, 1424.511231154813004, 184.4969362830124169 ) ) ;
#37411 = CARTESIAN_POINT ( 'NONE',  ( -2.295166956463912555, 1406.025797069441978, 266.9593544920077761 ) ) ;
#37412 = EDGE_CURVE ( 'NONE', #55324, #48821, #51385, .T. ) ;
#37413 = VECTOR ( 'NONE', #109714, 1000.000000000000000 ) ;
#37414 = CARTESIAN_POINT ( 'NONE',  ( 2.664535259099999805E-15, 1420.121162737279974, 209.1218459616989946 ) ) ;
#37415 = CARTESIAN_POINT ( 'NONE',  ( -23.64337587120000350, 1435.765690983199875, 212.0349968398180067 ) ) ;
#37416 = VECTOR ( 'NONE', #63115, 1000.000000000000114 ) ;
#37417 = CARTESIAN_POINT ( 'NONE',  ( 22.61120763781960008, 1471.946618767329937, 268.2742167358389906 ) ) ;
#37418 = CARTESIAN_POINT ( 'NONE',  ( 12.15086845379999936, 1416.067629296030191, 223.4638310076980190 ) ) ;
#37419 = DIRECTION ( 'NONE',  ( 0.9455185755993166241, -1.675808339056839216E-14, -0.3255681544571569219 ) ) ;
#37420 = CARTESIAN_POINT ( 'NONE',  ( 6.933616821004999764, 1516.548716157039962, 206.8295387017270173 ) ) ;
#37421 = ADVANCED_FACE ( 'NONE', ( #42996 ), #29484, .T. ) ;
#37422 = ORIENTED_EDGE ( 'NONE', *, *, #98140, .T. ) ;
#37423 = CARTESIAN_POINT ( 'NONE',  ( -2.023055664010000143, 1438.317420438290128, 227.6217140021989849 ) ) ;
#37424 = CARTESIAN_POINT ( 'NONE',  ( 1.471210503239640088, 1485.356266705550070, 182.0621681642270175 ) ) ;
#37425 = VERTEX_POINT ( 'NONE', #72088 ) ;
#37426 = CARTESIAN_POINT ( 'NONE',  ( 7.178570183835717877, 1456.617266911955539, 227.6511887398625618 ) ) ;
#37427 = CARTESIAN_POINT ( 'NONE',  ( -18.89905695062199698, 1416.828039266840278, 207.5749027128360069 ) ) ;
#37428 = CARTESIAN_POINT ( 'NONE',  ( -23.10251492229999926, 1410.654477831930080, 210.9078341742080056 ) ) ;
#37429 = CARTESIAN_POINT ( 'NONE',  ( -43.65213544080000219, 1390.875024450579986, 230.7167253256590129 ) ) ;
#37430 = LINE ( 'NONE', #56998, #23453 ) ;
#37431 = CARTESIAN_POINT ( 'NONE',  ( 21.12232554610000079, 1409.814838513229915, 201.9876924679279853 ) ) ;
#37432 = CARTESIAN_POINT ( 'NONE',  ( -2.500000000000000000, 1447.900699890634087, 170.5263301012278703 ) ) ;
#37433 = CARTESIAN_POINT ( 'NONE',  ( -25.45241361353140164, 1455.866316869260118, 210.5319270057530048 ) ) ;
#37434 = CARTESIAN_POINT ( 'NONE',  ( 11.72865777870000059, 1490.920838208090117, 205.3345067772989978 ) ) ;
#37435 = CARTESIAN_POINT ( 'NONE',  ( 0.5698001572631269385, 1450.893161896769925, 181.2939298055520112 ) ) ;
#37436 = AXIS2_PLACEMENT_3D ( 'NONE', #39488, #22094, #41131 ) ;
#37437 = CARTESIAN_POINT ( 'NONE',  ( 2.500000000000000000, 1439.336914142910018, 160.7446215807900103 ) ) ;
#37438 = CARTESIAN_POINT ( 'NONE',  ( -2.869693497065000098, 1517.070197312179971, 214.9093229647470196 ) ) ;
#37439 = CARTESIAN_POINT ( 'NONE',  ( 3.355801963978102709, 1523.843263703804496, 242.0624709300151380 ) ) ;
#37440 = ORIENTED_EDGE ( 'NONE', *, *, #44818, .T. ) ;
#37441 = CARTESIAN_POINT ( 'NONE',  ( -17.18995323200000058, 1417.426350748869936, 207.0509207859589935 ) ) ;
#37442 = CARTESIAN_POINT ( 'NONE',  ( -4.794426340529999386, 1463.608615258990085, 228.2108236244990280 ) ) ;
#37443 = DIRECTION ( 'NONE',  ( -1.755985294532469921E-16, 1.000000000000000000, -1.338183447452831989E-16 ) ) ;
#37444 = CARTESIAN_POINT ( 'NONE',  ( -11113.05219664940705, 50.13405481578727318, 8751.225064238135019 ) ) ;
#37445 = CARTESIAN_POINT ( 'NONE',  ( -38.21397471328810269, 1448.627478676439978, 136.4064453422460303 ) ) ;
#37446 = LINE ( 'NONE', #4930, #46037 ) ;
#37447 = CARTESIAN_POINT ( 'NONE',  ( -6.850948850460000017, 1456.378850171129898, 224.8635561661979807 ) ) ;
#37448 = CARTESIAN_POINT ( 'NONE',  ( -2.643034510968909956, 1464.878779939289871, 184.1462389150400156 ) ) ;
#37449 = CARTESIAN_POINT ( 'NONE',  ( 11.42365759299999972, 1433.140261693259845, 151.3530816855979992 ) ) ;
#37450 = CARTESIAN_POINT ( 'NONE',  ( -45.39783323183259967, 1444.747477121759857, 268.9810394864909995 ) ) ;
#37451 = CARTESIAN_POINT ( 'NONE',  ( -10.43128891525519997, 1461.757356303399774, 210.7313694234769912 ) ) ;
#37452 = CARTESIAN_POINT ( 'NONE',  ( -109.3310407770000126, 1385.265527105730143, 297.1549990084589581 ) ) ;
#37453 = CARTESIAN_POINT ( 'NONE',  ( 10.06226723659419875, 1500.632405250589954, 203.5390182893460178 ) ) ;
#37454 = ORIENTED_EDGE ( 'NONE', *, *, #15824, .T. ) ;
#37455 = CARTESIAN_POINT ( 'NONE',  ( 22.84654337450259831, 1507.483738429069717, 210.0129884701899812 ) ) ;
#37456 = CARTESIAN_POINT ( 'NONE',  ( -3.141370515551505260, 1525.159196711359755, 176.7077266983532411 ) ) ;
#37457 = CARTESIAN_POINT ( 'NONE',  ( -19.36230209990018025, 1485.611961570589528, 189.8635189068809268 ) ) ;
#37458 = CARTESIAN_POINT ( 'NONE',  ( -1.191524307911310698, 1526.382868172864164, 239.2353018730791518 ) ) ;
#37459 = CARTESIAN_POINT ( 'NONE',  ( 2.376090132089999862, 1482.817598545530018, 234.9716043272979960 ) ) ;
#37460 = AXIS2_PLACEMENT_3D ( 'NONE', #86172, #96232, #103513 ) ;
#37461 = CARTESIAN_POINT ( 'NONE',  ( -16.41917143159986026, 1420.127254725630564, 208.8252928080606807 ) ) ;
#37462 = CARTESIAN_POINT ( 'NONE',  ( -15.36975367949999871, 1507.878415112629909, 231.4074980585979802 ) ) ;
#37463 = CARTESIAN_POINT ( 'NONE',  ( -22.73541431592179762, 1383.850630038179816, 222.0790162367429730 ) ) ;
#37464 = CARTESIAN_POINT ( 'NONE',  ( -3.116127437694289792, 1509.034538005060085, 204.6344859856109792 ) ) ;
#37465 = CARTESIAN_POINT ( 'NONE',  ( 5.555191409685329873, 1422.974801224869907, 110.9492657717959929 ) ) ;
#37466 = DIRECTION ( 'NONE',  ( 0.000000000000000000, 0.000000000000000000, 1.000000000000000000 ) ) ;
#37467 = CARTESIAN_POINT ( 'NONE',  ( 1.422559892400000026, 1466.356769739329820, 235.0198037906980062 ) ) ;
#37469 = EDGE_LOOP ( 'NONE', ( #16287, #101346, #84185, #25871 ) ) ;
#37468 = CARTESIAN_POINT ( 'NONE',  ( -4.491293135916502699, 1508.884207228266632, 212.6094329811311354 ) ) ;
#37470 = CARTESIAN_POINT ( 'NONE',  ( -1.107844858910000063, 1451.282733439329832, 183.1474623122980177 ) ) ;
#37471 = CARTESIAN_POINT ( 'NONE',  ( -6.354406034210000165, 1384.502204350209922, 199.7451528500290010 ) ) ;
#37472 = CARTESIAN_POINT ( 'NONE',  ( -25.78156655170059608, 1509.813372604039841, 223.1298223243570078 ) ) ;
#37474 = VERTEX_POINT ( 'NONE', #20519 ) ;
#37473 = CARTESIAN_POINT ( 'NONE',  ( -31.52384642519460911, 1525.730671215514576, 217.0357139665296700 ) ) ;
#37475 = CARTESIAN_POINT ( 'NONE',  ( -14.38098269158279940, 1422.143816687460003, 196.2925691453790193 ) ) ;
#37476 = ORIENTED_EDGE ( 'NONE', *, *, #44754, .T. ) ;
#37477 = PRODUCT_DEFINITION_SHAPE ( 'NONE', 'NONE',  #110837 ) ;
#37478 = CARTESIAN_POINT ( 'NONE',  ( -9.233185807659999966, 1388.318973794420117, 217.5719053405290140 ) ) ;
#37479 = CARTESIAN_POINT ( 'NONE',  ( -29.30029655192934257, 1525.907212628473644, 221.3719603026177367 ) ) ;
#37480 = DIRECTION ( 'NONE',  ( 0.8539859765994181062, 0.000000000000000000, -0.5202960232132650686 ) ) ;
#37481 = CIRCLE ( 'NONE', #19641, 1.999999999999997780 ) ;
#37482 = CARTESIAN_POINT ( 'NONE',  ( 23.55007129670912036, 1410.927094386046747, 207.7715154849149144 ) ) ;
#37483 = FACE_OUTER_BOUND ( 'NONE', #101686, .T. ) ;
#37484 = CARTESIAN_POINT ( 'NONE',  ( -10.06543680052650203, 1473.157550441890180, 207.3953233922799768 ) ) ;
#37485 = CARTESIAN_POINT ( 'NONE',  ( 12.85129650592379846, 1409.361837545100116, 216.7469526318749899 ) ) ;
#37486 = CARTESIAN_POINT ( 'NONE',  ( -7.966153717961919511, 1384.908122895999895, 199.4893165508340189 ) ) ;
#37487 = CARTESIAN_POINT ( 'NONE',  ( -88.24164336956870613, 1385.187133139050275, 291.4137164603869792 ) ) ;
#37488 = CARTESIAN_POINT ( 'NONE',  ( -18.41416944129999678, 1437.064010179910156, 192.2764675452979759 ) ) ;
#37489 = CARTESIAN_POINT ( 'NONE',  ( 24.02863916850529691, 1507.902931906480035, 195.9323055859989893 ) ) ;
#37490 = CIRCLE ( 'NONE', #19573, 0.2999999999999669598 ) ;
#37491 = CARTESIAN_POINT ( 'NONE',  ( 10.91851345119660088, 1489.922152752260217, 208.2558192066160245 ) ) ;
#37492 = ORIENTED_EDGE ( 'NONE', *, *, #106736, .F. ) ;
#37493 = ORIENTED_EDGE ( 'NONE', *, *, #61812, .F. ) ;
#37494 = CARTESIAN_POINT ( 'NONE',  ( -11.53151684693130008, 1415.184612914939862, 195.3895478472830121 ) ) ;
#37495 = FACE_OUTER_BOUND ( 'NONE', #2851, .T. ) ;
#37496 = CARTESIAN_POINT ( 'NONE',  ( 31.15391034571117146, 1461.365240553406920, 269.4835205282784045 ) ) ;
#37497 = CARTESIAN_POINT ( 'NONE',  ( 11.48693412901199906, 1427.591069643789979, 209.4851071871740089 ) ) ;
#37498 = CARTESIAN_POINT ( 'NONE',  ( 3.911218387687235953, 1414.913060387329779, 224.8752140912787354 ) ) ;
#37499 = CARTESIAN_POINT ( 'NONE',  ( 32.85805783624305576, 1523.678648413191695, 201.0453875934054224 ) ) ;
#37500 = CARTESIAN_POINT ( 'NONE',  ( -1.197234916440000019, 1467.463882650130017, 182.9502258106980150 ) ) ;
#37501 = CARTESIAN_POINT ( 'NONE',  ( -10.02185219040722153, 1364.916310432309956, 210.6218459616991936 ) ) ;
#37502 = CARTESIAN_POINT ( 'NONE',  ( -26.76690114070098758, 1436.758409284090476, 136.7827424958600204 ) ) ;
#37503 = CARTESIAN_POINT ( 'NONE',  ( -7.725990199955000470, 1517.181921232829836, 206.6366402828969910 ) ) ;
#37504 = CIRCLE ( 'NONE', #53691, 1.000000000000001554 ) ;
#37505 = CARTESIAN_POINT ( 'NONE',  ( -12.96903165645690059, 1434.787792369200133, 149.4958389638820222 ) ) ;
#37506 = CARTESIAN_POINT ( 'NONE',  ( -8.594535950999999230, 1385.265555896049818, 218.6506679551489754 ) ) ;
#37507 = B_SPLINE_SURFACE_WITH_KNOTS ( 'NONE', 4, 5, ( 
 ( #33857, #69712, #68048, #837, #8648, #59632 ),
 ( #85924, #41713, #9227, #77533, #101596, #110572 ),
 ( #7559, #75873, #15933, #42825, #59088, #8101 ),
 ( #43385, #50136, #25990, #17022, #93210, #16479 ),
 ( #35520, #102695, #103832, #52352, #34418, #34963 ) ),
 .UNSPECIFIED., .F., .F., .F.,
 ( 5, 5 ),
 ( 6, 6 ),
 ( 6.734755223250000533, 23.51228018150000310 ),
 ( -2.775557561569999727E-17, 1.000000000000000000 ),
 .UNSPECIFIED. ) ;
#37508 = CARTESIAN_POINT ( 'NONE',  ( 1.341974321609999743, 1416.832348283729971, 190.1632194751979910 ) ) ;
#37509 = CARTESIAN_POINT ( 'NONE',  ( 2.257543447819999827, 1497.637321272190093, 197.6769954692990154 ) ) ;
#37510 = CARTESIAN_POINT ( 'NONE',  ( -16.22971081790149839, 1485.231972063210151, 229.4479590017650139 ) ) ;
#37511 = CARTESIAN_POINT ( 'NONE',  ( 41.63873300600299387, 1444.030015486870070, 135.9017893062919882 ) ) ;
#37512 = ORIENTED_EDGE ( 'NONE', *, *, #38968, .F. ) ;
#37513 = ADVANCED_FACE ( 'NONE', ( #81001 ), #109010, .F. ) ;
#37514 = CARTESIAN_POINT ( 'NONE',  ( 7.132053334199999206, 1405.830928060730230, 267.2558864130979828 ) ) ;
#37515 = CARTESIAN_POINT ( 'NONE',  ( -26.91706399349999757, 1488.687396145830007, 206.2930393126480055 ) ) ;
#37517 = CARTESIAN_POINT ( 'NONE',  ( -0.7038401922759969231, 1507.336008941910222, 231.8508856179180100 ) ) ;
#37516 = CARTESIAN_POINT ( 'NONE',  ( -10.04958432075110153, 1425.197681561259969, 97.53048915649959838 ) ) ;
#37518 = DIRECTION ( 'NONE',  ( 0.000000000000000000, -1.000000000000000000, 0.000000000000000000 ) ) ;
#37519 = AXIS2_PLACEMENT_3D ( 'NONE', #48077, #46985, #30147 ) ;
#37520 = CARTESIAN_POINT ( 'NONE',  ( -5.038677021079999818, 1414.987262864929789, 244.5742075775979743 ) ) ;
#37521 = CARTESIAN_POINT ( 'NONE',  ( 2.137002880650000325, 1486.596861473290119, 219.7231104124990111 ) ) ;
#37522 = ADVANCED_FACE ( 'NONE', ( #21068 ), #56211, .T. ) ;
#37523 = CARTESIAN_POINT ( 'NONE',  ( 19.75716384889999944, 1473.226869026490021, 205.2905475991589981 ) ) ;
#37524 = CARTESIAN_POINT ( 'NONE',  ( 32.73687869649999982, 1451.769863600429971, 134.7502305315980209 ) ) ;
#37525 = ORIENTED_EDGE ( 'NONE', *, *, #82945, .F. ) ;
#37526 = CARTESIAN_POINT ( 'NONE',  ( -2.500000000000000000, 1429.342233201230101, 157.2075084771979903 ) ) ;
#37527 = CARTESIAN_POINT ( 'NONE',  ( 11.56080089750725115, 1512.916366990813913, 225.4987921079732018 ) ) ;
#37528 = CARTESIAN_POINT ( 'NONE',  ( 5.943024939599999001, 1509.160954526729938, 238.4862494313980221 ) ) ;
#37529 = EDGE_LOOP ( 'NONE', ( #71167, #36005, #66771, #93879, #84572 ) ) ;
#37530 = ORIENTED_EDGE ( 'NONE', *, *, #4050, .F. ) ;
#37531 = CARTESIAN_POINT ( 'NONE',  ( -10.56484691688378597, 1423.845928272108267, 137.4577028072829421 ) ) ;
#37532 = CARTESIAN_POINT ( 'NONE',  ( -22.81024108693009822, 1409.709601909520188, 208.9207945697700097 ) ) ;
#37533 = EDGE_LOOP ( 'NONE', ( #22610, #77926, #9260, #11699 ) ) ;
#37534 = CARTESIAN_POINT ( 'NONE',  ( -3.660374594542989968, 1507.478316997890033, 221.4607952786410010 ) ) ;
#37535 = B_SPLINE_CURVE_WITH_KNOTS ( 'NONE', 3,
 ( #107122, #37174, #89769, #13040 ),
 .UNSPECIFIED., .F., .F.,
 ( 4, 4 ),
 ( 0.000000000000000000, 0.0002960034161023847310 ),
 .UNSPECIFIED. ) ;
#37536 = CARTESIAN_POINT ( 'NONE',  ( 4.500000000000000000, 1425.929641636930000, 183.3886486283980162 ) ) ;
#37537 = CARTESIAN_POINT ( 'NONE',  ( 4.219439073160000220, 1441.595895977600094, 127.8666744532979891 ) ) ;
#37538 = CARTESIAN_POINT ( 'NONE',  ( -1.976821269320000019, 1489.062954066330121, 236.2429157177979846 ) ) ;
#37539 = CARTESIAN_POINT ( 'NONE',  ( 5.409864550977149911, 1440.893826613949841, 154.8143284419219867 ) ) ;
#37540 = VERTEX_POINT ( 'NONE', #108406 ) ;
#37541 = CARTESIAN_POINT ( 'NONE',  ( 11.73643181629999965, 1426.280401702730160, 144.1638243103979846 ) ) ;
#37542 = CARTESIAN_POINT ( 'NONE',  ( -12.02797161415869986, 1415.088136167450102, 221.1177398843049957 ) ) ;
#37543 = CARTESIAN_POINT ( 'NONE',  ( 14.91364890520000053, 1485.710536188930064, 225.0739173850980137 ) ) ;
#37544 = ORIENTED_EDGE ( 'NONE', *, *, #6881, .T. ) ;
#37545 = CARTESIAN_POINT ( 'NONE',  ( 6.549762446985000430, 1516.729202374750002, 204.5030968636170030 ) ) ;
#37546 = ORIENTED_EDGE ( 'NONE', *, *, #42400, .F. ) ;
#37547 = CARTESIAN_POINT ( 'NONE',  ( 11.83309251696740105, 1430.099177678210026, 149.5098043249829800 ) ) ;
#37548 = B_SPLINE_CURVE_WITH_KNOTS ( 'NONE', 5,
 ( #53495, #18744, #339, #10360, #102209, #94925 ),
 .UNSPECIFIED., .F., .F.,
 ( 6, 6 ),
 ( 0.000000000000000000, 1.000000000000000000 ),
 .UNSPECIFIED. ) ;
#37549 = AXIS2_PLACEMENT_3D ( 'NONE', #14652, #108161, #74028 ) ;
#37550 = FACE_OUTER_BOUND ( 'NONE', #31966, .T. ) ;
#37551 = ORIENTED_EDGE ( 'NONE', *, *, #10943, .F. ) ;
#37552 = VERTEX_POINT ( 'NONE', #47952 ) ;
#37553 = CARTESIAN_POINT ( 'NONE',  ( -103.5801209296959939, 1379.883073482990085, 303.9981235976169955 ) ) ;
#37554 = CARTESIAN_POINT ( 'NONE',  ( 10.44087869485973030, 1517.151704408390060, 212.8912867333128531 ) ) ;
#37555 = CARTESIAN_POINT ( 'NONE',  ( 7.795806952825950376, 1499.846699301729814, 200.6023917261699978 ) ) ;
#37556 = CARTESIAN_POINT ( 'NONE',  ( -7.344976460507339766, 1469.674713007590071, 216.6639152125200098 ) ) ;
#37557 = CARTESIAN_POINT ( 'NONE',  ( 20.52137544053379870, 1452.196438165939981, 142.6117432215559973 ) ) ;
#37558 = VECTOR ( 'NONE', #52004, 1000.000000000000227 ) ;
#37559 = CARTESIAN_POINT ( 'NONE',  ( 1.438079373956610008, 1409.221132550520224, 270.3713132426580046 ) ) ;
#37560 = CARTESIAN_POINT ( 'NONE',  ( -21.84020450222076448, 1512.187213306747481, 183.2638850454220858 ) ) ;
#37561 = CARTESIAN_POINT ( 'NONE',  ( 5.402232622379999017E-16, 1413.913060387330006, 209.1218459616979999 ) ) ;
#37562 = DIRECTION ( 'NONE',  ( -9.066331650111889066E-17, 1.000000000000000000, -7.714096702464409664E-17 ) ) ;
#37564 = CARTESIAN_POINT ( 'NONE',  ( 15.89248692530000007, 1471.309462467230105, 194.8090275957980282 ) ) ;
#37563 = CARTESIAN_POINT ( 'NONE',  ( -18.26050052379999755, 1504.444625823090064, 209.3988868026209786 ) ) ;
#37565 = CARTESIAN_POINT ( 'NONE',  ( -54.44063311572099906, 1379.743533639908492, 254.0790799865290239 ) ) ;
#37566 = CARTESIAN_POINT ( 'NONE',  ( 17.98175490010330080, 1423.057749139549969, 225.1621279517349876 ) ) ;
#37567 = CARTESIAN_POINT ( 'NONE',  ( -7.521073069125000288, 1513.760531203550045, 202.2873616486669732 ) ) ;
#37568 = ORIENTED_EDGE ( 'NONE', *, *, #108341, .T. ) ;
#37569 = CARTESIAN_POINT ( 'NONE',  ( 17.87874083579999862, 1415.075539390429867, 265.6112251771979800 ) ) ;
#37570 = VECTOR ( 'NONE', #89988, 1000.000000000000000 ) ;
#37571 = CARTESIAN_POINT ( 'NONE',  ( 21.84020450222037724, 1523.382868172864164, 183.2638850454218016 ) ) ;
#37572 = CARTESIAN_POINT ( 'NONE',  ( -60.96689588341559585, 1385.061429299729980, 282.5775017028749971 ) ) ;
#37573 = CARTESIAN_POINT ( 'NONE',  ( 5.300910123630000470, 1506.315325122790000, 219.5100740960989754 ) ) ;
#37574 = CARTESIAN_POINT ( 'NONE',  ( 39.26193983301609336, 1423.042221552809906, 269.8021829593399730 ) ) ;
#37576 = ORIENTED_EDGE ( 'NONE', *, *, #62503, .T. ) ;
#37575 = CARTESIAN_POINT ( 'NONE',  ( -17.70335225402379820, 1419.745088214420093, 206.7394850893050204 ) ) ;
#37577 = CARTESIAN_POINT ( 'NONE',  ( -15.92643154291071461, 1416.091409276738204, 209.7524194240169777 ) ) ;
#37578 = CARTESIAN_POINT ( 'NONE',  ( 19.84405992990000200, 1475.251132489289830, 205.2734896568690033 ) ) ;
#37579 = CARTESIAN_POINT ( 'NONE',  ( -0.8280578839340340114, 1450.871635902641628, 154.2446588023700542 ) ) ;
#37580 = CARTESIAN_POINT ( 'NONE',  ( 14.10835366113500022, 1513.596256836700150, 225.7720208619669791 ) ) ;
#37581 = CARTESIAN_POINT ( 'NONE',  ( -10.45459916649999954, 1441.816060358160030, 186.8492846416980058 ) ) ;
#37582 = CARTESIAN_POINT ( 'NONE',  ( 6.560537731721620247, 1509.222499095490093, 179.2361269201259972 ) ) ;
#37583 = CARTESIAN_POINT ( 'NONE',  ( 7.294923696395279933, 1458.268530975320118, 201.0098625615580090 ) ) ;
#37584 = CARTESIAN_POINT ( 'NONE',  ( -14.59882275830000076, 1475.513060387329915, 223.7206687204979971 ) ) ;
#37585 = CARTESIAN_POINT ( 'NONE',  ( 16.58222327440000399, 1412.750976071529976, 226.6462158149980155 ) ) ;
#37586 = CARTESIAN_POINT ( 'NONE',  ( -0.4346943098025670138, 1517.051704408590012, 216.8444262844809884 ) ) ;
#37587 = CARTESIAN_POINT ( 'NONE',  ( -20.60985939166187464, 1525.581535527370988, 236.5072125268898731 ) ) ;
#37588 = VECTOR ( 'NONE', #58971, 1000.000000000000227 ) ;
#37589 = CARTESIAN_POINT ( 'NONE',  ( -3.269184946495000244, 1516.940296199220029, 206.8376465686969823 ) ) ;
#37590 = CARTESIAN_POINT ( 'NONE',  ( 45.57495757519999557, 1434.881052582139773, 268.2238934247979500 ) ) ;
#37591 = CARTESIAN_POINT ( 'NONE',  ( -18.39324904740000122, 1410.479025241530053, 224.0575692145980042 ) ) ;
#37592 = B_SPLINE_CURVE_WITH_KNOTS ( 'NONE', 5,
 ( #68748, #102851, #94451, #80988, #98331, #73142, #55812, #30580, #90478 ),
 .UNSPECIFIED., .F., .F.,
 ( 6, 3, 6 ),
 ( 0.000000000000000000, 0.5447623589902206298, 1.000000000000000000 ),
 .UNSPECIFIED. ) ;
#37593 = CARTESIAN_POINT ( 'NONE',  ( 17.61383487560000205, 1435.259801188919937, 146.8137243960979959 ) ) ;
#37594 = CARTESIAN_POINT ( 'NONE',  ( 22.47117279520000110, 1488.581167089130076, 194.6265784292980072 ) ) ;
#37595 = CARTESIAN_POINT ( 'NONE',  ( 29.67496808539234365, 1509.980355513194809, 207.9080589769481833 ) ) ;
#37596 = DIRECTION ( 'NONE',  ( 0.02091224828123190022, 0.9990482215818557998, 0.03827961371219716635 ) ) ;
#37597 = CARTESIAN_POINT ( 'NONE',  ( -21.85618413279999572, 1471.634021946630128, 266.7712522008980613 ) ) ;
#37598 = CARTESIAN_POINT ( 'NONE',  ( 12.51530806464030121, 1427.043259357019906, 206.3792954839019842 ) ) ;
#37599 = CARTESIAN_POINT ( 'NONE',  ( -39.85331543310000058, 1441.120390181860103, 136.8371630922980273 ) ) ;
#37600 = CARTESIAN_POINT ( 'NONE',  ( -8.971317772902260401, 1408.181544129620079, 199.2698409955270051 ) ) ;
#37601 = CARTESIAN_POINT ( 'NONE',  ( -12.58432885909999932, 1415.426210663629945, 196.9819687637979939 ) ) ;
#37602 = VECTOR ( 'NONE', #10094, 1000.000000000000000 ) ;
#37603 = CARTESIAN_POINT ( 'NONE',  ( -12.88966618989999979, 1442.875255404869904, 186.4032537866980022 ) ) ;
#37604 = CARTESIAN_POINT ( 'NONE',  ( 9.813597453882589861, 1516.551188145990182, 214.6853868983759810 ) ) ;
#37605 = CARTESIAN_POINT ( 'NONE',  ( 3.992841683700380617, 1455.996149397760064, 218.9659736531049816 ) ) ;
#37606 = CARTESIAN_POINT ( 'NONE',  ( -27.70478114339999820, 1435.630643383260121, 136.1390072790979957 ) ) ;
#37607 = DIRECTION ( 'NONE',  ( 0.9455185755993178454, 0.000000000000000000, -0.3255681544571539243 ) ) ;
#37608 = VERTEX_POINT ( 'NONE', #92154 ) ;
#37609 = CARTESIAN_POINT ( 'NONE',  ( 6.191282256226939396, 1510.848430436206854, 216.5799282118206008 ) ) ;
#37610 = CARTESIAN_POINT ( 'NONE',  ( -6.697668172239800377, 1409.146948113720100, 222.5083809332480200 ) ) ;
#37611 = CARTESIAN_POINT ( 'NONE',  ( 13.10742788021580019, 1414.941152333586842, 197.9471227725614426 ) ) ;
#37612 = CARTESIAN_POINT ( 'NONE',  ( -13.35927778977159974, 1507.978183412450107, 209.3898014577139861 ) ) ;
#37613 = CARTESIAN_POINT ( 'NONE',  ( -4.065119941006720694, 1421.084427985996399, 137.4065821739406772 ) ) ;
#37614 = CARTESIAN_POINT ( 'NONE',  ( -37.54399022510000350, 1461.570446756029924, 266.4251594875980231 ) ) ;
#37615 = CARTESIAN_POINT ( 'NONE',  ( -29.70307915522685960, 1525.408327360766862, 196.2982788325003867 ) ) ;
#37616 = CARTESIAN_POINT ( 'NONE',  ( 9.722207004026980570, 1428.114070666289763, 212.2005352792010058 ) ) ;
#37617 = CARTESIAN_POINT ( 'NONE',  ( -26.88792329530000202, 1508.603612637529977, 212.0174590681980078 ) ) ;
#37618 = CARTESIAN_POINT ( 'NONE',  ( -87.62118790240700150, 1384.623622514330009, 307.8351744068140192 ) ) ;
#37619 = CARTESIAN_POINT ( 'NONE',  ( -39.59907641771560094, 1384.988928994350090, 212.5044586702960032 ) ) ;
#37620 = CARTESIAN_POINT ( 'NONE',  ( -5.473267998913230237, 1374.913303669990000, 214.9198275724610028 ) ) ;
#37621 = CARTESIAN_POINT ( 'NONE',  ( 14.17095083369999919, 1415.425644477329797, 219.3842840303979926 ) ) ;
#37622 = CARTESIAN_POINT ( 'NONE',  ( 15.30965536770000135, 1495.931236920830088, 224.3053488962979998 ) ) ;
#37624 = VERTEX_POINT ( 'NONE', #31688 ) ;
#37623 = CARTESIAN_POINT ( 'NONE',  ( 3.829620175029999629, 1515.551704176389876, 207.2788819937790095 ) ) ;
#37625 = CARTESIAN_POINT ( 'NONE',  ( -8.156119896610000808, 1384.930225391789918, 199.6467426484390160 ) ) ;
#37626 = CARTESIAN_POINT ( 'NONE',  ( 2.372478608332516892, 1512.187213306747481, 243.3440112565233449 ) ) ;
#37627 =( BOUNDED_CURVE ( )  B_SPLINE_CURVE ( 3, ( #84957, #102858, #94461, #58138 ),
 .UNSPECIFIED., .F., .T. ) 
 B_SPLINE_CURVE_WITH_KNOTS ( ( 4, 4 ),
 ( 4.131751671967750283, 5.293027011176480556 ),
 .UNSPECIFIED. ) 
 CURVE ( )  GEOMETRIC_REPRESENTATION_ITEM ( )  RATIONAL_B_SPLINE_CURVE ( ( 1.000000000000000000, 0.8907420144464277545, 0.8907420144464277545, 1.000000000000000000 ) ) 
 REPRESENTATION_ITEM ( '' )  );
#37628 = CARTESIAN_POINT ( 'NONE',  ( 3.037408418089064810, 1369.431655480266272, 210.6218459616999041 ) ) ;
#37629 = CARTESIAN_POINT ( 'NONE',  ( -22.03465957474533354, 1522.382868172863937, 235.4136513321633117 ) ) ;
#37630 = CARTESIAN_POINT ( 'NONE',  ( 1.758980145960000074, 1423.182207406469843, 192.9748505280989832 ) ) ;
#37631 = CARTESIAN_POINT ( 'NONE',  ( 22.50003437009999629, 1409.698778901130254, 210.1517532643880202 ) ) ;
#37632 = B_SPLINE_SURFACE_WITH_KNOTS ( 'NONE', 5, 5, ( 
 ( #96520, #62965, #97077, #41006, #90858, #58377 ),
 ( #100893, #30401, #99243, #48889, #14145, #48332 ),
 ( #4661, #64592, #24189, #66248, #83017, #98711 ),
 ( #75184, #15770, #6309, #109334, #57298, #13581 ),
 ( #14700, #32617, #40455, #66793, #49972, #15238 ),
 ( #22520, #92503, #90300, #30955, #38799, #107113 ) ),
 .UNSPECIFIED., .F., .F., .F.,
 ( 6, 6 ),
 ( 6, 6 ),
 ( 5.893388375715320038, 9.819929736134680454 ),
 ( 0.000000000000000000, 0.5002947206946759540 ),
 .UNSPECIFIED. ) ;
#37633 = CARTESIAN_POINT ( 'NONE',  ( -106.4903149258919939, 1391.913060387289988, 305.1044923263290229 ) ) ;
#37634 = CARTESIAN_POINT ( 'NONE',  ( 18.96326924193710184, 1459.304563651490071, 220.4161041720870173 ) ) ;
#37635 = CARTESIAN_POINT ( 'NONE',  ( -16.57624646909999910, 1421.408089520330122, 226.9966418715980012 ) ) ;
#37637 = CARTESIAN_POINT ( 'NONE',  ( -11.68514080771860009, 1426.730168479550002, 140.4580954921360103 ) ) ;
#37636 = CARTESIAN_POINT ( 'NONE',  ( -11.87490713740000103, 1433.006767100669776, 150.3951466367980174 ) ) ;
#37638 = CARTESIAN_POINT ( 'NONE',  ( 0.3110986828880000221, 1414.379630184029793, 233.4276179574980006 ) ) ;
#37639 = DIRECTION ( 'NONE',  ( -0.9999999999532290795, -9.321873569642529338E-06, 2.577697155618075134E-06 ) ) ;
#37640 = VECTOR ( 'NONE', #47146, 1000.000000000000114 ) ;
#37641 = CYLINDRICAL_SURFACE ( 'NONE', #93743, 2.000000000000003553 ) ;
#37642 = DIRECTION ( 'NONE',  ( -0.8236474686107853049, 0.5669078173018522460, -0.01484500364079620674 ) ) ;
#37643 = CARTESIAN_POINT ( 'NONE',  ( -9.934709065799999905, 1365.494406819940195, 210.6218459616991936 ) ) ;
#37644 = CARTESIAN_POINT ( 'NONE',  ( -6.559168674874999105, 1516.960844870249957, 204.1192525727769862 ) ) ;
#37645 = CARTESIAN_POINT ( 'NONE',  ( -23.74108753817469974, 1436.296634041249945, 212.5883363871789982 ) ) ;
#37646 = CARTESIAN_POINT ( 'NONE',  ( -15.48464347335860047, 1485.614289314720054, 187.1168877932479973 ) ) ;
#37647 = AXIS2_PLACEMENT_3D ( 'NONE', #17100, #33374, #32293 ) ;
#37648 = CARTESIAN_POINT ( 'NONE',  ( 1776.830386524950200, 5182.767774292099602, -8872.362978888699217 ) ) ;
#37649 = CARTESIAN_POINT ( 'NONE',  ( -4.283857371189049523, 1440.956241081810049, 155.9231041381889895 ) ) ;
#37651 = ORIENTED_EDGE ( 'NONE', *, *, #63800, .F. ) ;
#37650 = CARTESIAN_POINT ( 'NONE',  ( -68.44382096765579604, 1379.747259237049775, 280.0252539470139936 ) ) ;
#37652 = VERTEX_POINT ( 'NONE', #22161 ) ;
#37653 = CARTESIAN_POINT ( 'NONE',  ( 27.96002538619999811, 1508.622315501829917, 211.1985762216579872 ) ) ;
#37654 = ORIENTED_EDGE ( 'NONE', *, *, #56365, .T. ) ;
#37655 = CARTESIAN_POINT ( 'NONE',  ( 20.21024070146847151, 1526.107876515966609, 184.5539461604345775 ) ) ;
#37656 = CARTESIAN_POINT ( 'NONE',  ( -109.9855944279999989, 1384.926148861439970, 311.4562326602589906 ) ) ;
#37658 = LINE ( 'NONE', #55582, #14675 ) ;
#37657 = CARTESIAN_POINT ( 'NONE',  ( 1.580871945720000005, 1426.963505220229990, 133.6118001900980232 ) ) ;
#37659 = CARTESIAN_POINT ( 'NONE',  ( 11.97724519069999971, 1441.600846913620217, 147.6096801420980000 ) ) ;
#37660 = CARTESIAN_POINT ( 'NONE',  ( -25.30806138896770108, 1450.980851669160074, 137.3985563705309971 ) ) ;
#37661 = CARTESIAN_POINT ( 'NONE',  ( 0.8333005674559990084, 1467.257208946589799, 220.1998364950989924 ) ) ;
#37662 = CARTESIAN_POINT ( 'NONE',  ( 5.842743512439999343, 1410.494458809630032, 231.1215182491980045 ) ) ;
#37663 = CARTESIAN_POINT ( 'NONE',  ( 9.424585447077209466, 1482.249723839049921, 215.0732731526550197 ) ) ;
#37664 = ADVANCED_FACE ( 'NONE', ( #15426 ), #40095, .F. ) ;
#37665 = CARTESIAN_POINT ( 'NONE',  ( -1.119439127814999990, 1517.026534522949987, 212.3908711059869745 ) ) ;
#37666 = CARTESIAN_POINT ( 'NONE',  ( 41.66177311458239529, 1443.657316189979838, 134.0999999982009854 ) ) ;
#37667 = AXIS2_PLACEMENT_3D ( 'NONE', #40760, #66548, #109625 ) ;
#37668 = CARTESIAN_POINT ( 'NONE',  ( 17.76546875260000036, 1430.865606781589804, 204.9340536459789917 ) ) ;
#37669 = ORIENTED_EDGE ( 'NONE', *, *, #42486, .F. ) ;
#37670 = CARTESIAN_POINT ( 'NONE',  ( 18.99432114591609988, 1459.501257801400243, 220.3864165788380092 ) ) ;
#37671 = CYLINDRICAL_SURFACE ( 'NONE', #10119, 0.4999999999999449329 ) ;
#37672 = ORIENTED_EDGE ( 'NONE', *, *, #21926, .F. ) ;
#37673 = EDGE_LOOP ( 'NONE', ( #109639, #12872, #77054, #52399 ) ) ;
#37674 = EDGE_LOOP ( 'NONE', ( #63298, #107422, #52880, #93333 ) ) ;
#37675 = CARTESIAN_POINT ( 'NONE',  ( -6.096095868995000444, 1514.881364185380107, 217.1628748908970010 ) ) ;
#37676 = CARTESIAN_POINT ( 'NONE',  ( 16.53526709313100795, 1514.188985849830942, 194.8337175523576548 ) ) ;
#37677 = CIRCLE ( 'NONE', #59189, 2.000000000000003553 ) ;
#37678 = CARTESIAN_POINT ( 'NONE',  ( 13.00130910693166975, 1451.219797464038720, 150.9319667301929826 ) ) ;
#37679 = CARTESIAN_POINT ( 'NONE',  ( -2.487935121788300119, 1509.038615937200120, 204.6345961869410246 ) ) ;
#37680 = CARTESIAN_POINT ( 'NONE',  ( 10.51639688740000089, 1461.562446843690168, 209.7842554828359880 ) ) ;
#37681 = CARTESIAN_POINT ( 'NONE',  ( -17.63885398217787781, 1447.971996929747547, 217.7157177369595047 ) ) ;
#37682 = CARTESIAN_POINT ( 'NONE',  ( -68.13057759640398103, 1379.746676104469316, 278.6999125972471347 ) ) ;
#37683 = CARTESIAN_POINT ( 'NONE',  ( -0.09961128158209880956, 1464.896202565289968, 198.8671910008989983 ) ) ;
#37684 = CARTESIAN_POINT ( 'NONE',  ( 3.456073863659999912, 1414.971339025629959, 192.2203226080980016 ) ) ;
#37685 = VERTEX_POINT ( 'NONE', #90493 ) ;
#37686 = CARTESIAN_POINT ( 'NONE',  ( -0.01265822594359850006, 1516.959716008189844, 207.4120794380770292 ) ) ;
#37688 = ORIENTED_EDGE ( 'NONE', *, *, #104411, .F. ) ;
#37687 = B_SPLINE_CURVE_WITH_KNOTS ( 'NONE', 5,
 ( #49203, #83331, #6627, #79361, #60354, #26168, #26734, #9388, #9934 ),
 .UNSPECIFIED., .F., .F.,
 ( 6, 3, 6 ),
 ( -3.121899836449999910, -2.731662331479999928, 4.440892098500626162E-16 ),
 .UNSPECIFIED. ) ;
#37689 = CARTESIAN_POINT ( 'NONE',  ( 28.96304334425650140, 1440.913060387330006, 249.8538069052020205 ) ) ;
#37690 = CIRCLE ( 'NONE', #102004, 11.73843354579999954 ) ;
#37691 = CARTESIAN_POINT ( 'NONE',  ( 11.66147129757649914, 1479.066346190409831, 207.6019141534899859 ) ) ;
#37692 = ORIENTED_EDGE ( 'NONE', *, *, #94421, .T. ) ;
#37693 = CARTESIAN_POINT ( 'NONE',  ( -7.166264985072499982, 1508.551567432899901, 203.0889892476990042 ) ) ;
#37694 = CARTESIAN_POINT ( 'NONE',  ( -14.04326434459999895, 1410.776247947130059, 190.2283950358979894 ) ) ;
#37695 = CARTESIAN_POINT ( 'NONE',  ( -109.0938067140002232, 1384.498046937599838, 311.2419503292331342 ) ) ;
#37697 = DIRECTION ( 'NONE',  ( -0.01245851141472737768, -0.0004350606870917433900, -0.9999222950887373118 ) ) ;
#37696 = CARTESIAN_POINT ( 'NONE',  ( 30.51231035492518728, 1524.382868172863937, 200.0858385050239008 ) ) ;
#37698 = CARTESIAN_POINT ( 'NONE',  ( 22.08732799627270182, 1410.055779663399790, 206.2710209263929926 ) ) ;
#37699 = B_SPLINE_CURVE_WITH_KNOTS ( 'NONE', 3,
 ( #52251, #67952, #93115, #61224, #16385, #95338 ),
 .UNSPECIFIED., .F., .F.,
 ( 4, 2, 4 ),
 ( 9.026196891026570071E-07, 0.4991090056710880130, 0.9980282895626380046 ),
 .UNSPECIFIED. ) ;
#37700 = CARTESIAN_POINT ( 'NONE',  ( -122.4487580624700058, 1378.528619065190014, 299.2784868977390147 ) ) ;
#37701 = CARTESIAN_POINT ( 'NONE',  ( 2.149988386126029882E-09, 1405.989059316979819, 266.9611530767110139 ) ) ;
#37702 = CARTESIAN_POINT ( 'NONE',  ( 2.140036995326180090E-16, 1390.913060387289988, 209.1218459572589836 ) ) ;
#37704 = EDGE_CURVE ( 'NONE', #61557, #51642, #54669, .T. ) ;
#37703 = FACE_OUTER_BOUND ( 'NONE', #77599, .T. ) ;
#37706 = CARTESIAN_POINT ( 'NONE',  ( -2.889942526720000071, 1491.528343827289973, 188.3843089064990011 ) ) ;
#37705 = CARTESIAN_POINT ( 'NONE',  ( 7.749473586019999694, 1464.901857590230065, 233.2267652364979824 ) ) ;
#37707 = CARTESIAN_POINT ( 'NONE',  ( 1.710004548794999968, 1516.557392317769882, 215.6678473207969944 ) ) ;
#37708 = LINE ( 'NONE', #106562, #78419 ) ;
#37709 = CARTESIAN_POINT ( 'NONE',  ( 5.567226347498220207, 1511.487400615810202, 217.6749160448409839 ) ) ;
#37710 = CARTESIAN_POINT ( 'NONE',  ( 18.33920247187146302, 1446.399485069377306, 215.8072429957955478 ) ) ;
#37711 = CARTESIAN_POINT ( 'NONE',  ( -7.709032175815000443, 1516.534320418310244, 211.6070631641669877 ) ) ;
#37712 = CARTESIAN_POINT ( 'NONE',  ( -18.84387474539999729, 1434.822844257510042, 209.4888865856029838 ) ) ;
#37713 = CARTESIAN_POINT ( 'NONE',  ( -4.273307515800790490, 1483.235679352140096, 199.3608564754620147 ) ) ;
#37715 = ORIENTED_EDGE ( 'NONE', *, *, #93623, .T. ) ;
#37714 = CARTESIAN_POINT ( 'NONE',  ( -109.9987472970000084, 1390.510529229799886, 304.4717760960590454 ) ) ;
#37716 = AXIS2_PLACEMENT_3D ( 'NONE', #72770, #106898, #47564 ) ;
#37717 = CARTESIAN_POINT ( 'NONE',  ( 3.552713678799999608E-15, 1415.677402202029953, 209.1218459616989946 ) ) ;
#37718 = CARTESIAN_POINT ( 'NONE',  ( 23.86131649859999726, 1453.015588120629900, 232.0003380056980120 ) ) ;
#37719 = CARTESIAN_POINT ( 'NONE',  ( -11.77007789369999990, 1432.382129548040211, 150.8117526338979815 ) ) ;
#37720 = CARTESIAN_POINT ( 'NONE',  ( -14.39820424329999859, 1415.677402202029953, 205.1327016663190079 ) ) ;
#37721 = LINE ( 'NONE', #105483, #79047 ) ;
#37722 = CARTESIAN_POINT ( 'NONE',  ( -18.63567686369149712, 1430.070544426440165, 209.4876081949650199 ) ) ;
#37724 = DIRECTION ( 'NONE',  ( -0.3390050494209005394, -0.7071067811868606556, -0.6205445805634677292 ) ) ;
#37723 = CARTESIAN_POINT ( 'NONE',  ( -20.55070256179999788, 1444.800646429470135, 223.1595721194979944 ) ) ;
#37725 = CARTESIAN_POINT ( 'NONE',  ( 0.04704307171739999932, 1470.812340169630033, 188.5971280676980086 ) ) ;
#37726 = CARTESIAN_POINT ( 'NONE',  ( -105.6827308188049983, 1379.955630914150106, 307.3343922173510236 ) ) ;
#37727 = ORIENTED_EDGE ( 'NONE', *, *, #42552, .T. ) ;
#37728 = CARTESIAN_POINT ( 'NONE',  ( -2.296124889065000119, 1516.677239312369920, 204.5136991508470032 ) ) ;
#37729 = CARTESIAN_POINT ( 'NONE',  ( 2.101979435200000079, 1406.024670839530017, 266.9594151837979439 ) ) ;
#37730 = VECTOR ( 'NONE', #83356, 1000.000000000000000 ) ;
#37731 = CARTESIAN_POINT ( 'NONE',  ( -1.491420627269999910, 1515.551704408389924, 213.0272754455090194 ) ) ;
#37732 = ADVANCED_FACE ( 'NONE', ( #58019 ), #23870, .F. ) ;
#37733 = CARTESIAN_POINT ( 'NONE',  ( 41.13051483880099113, 1450.960394653560115, 270.0519150180469978 ) ) ;
#37734 = EDGE_CURVE ( 'NONE', #81438, #82322, #33174, .T. ) ;
#37735 = CARTESIAN_POINT ( 'NONE',  ( 1.813981524939379364, 1464.111506541877816, 199.4724776592340731 ) ) ;
#37736 = CARTESIAN_POINT ( 'NONE',  ( 11.60004869885203682, 1422.941111951575749, 135.6422307863141157 ) ) ;
#37737 = CIRCLE ( 'NONE', #62794, 1.999997933727205579 ) ;
#37738 = EDGE_CURVE ( 'NONE', #30213, #95653, #86814, .T. ) ;
#37739 = CARTESIAN_POINT ( 'NONE',  ( -18.18137283769999968, 1507.608465321030053, 229.7139307937979993 ) ) ;
#37740 = CARTESIAN_POINT ( 'NONE',  ( 2.295797454685203576, 1449.787077434956245, 154.4026079438378929 ) ) ;
#37741 = CARTESIAN_POINT ( 'NONE',  ( -3.994937574034520100, 1430.106198372560129, 201.8091617894969829 ) ) ;
#37742 = EDGE_CURVE ( 'NONE', #108962, #20905, #34743, .T. ) ;
#37743 = CARTESIAN_POINT ( 'NONE',  ( -1.438891081339280120, 1452.191228260170192, 183.8587004481619829 ) ) ;
#37744 = ADVANCED_FACE ( 'NONE', ( #35551 ), #77024, .T. ) ;
#37745 = CARTESIAN_POINT ( 'NONE',  ( 25.91590772989999891, 1441.261220175949802, 138.4451201509980365 ) ) ;
#37746 = CARTESIAN_POINT ( 'NONE',  ( -5.411583886059999848, 1438.069580177289936, 208.0725929255889923 ) ) ;
#37747 = CIRCLE ( 'NONE', #23416, 1.000000000000000444 ) ;
#37748 = ORIENTED_EDGE ( 'NONE', *, *, #102772, .F. ) ;
#37749 = CARTESIAN_POINT ( 'NONE',  ( -11.47403709489999990, 1414.639208232530109, 262.6648722511980054 ) ) ;
#37750 = ADVANCED_FACE ( 'NONE', ( #95469 ), #10349, .T. ) ;
#37752 = CARTESIAN_POINT ( 'NONE',  ( 4.391391641444769789, 1465.488788256659973, 200.1904207473230031 ) ) ;
#37751 =( REPRESENTATION_RELATIONSHIP ('NONE','NONE', #14372, #10812 ) REPRESENTATION_RELATIONSHIP_WITH_TRANSFORMATION ( #7901 )SHAPE_REPRESENTATION_RELATIONSHIP( ) );
#37753 = AXIS2_PLACEMENT_3D ( 'NONE', #8663, #75357, #109497 ) ;
#37754 = CARTESIAN_POINT ( 'NONE',  ( -0.5564123471769999441, 1475.757529860029990, 269.0455876596980147 ) ) ;
#37755 = B_SPLINE_CURVE_WITH_KNOTS ( 'NONE', 3,
 ( #18815, #95542, #53009, #86587 ),
 .UNSPECIFIED., .F., .F.,
 ( 4, 4 ),
 ( 0.000000000000000000, 1.000000000000000000 ),
 .UNSPECIFIED. ) ;
#37756 = CARTESIAN_POINT ( 'NONE',  ( 7.805006001919999825, 1501.592229138889934, 206.4628694236189972 ) ) ;
#37757 = CARTESIAN_POINT ( 'NONE',  ( -28.09993212570000054, 1509.169756167430023, 210.4944500219079941 ) ) ;
#37758 = CARTESIAN_POINT ( 'NONE',  ( -3.989402217979193033, 1448.297716895625172, 185.0737791360926963 ) ) ;
#37759 = CARTESIAN_POINT ( 'NONE',  ( -24.84597174231020134, 1384.846610513310225, 223.5967099743799906 ) ) ;
#37760 = CARTESIAN_POINT ( 'NONE',  ( 0.9449119460842639873, 1430.444995504165263, 217.4187635772842100 ) ) ;
#37761 = CARTESIAN_POINT ( 'NONE',  ( -4.987078460856490203, 1508.551704408389924, 212.6094383991630252 ) ) ;
#37762 = CARTESIAN_POINT ( 'NONE',  ( 26.80191237839250107, 1435.454312953110048, 135.5610332147589929 ) ) ;
#37763 = CARTESIAN_POINT ( 'NONE',  ( -6.646217445733189955, 1396.145151416729959, 217.9435964253609939 ) ) ;
#37764 = EDGE_CURVE ( 'NONE', #51540, #63441, #78667, .T. ) ;
#37765 = CIRCLE ( 'NONE', #10911, 0.9999999999999873435 ) ;
#37766 = CARTESIAN_POINT ( 'NONE',  ( -15.22947800210000047, 1422.122175526829778, 227.7536867804980147 ) ) ;
#37767 = CARTESIAN_POINT ( 'NONE',  ( 11.86716023049999968, 1432.353341358199941, 147.6509521729980179 ) ) ;
#37768 = ORIENTED_EDGE ( 'NONE', *, *, #17950, .T. ) ;
#37770 = EDGE_CURVE ( 'NONE', #12262, #36031, #104157, .T. ) ;
#37769 = CARTESIAN_POINT ( 'NONE',  ( 1.804213693440000155, 1410.351307743929965, 232.1928990402979878 ) ) ;
#37771 = DIRECTION ( 'NONE',  ( -1.274053389372359975E-11, 4.864808734250780256E-10, -1.000000000000000000 ) ) ;
#37772 = VECTOR ( 'NONE', #70956, 1000.000000000000000 ) ;
#37774 = CARTESIAN_POINT ( 'NONE',  ( -12.04512428226500020, 1511.810036768419877, 193.6554415476670101 ) ) ;
#37773 = CARTESIAN_POINT ( 'NONE',  ( 10.62480271660000142, 1425.043747535729835, 132.2061233091980057 ) ) ;
#37775 = CARTESIAN_POINT ( 'NONE',  ( -9.258462901215001040, 1517.051704408389924, 221.5128288575669728 ) ) ;
#37776 = EDGE_CURVE ( 'NONE', #64419, #90411, #102856, .T. ) ;
#37777 = CARTESIAN_POINT ( 'NONE',  ( -9.000838837759999933, 1450.837337738590122, 206.6584664167089898 ) ) ;
#37778 = B_SPLINE_CURVE_WITH_KNOTS ( 'NONE', 3,
 ( #49276, #83405, #6701, #40856, #75031, #48730, #109183, #32994, #58772, #108613, #32468, #40303, #41966, #100743, #66089, #109719, #102408, #58227, #68300, #76120, #83959, #110260, #67183, #33536, #92351, #7259, #93451, #16722, #15623, #34109, #67736, #101845, #50923, #85053, #42507, #76667, #110816 ),
 .UNSPECIFIED., .F., .F.,
 ( 4, 3, 3, 3, 3, 3, 3, 3, 3, 3, 3, 3, 4 ),
 ( -12.51705759590000078, -12.22413941043480001, -11.58026520907609935, -10.89731576345280040, -10.17759668157450115, -9.397776376799340525, -8.458468502643359699, -7.545168930068030022, -6.795306101010590183, -5.915671535258179681, -5.141253452723230311, -4.456700984109849273, -3.809711666909999295 ),
 .UNSPECIFIED. ) ;
#37779 = CARTESIAN_POINT ( 'NONE',  ( 2.291514297774999598, 1517.194972660189933, 201.3955140066269962 ) ) ;
#37780 = CARTESIAN_POINT ( 'NONE',  ( 7.678276105319999267, 1426.141326229849938, 211.9767368881090022 ) ) ;
#37781 = CARTESIAN_POINT ( 'NONE',  ( 22.14279730899999876, 1473.984189751590065, 210.1089390466149780 ) ) ;
#37782 = CARTESIAN_POINT ( 'NONE',  ( 1.716045945209999868, 1509.007693206030126, 179.5167849949980052 ) ) ;
#37783 = CARTESIAN_POINT ( 'NONE',  ( 7.599227145645000903, 1512.341036949130057, 206.8869232832669809 ) ) ;
#37784 = CARTESIAN_POINT ( 'NONE',  ( -69.65452950130000431, 1376.422073654990072, 286.5559970480589982 ) ) ;
#37785 = ADVANCED_FACE ( 'NONE', ( #3642 ), #108067, .T. ) ;
#37786 = CARTESIAN_POINT ( 'NONE',  ( 3.399663236026384538, 1367.129113533974078, 209.6218459617148824 ) ) ;
#37788 = ORIENTED_EDGE ( 'NONE', *, *, #67787, .F. ) ;
#37787 = CARTESIAN_POINT ( 'NONE',  ( 8.301150669200000110, 1452.680711464789965, 213.4379032366990145 ) ) ;
#37789 = ORIENTED_EDGE ( 'NONE', *, *, #4853, .F. ) ;
#37790 = CARTESIAN_POINT ( 'NONE',  ( -7.738809642880000617, 1396.243216920830037, 200.0727852474580004 ) ) ;
#37791 = CARTESIAN_POINT ( 'NONE',  ( -4.163739766079999960, 1409.058461383930080, 188.2538941213980195 ) ) ;
#37792 = CARTESIAN_POINT ( 'NONE',  ( 12.54268436849999979, 1408.913060387329779, 223.0428732173979824 ) ) ;
#37793 = CARTESIAN_POINT ( 'NONE',  ( -7.635834400824999868, 1511.005930286180046, 213.0490718368869807 ) ) ;
#37795 = CARTESIAN_POINT ( 'NONE',  ( -1.365172581131870011, 1416.963969358779877, 185.3230370589230063 ) ) ;
#37794 = CARTESIAN_POINT ( 'NONE',  ( -7.764758114139999279, 1384.743521014100224, 218.9160524088590023 ) ) ;
#37796 = CARTESIAN_POINT ( 'NONE',  ( 1.914833391339999968, 1429.772458808630063, 184.5724300327979961 ) ) ;
#37797 = CARTESIAN_POINT ( 'NONE',  ( -41.12450279298050049, 1446.742067430790030, 135.7069966715910141 ) ) ;
#37798 = B_SPLINE_CURVE_WITH_KNOTS ( 'NONE', 5,
 ( #47735, #75695, #6272, #14107, #81869, #15200 ),
 .UNSPECIFIED., .F., .F.,
 ( 6, 6 ),
 ( -1.510872622183800029, -4.733984335647534181E-07 ),
 .UNSPECIFIED. ) ;
#37799 = CARTESIAN_POINT ( 'NONE',  ( -2.500000000000079936, 1448.853500281970128, 156.0591697921909997 ) ) ;
#37800 = CARTESIAN_POINT ( 'NONE',  ( 29.16088018400000337, 1435.515811254470009, 135.2139231482979937 ) ) ;
#37801 = CARTESIAN_POINT ( 'NONE',  ( 0.9044596846589999517, 1416.819756528429934, 190.2149403000979930 ) ) ;
#37802 = CARTESIAN_POINT ( 'NONE',  ( -3.816632885168049771, 1406.173185440710085, 269.0404319194170171 ) ) ;
#37803 = CARTESIAN_POINT ( 'NONE',  ( 40.27186280670000684, 1443.842024488900051, 137.1351532911979803 ) ) ;
#37804 = ORIENTED_EDGE ( 'NONE', *, *, #87314, .F. ) ;
#37805 = CARTESIAN_POINT ( 'NONE',  ( -16.69297358003532139, 1526.382868172864164, 183.6963177704346606 ) ) ;
#37806 = CARTESIAN_POINT ( 'NONE',  ( 12.71388170200000189, 1442.799400843799958, 186.7083504157980087 ) ) ;
#37807 = ORIENTED_EDGE ( 'NONE', *, *, #54309, .T. ) ;
#37808 = ORIENTED_EDGE ( 'NONE', *, *, #6645, .T. ) ;
#37809 = CARTESIAN_POINT ( 'NONE',  ( 8.627556093114655766, 1517.551704408390151, 234.1780882150808907 ) ) ;
#37810 = CARTESIAN_POINT ( 'NONE',  ( -15.46700374319999938, 1461.188231601529878, 228.6959067671980108 ) ) ;
#37811 = CARTESIAN_POINT ( 'NONE',  ( 2.487103419534999915, 1516.577434278289957, 215.6681487122470173 ) ) ;
#37812 = CARTESIAN_POINT ( 'NONE',  ( 2.996785032205000032, 1512.020737142380085, 217.0152570523270015 ) ) ;
#37813 = COLOUR_RGB ( '', 0.31764706, 0.68627451, 0.89019608) ;
#37814 = EDGE_CURVE ( 'NONE', #9164, #2539, #62754, .T. ) ;
#37815 = VERTEX_POINT ( 'NONE', #48941 ) ;
#37816 = CARTESIAN_POINT ( 'NONE',  ( -2.953089928408080045, 1509.083816246680044, 179.3119815030040058 ) ) ;
#37817 = CARTESIAN_POINT ( 'NONE',  ( -72.92954128540000625, 1375.020180580649821, 284.3347022688589618 ) ) ;
#37818 = EDGE_CURVE ( 'NONE', #100587, #52269, #110076, .T. ) ;
#37819 = CIRCLE ( 'NONE', #70059, 3.250000000000000000 ) ;
#37820 = CARTESIAN_POINT ( 'NONE',  ( 2.763736212470000009, 1415.425644477229980, 226.3988609140980088 ) ) ;
#37821 = CARTESIAN_POINT ( 'NONE',  ( -2.490245952555000031, 1516.691389976299888, 204.5134284255869943 ) ) ;
#37822 = CARTESIAN_POINT ( 'NONE',  ( 20.20959865099491992, 1512.187213306747481, 236.2316688286738611 ) ) ;
#37823 = CARTESIAN_POINT ( 'NONE',  ( -109.9987473190000031, 1385.131185875960000, 297.1742054003590283 ) ) ;
#37824 = CARTESIAN_POINT ( 'NONE',  ( -3.576202738689999716, 1409.205377980830008, 231.7680162657979963 ) ) ;
#37826 = ORIENTED_EDGE ( 'NONE', *, *, #97509, .T. ) ;
#37825 = CARTESIAN_POINT ( 'NONE',  ( -3.679272716979999913, 1453.313060387329870, 189.6495746351980074 ) ) ;
#37827 = CARTESIAN_POINT ( 'NONE',  ( -14.11276137784757978, 1435.081324051009688, 149.0356280077207032 ) ) ;
#37828 = CARTESIAN_POINT ( 'NONE',  ( -26.54480924795199925, 1440.913060445639985, 224.6644947001300068 ) ) ;
#37829 = CARTESIAN_POINT ( 'NONE',  ( -19.19648987400000095, 1384.187074975920041, 220.4662455178590221 ) ) ;
#37831 = EDGE_CURVE ( 'NONE', #23724, #3072, #54798, .T. ) ;
#37830 = DIRECTION ( 'NONE',  ( 0.000000000000000000, 0.000000000000000000, 1.000000000000000000 ) ) ;
#37832 = CIRCLE ( 'NONE', #100401, 12.49965726619999984 ) ;
#37833 = CARTESIAN_POINT ( 'NONE',  ( 41.55348321080259666, 1432.499391167679960, 270.0571128646830061 ) ) ;
#37834 = CARTESIAN_POINT ( 'NONE',  ( 4.622842844184999578, 1516.901952101700090, 213.1523604828169880 ) ) ;
#37835 = CARTESIAN_POINT ( 'NONE',  ( -65.02291513639998755, 1379.744055000310027, 272.5993806172590439 ) ) ;
#37836 = CARTESIAN_POINT ( 'NONE',  ( 23.29389168950000411, 1409.986405036029964, 208.3140838675509769 ) ) ;
#37837 = CARTESIAN_POINT ( 'NONE',  ( -2.640434834157761479, 1526.748660780343471, 241.3121066639439221 ) ) ;
#37838 = CARTESIAN_POINT ( 'NONE',  ( 8.972130450985041250, 1425.592216824180241, 193.4866236545800007 ) ) ;
#37839 = CARTESIAN_POINT ( 'NONE',  ( 20.72660872792978282, 1410.996521324362220, 199.1611606857948686 ) ) ;
#37840 = CARTESIAN_POINT ( 'NONE',  ( 2.873919002525000099, 1516.940252185109784, 209.1085733957019954 ) ) ;
#37841 = EDGE_LOOP ( 'NONE', ( #1207, #637, #70066, #73191 ) ) ;
#37842 = CARTESIAN_POINT ( 'NONE',  ( -4.291175242752039765, 1446.971469842819943, 154.7965863647420122 ) ) ;
#37843 = CARTESIAN_POINT ( 'NONE',  ( -6.008305668000000210, 1417.906421182329950, 231.8399811658979957 ) ) ;
#37844 = CARTESIAN_POINT ( 'NONE',  ( -86.93036351089999414, 1384.859295106799891, 307.7327112012590078 ) ) ;
#37845 = VERTEX_POINT ( 'NONE', #15293 ) ;
#37847 = AXIS2_PLACEMENT_3D ( 'NONE', #104117, #1679, #77279 ) ;
#37846 = CARTESIAN_POINT ( 'NONE',  ( -20.71467568763819855, 1385.273462423449928, 221.2323961153799985 ) ) ;
#37848 = EDGE_CURVE ( 'NONE', #53940, #24144, #27833, .T. ) ;
#37849 = CYLINDRICAL_SURFACE ( 'NONE', #85301, 2.000000000000003553 ) ;
#37850 = CARTESIAN_POINT ( 'NONE',  ( -7.105427357599999217E-15, 1432.413060387330006, 146.1721969590979882 ) ) ;
#37851 = EDGE_CURVE ( 'NONE', #27633, #78418, #78782, .T. ) ;
#37852 = CARTESIAN_POINT ( 'NONE',  ( 5.614653816015000132, 1512.956339156650074, 203.5071921160869977 ) ) ;
#37853 = CARTESIAN_POINT ( 'NONE',  ( -0.1796713856869999737, 1410.302588876229947, 233.2312010261979935 ) ) ;
#37854 = CARTESIAN_POINT ( 'NONE',  ( 0.1601811252895079807, 1420.470269613179880, 182.7389971891749951 ) ) ;
#37856 = CARTESIAN_POINT ( 'NONE',  ( -16.38047698457823032, 1416.780647377006062, 208.1117118038502554 ) ) ;
#37855 = CARTESIAN_POINT ( 'NONE',  ( 4.038637462725000127, 1516.734985836460055, 214.8955147850770118 ) ) ;
#37857 = CARTESIAN_POINT ( 'NONE',  ( 19.56461708790000031, 1509.492094473429916, 187.5226862208980094 ) ) ;
#37858 = CARTESIAN_POINT ( 'NONE',  ( 9.941125970135800571, 1469.097218566779929, 207.7382653174890095 ) ) ;
#37859 = EDGE_LOOP ( 'NONE', ( #5369, #20163, #91253, #104324 ) ) ;
#37860 = CARTESIAN_POINT ( 'NONE',  ( 5.778999773775000293, 1516.955859323880077, 201.7887757972170277 ) ) ;
#37861 = CARTESIAN_POINT ( 'NONE',  ( 15.72751745975079984, 1522.051704408389924, 206.8816388537309763 ) ) ;
#37862 = ORIENTED_EDGE ( 'NONE', *, *, #43449, .F. ) ;
#37863 = AXIS2_PLACEMENT_3D ( 'NONE', #95290, #102554, #42677 ) ;
#37864 = CARTESIAN_POINT ( 'NONE',  ( 10.37096375755954192, 1396.275222422115121, 201.1218459616979999 ) ) ;
#37865 = EDGE_CURVE ( 'NONE', #34771, #102504, #65345, .T. ) ;
#37866 = CARTESIAN_POINT ( 'NONE',  ( 10.68507717228444243, 1434.716557689225283, 152.0058149931969353 ) ) ;
#37867 = CARTESIAN_POINT ( 'NONE',  ( 8.289603071667819734, 1511.655824793919919, 203.1726102367569808 ) ) ;
#37868 = PRODUCT_DEFINITION_CONTEXT ( 'detailed design', #64909, 'design' ) ;
#37869 = CARTESIAN_POINT ( 'NONE',  ( 2.780476011279999771, 1442.828392787190069, 217.5657236421889991 ) ) ;
#37870 = CARTESIAN_POINT ( 'NONE',  ( 16.81342751137891511, 1421.939823536384210, 226.9481537518386176 ) ) ;
#37871 = CARTESIAN_POINT ( 'NONE',  ( 6.313072733930000346, 1422.316561012229840, 186.3238498068980107 ) ) ;
#37873 = ADVANCED_FACE ( 'NONE', ( #90352 ), #47455, .F. ) ;
#37872 = CARTESIAN_POINT ( 'NONE',  ( -18.15573960440000434, 1424.737936287830053, 225.8718214486980003 ) ) ;
#37874 = CARTESIAN_POINT ( 'NONE',  ( 17.84338787552341543, 1523.481610118011986, 180.3600277898069919 ) ) ;
#37875 = CARTESIAN_POINT ( 'NONE',  ( -7.320561577120000329, 1432.353341358199941, 149.5448088695980005 ) ) ;
#37876 = CARTESIAN_POINT ( 'NONE',  ( 18.34036076829999828, 1488.313847894929722, 189.1254428722979810 ) ) ;
#37878 = CARTESIAN_POINT ( 'NONE',  ( -16.64494502007340770, 1432.422161184578044, 218.5249863156588219 ) ) ;
#37877 = CARTESIAN_POINT ( 'NONE',  ( -32.66476241579304940, 1526.382868172863937, 219.1158660759124643 ) ) ;
#37879 = CARTESIAN_POINT ( 'NONE',  ( 2.038847259693655545, 1522.861859112239017, 244.9330574173661716 ) ) ;
#37880 = ORIENTED_EDGE ( 'NONE', *, *, #61044, .F. ) ;
#37881 = CARTESIAN_POINT ( 'NONE',  ( -103.9247617160000203, 1379.900991233349941, 303.2459714484589881 ) ) ;
#37882 = CARTESIAN_POINT ( 'NONE',  ( -11.26545136039999839, 1508.551704408389924, 217.7655129179189828 ) ) ;
#37883 = CARTESIAN_POINT ( 'NONE',  ( 11.76640019110000068, 1437.123680669209989, 147.7210023317979903 ) ) ;
#37884 = EDGE_CURVE ( 'NONE', #56179, #9541, #94851, .T. ) ;
#37885 = CARTESIAN_POINT ( 'NONE',  ( -24.52306583130000206, 1436.926870631639986, 210.6343607071179918 ) ) ;
#37886 = CARTESIAN_POINT ( 'NONE',  ( -4.729727150590000484, 1484.839046518389978, 198.6511715847990160 ) ) ;
#37887 = CARTESIAN_POINT ( 'NONE',  ( -15.90344751825240799, 1418.061016069739026, 203.7331501587224238 ) ) ;
#37888 = CARTESIAN_POINT ( 'NONE',  ( -2.986444372602363728, 1425.988535542772979, 185.4516627005385772 ) ) ;
#37889 = CARTESIAN_POINT ( 'NONE',  ( 12.44994833213096008, 1435.748311113976797, 150.9813188435746270 ) ) ;
#37890 = CARTESIAN_POINT ( 'NONE',  ( -17.11050544143609997, 1414.913527275050001, 207.5943401297909929 ) ) ;
#37891 = CARTESIAN_POINT ( 'NONE',  ( 4.336695207250549799, 1494.691757117450152, 219.8673055875190130 ) ) ;
#37892 = ADVANCED_FACE ( 'NONE', ( #51132 ), #24044, .F. ) ;
#37893 = EDGE_CURVE ( 'NONE', #70768, #17951, #31081, .T. ) ;
#37894 = CARTESIAN_POINT ( 'NONE',  ( -6.684245985025539127, 1487.813528818469877, 218.7500381969930174 ) ) ;
#37895 = CARTESIAN_POINT ( 'NONE',  ( -9.609628710759999137, 1464.248356776189894, 228.1965957863990013 ) ) ;
#37896 = CARTESIAN_POINT ( 'NONE',  ( -85.71654444118949812, 1383.773072311060105, 306.8335668707890136 ) ) ;
#37897 = CARTESIAN_POINT ( 'NONE',  ( -108.9547098300069905, 1384.162005566360222, 311.1881139208990135 ) ) ;
#37898 = CARTESIAN_POINT ( 'NONE',  ( 5.885377578960000022, 1429.730554523590172, 216.6318111531790009 ) ) ;
#37900 = VERTEX_POINT ( 'NONE', #48106 ) ;
#37899 = CARTESIAN_POINT ( 'NONE',  ( 21.02378441960000188, 1508.374119905930002, 190.5095349432980072 ) ) ;
#37901 = B_SPLINE_CURVE_WITH_KNOTS ( 'NONE', 3,
 ( #43873, #52839, #86966, #19759, #19185, #109555, #53389, #58606, #96479, #44433, #87538, #44998, #7630, #79142, #43330, #69094, #103195, #26500, #60696, #18096, #52291, #14098, #80781, #106526, #71876, #105434, #71319, #98112, #29813, #3548, #30909, #99201, #28722, #11919, #62928, #97039, #20850, #37119, #22480, #81860 ),
 .UNSPECIFIED., .F., .F.,
 ( 4, 3, 3, 3, 3, 3, 3, 3, 3, 3, 3, 3, 3, 4 ),
 ( -12.02648879740000076, -11.98563415181089908, -11.30522982652169972, -10.58397085564349993, -9.831326559260959996, -9.032570767541811207, -8.137609212483280174, -7.249943402468200127, -7.107856609420229788, -6.496713401214210037, -5.822552568774050030, -5.084697154694810095, -4.319144763170720935, -3.650975912550000757 ),
 .UNSPECIFIED. ) ;
#37902 = CARTESIAN_POINT ( 'NONE',  ( -106.4664531209999865, 1381.040142295360056, 309.4626932862590252 ) ) ;
#37903 = CARTESIAN_POINT ( 'NONE',  ( 13.08508097766669920, 1512.436270050390021, 224.3649262596819938 ) ) ;
#37904 = EDGE_LOOP ( 'NONE', ( #33798, #16988, #36991, #93243, #104734 ) ) ;
#37905 = EDGE_LOOP ( 'NONE', ( #21914, #39737, #34788, #36643, #50615 ) ) ;
#37906 = CARTESIAN_POINT ( 'NONE',  ( -110.0628372420000005, 1384.916020893610039, 296.9513042793590216 ) ) ;
#37907 = CARTESIAN_POINT ( 'NONE',  ( 12.90411285433943611, 1442.893553763067530, 169.4358074260771332 ) ) ;
#37909 = CARTESIAN_POINT ( 'NONE',  ( -25.42953938249999979, 1453.762068279829919, 238.1443916851980305 ) ) ;
#37908 = CARTESIAN_POINT ( 'NONE',  ( 31.13322700354939343, 1420.444298374236496, 269.4832979485171904 ) ) ;
#37910 = CARTESIAN_POINT ( 'NONE',  ( -19.98650548909999713, 1487.993256480629952, 190.6491142766980147 ) ) ;
#37911 = CARTESIAN_POINT ( 'NONE',  ( -11.92631326350000087, 1433.455531743929896, 150.1111345919979954 ) ) ;
#37912 = TOROIDAL_SURFACE ( 'NONE', #30540, 24.00000000000000000, 1.000000000000000000 ) ;
#37913 = CARTESIAN_POINT ( 'NONE',  ( 27.48210477259999962, 1509.872756633229983, 199.3218240744180036 ) ) ;
#37914 = CARTESIAN_POINT ( 'NONE',  ( -19.20165183970000200, 1486.139761766429956, 189.5810907390980162 ) ) ;
#37915 = CARTESIAN_POINT ( 'NONE',  ( 4.780307568339999591, 1467.625956517089890, 217.8721402715589761 ) ) ;
#37916 = CARTESIAN_POINT ( 'NONE',  ( -3.677001408430000229, 1443.877114344990105, 218.5311880179489776 ) ) ;
#37917 = CARTESIAN_POINT ( 'NONE',  ( 4.540052872590000455, 1421.340300729830005, 185.5158982254980060 ) ) ;
#37919 = EDGE_CURVE ( 'NONE', #48060, #37972, #106565, .T. ) ;
#37918 = CARTESIAN_POINT ( 'NONE',  ( -24.40996130410000120, 1440.626642977380016, 212.0145020556379905 ) ) ;
#37920 = CARTESIAN_POINT ( 'NONE',  ( -107.8662654264032170, 1378.913060344626274, 308.7118336974646695 ) ) ;
#37921 = CARTESIAN_POINT ( 'NONE',  ( -6.112747810279289595, 1477.579416776660082, 218.9411244695629932 ) ) ;
#37922 = CARTESIAN_POINT ( 'NONE',  ( 32.77044109517470361, 1525.581535527371443, 199.0807904155084600 ) ) ;
#37924 = EDGE_LOOP ( 'NONE', ( #108288, #20538 ) ) ;
#37923 = CARTESIAN_POINT ( 'NONE',  ( 1.895454726076929561E-09, 1410.564254227580022, 257.2398119582219920 ) ) ;
#37925 = ORIENTED_EDGE ( 'NONE', *, *, #12860, .T. ) ;
#37926 = CARTESIAN_POINT ( 'NONE',  ( -11.85748657036189968, 1431.735414931930109, 149.9492757270899972 ) ) ;
#37927 = CARTESIAN_POINT ( 'NONE',  ( -21.53550188629999695, 1488.484788005089968, 202.1758863209290098 ) ) ;
#37928 = CARTESIAN_POINT ( 'NONE',  ( -8.322172262500000528, 1473.608514543630008, 270.1222559170979594 ) ) ;
#37929 = CARTESIAN_POINT ( 'NONE',  ( -23.86106795586941942, 1435.967792748258717, 211.4074662604529067 ) ) ;
#37930 = CARTESIAN_POINT ( 'NONE',  ( -106.1286243849658177, 1375.179104070688027, 316.4799049169590717 ) ) ;
#37931 = CARTESIAN_POINT ( 'NONE',  ( -15.05666906759999968, 1495.930445535429953, 224.5094625774979988 ) ) ;
#37932 = CIRCLE ( 'NONE', #109465, 1.000000000000002442 ) ;
#37933 = B_SPLINE_CURVE_WITH_KNOTS ( 'NONE', 5,
 ( #110687, #48603, #67060, #109057, #58103, #32341, #33979, #50790, #40181 ),
 .UNSPECIFIED., .F., .F.,
 ( 6, 3, 6 ),
 ( 0.000000000000000000, 0.1586384821461520045, 1.000000000000000000 ),
 .UNSPECIFIED. ) ;
#37934 = CARTESIAN_POINT ( 'NONE',  ( 0.2099472870183970163, 1452.743325152459875, 183.2501930988930212 ) ) ;
#37935 = CARTESIAN_POINT ( 'NONE',  ( -13.37979245520000049, 1421.464012522729945, 229.5728339053979994 ) ) ;
#37936 = CARTESIAN_POINT ( 'NONE',  ( -13.07344736774610183, 1516.551188146160030, 225.7923144865690119 ) ) ;
#37937 = CARTESIAN_POINT ( 'NONE',  ( -8.571847540900000340, 1459.808793802090122, 213.9952768880189922 ) ) ;
#37938 = CARTESIAN_POINT ( 'NONE',  ( 7.359670431058202844, 1360.525381303870972, 210.6218459617030021 ) ) ;
#37939 = CARTESIAN_POINT ( 'NONE',  ( -44.41403626570249941, 1432.254696578300127, 268.8004549980919933 ) ) ;
#37940 = ORIENTED_EDGE ( 'NONE', *, *, #39428, .T. ) ;
#37941 = CARTESIAN_POINT ( 'NONE',  ( -3.536775676796930501, 1494.955962957219981, 181.4953438780639772 ) ) ;
#37942 = EDGE_LOOP ( 'NONE', ( #43692, #65750, #38346, #65202, #107720, #19301 ) ) ;
#37943 = ORIENTED_EDGE ( 'NONE', *, *, #88228, .T. ) ;
#37944 = CARTESIAN_POINT ( 'NONE',  ( 0.7579262867720020225, 1516.927039499179955, 210.8260166843570005 ) ) ;
#37945 = CARTESIAN_POINT ( 'NONE',  ( -9.718888103667799427, 1446.855032085529956, 212.2079679782489734 ) ) ;
#37946 = CARTESIAN_POINT ( 'NONE',  ( 17.05103420828933380, 1409.778319746613079, 224.8086557538146906 ) ) ;
#37947 = CARTESIAN_POINT ( 'NONE',  ( -2.665104874070000296, 1425.412186680530112, 185.9059251853979902 ) ) ;
#37948 = CIRCLE ( 'NONE', #46918, 7.842199003069996621 ) ;
#37949 = CARTESIAN_POINT ( 'NONE',  ( -27.02656364750020401, 1451.901091008129924, 135.4178927912169854 ) ) ;
#37950 = ORIENTED_EDGE ( 'NONE', *, *, #3143, .T. ) ;
#37951 =( BOUNDED_SURFACE ( )  B_SPLINE_SURFACE ( 3, 2, ( 
 ( #110345, #40938, #102483 ),
 ( #8424, #23579, #24654 ),
 ( #101929, #34191, #77313 ),
 ( #42595, #16802, #49905 ),
 ( #85137, #101363, #58855 ),
 ( #15164, #25772, #93532 ) ),
 .UNSPECIFIED., .F., .F., .F. ) 
 B_SPLINE_SURFACE_WITH_KNOTS ( ( 4, 2, 4 ),
 ( 3, 3 ),
 ( 2.723515857283587138E-16, 0.001312027981647352279, 0.002624055963294432206 ),
 ( 0.000000000000000000, 1.000000000000000000 ),
 .UNSPECIFIED. ) 
 GEOMETRIC_REPRESENTATION_ITEM ( )  RATIONAL_B_SPLINE_SURFACE ( (
 ( 1.000000000000000000, 0.9376006582765955555, 1.000000000000000000),
 ( 1.000000000000000000, 0.9569320108030413552, 1.000000000000000000),
 ( 1.000000000000000000, 0.9725743441608736273, 1.000000000000000000),
 ( 1.000000000000000000, 0.9942095667145922633, 1.000000000000000000),
 ( 1.000000000000000000, 1.000043666449937030, 1.000000000000000000),
 ( 1.000000000000000000, 1.000000000000000000, 1.000000000000000000) ) ) 
 REPRESENTATION_ITEM ( '' )  SURFACE ( )  );
#37952 = CARTESIAN_POINT ( 'NONE',  ( -3.454748846324999789, 1516.609912606490070, 201.7988116581369979 ) ) ;
#37953 = DIRECTION ( 'NONE',  ( -0.3363363969988524271, -0.9417419115945887542, 0.000000000000000000 ) ) ;
#37954 = CARTESIAN_POINT ( 'NONE',  ( -15.50041385721359966, 1384.523326672639996, 200.7202488855130014 ) ) ;
#37955 = ORIENTED_EDGE ( 'NONE', *, *, #26212, .F. ) ;
#37956 = CARTESIAN_POINT ( 'NONE',  ( -9.584254063140670965, 1410.554478348119801, 270.0755687917119872 ) ) ;
#37957 = CARTESIAN_POINT ( 'NONE',  ( -2.286265947080000416, 1427.727383903629971, 112.4493539157979995 ) ) ;
#37958 = CARTESIAN_POINT ( 'NONE',  ( 8.561929138950318929, 1436.589287696300062, 208.1473329548439892 ) ) ;
#37960 = ORIENTED_EDGE ( 'NONE', *, *, #69222, .T. ) ;
#37959 = CARTESIAN_POINT ( 'NONE',  ( -8.103279866443569901, 1365.019086496305590, 208.3718459617061285 ) ) ;
#37961 = VERTEX_POINT ( 'NONE', #12276 ) ;
#37962 = CARTESIAN_POINT ( 'NONE',  ( 44.74112653917228499, 1447.656416290266407, 268.9998424599907025 ) ) ;
#37963 = CARTESIAN_POINT ( 'NONE',  ( 11.39798805746750077, 1471.122479896730056, 209.6527432349059836 ) ) ;
#37964 = CARTESIAN_POINT ( 'NONE',  ( -14.22053218827930188, 1436.255562567059997, 150.1050894581620128 ) ) ;
#37965 = CARTESIAN_POINT ( 'NONE',  ( -0.3255694447470000030, 1486.004385721930021, 181.7846486939979798 ) ) ;
#37966 = CARTESIAN_POINT ( 'NONE',  ( -21.76163504101332080, 1506.366982243313487, 212.1069626703776407 ) ) ;
#37967 = CARTESIAN_POINT ( 'NONE',  ( 5.391625819569999756, 1433.099291512059835, 154.6242831037980068 ) ) ;
#37968 = CARTESIAN_POINT ( 'NONE',  ( 15.86141264426099973, 1474.310288337290103, 267.4439829464420200 ) ) ;
#37969 = CARTESIAN_POINT ( 'NONE',  ( 11.20854081390000090, 1414.996444526030018, 222.5314265605980211 ) ) ;
#37970 = CARTESIAN_POINT ( 'NONE',  ( 7.678837752449999776, 1445.740092221990153, 183.5513996952979880 ) ) ;
#37971 = CARTESIAN_POINT ( 'NONE',  ( -3.461995196814999787, 1516.906233342200039, 206.2559344154570056 ) ) ;
#37972 = VERTEX_POINT ( 'NONE', #65472 ) ;
#37973 = CARTESIAN_POINT ( 'NONE',  ( -38.81202641437909762, 1436.797832205920031, 135.3761633872119887 ) ) ;
#37974 = CARTESIAN_POINT ( 'NONE',  ( -21.36341525586438550, 1454.134263472093608, 222.4395773065823789 ) ) ;
#37975 = VERTEX_POINT ( 'NONE', #1854 ) ;
#37976 = CARTESIAN_POINT ( 'NONE',  ( -2.470168521978398868, 1512.187213306747481, 242.8787258963054683 ) ) ;
#37977 = EDGE_CURVE ( 'NONE', #67344, #77058, #107440, .T. ) ;
#37978 = CARTESIAN_POINT ( 'NONE',  ( 25.28734891721619960, 1450.982973813519720, 137.4270881049000081 ) ) ;
#37979 = DIRECTION ( 'NONE',  ( -1.755985294532469921E-16, 1.000000000000000000, -1.338183447452831989E-16 ) ) ;
#37980 = CARTESIAN_POINT ( 'NONE',  ( -6.544148738009999633, 1414.829190269450010, 206.3506811497689739 ) ) ;
#37981 = CARTESIAN_POINT ( 'NONE',  ( 18.47322038440000114, 1409.558159458129921, 197.4202168127980030 ) ) ;
#37982 = CARTESIAN_POINT ( 'NONE',  ( 22.91694143579999832, 1410.643289488730034, 207.1553313229279922 ) ) ;
#37983 = CARTESIAN_POINT ( 'NONE',  ( -26.56555459097119964, 1481.927937259539931, 210.5566609482799834 ) ) ;
#37984 = CARTESIAN_POINT ( 'NONE',  ( -14.05223976236401207, 1379.587684537167888, 211.8183454839635260 ) ) ;
#37985 = CARTESIAN_POINT ( 'NONE',  ( 0.6813382182996269298, 1451.459142117649890, 182.8216330104679912 ) ) ;
#37986 = B_SPLINE_CURVE_WITH_KNOTS ( 'NONE', 3,
 ( #40336, #56051, #5650, #91295, #62990, #90178 ),
 .UNSPECIFIED., .F., .F.,
 ( 4, 2, 4 ),
 ( 0.000000000000000000, 0.5000395032561160136, 1.000267919028009933 ),
 .UNSPECIFIED. ) ;
#37987 = LINE ( 'NONE', #63756, #101561 ) ;
#37988 = CARTESIAN_POINT ( 'NONE',  ( -5.000083865865000199, 1516.858456333729919, 214.1306941701269864 ) ) ;
#37989 = CARTESIAN_POINT ( 'NONE',  ( 3.350338079455627671, 1523.604703353109926, 242.0808062845893289 ) ) ;
#37990 = VERTEX_POINT ( 'NONE', #46470 ) ;
#37991 = CARTESIAN_POINT ( 'NONE',  ( -17.13241642390000052, 1417.472910479740221, 206.6641778192989989 ) ) ;
#37992 = DIRECTION ( 'NONE',  ( 0.03084238745359989264, -0.9990097612528838766, 0.03206624483187858754 ) ) ;
#37993 = CARTESIAN_POINT ( 'NONE',  ( 2.500000000000000000, 1439.114301455650093, 157.7261946041980138 ) ) ;
#37994 = CARTESIAN_POINT ( 'NONE',  ( -9.236170142511459957, 1423.625851892860055, 144.1551608696729829 ) ) ;
#37995 = CARTESIAN_POINT ( 'NONE',  ( -36.08318819676349420, 1449.986793179470169, 136.2470111316459906 ) ) ;
#37996 = CARTESIAN_POINT ( 'NONE',  ( 10.85733419331820393, 1424.789793182321318, 138.1870230799576404 ) ) ;
#37997 = CARTESIAN_POINT ( 'NONE',  ( -3.272667022753708466, 1522.051704408389924, 189.0363362235078171 ) ) ;
#37998 = CARTESIAN_POINT ( 'NONE',  ( -2.898404794048390354, 1484.263598554799955, 183.3162688752209704 ) ) ;
#38000 = ADVANCED_FACE ( 'NONE', ( #97933 ), #20290, .T. ) ;
#37999 = CARTESIAN_POINT ( 'NONE',  ( -12.31052647389649835, 1378.376188973679973, 209.7933296302919928 ) ) ;
#38001 = DIRECTION ( 'NONE',  ( -1.000000000000000000, -2.249639673992789970E-32, -1.224646799147350002E-16 ) ) ;
#38002 = CARTESIAN_POINT ( 'NONE',  ( 25.01304800111659787, 1440.913060398049993, 216.1348349641639857 ) ) ;
#38003 = CARTESIAN_POINT ( 'NONE',  ( -109.5388894170000071, 1385.012700822230272, 297.1239152411590112 ) ) ;
#38004 = CARTESIAN_POINT ( 'NONE',  ( 10.72043382369189857, 1500.413529223420028, 204.6654587861600021 ) ) ;
#38005 = EDGE_LOOP ( 'NONE', ( #107086, #53757, #24701, #33505, #19320, #6303, #76801, #39455, #69891, #83818, #74948, #82475 ) ) ;
#38006 = EDGE_CURVE ( 'NONE', #104414, #103300, #92003, .T. ) ;
#38007 = CARTESIAN_POINT ( 'NONE',  ( -3.355892881418364837, 1523.847233649538339, 176.1815261159892145 ) ) ;
#38008 = EDGE_CURVE ( 'NONE', #28026, #22756, #66109, .T. ) ;
#38009 = CARTESIAN_POINT ( 'NONE',  ( -113.4000000000000057, 1379.886883438980021, 304.2218459572590064 ) ) ;
#38010 = CARTESIAN_POINT ( 'NONE',  ( -1.249906575759999861, 1443.441360560090061, 200.1672907908790080 ) ) ;
#38011 = CARTESIAN_POINT ( 'NONE',  ( 12.24666786109679961, 1501.370948797369920, 211.6632830822960045 ) ) ;
#38012 = VECTOR ( 'NONE', #73821, 999.9999999999998863 ) ;
#38013 = ADVANCED_FACE ( 'NONE', ( #7740 ), #39208, .T. ) ;
#38014 = FACE_OUTER_BOUND ( 'NONE', #830, .T. ) ;
#38015 = CARTESIAN_POINT ( 'NONE',  ( -12.04996996890000105, 1508.335006800029987, 233.7287155051980108 ) ) ;
#38016 = CARTESIAN_POINT ( 'NONE',  ( -25.99927661702099968, 1383.846917199799918, 224.2199440044900030 ) ) ;
#38017 = CARTESIAN_POINT ( 'NONE',  ( -2.487922500652269608, 1508.611354795260013, 204.4437021699770014 ) ) ;
#38018 = CARTESIAN_POINT ( 'NONE',  ( 5.372875771976799442, 1422.387436188309948, 137.8049185903410319 ) ) ;
#38019 = CARTESIAN_POINT ( 'NONE',  ( -203.9558787908000284, -8382.262153571269664, 2179.147420460110425 ) ) ;
#38020 = CARTESIAN_POINT ( 'NONE',  ( 1.551201541590000232, 1466.314669792330051, 234.8893240182980264 ) ) ;
#38022 = ORIENTED_EDGE ( 'NONE', *, *, #52153, .F. ) ;
#38021 = CARTESIAN_POINT ( 'NONE',  ( 9.707170653865018650, 1452.234477919450001, 209.8040067783620088 ) ) ;
#38023 = CARTESIAN_POINT ( 'NONE',  ( -1.019439684479999997, 1451.327316323330024, 183.0760546737980121 ) ) ;
#38024 = CARTESIAN_POINT ( 'NONE',  ( -37.09676805939999866, 1383.024146519360102, 210.3189902961190114 ) ) ;
#38025 = CARTESIAN_POINT ( 'NONE',  ( 3.136939361377039770, 1508.551704408389924, 204.2190535551970072 ) ) ;
#38027 = VERTEX_POINT ( 'NONE', #41357 ) ;
#38026 = CARTESIAN_POINT ( 'NONE',  ( -16.63478241967279914, 1414.913060387399810, 207.7445871609179733 ) ) ;
#38028 = CARTESIAN_POINT ( 'NONE',  ( -22.19118223659430100, 1483.601855164859899, 216.8114985404419883 ) ) ;
#38029 = EDGE_LOOP ( 'NONE', ( #101276, #2727, #7516, #50935 ) ) ;
#38030 = CARTESIAN_POINT ( 'NONE',  ( -12.31798489929459883, 1389.268006845099990, 215.3113464096479959 ) ) ;
#38031 = DIRECTION ( 'NONE',  ( 0.8495773475194792201, -0.1203693149516160271, 0.5135460627829260272 ) ) ;
#38032 = CARTESIAN_POINT ( 'NONE',  ( -9.659668719498959888, 1460.930246227030011, 210.9154259961320008 ) ) ;
#38033 = CARTESIAN_POINT ( 'NONE',  ( -11.60004869885202972, 1426.698742266320096, 134.5125406510034338 ) ) ;
#38034 = CARTESIAN_POINT ( 'NONE',  ( -15.61462149936531496, 1419.935087858347742, 211.2718617567576871 ) ) ;
#38035 = CARTESIAN_POINT ( 'NONE',  ( 21.21789656210188468, 1509.702941487444605, 188.2403193419460479 ) ) ;
#38036 = CARTESIAN_POINT ( 'NONE',  ( 14.91913257496040046, 1409.434047977000091, 208.5473241550759838 ) ) ;
#38037 = CARTESIAN_POINT ( 'NONE',  ( -7.965810688893188996, 1384.899971919800009, 199.4892299149449855 ) ) ;
#38038 = CARTESIAN_POINT ( 'NONE',  ( -98.60501928763169133, 1385.217285518659992, 295.9932508494239869 ) ) ;
#38039 = EDGE_CURVE ( 'NONE', #39681, #42334, #99971, .T. ) ;
#38040 = CARTESIAN_POINT ( 'NONE',  ( -18.23663199019999936, 1440.788381478219890, 191.4112727536980003 ) ) ;
#38041 = CARTESIAN_POINT ( 'NONE',  ( -67.63612853559999394, 1379.748709736400087, 277.8550023105590299 ) ) ;
#38042 = CARTESIAN_POINT ( 'NONE',  ( 10.85247041220890019, 1489.752500976519968, 207.7569310478100135 ) ) ;
#38043 = EDGE_LOOP ( 'NONE', ( #22182, #18120, #81674, #50813 ) ) ;
#38044 = VERTEX_POINT ( 'NONE', #101784 ) ;
#38045 = B_SPLINE_CURVE_WITH_KNOTS ( 'NONE', 3,
 ( #58231, #34113, #68303, #94015, #17279, #31907, #100222, #23502, #15088, #49281, #6705, #40860, #92355, #15627, #10578, #61551, #35218, #2205, #69404, #9467, #69960, #1640, #70516, #62110, #77240, #104631, #35778, #43632, #27369, #1092, #77782, #95684, #87853, #53716, #2753, #36873, #102953, #104074, #53145, #52593, #88385, #71067, #78328, #27928, #62674, #18950, #96234, #87283, #103515, #86727, #54259, #43080, #26254, #10018, #44749, #17835, #68851, #26819, #86174, #94560, #61006, #11142, #105189, #541, #95132, #45302, #34665, #52038, #36319 ),
 .UNSPECIFIED., .F., .F.,
 ( 4, 2, 2, 2, 2, 2, 1, 1, 2, 2, 2, 2, 1, 1, 2, 2, 2, 2, 1, 1, 2, 2, 2, 1, 2, 2, 2, 1, 1, 1, 2, 2, 2, 2, 1, 1, 1, 1, 1, 2, 2, 4 ),
 ( 0.000000000000000000, 0.03124999999976661724, 0.04687499999965134140, 0.06249999999953606555, 0.07812499999942078277, 0.08593749999936303730, 0.08984374999934520434, 0.09179687499932684402, 0.09277343749930819228, 0.09374999999928952665, 0.1093749999990587252, 0.1171874999989445804, 0.1210937499988954391, 0.1230468749988719857, 0.1240234374988613553, 0.1249999999988507110, 0.1562499999987173038, 0.1718749999986504684, 0.1796874999986185217, 0.1835937499986117216, 0.1855468749986193822, 0.1874999999986270149, 0.2187499999986969867, 0.2343749999987318755, 0.2421874999987381205, 0.2499999999987443378, 0.3749999999989568900, 0.4374999999990732968, 0.4687499999991417421, 0.4843749999991775468, 0.4921874999991939781, 0.4999999999992104094, 0.6249999999994299005, 0.6874999999995489164, 0.7187499999996067590, 0.7343749999996357358, 0.7421874999996502797, 0.7460937499996576072, 0.7480468749996712630, 0.7490234374996782574, 0.7499999999996851408, 1.000000000000000000 ),
 .UNSPECIFIED. ) ;
#38046 = EDGE_CURVE ( 'NONE', #9383, #17126, #6640, .T. ) ;
#38047 = CARTESIAN_POINT ( 'NONE',  ( -7.266079668920959911, 1509.032014039220030, 215.8914689751280207 ) ) ;
#38048 = CARTESIAN_POINT ( 'NONE',  ( -11.26466626661590098, 1415.020374543960088, 195.6559317589140221 ) ) ;
#38049 = CARTESIAN_POINT ( 'NONE',  ( -11.93818408299999945, 1433.480074519959999, 149.8972116839979947 ) ) ;
#38050 = CARTESIAN_POINT ( 'NONE',  ( 3.111006074948589777E-10, 1465.532046810729980, 239.7303713660589892 ) ) ;
#38051 = CARTESIAN_POINT ( 'NONE',  ( -20.16694168119990138, 1493.837731802399958, 190.7961038711720221 ) ) ;
#38052 = CARTESIAN_POINT ( 'NONE',  ( 2.546717553650000188, 1397.067799814130012, 221.7839619645980065 ) ) ;
#38053 = CARTESIAN_POINT ( 'NONE',  ( 31.30542570072814712, 1525.651285554129345, 201.9631097759967133 ) ) ;
#38054 = CARTESIAN_POINT ( 'NONE',  ( -18.97219799319119815, 1486.246528605739741, 189.3000344508529906 ) ) ;
#38055 = CARTESIAN_POINT ( 'NONE',  ( -10.32721170034283809, 1366.899502727329264, 207.6218459616987673 ) ) ;
#38056 = CARTESIAN_POINT ( 'NONE',  ( 3.355893228018326457, 1523.847248782568613, 176.1815272790888685 ) ) ;
#38057 = CARTESIAN_POINT ( 'NONE',  ( -0.01265822594359850006, 1516.959716008189844, 207.4120794380770292 ) ) ;
#38058 = CARTESIAN_POINT ( 'NONE',  ( -13.62986346476509958, 1435.068496676610039, 149.3976263793470025 ) ) ;
#38059 = CARTESIAN_POINT ( 'NONE',  ( -3.271538019026510202, 1454.292002138270163, 199.1638778078030043 ) ) ;
#38060 = CARTESIAN_POINT ( 'NONE',  ( 0.9044594075830000302, 1416.819760216229952, 190.2149401804979902 ) ) ;
#38061 = CARTESIAN_POINT ( 'NONE',  ( 2.045592726109999759, 1498.492550166889941, 197.9893586035990154 ) ) ;
#38062 = CARTESIAN_POINT ( 'NONE',  ( 13.33054332923500063, 1520.551704408390151, 211.1218459511669892 ) ) ;
#38063 = B_SPLINE_CURVE_WITH_KNOTS ( 'NONE', 5,
 ( #7833, #78362, #42002, #110298, #85636, #59374 ),
 .UNSPECIFIED., .F., .F.,
 ( 6, 6 ),
 ( 0.000000000000000000, 11.48858425020000240 ),
 .UNSPECIFIED. ) ;
#38064 = ORIENTED_EDGE ( 'NONE', *, *, #39759, .F. ) ;
#38065 = CARTESIAN_POINT ( 'NONE',  ( 29.79081509879999601, 1435.029579668840142, 240.1465591088980034 ) ) ;
#38066 = CARTESIAN_POINT ( 'NONE',  ( -25.27895407679999806, 1469.239702726530140, 203.5787248714279940 ) ) ;
#38068 = CARTESIAN_POINT ( 'NONE',  ( 2.509110313610579488E-14, 1423.297483101070156, 232.1344543676479759 ) ) ;
#38067 = CARTESIAN_POINT ( 'NONE',  ( -2.550919205790000088, 1504.648467973429888, 180.9569263682979852 ) ) ;
#38069 = CARTESIAN_POINT ( 'NONE',  ( 4.329448776040000446, 1515.064792882589927, 210.9648081929590262 ) ) ;
#38070 = CARTESIAN_POINT ( 'NONE',  ( -15.47923624559999922, 1416.261629426230002, 248.5133305101979886 ) ) ;
#38071 = CARTESIAN_POINT ( 'NONE',  ( 0.9805682090549989738, 1486.537029112289929, 220.0330171165990123 ) ) ;
#38072 = CARTESIAN_POINT ( 'NONE',  ( 0.8426039787746957277, 1415.538311208945288, 233.2356076681966783 ) ) ;
#38073 = FACE_OUTER_BOUND ( 'NONE', #88113, .T. ) ;
#38074 = EDGE_LOOP ( 'NONE', ( #74038, #1132, #65431 ) ) ;
#38075 = CARTESIAN_POINT ( 'NONE',  ( -2.500000000000000000, 1432.112068525799941, 157.4891847571979895 ) ) ;
#38076 = CARTESIAN_POINT ( 'NONE',  ( 14.47449472319151376, 1514.320576839395017, 225.5689061850603991 ) ) ;
#38077 = DIRECTION ( 'NONE',  ( 0.1838871638018280408, 0.9727212700611359564, -0.1414172611797089030 ) ) ;
#38078 = VERTEX_POINT ( 'NONE', #40795 ) ;
#38079 = ORIENTED_EDGE ( 'NONE', *, *, #19891, .F. ) ;
#38080 = CARTESIAN_POINT ( 'NONE',  ( 9.649574114248718359, 1452.507656576000045, 210.4986084856580248 ) ) ;
#38081 = CARTESIAN_POINT ( 'NONE',  ( -23.71385237390180123, 1410.153949763399851, 208.7056816592929920 ) ) ;
#38083 = ORIENTED_EDGE ( 'NONE', *, *, #57524, .F. ) ;
#38082 = B_SPLINE_CURVE_WITH_KNOTS ( 'NONE', 3,
 ( #13226, #107308, #41210, #25485, #58573, #7599, #110614, #8141, #24923, #50711, #50180, #41753, #33896, #92701, #75912, #16520, #84841, #42307, #51260, #109519, #59134, #102205, #42870, #84307, #66979, #33339, #24389, #68092, #110064, #67534, #101634 ),
 .UNSPECIFIED., .F., .F.,
 ( 4, 3, 3, 3, 3, 3, 3, 3, 3, 3, 4 ),
 ( -15.26427302110819895, -15.05934333483120113, -14.73799943699000004, -14.51062177820000088, -14.45665274134599976, -14.26912914067029980, -14.02763650314049926, -13.81025237607900102, -13.62933106218500079, -13.46144724711600027, -13.44470524421359947 ),
 .UNSPECIFIED. ) ;
#38084 = CARTESIAN_POINT ( 'NONE',  ( -0.1314063909958990140, 1442.749369516519891, 202.9452824733500051 ) ) ;
#38085 = LINE ( 'NONE', #35893, #13321 ) ;
#38086 = CARTESIAN_POINT ( 'NONE',  ( -0.4938443966799999640, 1470.488522285229919, 235.7260322168980053 ) ) ;
#38087 = CARTESIAN_POINT ( 'NONE',  ( -113.4000000000000057, 1390.913060387289988, 304.2218459572590064 ) ) ;
#38088 = VERTEX_POINT ( 'NONE', #59277 ) ;
#38089 = CARTESIAN_POINT ( 'NONE',  ( 11.43729524049999924, 1425.481262536329950, 144.1593964291980114 ) ) ;
#38090 = CARTESIAN_POINT ( 'NONE',  ( -13.01671764799590036, 1416.842625005220043, 221.9093393807470136 ) ) ;
#38091 = CARTESIAN_POINT ( 'NONE',  ( 13.40854346959999965, 1452.823344015929933, 224.6980477592980208 ) ) ;
#38092 = CARTESIAN_POINT ( 'NONE',  ( 4.031142351675000235, 1516.929569650079884, 204.1114229688670036 ) ) ;
#38093 = EDGE_LOOP ( 'NONE', ( #94525, #98545, #34522, #24485, #62472, #52694, #28660, #13744 ) ) ;
#38094 = CARTESIAN_POINT ( 'NONE',  ( 10.75039077348039918, 1481.132873321739908, 213.9959934367710161 ) ) ;
#38095 = CARTESIAN_POINT ( 'NONE',  ( 13.51730467772499722, 1443.864691789369090, 188.0480164084754904 ) ) ;
#38096 = ORIENTED_EDGE ( 'NONE', *, *, #34468, .T. ) ;
#38097 = ORIENTED_EDGE ( 'NONE', *, *, #2105, .F. ) ;
#38098 = CARTESIAN_POINT ( 'NONE',  ( 2.580915939757335575, 1524.130440953581001, 175.8924427158433446 ) ) ;
#38099 = CARTESIAN_POINT ( 'NONE',  ( -2.672221962908839732, 1508.496458072200085, 220.4565680788469990 ) ) ;
#38100 = CARTESIAN_POINT ( 'NONE',  ( 12.71039585379999970, 1507.471771701229954, 233.3404624238980034 ) ) ;
#38101 = CARTESIAN_POINT ( 'NONE',  ( -6.488950515515869988, 1468.824231596619939, 218.3969576502859979 ) ) ;
#38102 = CARTESIAN_POINT ( 'NONE',  ( 14.55389011864330051, 1452.404827345299964, 148.1692795786860017 ) ) ;
#38103 = CARTESIAN_POINT ( 'NONE',  ( 8.757425179709999341, 1421.002068976639976, 196.4497576583989940 ) ) ;
#38104 = CARTESIAN_POINT ( 'NONE',  ( 1.831535152954090195, 1474.831757411260014, 220.3926950305869923 ) ) ;
#38105 = DIRECTION ( 'NONE',  ( 0.000000000000000000, 0.000000000000000000, -1.000000000000000000 ) ) ;
#38106 = DIRECTION ( 'NONE',  ( 0.000000000000000000, 1.000000000000000000, 0.000000000000000000 ) ) ;
#38107 = CARTESIAN_POINT ( 'NONE',  ( 0.03486440002950671330, 1409.388410587884891, 232.8483323310555591 ) ) ;
#38109 = DIRECTION ( 'NONE',  ( -0.000000000000000000, -0.000000000000000000, 1.000000000000000000 ) ) ;
#38108 = CARTESIAN_POINT ( 'NONE',  ( -12.68088003869999980, 1503.103876362690016, 208.6356514325480020 ) ) ;
#38110 = CARTESIAN_POINT ( 'NONE',  ( -43.47249194638170877, 1379.734446419809728, 233.2730947036674820 ) ) ;
#38111 = CARTESIAN_POINT ( 'NONE',  ( -24.30503083389229602, 1508.888284146479918, 222.4513817739089916 ) ) ;
#38112 = CARTESIAN_POINT ( 'NONE',  ( -6.597706052855000003, 1512.335510084600173, 201.0409955017370010 ) ) ;
#38113 = VERTEX_POINT ( 'NONE', #93395 ) ;
#38114 = CARTESIAN_POINT ( 'NONE',  ( 7.553102826339999964, 1423.481562109630204, 234.3916895958979865 ) ) ;
#38115 = CARTESIAN_POINT ( 'NONE',  ( 21.38516915557986309, 1501.977400791986611, 237.8497028174237471 ) ) ;
#38116 = CARTESIAN_POINT ( 'NONE',  ( -86.43489313709348210, 1384.977908500060039, 307.3521131436049814 ) ) ;
#38117 = CARTESIAN_POINT ( 'NONE',  ( 4.944136252469999881, 1506.455065028490026, 219.6922201799989693 ) ) ;
#38118 = CARTESIAN_POINT ( 'NONE',  ( 43.03456162790020301, 1428.697681977020011, 269.7258210693699993 ) ) ;
#38120 = VERTEX_POINT ( 'NONE', #42446 ) ;
#38119 = CARTESIAN_POINT ( 'NONE',  ( 3.387394683297223708, 1486.863201838490568, 198.4078931434325455 ) ) ;
#38121 = CARTESIAN_POINT ( 'NONE',  ( 1.529315676469999774, 1429.868337973490043, 217.3144367521890103 ) ) ;
#38122 = DIRECTION ( 'NONE',  ( 0.000000000000000000, 0.000000000000000000, 1.000000000000000000 ) ) ;
#38123 = CARTESIAN_POINT ( 'NONE',  ( -1.074557793710971598, 1450.811636816389637, 154.2492438910815622 ) ) ;
#38125 = EDGE_CURVE ( 'NONE', #102452, #89999, #63914, .T. ) ;
#38124 = CARTESIAN_POINT ( 'NONE',  ( 0.6998493108949769281, 1430.651357711089986, 199.7101808117699875 ) ) ;
#38126 = CARTESIAN_POINT ( 'NONE',  ( 15.02579302773500025, 1513.907445464710236, 224.5270601239670043 ) ) ;
#38127 = FACE_OUTER_BOUND ( 'NONE', #55597, .T. ) ;
#38128 = CARTESIAN_POINT ( 'NONE',  ( 18.75982378228949798, 1509.568167869620083, 185.1556198730530127 ) ) ;
#38129 = CARTESIAN_POINT ( 'NONE',  ( 4.455250013253990282, 1458.875479649829913, 200.5222135128619811 ) ) ;
#38130 = CARTESIAN_POINT ( 'NONE',  ( 12.01847341019976589, 1433.726575741404076, 149.8323943637946059 ) ) ;
#38131 = CARTESIAN_POINT ( 'NONE',  ( 15.32255284400000050, 1419.766531890930082, 227.7483529289979742 ) ) ;
#38132 = CARTESIAN_POINT ( 'NONE',  ( -21.19880661588965509, 1526.382868172863937, 233.5487980989313712 ) ) ;
#38133 = CARTESIAN_POINT ( 'NONE',  ( -3.463767296015000330, 1517.014196759610059, 207.4190915607570105 ) ) ;
#38134 = CARTESIAN_POINT ( 'NONE',  ( 41.00899597450000300, 1425.451880489129962, 269.1035016206980117 ) ) ;
#38135 = CARTESIAN_POINT ( 'NONE',  ( -18.21389191229999938, 1409.549103508730013, 222.3583561910980109 ) ) ;
#38136 = CARTESIAN_POINT ( 'NONE',  ( 19.62004841539999944, 1435.182524171729938, 143.5804541147979876 ) ) ;
#38137 = CARTESIAN_POINT ( 'NONE',  ( 25.45525579099999902, 1488.577326412729917, 202.6760865476379934 ) ) ;
#38138 = CARTESIAN_POINT ( 'NONE',  ( 24.57285633690000282, 1439.622216053659940, 213.1838506830980009 ) ) ;
#38139 = ADVANCED_FACE ( 'NONE', ( #15565 ), #66106, .F. ) ;
#38140 = CARTESIAN_POINT ( 'NONE',  ( -0.3382973561789999750, 1475.836249162829972, 266.9611136385980217 ) ) ;
#38141 = FACE_OUTER_BOUND ( 'NONE', #45534, .T. ) ;
#38142 = CARTESIAN_POINT ( 'NONE',  ( -39.20985834264440228, 1439.158936599190156, 136.6284022834660163 ) ) ;
#38143 = CARTESIAN_POINT ( 'NONE',  ( 0.2084417785648140231, 1458.224878346390142, 183.0292437909860155 ) ) ;
#38144 = CARTESIAN_POINT ( 'NONE',  ( -13.84827599230330009, 1408.877987748370060, 207.9041386013730346 ) ) ;
#38145 = CARTESIAN_POINT ( 'NONE',  ( 9.564625103933238393, 1428.147876255639858, 212.3796509962729715 ) ) ;
#38146 = B_SPLINE_CURVE_WITH_KNOTS ( 'NONE', 3,
 ( #107205, #90949, #14235, #48424 ),
 .UNSPECIFIED., .F., .F.,
 ( 4, 4 ),
 ( 0.000000000000000000, 0.0002220129587134778832 ),
 .UNSPECIFIED. ) ;
#38147 = CARTESIAN_POINT ( 'NONE',  ( 19.33418355719898329, 1523.342713519622976, 179.0109766843270052 ) ) ;
#38148 = ADVANCED_FACE ( 'NONE', ( #70323 ), #43437, .F. ) ;
#38149 = CARTESIAN_POINT ( 'NONE',  ( -27.78647954532239694, 1508.087771980839989, 210.4724892245600074 ) ) ;
#38150 = CARTESIAN_POINT ( 'NONE',  ( -4.291175242752039765, 1446.971469842819943, 154.7965863647420122 ) ) ;
#38151 = CARTESIAN_POINT ( 'NONE',  ( -26.80765817130000173, 1436.328495614390022, 136.7303568460980046 ) ) ;
#38152 = CARTESIAN_POINT ( 'NONE',  ( 2.871913733999305940, 1466.359209332784530, 234.1530941677849569 ) ) ;
#38153 = ORIENTED_EDGE ( 'NONE', *, *, #19284, .F. ) ;
#38154 = FACE_OUTER_BOUND ( 'NONE', #66898, .T. ) ;
#38155 = FACE_OUTER_BOUND ( 'NONE', #39321, .T. ) ;
#38156 = CARTESIAN_POINT ( 'NONE',  ( -10.99776467329999896, 1492.242005317089934, 208.0361729597790088 ) ) ;
#38157 = CARTESIAN_POINT ( 'NONE',  ( -8.589458402129759307, 1436.797986341739943, 209.9032590128110201 ) ) ;
#38158 = CARTESIAN_POINT ( 'NONE',  ( 15.41405264505409889, 1509.425107283729858, 233.4982122163600309 ) ) ;
#38159 = CARTESIAN_POINT ( 'NONE',  ( -29.78098341020000106, 1466.870135787829895, 269.3614920601979748 ) ) ;
#38160 = CARTESIAN_POINT ( 'NONE',  ( -16.72308823676789657, 1489.783577386040179, 223.6951472220740129 ) ) ;
#38161 = CARTESIAN_POINT ( 'NONE',  ( 18.64672481370000057, 1416.851343898729965, 209.6839434896789669 ) ) ;
#38162 = CARTESIAN_POINT ( 'NONE',  ( -27.13474158619999699, 1509.190014537030038, 212.0481536874080177 ) ) ;
#38163 = CARTESIAN_POINT ( 'NONE',  ( -90.01802904232170022, 1384.619177581419990, 308.7061652526469970 ) ) ;
#38164 = CARTESIAN_POINT ( 'NONE',  ( -36.70638529991089882, 1384.982332475140083, 210.0042769290089950 ) ) ;
#38165 = CARTESIAN_POINT ( 'NONE',  ( -7.980162481601299262, 1424.786834349992887, 210.5240428619318322 ) ) ;
#38166 = CARTESIAN_POINT ( 'NONE',  ( 20.59686811859999978, 1507.763399985229853, 227.6863920494979823 ) ) ;
#38167 = CARTESIAN_POINT ( 'NONE',  ( -29.68037260229820262, 1509.976800595009991, 208.5710708581900121 ) ) ;
#38168 = FACE_OUTER_BOUND ( 'NONE', #82223, .T. ) ;
#38170 = VERTEX_POINT ( 'NONE', #78687 ) ;
#38169 = CARTESIAN_POINT ( 'NONE',  ( 0.5019399832390400995, 1413.804834606910163, 184.9224728268669935 ) ) ;
#38171 = CARTESIAN_POINT ( 'NONE',  ( -12.37364323390000109, 1509.415518769829987, 181.8814867841980174 ) ) ;
#38172 = DIRECTION ( 'NONE',  ( 1.000000000000000000, -0.000000000000000000, 1.224646799147353207E-16 ) ) ;
#38173 = EDGE_CURVE ( 'NONE', #98691, #2271, #54716, .T. ) ;
#38174 = LINE ( 'NONE', #11882, #103401 ) ;
#38175 = CARTESIAN_POINT ( 'NONE',  ( -12.15086845379999936, 1416.067629296030191, 194.7798609157979968 ) ) ;
#38176 = CARTESIAN_POINT ( 'NONE',  ( -1.412825010259999736, 1422.092295416799743, 193.3406738546989914 ) ) ;
#38177 = CARTESIAN_POINT ( 'NONE',  ( 22.07912570460000268, 1409.684080446629878, 211.6989830675280189 ) ) ;
#38178 = CARTESIAN_POINT ( 'NONE',  ( -106.4682402945449979, 1391.913060387289988, 304.9855591817990330 ) ) ;
#38179 = CARTESIAN_POINT ( 'NONE',  ( 1.080077838119999800, 1463.747891711090006, 230.5571479593990034 ) ) ;
#38180 = CARTESIAN_POINT ( 'NONE',  ( -15.81258200789999790, 1421.897701213729988, 227.3576972447979756 ) ) ;
#38182 = CARTESIAN_POINT ( 'NONE',  ( -12.47403649690000016, 1380.456715030230043, 204.1115024872290178 ) ) ;
#38181 = CARTESIAN_POINT ( 'NONE',  ( -11.30563979010000075, 1432.585777830499865, 151.5215853277979932 ) ) ;
#38183 = CARTESIAN_POINT ( 'NONE',  ( 20.98459803409886959, 1522.051704408389924, 216.7582258867871587 ) ) ;
#38184 = CARTESIAN_POINT ( 'NONE',  ( 41.95590887306681793, 1512.187213306747481, 225.5974093378518148 ) ) ;
#38185 = CARTESIAN_POINT ( 'NONE',  ( 16.62993785878378006, 1526.306647125542895, 235.0749286977620045 ) ) ;
#38186 = CARTESIAN_POINT ( 'NONE',  ( -1.435685682569999955, 1417.080663547029872, 233.9312154598979987 ) ) ;
#38187 = CARTESIAN_POINT ( 'NONE',  ( 3.426613460960000079, 1360.656565846699777, 210.6218459616991936 ) ) ;
#38188 = CARTESIAN_POINT ( 'NONE',  ( 1.703779605225000049, 1517.057265928030120, 205.0766634521770015 ) ) ;
#38189 = CARTESIAN_POINT ( 'NONE',  ( -18.38030196201400202, 1485.844866795689995, 189.0206862885210057 ) ) ;
#38190 = ORIENTED_EDGE ( 'NONE', *, *, #28902, .T. ) ;
#38191 = CARTESIAN_POINT ( 'NONE',  ( -8.619814553459999473, 1424.664384728270079, 205.6756477520589783 ) ) ;
#38192 = CARTESIAN_POINT ( 'NONE',  ( -11.41393124623838773, 1422.045517156225287, 210.6385245698202198 ) ) ;
#38194 = ORIENTED_EDGE ( 'NONE', *, *, #46003, .F. ) ;
#38193 = CARTESIAN_POINT ( 'NONE',  ( -67.60933340069999531, 1379.747570940439800, 278.8523720603590164 ) ) ;
#38195 = ORIENTED_EDGE ( 'NONE', *, *, #29511, .T. ) ;
#38196 = CARTESIAN_POINT ( 'NONE',  ( 28.07231212390000152, 1508.101920094730076, 210.4687657402579930 ) ) ;
#38197 = ORIENTED_EDGE ( 'NONE', *, *, #38357, .T. ) ;
#38198 = CARTESIAN_POINT ( 'NONE',  ( 2.994586639156319841, 1484.901524374630299, 220.5882564702210118 ) ) ;
#38199 = DIRECTION ( 'NONE',  ( -0.7122454525621805255, 0.000000000000000000, -0.7019304917899598095 ) ) ;
#38201 = CARTESIAN_POINT ( 'NONE',  ( 20.34226454299999887, 1454.597587043530211, 225.1509561457980340 ) ) ;
#38200 = CARTESIAN_POINT ( 'NONE',  ( 15.96313815125649782, 1420.408442670840031, 191.2218829645730125 ) ) ;
#38202 = DIRECTION ( 'NONE',  ( 0.000000000000000000, 0.000000000000000000, 1.000000000000000000 ) ) ;
#38203 = CARTESIAN_POINT ( 'NONE',  ( -25.12509679820039921, 1451.311955931910006, 137.4238367825970215 ) ) ;
#38204 = CARTESIAN_POINT ( 'NONE',  ( 12.84239221398829933, 1435.935692713660046, 150.8114773724069835 ) ) ;
#38205 = CARTESIAN_POINT ( 'NONE',  ( 5.852848188970000365, 1410.053989038129885, 231.0988934593979991 ) ) ;
#38206 = CARTESIAN_POINT ( 'NONE',  ( 8.208364431944110251, 1484.299506827869891, 216.1663257859750047 ) ) ;
#38207 =( NAMED_UNIT ( * ) SI_UNIT ( $, .STERADIAN. ) SOLID_ANGLE_UNIT ( ) );
#38208 = CARTESIAN_POINT ( 'NONE',  ( 40.27155789680160325, 1448.225093240230080, 134.0999999982899737 ) ) ;
#38209 = CARTESIAN_POINT ( 'NONE',  ( -113.4000000000000057, 1384.926148861439970, 304.2218459572590064 ) ) ;
#38210 = ORIENTED_EDGE ( 'NONE', *, *, #40056, .F. ) ;
#38211 = CARTESIAN_POINT ( 'NONE',  ( 14.17511321471899954, 1428.761346845179787, 195.0897062075739825 ) ) ;
#38212 = CARTESIAN_POINT ( 'NONE',  ( -15.68560764121220252, 1410.853875961199947, 226.7268370761429992 ) ) ;
#38213 = ORIENTED_EDGE ( 'NONE', *, *, #101461, .T. ) ;
#38214 = ORIENTED_EDGE ( 'NONE', *, *, #17330, .F. ) ;
#38215 = VERTEX_POINT ( 'NONE', #42322 ) ;
#38216 = AXIS2_PLACEMENT_3D ( 'NONE', #15725, #39867, #98665 ) ;
#38217 = CARTESIAN_POINT ( 'NONE',  ( 9.847354017823224837, 1410.631711604590237, 229.8729602667554559 ) ) ;
#38218 = CARTESIAN_POINT ( 'NONE',  ( 0.000000000000000000, 1402.754281879943164, 135.5999999980979851 ) ) ;
#38219 = CARTESIAN_POINT ( 'NONE',  ( 3.388329910033260006, 1451.546035976184839, 153.9285079010525124 ) ) ;
#38220 = CARTESIAN_POINT ( 'NONE',  ( -8.861481481760000278, 1384.950957064560043, 218.6848129458689982 ) ) ;
#38221 = CARTESIAN_POINT ( 'NONE',  ( -17.50616331224802735, 1448.242994606246612, 218.0980532679095063 ) ) ;
#38222 = CARTESIAN_POINT ( 'NONE',  ( -68.43253263535059716, 1379.747293324333214, 279.3372337453455998 ) ) ;
#38223 = CARTESIAN_POINT ( 'NONE',  ( 0.8851935269000009709, 1465.434339089689956, 198.5254376396989926 ) ) ;
#38224 = DIRECTION ( 'NONE',  ( 1.171491307323471973E-14, 1.000000000000000000, -1.371895365494980038E-14 ) ) ;
#38225 = CARTESIAN_POINT ( 'NONE',  ( 1.546874264509999986, 1416.828040557830036, 190.2227689706980129 ) ) ;
#38226 = CARTESIAN_POINT ( 'NONE',  ( -53.73769481676529836, 1384.637522084219881, 231.5445279993439840 ) ) ;
#38227 = VERTEX_POINT ( 'NONE', #76475 ) ;
#38228 = CARTESIAN_POINT ( 'NONE',  ( -2.494020320564999782, 1516.876240617270014, 206.8389307488369866 ) ) ;
#38229 = ORIENTED_EDGE ( 'NONE', *, *, #15751, .T. ) ;
#38230 = CARTESIAN_POINT ( 'NONE',  ( 25.94212426325589860, 1440.913060387330006, 242.0455472739620006 ) ) ;
#38231 = FACE_OUTER_BOUND ( 'NONE', #23340, .T. ) ;
#38232 = ORIENTED_EDGE ( 'NONE', *, *, #3811, .F. ) ;
#38233 = LINE ( 'NONE', #72957, #3465 ) ;
#38234 = CARTESIAN_POINT ( 'NONE',  ( -16.14044004459999826, 1410.408804127830081, 191.4391529896979876 ) ) ;
#38235 = CARTESIAN_POINT ( 'NONE',  ( -108.6616353267809956, 1383.758284946439971, 311.0749865448200353 ) ) ;
#38237 = DIRECTION ( 'NONE',  ( 0.000000000000000000, 0.000000000000000000, 1.000000000000000000 ) ) ;
#38236 = CARTESIAN_POINT ( 'NONE',  ( -24.39250185919999936, 1440.969627941150065, 211.3361222571480198 ) ) ;
#38238 = CARTESIAN_POINT ( 'NONE',  ( -5.244363409054339620, 1434.381075504319824, 217.2110953212229845 ) ) ;
#38239 = AXIS2_PLACEMENT_3D ( 'NONE', #71161, #72795, #38077 ) ;
#38240 = CARTESIAN_POINT ( 'NONE',  ( 13.46831950203149830, 1436.161406562190223, 150.5249638017590144 ) ) ;
#38241 = CARTESIAN_POINT ( 'NONE',  ( 3.757756526780000161, 1406.106055978829772, 266.9554538344980301 ) ) ;
#38242 = CARTESIAN_POINT ( 'NONE',  ( -113.4000000000000057, 1379.913060387289988, 304.2218459572590064 ) ) ;
#38243 = CARTESIAN_POINT ( 'NONE',  ( -20.60985939166342007, 1525.581535527372353, 181.7364793965089405 ) ) ;
#38245 = CARTESIAN_POINT ( 'NONE',  ( 2.121334001142850118E-11, 1407.752913430750141, 267.9039250724300132 ) ) ;
#38244 = CARTESIAN_POINT ( 'NONE',  ( 6.226325556679999984, 1465.716049800030078, 233.5720425652980055 ) ) ;
#38246 = CARTESIAN_POINT ( 'NONE',  ( -3.452289220704999551, 1517.069378699710114, 215.6835323934670328 ) ) ;
#38247 = CARTESIAN_POINT ( 'NONE',  ( -0.1976107320300010128, 1469.705836264889967, 216.4285800060690121 ) ) ;
#38248 = CYLINDRICAL_SURFACE ( 'NONE', #78607, 1.999999999999999556 ) ;
#38249 = CARTESIAN_POINT ( 'NONE',  ( 19.18867383189600417, 1443.582650154266503, 213.4775594393471749 ) ) ;
#38251 = B_SPLINE_CURVE_WITH_KNOTS ( 'NONE', 5,
 ( #33389, #49129, #50234, #8743, #24982, #93308 ),
 .UNSPECIFIED., .F., .F.,
 ( 6, 6 ),
 ( 4.250950522270000143, 7.082025451739999866 ),
 .UNSPECIFIED. ) ;
#38250 = CARTESIAN_POINT ( 'NONE',  ( -3.252530653725000054, 1516.827328999679821, 212.0018028951869837 ) ) ;
#38252 = CARTESIAN_POINT ( 'NONE',  ( -21.39582113410000019, 1488.805759879029893, 208.9522497871160169 ) ) ;
#38253 = CARTESIAN_POINT ( 'NONE',  ( -4.041144483454799818, 1483.296311158560002, 199.2628329227509880 ) ) ;
#38255 = EDGE_LOOP ( 'NONE', ( #107737, #19940, #8758, #59553, #109830 ) ) ;
#38254 = CARTESIAN_POINT ( 'NONE',  ( -16.76078030769999927, 1420.494757909599912, 203.1294657649889928 ) ) ;
#38256 = CARTESIAN_POINT ( 'NONE',  ( -8.156522882179999101, 1384.901372997500175, 199.6468678763889955 ) ) ;
#38257 = CARTESIAN_POINT ( 'NONE',  ( 2.174183498839999729, 1508.551704408389924, 219.6416074559989795 ) ) ;
#38258 = CARTESIAN_POINT ( 'NONE',  ( -8.494709133442391646, 1488.072329454872261, 217.7903042299439562 ) ) ;
#38259 = CARTESIAN_POINT ( 'NONE',  ( -26.09830977477409775, 1509.824433447099864, 222.5363761071970146 ) ) ;
#38260 = CARTESIAN_POINT ( 'NONE',  ( -0.4599427841477299883, 1508.922901691350035, 238.6016026774880174 ) ) ;
#38261 = FACE_OUTER_BOUND ( 'NONE', #31195, .T. ) ;
#38262 = CARTESIAN_POINT ( 'NONE',  ( 12.76595157039999862, 1446.243769161290174, 188.3984060521979984 ) ) ;
#38264 = CARTESIAN_POINT ( 'NONE',  ( 12.98226713004290112, 1414.913060387349788, 198.3280232619060257 ) ) ;
#38263 = CARTESIAN_POINT ( 'NONE',  ( -24.08426305480000451, 1411.115211393229856, 208.6111285346999864 ) ) ;
#38265 = CARTESIAN_POINT ( 'NONE',  ( -14.08142637225379978, 1379.709117121690042, 211.5303641152310092 ) ) ;
#38266 = ORIENTED_EDGE ( 'NONE', *, *, #60045, .F. ) ;
#38267 = CARTESIAN_POINT ( 'NONE',  ( -4.040527342105000308, 1516.815231249920089, 204.5109077207270047 ) ) ;
#38268 = CARTESIAN_POINT ( 'NONE',  ( 2.776430554999999689, 1405.810978695030144, 267.5339349680979808 ) ) ;
#38269 = CARTESIAN_POINT ( 'NONE',  ( 1.842963808589999974, 1515.492058141890084, 213.2603893764890017 ) ) ;
#38270 = B_SPLINE_CURVE_WITH_KNOTS ( 'NONE', 3,
 ( #81780, #96406, #89096, #54970, #71233, #28089, #88562, #19682, #56052, #106451, #106992, #29734, #11846, #63920, #98589, #36493 ),
 .UNSPECIFIED., .F., .F.,
 ( 4, 2, 2, 2, 2, 2, 2, 4 ),
 ( 8.544639080107319913E-08, 0.4101168854422549970, 0.8109689984529260265, 1.212505501424880006, 1.416242740394599853, 1.518121827656090161, 1.569055395889600080, 1.620000854487389841 ),
 .UNSPECIFIED. ) ;
#38271 = B_SPLINE_CURVE_WITH_KNOTS ( 'NONE', 3,
 ( #17118, #101689, #50762, #24980, #85443, #8190, #62950, #53983, #96502, #53410, #42356, #45022, #37145, #33387, #36053, #105456, #10850, #87561, #79167, #77081, #36592, #70789, #16567, #28745, #67583, #95948, #59186, #11406, #84898, #93305, #110660, #88117, #59727, #68147, #93846, #28190, #33953, #62376, #104347, #97061, #42924, #102257, #61825, #41806, #104901, #70240, #20326, #45574, #25536, #27640, #389, #51306, #79716, #19208, #19782, #3023, #54531, #7649, #75963, #99225 ),
 .UNSPECIFIED., .F., .F.,
 ( 4, 2, 2, 2, 2, 2, 2, 1, 1, 1, 1, 1, 1, 2, 2, 2, 2, 2, 2, 2, 1, 1, 1, 1, 1, 1, 2, 2, 2, 2, 2, 2, 2, 2, 2, 4 ),
 ( 0.000000000000000000, 0.06249999999921360128, 0.1249999999984272026, 0.1874999999976408038, 0.2187499999972475906, 0.2343749999970505260, 0.2421874999969520492, 0.2460937499969024223, 0.2480468749968771647, 0.2490234374968641196, 0.2495117187468572084, 0.2497558593718541831, 0.2498779296843522402, 0.2499389648406012965, 0.2499999999968503250, 0.3124999999970974884, 0.3749999999973447351, 0.4374999999975927589, 0.4687499999977168263, 0.4843749999977786103, 0.4921874999978098630, 0.4960937499978254617, 0.4980468749978333443, 0.4990234374978368970, 0.4995117187478387843, 0.4997558593728400056, 0.4998779296853406162, 0.4999999999978411713, 0.5624999999981110665, 0.6249999999983808507, 0.6874999999986507460, 0.7499999999989206412, 0.8124999999991905364, 0.8749999999994603206, 0.9374999999997302158, 1.000000000000000000 ),
 .UNSPECIFIED. ) ;
#38272 = CARTESIAN_POINT ( 'NONE',  ( 6.690595718171389983, 1474.175196074600080, 270.1377304235489873 ) ) ;
#38273 = CARTESIAN_POINT ( 'NONE',  ( -0.3555850868473771631, 1463.527481276508070, 199.3363023076782952 ) ) ;
#38274 =( BOUNDED_SURFACE ( )  B_SPLINE_SURFACE ( 3, 2, ( 
 ( #82316, #49280, #81202 ),
 ( #38652, #72827, #106960 ),
 ( #64439, #5614, #73927 ),
 ( #98555, #21824, #57139 ),
 ( #90148, #91267, #13430 ),
 ( #108057, #73374, #31353 ),
 ( #9466, #109722, #59890 ),
 ( #94559, #86173, #8902 ),
 ( #1091, #84515, #17278 ),
 ( #110820, #33539, #32999 ),
 ( #103514, #26818, #41425 ),
 ( #110263, #50387, #60441 ),
 ( #102411, #25693, #52037 ),
 ( #25141, #24582, #43631 ) ),
 .UNSPECIFIED., .F., .F., .T. ) 
 B_SPLINE_SURFACE_WITH_KNOTS ( ( 4, 2, 2, 2, 2, 2, 4 ),
 ( 3, 3 ),
 ( 2.424276057677587914E-16, 0.0009443072508238471762, 0.001416460876235649605, 0.001888614501647451925, 0.002360768127059254245, 0.002832921752471056782, 0.003777229003294661422 ),
 ( 0.000000000000000000, 1.000000000000000000 ),
 .UNSPECIFIED. ) 
 GEOMETRIC_REPRESENTATION_ITEM ( )  RATIONAL_B_SPLINE_SURFACE ( (
 ( 1.000000000000000000, 0.9376006582765967767, 1.000000000000000000),
 ( 1.000000000000000000, 0.9283977714668572023, 1.000000000000000000),
 ( 1.000000000000000000, 0.9189750060570894830, 1.000000000000000000),
 ( 1.000000000000000000, 0.9042792056081997432, 1.000000000000000000),
 ( 1.000000000000000000, 0.8992469033881916873, 1.000000000000000000),
 ( 1.000000000000000000, 0.8891280264643571796, 1.000000000000000000),
 ( 1.000000000000000000, 0.8840337471673896941, 1.000000000000000000),
 ( 1.000000000000000000, 0.8736395124165009518, 1.000000000000000000),
 ( 1.000000000000000000, 0.8683406746555940581, 1.000000000000000000),
 ( 1.000000000000000000, 0.8573361860704523663, 1.000000000000000000),
 ( 1.000000000000000000, 0.8516508399500207771, 1.000000000000000000),
 ( 1.000000000000000000, 0.8340914917058259714, 1.000000000000000000),
 ( 1.000000000000000000, 0.8215597275867865257, 1.000000000000000000),
 ( 1.000000000000000000, 0.8070209408750127489, 1.000000000000000000) ) ) 
 REPRESENTATION_ITEM ( '' )  SURFACE ( )  );
#38275 = CARTESIAN_POINT ( 'NONE',  ( 11.60004869885879231, 1423.657548013328096, 137.0691450735224350 ) ) ;
#38276 = CARTESIAN_POINT ( 'NONE',  ( -6.057897975499958676, 1440.290016138275178, 202.7497801027471382 ) ) ;
#38277 = CARTESIAN_POINT ( 'NONE',  ( -6.617556317490000062, 1459.313145877689976, 217.6703565655190005 ) ) ;
#38278 = CARTESIAN_POINT ( 'NONE',  ( -1.636727350584959773, 1450.664746045244556, 183.2094855785913978 ) ) ;
#38279 = CARTESIAN_POINT ( 'NONE',  ( 2.431405075025240059, 1449.537433731769852, 154.7921670947710027 ) ) ;
#38280 = CARTESIAN_POINT ( 'NONE',  ( -13.69065454899539880, 1415.152886233429854, 220.6114883211280073 ) ) ;
#38281 = CARTESIAN_POINT ( 'NONE',  ( -4.329448786299999519, 1515.064792490889886, 210.9648092169189795 ) ) ;
#38282 = ORIENTED_EDGE ( 'NONE', *, *, #49655, .T. ) ;
#38283 = CARTESIAN_POINT ( 'NONE',  ( -30.40113726520000270, 1433.623945462319853, 255.3819207682979595 ) ) ;
#38284 = CIRCLE ( 'NONE', #63347, 7.500000000000000000 ) ;
#38285 = CARTESIAN_POINT ( 'NONE',  ( 4.269304843480000500, 1441.143128249819938, 158.1185154358979901 ) ) ;
#38286 = CARTESIAN_POINT ( 'NONE',  ( -0.2126388994629999918, 1475.048161703429969, 269.6500587019980344 ) ) ;
#38287 = CARTESIAN_POINT ( 'NONE',  ( -28.53738135360000072, 1451.916516915729972, 134.8736009463979997 ) ) ;
#38288 = DIRECTION ( 'NONE',  ( 0.000000000000000000, 1.000000000000000000, 0.000000000000000000 ) ) ;
#38289 = CARTESIAN_POINT ( 'NONE',  ( -2.976586033138599596, 1448.268719613186704, 184.4363391144643458 ) ) ;
#38290 = CARTESIAN_POINT ( 'NONE',  ( -31.26379401350899556, 1384.823741200369795, 229.4291413252929885 ) ) ;
#38291 = AXIS2_PLACEMENT_3D ( 'NONE', #41630, #24256, #85265 ) ;
#38292 = B_SPLINE_SURFACE_WITH_KNOTS ( 'NONE', 5, 5, ( 
 ( #58240, #73937, #81759, #41437, #33013, #32483, #57152, #108069, #67199 ),
 ( #99656, #83419, #99108, #66655, #6715, #40871, #24047, #5627, #64990 ),
 ( #22385, #101298, #23512, #82870, #100233, #65547, #75047, #91277, #90160 ),
 ( #109199, #24593, #48747, #13441, #57705, #6164, #56585, #90719, #40318 ),
 ( #74500, #92364, #47631, #15637, #5063, #39210, #14003, #31916, #66108 ),
 ( #42525, #76134, #51485, #102967, #68313, #33552, #61985, #76680, #85615 ),
 ( #16197, #551, #67749, #59356, #8915, #94026, #101241, #102422, #34124 ),
 ( #59905, #101859, #110276, #25703, #17289, #68863, #58786, #92925, #43090 ),
 ( #77251, #41985, #85068, #34675, #27799, #96101, #50398, #25153, #84527 ) ),
 .UNSPECIFIED., .F., .F., .F.,
 ( 6, 3, 6 ),
 ( 6, 3, 6 ),
 ( 3.495303171621910288, 6.017914243079999892, 8.540525314547538827 ),
 ( 0.000000000000000000, 1.500000000000000000, 3.000238679058089719 ),
 .UNSPECIFIED. ) ;
#38293 = CARTESIAN_POINT ( 'NONE',  ( 12.05020405772690140, 1491.375760444399930, 206.7358482363899839 ) ) ;
#38294 = CARTESIAN_POINT ( 'NONE',  ( 32.38114538885255200, 1523.604703353109926, 216.1203639561428815 ) ) ;
#38295 = CARTESIAN_POINT ( 'NONE',  ( 8.220025357896366458, 1511.455724274470640, 205.0451695456004870 ) ) ;
#38296 = CARTESIAN_POINT ( 'NONE',  ( -5.980973321690750133, 1396.121920580289952, 218.4025002956929882 ) ) ;
#38297 = B_SPLINE_CURVE_WITH_KNOTS ( 'NONE', 3,
 ( #97674, #79792, #54058, #88735 ),
 .UNSPECIFIED., .F., .F.,
 ( 4, 4 ),
 ( -19.11832560899999933, -0.3666095563249989198 ),
 .UNSPECIFIED. ) ;
#38298 = CARTESIAN_POINT ( 'NONE',  ( -15.35996473989999878, 1420.804668691529969, 227.0340416244980020 ) ) ;
#38299 = CARTESIAN_POINT ( 'NONE',  ( 19.28298846601172301, 1455.999974110760149, 225.1882103107009243 ) ) ;
#38300 = ORIENTED_EDGE ( 'NONE', *, *, #3790, .F. ) ;
#38301 = CARTESIAN_POINT ( 'NONE',  ( -11.33207981915198204, 1503.013677552742820, 207.0720892954946635 ) ) ;
#38302 = CARTESIAN_POINT ( 'NONE',  ( 2.923521583079999875, 1410.394928893030283, 231.6309338985980162 ) ) ;
#38303 = CARTESIAN_POINT ( 'NONE',  ( -9.624872151419999966, 1503.621315096290118, 228.8144366447990024 ) ) ;
#38305 = CARTESIAN_POINT ( 'NONE',  ( -13.32051257826499935, 1512.868709057579963, 192.3735960303669970 ) ) ;
#38304 = CARTESIAN_POINT ( 'NONE',  ( 10.97118381930000020, 1425.274992001930059, 132.2037382631980051 ) ) ;
#38306 = CARTESIAN_POINT ( 'NONE',  ( -5426.659192927121694, 54.07981494722833560, 8449.939230966660034 ) ) ;
#38307 = B_SPLINE_CURVE_WITH_KNOTS ( 'NONE', 3,
 ( #26007, #855, #9243, #8118, #110041, #60772, #25458, #94896, #18171, #34982, #34436, #52368, #43949, #67509, #17039, #76435, #24364, #84284, #42285, #60204, #110588, #102713, #78092, #94323, #85369, #8664, #1394, #101067, #66958, #59106, #85940, #92678, #15954, #33874, #101612, #50155, #16498, #68065, #42842, #7577 ),
 .UNSPECIFIED., .F., .F.,
 ( 4, 3, 3, 3, 3, 3, 3, 3, 3, 3, 3, 3, 3, 4 ),
 ( -168.5477118249999933, -162.5507363268910126, -153.8407794596359963, -144.7791047296130102, -135.4369637970760039, -125.4361478828139980, -114.7710760797919960, -103.0116084759360007, -88.20793680898479749, -73.11625194994489618, -61.36907839288639366, -50.68835095691321158, -40.67933903265419815, -31.15146013443029460 ),
 .UNSPECIFIED. ) ;
#38308 = CARTESIAN_POINT ( 'NONE',  ( -12.45478753333599720, 1442.762691980110048, 151.6226032058479802 ) ) ;
#38309 = ADVANCED_FACE ( 'NONE', ( #110628 ), #99106, .T. ) ;
#38310 = CARTESIAN_POINT ( 'NONE',  ( -109.9870827704239957, 1384.734719174579823, 311.4521501216929664 ) ) ;
#38311 = CARTESIAN_POINT ( 'NONE',  ( 7.513421685239999981, 1426.406794065100030, 212.3389288288790056 ) ) ;
#38312 = CARTESIAN_POINT ( 'NONE',  ( 16.50821402049999875, 1494.476688022989947, 193.0250027032990090 ) ) ;
#38313 = CARTESIAN_POINT ( 'NONE',  ( 7.327188678030000624, 1507.874256059229992, 182.6136352915980297 ) ) ;
#38314 = CARTESIAN_POINT ( 'NONE',  ( 7.585404386385000031, 1511.813148765560072, 206.6464469953870093 ) ) ;
#38315 = CARTESIAN_POINT ( 'NONE',  ( -70.05038419870359689, 1379.267308317730112, 286.2875064122259801 ) ) ;
#38316 = CARTESIAN_POINT ( 'NONE',  ( 8.355117317390414300, 1365.835232130580835, 210.6218459617142003 ) ) ;
#38318 = ORIENTED_EDGE ( 'NONE', *, *, #110279, .T. ) ;
#38317 = CARTESIAN_POINT ( 'NONE',  ( -14.06310996700590010, 1379.653384448290126, 211.5922490258780044 ) ) ;
#38319 = VERTEX_POINT ( 'NONE', #106093 ) ;
#38320 = PLANE ( 'NONE',  #98028 ) ;
#38321 = CARTESIAN_POINT ( 'NONE',  ( 2.925327306374799985, 1410.322647625880109, 231.6260571398940158 ) ) ;
#38322 = CARTESIAN_POINT ( 'NONE',  ( -1.396725214890000011, 1415.041103191730144, 226.7314491796980178 ) ) ;
#38323 = DIRECTION ( 'NONE',  ( -1.699538841806929935E-33, 1.000000000000000000, -1.698192320643030073E-16 ) ) ;
#38324 = CARTESIAN_POINT ( 'NONE',  ( 0.000000000000000000, 1452.913060387330006, 179.9625354400980086 ) ) ;
#38325 = CARTESIAN_POINT ( 'NONE',  ( -8.370529003654999300, 1511.388520542559945, 213.6642613602169831 ) ) ;
#38327 = CARTESIAN_POINT ( 'NONE',  ( 17.09102838100000099, 1413.530045447530028, 226.3661571205980181 ) ) ;
#38326 = CARTESIAN_POINT ( 'NONE',  ( -8.163788229310002365, 1383.802161292700021, 218.6403764234589744 ) ) ;
#38328 = CARTESIAN_POINT ( 'NONE',  ( 2.020974489129999885, 1410.305613295530065, 185.4468934685980059 ) ) ;
#38329 = CARTESIAN_POINT ( 'NONE',  ( -41.11424902454939456, 1444.666461503340088, 136.8180534356220051 ) ) ;
#38330 = CARTESIAN_POINT ( 'NONE',  ( 40.66801799462539435, 1442.602446576360080, 136.9833458737259946 ) ) ;
#38331 = DIRECTION ( 'NONE',  ( 0.000000000000000000, 0.000000000000000000, 1.000000000000000000 ) ) ;
#38332 = CARTESIAN_POINT ( 'NONE',  ( 33.27874934317770084, 1436.988425504300039, 136.5809431225799813 ) ) ;
#38333 = CARTESIAN_POINT ( 'NONE',  ( 11.28006282179999964, 1430.719829126430113, 151.3394816934979872 ) ) ;
#38334 = CARTESIAN_POINT ( 'NONE',  ( 41.14066506200000362, 1444.183247956199921, 136.8991343562979921 ) ) ;
#38335 = ORIENTED_EDGE ( 'NONE', *, *, #74662, .T. ) ;
#38336 = CARTESIAN_POINT ( 'NONE',  ( 4.055275498809999490, 1423.964747713630231, 184.0972450836979988 ) ) ;
#38337 = CARTESIAN_POINT ( 'NONE',  ( 11.78238132140000083, 1440.882651473599935, 188.1224434270980055 ) ) ;
#38338 = ORIENTED_EDGE ( 'NONE', *, *, #55256, .T. ) ;
#38339 = ORIENTED_EDGE ( 'NONE', *, *, #91995, .T. ) ;
#38340 = CARTESIAN_POINT ( 'NONE',  ( -4.961196303140000374, 1424.964372189380128, 209.4833162189939912 ) ) ;
#38341 = CARTESIAN_POINT ( 'NONE',  ( 11.33251049156513623, 1391.913060387289988, 208.6449207241230965 ) ) ;
#38342 = CARTESIAN_POINT ( 'NONE',  ( -13.89782283490000125, 1452.807100928030195, 194.8455099693979662 ) ) ;
#38343 = CARTESIAN_POINT ( 'NONE',  ( -29.55269881708372637, 1525.821544997590536, 197.1295836072968655 ) ) ;
#38344 = CARTESIAN_POINT ( 'NONE',  ( -5.776491133374999976, 1516.858301627840092, 214.9045953718370185 ) ) ;
#38345 = CARTESIAN_POINT ( 'NONE',  ( -14.39218230554089928, 1380.275882964069979, 209.3755301335680201 ) ) ;
#38346 = ORIENTED_EDGE ( 'NONE', *, *, #53726, .F. ) ;
#38347 = CARTESIAN_POINT ( 'NONE',  ( -14.32724710653639910, 1509.467756537190098, 183.0197988060039904 ) ) ;
#38348 = CARTESIAN_POINT ( 'NONE',  ( -37.92577313569999831, 1377.672836988610015, 218.5611944450689919 ) ) ;
#38349 = EDGE_CURVE ( 'NONE', #68340, #41530, #88747, .T. ) ;
#38350 = EDGE_CURVE ( 'NONE', #101907, #1545, #29371, .T. ) ;
#38351 = CARTESIAN_POINT ( 'NONE',  ( 15.44258166179999847, 1414.913060387329779, 214.5365335479179976 ) ) ;
#38352 = CARTESIAN_POINT ( 'NONE',  ( 6.549762446985000430, 1516.729202374750002, 204.5030968636170030 ) ) ;
#38353 = EDGE_LOOP ( 'NONE', ( #16512, #51704, #91551, #595 ) ) ;
#38354 = CARTESIAN_POINT ( 'NONE',  ( 7.513435694541056975, 1375.426148861440197, 209.1218459572589836 ) ) ;
#38355 = ADVANCED_FACE ( 'NONE', ( #79805 ), #89836, .T. ) ;
#38357 = EDGE_CURVE ( 'NONE', #109512, #17927, #1073, .T. ) ;
#38356 = CARTESIAN_POINT ( 'NONE',  ( -35.04400506982609187, 1424.099278616513175, 269.5321162145484095 ) ) ;
#38358 = CARTESIAN_POINT ( 'NONE',  ( -11.16950626350000064, 1409.469289622230008, 228.3240238616979809 ) ) ;
#38360 = ORIENTED_EDGE ( 'NONE', *, *, #82360, .F. ) ;
#38359 = CARTESIAN_POINT ( 'NONE',  ( -31.18494820112229249, 1524.152444737676660, 196.3673256080876968 ) ) ;
#38361 = CARTESIAN_POINT ( 'NONE',  ( 2.500000000000000000, 1419.446092955830181, 146.1320802672979937 ) ) ;
#38362 = CARTESIAN_POINT ( 'NONE',  ( -30.52556887503000027, 1440.913060387399810, 239.9851491244249928 ) ) ;
#38363 = AXIS2_PLACEMENT_3D ( 'NONE', #20858, #55055, #96486 ) ;
#38364 = CARTESIAN_POINT ( 'NONE',  ( -25.97701990859999910, 1384.174749255760162, 224.1963252206589914 ) ) ;
#38365 = DIRECTION ( 'NONE',  ( 0.8672669759446630655, 0.000000000000000000, -0.4978433412588735285 ) ) ;
#38366 = CARTESIAN_POINT ( 'NONE',  ( 24.89781524799989754, 1415.678878148830108, 269.9191937554660399 ) ) ;
#38367 = AXIS2_PLACEMENT_3D ( 'NONE', #108078, #38672, #49299 ) ;
#38368 = CARTESIAN_POINT ( 'NONE',  ( 2.297085715815000206, 1516.718889242609976, 213.1486234561869821 ) ) ;
#38369 = CARTESIAN_POINT ( 'NONE',  ( -67.44338435920001018, 1379.744787917099757, 277.3736694360590036 ) ) ;
#38370 = CIRCLE ( 'NONE', #100940, 17.27637083661241135 ) ;
#38371 = CARTESIAN_POINT ( 'NONE',  ( 23.16826695290000160, 1409.827445977929756, 208.5989265901500005 ) ) ;
#38372 = CARTESIAN_POINT ( 'NONE',  ( -8.113694374351904770, 1425.905879024222713, 225.6960958089561586 ) ) ;
#38373 = DIRECTION ( 'NONE',  ( 0.000000000000000000, 1.000000000000000000, -6.123233995736769734E-17 ) ) ;
#38374 = CARTESIAN_POINT ( 'NONE',  ( -7.715452159899959916, 1516.779489719169987, 209.6579840536579979 ) ) ;
#38375 = CARTESIAN_POINT ( 'NONE',  ( -7.713648872314999849, 1516.710624944440042, 209.8745175203999906 ) ) ;
#38376 = CARTESIAN_POINT ( 'NONE',  ( 0.2403276022373450060, 1424.313268885149910, 227.5210991795279938 ) ) ;
#38378 = EDGE_CURVE ( 'NONE', #79432, #53095, #19854, .T. ) ;
#38377 = CARTESIAN_POINT ( 'NONE',  ( -3.616492858290000001, 1417.910832933829852, 232.6758466721979914 ) ) ;
#38379 = CARTESIAN_POINT ( 'NONE',  ( -102.7375125960000020, 1384.595838641269893, 311.2202755702589911 ) ) ;
#38380 = ORIENTED_EDGE ( 'NONE', *, *, #61317, .F. ) ;
#38381 = CARTESIAN_POINT ( 'NONE',  ( -29.36584213358230144, 1385.236513890409924, 227.3793372904949877 ) ) ;
#38382 = CYLINDRICAL_SURFACE ( 'NONE', #99595, 1.000000000000001554 ) ;
#38383 = CARTESIAN_POINT ( 'NONE',  ( 0.7830886349010000025, 1415.510552653030118, 233.2794445565979800 ) ) ;
#38384 = EDGE_CURVE ( 'NONE', #6621, #106581, #110147, .T. ) ;
#38385 = CARTESIAN_POINT ( 'NONE',  ( -20.37003372361249731, 1507.842576381340223, 228.6074795959160042 ) ) ;
#38386 = CARTESIAN_POINT ( 'NONE',  ( 3.024787391539411242E-15, 1522.051704408389924, 184.4225825198192013 ) ) ;
#38387 = EDGE_CURVE ( 'NONE', #24269, #15596, #11491, .T. ) ;
#38388 = CARTESIAN_POINT ( 'NONE',  ( 11.00924500930000072, 1425.566778448970126, 205.8224405914690180 ) ) ;
#38389 = CARTESIAN_POINT ( 'NONE',  ( 9.862951377358559313, 1519.551704408389924, 189.8497022443989977 ) ) ;
#38391 = CARTESIAN_POINT ( 'NONE',  ( -7.989567385690000023, 1384.306347471770096, 199.5291465469090042 ) ) ;
#38390 = CARTESIAN_POINT ( 'NONE',  ( 7.718134629434999283, 1516.881930554049859, 216.4517759834270123 ) ) ;
#38392 = CARTESIAN_POINT ( 'NONE',  ( 4.163173891473259225, 1457.139433440971288, 199.2031176836267718 ) ) ;
#38393 = DIRECTION ( 'NONE',  ( 0.9455185755993178454, 0.000000000000000000, -0.3255681544571537578 ) ) ;
#38394 = ORIENTED_EDGE ( 'NONE', *, *, #94108, .F. ) ;
#38395 = CARTESIAN_POINT ( 'NONE',  ( -5.780232115465000042, 1516.760434454289907, 201.7950504087270076 ) ) ;
#38396 = CARTESIAN_POINT ( 'NONE',  ( -15.52404079726500008, 1511.843510977570077, 220.5312950707669870 ) ) ;
#38397 = VERTEX_POINT ( 'NONE', #63036 ) ;
#38398 = CARTESIAN_POINT ( 'NONE',  ( -14.72576942166499947, 1512.123542805230272, 221.3115653187670091 ) ) ;
#38399 = AXIS2_PLACEMENT_3D ( 'NONE', #85147, #86808, #52124 ) ;
#38400 = CARTESIAN_POINT ( 'NONE',  ( 22.59589508572869931, 1507.700907081449941, 227.3081682119560014 ) ) ;
#38401 = CARTESIAN_POINT ( 'NONE',  ( 7.653560456693386804, 1423.197433329561591, 195.7764355311638269 ) ) ;
#38402 = CARTESIAN_POINT ( 'NONE',  ( 2.366397864590000122, 1442.164712771990025, 218.0400648220289952 ) ) ;
#38403 = CARTESIAN_POINT ( 'NONE',  ( -26.85483190386980112, 1509.266232500709975, 201.3403652348490311 ) ) ;
#38404 = CARTESIAN_POINT ( 'NONE',  ( -2.499999987950000335, 1447.625363425740034, 167.4763715217980007 ) ) ;
#38405 = CARTESIAN_POINT ( 'NONE',  ( -19.81884662830000110, 1427.029209586630259, 224.1944963751980140 ) ) ;
#38406 = CARTESIAN_POINT ( 'NONE',  ( 8.189759204080917954, 1487.486609484756400, 202.0226346771893589 ) ) ;
#38407 = CARTESIAN_POINT ( 'NONE',  ( -9.675350337739999418, 1433.447543843880112, 148.7453054530979841 ) ) ;
#38408 = CARTESIAN_POINT ( 'NONE',  ( 16.97760447559999974, 1508.233635190930045, 188.0201034282980004 ) ) ;
#38410 = CARTESIAN_POINT ( 'NONE',  ( -18.49741831292255512, 1436.683225729171227, 212.7525086259309433 ) ) ;
#38409 = CARTESIAN_POINT ( 'NONE',  ( -106.0175964039999883, 1391.835588392369800, 302.7430365994590034 ) ) ;
#38411 = DIRECTION ( 'NONE',  ( -0.4709675661680092218, 0.8364468003938373419, 0.2802611313198711263 ) ) ;
#38412 = VERTEX_POINT ( 'NONE', #20410 ) ;
#38413 = CARTESIAN_POINT ( 'NONE',  ( -104.2041774089999961, 1379.825158453460062, 303.6443917302590307 ) ) ;
#38414 = CARTESIAN_POINT ( 'NONE',  ( -11.31089902619999954, 1508.551704403789927, 217.8497850877789972 ) ) ;
#38415 = CARTESIAN_POINT ( 'NONE',  ( 11.72470770320000000, 1437.821967610810134, 147.7443706334980220 ) ) ;
#38416 = CARTESIAN_POINT ( 'NONE',  ( 11.14978817083719953, 1470.287995331660113, 206.9593417752710138 ) ) ;
#38417 = CARTESIAN_POINT ( 'NONE',  ( -2.850336743489999769, 1485.269293374889912, 197.9872958246989754 ) ) ;
#38418 = CARTESIAN_POINT ( 'NONE',  ( 2.596261494520225366, 1525.907212628473644, 240.7735774411713123 ) ) ;
#38419 = CARTESIAN_POINT ( 'NONE',  ( -2.646287650837769956, 1525.055427061254704, 241.6502252480098605 ) ) ;
#38420 = CARTESIAN_POINT ( 'NONE',  ( -13.15646098871717129, 1443.074065570369839, 186.7349259480803596 ) ) ;
#38421 = B_SPLINE_SURFACE_WITH_KNOTS ( 'NONE', 5, 1, ( 
 ( #94247, #68533 ),
 ( #93683, #70601 ),
 ( #16962, #85290 ),
 ( #16418, #104719 ),
 ( #75813, #58465 ),
 ( #66878, #230 ) ),
 .UNSPECIFIED., .F., .F., .F.,
 ( 6, 6 ),
 ( 2, 2 ),
 ( 0.000000000000000000, 15.70013102750000122 ),
 ( 0.000000000000000000, 14.00000000000000000 ),
 .UNSPECIFIED. ) ;
#38422 = CARTESIAN_POINT ( 'NONE',  ( -17.09240173490840320, 1414.913527292460003, 207.6788998298750073 ) ) ;
#38423 = CARTESIAN_POINT ( 'NONE',  ( 4.874616599078260393, 1494.129475450019982, 219.3025786937440103 ) ) ;
#38424 = CARTESIAN_POINT ( 'NONE',  ( -3.071476887830000280, 1470.850261538789937, 187.3986309372990036 ) ) ;
#38425 = CARTESIAN_POINT ( 'NONE',  ( -15.44282314831900038, 1415.677402202029953, 209.4843333921439807 ) ) ;
#38426 = CARTESIAN_POINT ( 'NONE',  ( -9.532366409914120098, 1460.042444853610050, 210.5589214869069963 ) ) ;
#38427 = CARTESIAN_POINT ( 'NONE',  ( -0.4998264653690069892, 1516.789754148840075, 201.4061250449829856 ) ) ;
#38429 = ORIENTED_EDGE ( 'NONE', *, *, #38387, .T. ) ;
#38428 = DIRECTION ( 'NONE',  ( 0.000000000000000000, 1.000000000000000000, 0.000000000000000000 ) ) ;
#38430 = CARTESIAN_POINT ( 'NONE',  ( -109.9987473190000031, 1384.904025801279886, 297.1695833602590255 ) ) ;
#38431 = CARTESIAN_POINT ( 'NONE',  ( 12.77505761545979901, 1512.281672892750066, 224.2544213742990280 ) ) ;
#38432 = ORIENTED_EDGE ( 'NONE', *, *, #82993, .F. ) ;
#38433 = EDGE_LOOP ( 'NONE', ( #75544, #105477, #36548, #31265 ) ) ;
#38434 = DIRECTION ( 'NONE',  ( 5.980589973904019347E-17, -1.000000000000000000, 1.736889445713099699E-16 ) ) ;
#38435 = CARTESIAN_POINT ( 'NONE',  ( 13.37406854560000014, 1507.496451373729997, 233.0472692219979933 ) ) ;
#38436 = CARTESIAN_POINT ( 'NONE',  ( 6.925143992711317864, 1424.000660984779415, 213.5535729141376748 ) ) ;
#38438 = CARTESIAN_POINT ( 'NONE',  ( -36.81312677009999845, 1440.913060384420078, 254.5659337159979998 ) ) ;
#38437 = CARTESIAN_POINT ( 'NONE',  ( 30.75249563405095898, 1420.147177030162538, 269.4790404245597983 ) ) ;
#38439 = AXIS2_PLACEMENT_3D ( 'NONE', #32447, #17812, #101262 ) ;
#38440 = CARTESIAN_POINT ( 'NONE',  ( 8.594215834125739306, 1437.591654922809994, 210.1985574426290384 ) ) ;
#38441 = CARTESIAN_POINT ( 'NONE',  ( -11.69527910600000098, 1433.555496640800129, 150.9724154829980023 ) ) ;
#38442 = ADVANCED_FACE ( 'NONE', ( #14222 ), #86893, .T. ) ;
#38443 = DIRECTION ( 'NONE',  ( 0.000000000000000000, 1.000000000000000000, 0.000000000000000000 ) ) ;
#38444 = CARTESIAN_POINT ( 'NONE',  ( -19.02744254319999939, 1485.647624488630072, 189.5786657373980120 ) ) ;
#38445 = CARTESIAN_POINT ( 'NONE',  ( 8.370668212402989639, 1465.542310901930023, 214.3762783931849754 ) ) ;
#38446 = EDGE_CURVE ( 'NONE', #24977, #47969, #49231, .T. ) ;
#38447 = CARTESIAN_POINT ( 'NONE',  ( -26.71905419379999813, 1436.374501372160012, 136.7391346277979949 ) ) ;
#38449 = CARTESIAN_POINT ( 'NONE',  ( -0.3115382522500990126, 1515.152701004710025, 213.4489927825219979 ) ) ;
#38448 = AXIS2_PLACEMENT_3D ( 'NONE', #73962, #50422, #99679 ) ;
#38450 = CARTESIAN_POINT ( 'NONE',  ( -4.500000000000000000, 1417.575542696430148, 161.0097146498980010 ) ) ;
#38451 = CARTESIAN_POINT ( 'NONE',  ( -3.523962699983150149, 1476.511731499819916, 220.0526012347959863 ) ) ;
#38452 = CARTESIAN_POINT ( 'NONE',  ( 4.262353028408887745, 1360.811275533914113, 210.6218459616987957 ) ) ;
#38453 = CARTESIAN_POINT ( 'NONE',  ( 34.18677586421061676, 1522.906561336852974, 198.4504086008707873 ) ) ;
#38455 = ORIENTED_EDGE ( 'NONE', *, *, #72762, .T. ) ;
#38454 = CARTESIAN_POINT ( 'NONE',  ( 7.642515834685991225E-10, 1410.900380117609984, 256.4109302437369706 ) ) ;
#38456 = ORIENTED_EDGE ( 'NONE', *, *, #2511, .T. ) ;
#38457 = CARTESIAN_POINT ( 'NONE',  ( -11.86244099381709916, 1432.080345950339961, 149.9764139188839920 ) ) ;
#38458 = B_SPLINE_CURVE_WITH_KNOTS ( 'NONE', 3,
 ( #35448, #87521, #36011, #62339, #37655, #88079 ),
 .UNSPECIFIED., .F., .F.,
 ( 4, 2, 4 ),
 ( -1.285435071110569928E-05, 0.001079388306740477988, 0.002171630964192061610 ),
 .UNSPECIFIED. ) ;
#38459 = CARTESIAN_POINT ( 'NONE',  ( 9.687580767120000047, 1493.795581537490079, 188.2203327861989806 ) ) ;
#38460 = CARTESIAN_POINT ( 'NONE',  ( -33.45710699309999825, 1460.809384530529996, 270.1367558008980154 ) ) ;
#38461 = CARTESIAN_POINT ( 'NONE',  ( 3.156166260290000025, 1466.544008048530031, 236.1241471695980181 ) ) ;
#38462 = CARTESIAN_POINT ( 'NONE',  ( -113.4000000000000057, 1376.302340817389904, 316.0486468239590181 ) ) ;
#38463 = DIRECTION ( 'NONE',  ( -0.2054769195713296581, 0.000000000000000000, 0.9786619618251632957 ) ) ;
#38464 = EDGE_CURVE ( 'NONE', #85608, #69919, #23810, .T. ) ;
#38465 = CARTESIAN_POINT ( 'NONE',  ( 0.2142980244695730230, 1452.886707787869909, 183.2554660003850131 ) ) ;
#38466 = CARTESIAN_POINT ( 'NONE',  ( -14.49383156030000031, 1422.099018230730053, 229.4564958546980051 ) ) ;
#38467 = CARTESIAN_POINT ( 'NONE',  ( 0.4266141307560009643, 1456.468849147889841, 199.2577416451890144 ) ) ;
#38468 = CARTESIAN_POINT ( 'NONE',  ( -3.163822641140000336, 1456.764303476689975, 218.0770700807990181 ) ) ;
#38469 = CARTESIAN_POINT ( 'NONE',  ( 8.379275254589538591, 1362.454991452514150, 210.6218459616991936 ) ) ;
#38470 = CARTESIAN_POINT ( 'NONE',  ( -27.50738397533670110, 1412.571463151949956, 268.1607314479759907 ) ) ;
#38471 = VERTEX_POINT ( 'NONE', #57372 ) ;
#38472 = DIRECTION ( 'NONE',  ( 0.000000000000000000, 0.000000000000000000, -1.000000000000000000 ) ) ;
#38473 = ORIENTED_EDGE ( 'NONE', *, *, #105036, .T. ) ;
#38474 = ORIENTED_EDGE ( 'NONE', *, *, #59764, .T. ) ;
#38475 = CARTESIAN_POINT ( 'NONE',  ( 0.7579843820170020230, 1516.883361325900069, 211.4083188566570186 ) ) ;
#38476 = CARTESIAN_POINT ( 'NONE',  ( 4.631508481766313245, 1423.709513865996996, 183.8663217726549135 ) ) ;
#38477 = CARTESIAN_POINT ( 'NONE',  ( -17.60576718599832446, 1419.790616927256906, 206.7145629358298606 ) ) ;
#38478 = CARTESIAN_POINT ( 'NONE',  ( -15.45655017849999879, 1440.435998840410093, 189.5583962537980085 ) ) ;
#38479 = DIRECTION ( 'NONE',  ( -1.156023075842281927E-31, 1.000000000000000000, -1.698192320643030073E-16 ) ) ;
#38480 = ORIENTED_EDGE ( 'NONE', *, *, #71313, .T. ) ;
#38481 = EDGE_CURVE ( 'NONE', #110436, #14535, #91499, .T. ) ;
#38482 = EDGE_CURVE ( 'NONE', #39998, #46912, #66870, .T. ) ;
#38483 = CARTESIAN_POINT ( 'NONE',  ( -5.780232115465000042, 1516.760434454289907, 201.7950504087270076 ) ) ;
#38484 = CARTESIAN_POINT ( 'NONE',  ( 5.530560524640000253, 1471.884652610789999, 217.6741512182190093 ) ) ;
#38486 = AXIS2_PLACEMENT_3D ( 'NONE', #8457, #77343, #68963 ) ;
#38485 = CARTESIAN_POINT ( 'NONE',  ( -16.04653612434290011, 1384.524557204450048, 200.8152124474479763 ) ) ;
#38487 = ORIENTED_EDGE ( 'NONE', *, *, #40792, .F. ) ;
#38488 = CARTESIAN_POINT ( 'NONE',  ( -9.898755429526129745, 1408.724963430380058, 270.2742877825459686 ) ) ;
#38489 = CARTESIAN_POINT ( 'NONE',  ( 1.610281973209999908E-15, 1427.674934138829940, 112.4493539157979995 ) ) ;
#38490 = CARTESIAN_POINT ( 'NONE',  ( 9.712381508628240567, 1434.979473192740215, 207.7851750229139896 ) ) ;
#38492 = ORIENTED_EDGE ( 'NONE', *, *, #11652, .F. ) ;
#38491 = CARTESIAN_POINT ( 'NONE',  ( -8.123348129977994603, 1364.941198722160607, 208.3718459617061285 ) ) ;
#38493 = ORIENTED_EDGE ( 'NONE', *, *, #62702, .F. ) ;
#38494 = CARTESIAN_POINT ( 'NONE',  ( 42.36757903333897701, 1453.626821642604227, 269.0658443221472567 ) ) ;
#38495 = EDGE_CURVE ( 'NONE', #43234, #105296, #33259, .T. ) ;
#38496 = CARTESIAN_POINT ( 'NONE',  ( 11.07598440222710146, 1471.727447236650050, 211.9431201832250053 ) ) ;
#38497 = CARTESIAN_POINT ( 'NONE',  ( -13.39012931902800041, 1436.134316771910107, 150.5611366713399946 ) ) ;
#38498 = CARTESIAN_POINT ( 'NONE',  ( -0.03399551901351580141, 1409.332672981930045, 185.4489178702069978 ) ) ;
#38499 = CARTESIAN_POINT ( 'NONE',  ( 5.788691325514999875, 1517.157901477309906, 210.2449475486469908 ) ) ;
#38500 = ADVANCED_FACE ( 'NONE', ( #109414 ), #92010, .T. ) ;
#38501 = CARTESIAN_POINT ( 'NONE',  ( -20.62320340999438528, 1506.569407725107112, 217.0556035612084713 ) ) ;
#38502 = CARTESIAN_POINT ( 'NONE',  ( -18.38268101079999894, 1430.797810259230118, 225.7446671720980191 ) ) ;
#38503 = CARTESIAN_POINT ( 'NONE',  ( 15.74277789255459936, 1473.851709889820086, 269.2139740697160164 ) ) ;
#38504 = CARTESIAN_POINT ( 'NONE',  ( 12.72284891840000043, 1416.311719779230089, 222.6852781584979653 ) ) ;
#38505 = CARTESIAN_POINT ( 'NONE',  ( 7.567811368475000577, 1511.141271963160079, 206.0724820029969919 ) ) ;
#38506 = CARTESIAN_POINT ( 'NONE',  ( 2.283570633165000086, 1516.909589401870107, 206.2402975076569760 ) ) ;
#38507 = ORIENTED_EDGE ( 'NONE', *, *, #94710, .F. ) ;
#38508 = CARTESIAN_POINT ( 'NONE',  ( -33.91369111065759512, 1435.681798630919957, 135.0584844183200346 ) ) ;
#38509 = CARTESIAN_POINT ( 'NONE',  ( -23.92444880932286111, 1445.948748625923145, 213.1725788544748923 ) ) ;
#38510 = ORIENTED_EDGE ( 'NONE', *, *, #2746, .F. ) ;
#38511 = CARTESIAN_POINT ( 'NONE',  ( 7.411925917899073291, 1456.536940314574167, 227.5735638817602364 ) ) ;
#38512 = DIRECTION ( 'NONE',  ( 1.755985294532469921E-16, -1.000000000000000000, 1.338183447452831989E-16 ) ) ;
#38513 = CARTESIAN_POINT ( 'NONE',  ( -4.108880503800459216, 1440.120469803585365, 185.4247791707405497 ) ) ;
#38514 = DIRECTION ( 'NONE',  ( -1.000000000000000000, 0.000000000000000000, 0.000000000000000000 ) ) ;
#38515 = CARTESIAN_POINT ( 'NONE',  ( 20.70465513139999914, 1409.636082885830092, 202.1075812846079884 ) ) ;
#38516 = CARTESIAN_POINT ( 'NONE',  ( 31.23437356469446868, 1511.187213306747708, 222.8968241038843701 ) ) ;
#38517 = CARTESIAN_POINT ( 'NONE',  ( 15.94345642359999715, 1409.469818154030008, 225.2684697977979909 ) ) ;
#38518 = CARTESIAN_POINT ( 'NONE',  ( 32.38845792001183810, 1523.456924617338700, 202.1182848006293113 ) ) ;
#38519 = EDGE_CURVE ( 'NONE', #65949, #23788, #2834, .T. ) ;
#38520 = CARTESIAN_POINT ( 'NONE',  ( -2.469737631213410278, 1507.227429411520006, 221.7265308815400147 ) ) ;
#38521 = CARTESIAN_POINT ( 'NONE',  ( 4.253135465434060514, 1441.316943195099839, 160.6080137006729842 ) ) ;
#38522 = CARTESIAN_POINT ( 'NONE',  ( 2.500000000000000000, 1439.604493174409981, 166.9187913666470138 ) ) ;
#38523 = CARTESIAN_POINT ( 'NONE',  ( 6.944231748164999551, 1516.882690742909972, 215.6753703478370028 ) ) ;
#38524 = EDGE_CURVE ( 'NONE', #74404, #60042, #5198, .T. ) ;
#38525 = EDGE_LOOP ( 'NONE', ( #874, #45389, #24841, #31326 ) ) ;
#38526 = CARTESIAN_POINT ( 'NONE',  ( 7.709052374754190140, 1516.535093240819833, 207.2584636299989995 ) ) ;
#38527 = CARTESIAN_POINT ( 'NONE',  ( -4.124924170559999936, 1474.647204749290040, 198.4545245537989899 ) ) ;
#38528 = DIRECTION ( 'NONE',  ( 0.9970203751124365743, 0.07713865185920996959, 0.000000000000000000 ) ) ;
#38529 = CARTESIAN_POINT ( 'NONE',  ( -8.492687501607809608, 1424.222007390339968, 101.6998641355710049 ) ) ;
#38530 = AXIS2_PLACEMENT_3D ( 'NONE', #92398, #23548, #25188 ) ;
#38531 = CARTESIAN_POINT ( 'NONE',  ( -40.01985023196169777, 1445.652369265400011, 136.8565960713379752 ) ) ;
#38532 = CARTESIAN_POINT ( 'NONE',  ( 19.26336319460000013, 1457.977935815189767, 211.9550914373890009 ) ) ;
#38533 = CARTESIAN_POINT ( 'NONE',  ( -9.862951376772540968, 1521.951704408389787, 228.3939896807019920 ) ) ;
#38534 = CARTESIAN_POINT ( 'NONE',  ( -2.379356867398829678, 1477.797235972689805, 183.4954656640089752 ) ) ;
#38535 = CARTESIAN_POINT ( 'NONE',  ( 0.2249571944082079944, 1455.813922287919922, 198.5778828182170059 ) ) ;
#38536 = CARTESIAN_POINT ( 'NONE',  ( -45.63734462135529668, 1442.192498193280016, 268.9745364237319905 ) ) ;
#38537 = B_SPLINE_SURFACE_WITH_KNOTS ( 'NONE', 4, 5, ( 
 ( #39360, #21971, #39913, #56163, #72975, #108212 ),
 ( #47766, #81901, #5207, #74083, #65680, #73534 ),
 ( #82472, #100367, #107670, #5770, #65130, #31500 ),
 ( #99798, #23092, #91425, #74631, #108766, #32059 ),
 ( #49430, #23653, #57835, #91962, #83552, #6845 ) ),
 .UNSPECIFIED., .F., .F., .F.,
 ( 5, 5 ),
 ( 6, 6 ),
 ( 4.842510457999999574, 5.115712977159999397 ),
 ( 0.000000000000000000, 2.000000000000000000 ),
 .UNSPECIFIED. ) ;
#38538 = CARTESIAN_POINT ( 'NONE',  ( 28.16386307796540223, 1440.913060387279984, 231.8139636807940178 ) ) ;
#38539 = CARTESIAN_POINT ( 'NONE',  ( -110.0571759400000076, 1385.284143576950100, 296.9644176183589366 ) ) ;
#38540 = CARTESIAN_POINT ( 'NONE',  ( -10.01326586723869916, 1481.014341800280135, 205.7823588363200145 ) ) ;
#38541 = ORIENTED_EDGE ( 'NONE', *, *, #33709, .T. ) ;
#38542 = FACE_OUTER_BOUND ( 'NONE', #80996, .T. ) ;
#38543 = DIRECTION ( 'NONE',  ( 0.7414773880254614813, 0.000000000000000000, -0.6709778558543786353 ) ) ;
#38544 = CARTESIAN_POINT ( 'NONE',  ( -2.884827118950000102, 1442.301347507789842, 200.7110630097789965 ) ) ;
#38545 = CARTESIAN_POINT ( 'NONE',  ( -11.86716023049999968, 1432.353341358199941, 147.6509521729980179 ) ) ;
#38546 = CARTESIAN_POINT ( 'NONE',  ( 12.32716906920000000, 1492.190914771690132, 209.5898718715859843 ) ) ;
#38547 = CARTESIAN_POINT ( 'NONE',  ( -17.04970511980000225, 1508.515036612230006, 230.3270150111979717 ) ) ;
#38548 = CARTESIAN_POINT ( 'NONE',  ( -49.92459275517279593, 1383.812035811190071, 261.1885675870709633 ) ) ;
#38549 = VECTOR ( 'NONE', #6175, 1000.000000000000000 ) ;
#38550 = CARTESIAN_POINT ( 'NONE',  ( -2.487921567437299863, 1508.551704408389924, 204.2892348438399779 ) ) ;
#38551 = CARTESIAN_POINT ( 'NONE',  ( -15.57748978299999898, 1507.212883763329955, 192.6976421578980023 ) ) ;
#38552 = CARTESIAN_POINT ( 'NONE',  ( -11.69032781984710034, 1501.851939758080107, 208.8185134538140062 ) ) ;
#38553 = CARTESIAN_POINT ( 'NONE',  ( 1.908739326689999904, 1465.060976646429935, 235.3867066285980059 ) ) ;
#38555 = VERTEX_POINT ( 'NONE', #69080 ) ;
#38554 = CARTESIAN_POINT ( 'NONE',  ( -41.65674268029999894, 1443.992461967939789, 135.6790812281979868 ) ) ;
#38556 = CARTESIAN_POINT ( 'NONE',  ( -1.027621871790000085, 1451.767504252629806, 183.3788275550980131 ) ) ;
#38557 = CARTESIAN_POINT ( 'NONE',  ( -9.008611445770000614, 1379.827692983760016, 214.1021766380889915 ) ) ;
#38558 = CARTESIAN_POINT ( 'NONE',  ( -3.618491329580000304, 1476.620320023590011, 199.4078043363890060 ) ) ;
#38560 = ORIENTED_EDGE ( 'NONE', *, *, #19408, .T. ) ;
#38559 = CARTESIAN_POINT ( 'NONE',  ( -18.24633262864339756, 1416.842625005220043, 208.9597599549800009 ) ) ;
#38561 = CARTESIAN_POINT ( 'NONE',  ( -18.47516819563199775, 1466.235567073390030, 200.8822723802850021 ) ) ;
#38562 = ORIENTED_EDGE ( 'NONE', *, *, #22945, .F. ) ;
#38563 = CIRCLE ( 'NONE', #51060, 1.999999999999999556 ) ;
#38564 = CARTESIAN_POINT ( 'NONE',  ( -11.54871805396859941, 1389.257702312929950, 215.5751257078669880 ) ) ;
#38565 = CARTESIAN_POINT ( 'NONE',  ( 0.9645253690480010134, 1484.661534505690042, 201.1941721493990372 ) ) ;
#38566 = CARTESIAN_POINT ( 'NONE',  ( -18.19590854888185305, 1522.382868172863937, 180.0410247165186490 ) ) ;
#38567 = CARTESIAN_POINT ( 'NONE',  ( -3.330134203884999700, 1515.051704408389924, 213.4516374609670208 ) ) ;
#38568 = EDGE_CURVE ( 'NONE', #65245, #3729, #59948, .T. ) ;
#38569 = DIRECTION ( 'NONE',  ( -1.755985294532469921E-16, 1.000000000000000000, -1.338183447452831989E-16 ) ) ;
#38570 = CARTESIAN_POINT ( 'NONE',  ( -10.09235534473100060, 1472.733359838320212, 207.2792504626609968 ) ) ;
#38571 = CARTESIAN_POINT ( 'NONE',  ( -6.123233995736771213E-16, 1379.913060387289988, 209.1218459616989946 ) ) ;
#38572 = CARTESIAN_POINT ( 'NONE',  ( 18.02574752529999813, 1424.482706161330043, 224.6196056148980063 ) ) ;
#38573 = CARTESIAN_POINT ( 'NONE',  ( 1.166167165090000069, 1418.953384179930026, 184.8577940441979877 ) ) ;
#38574 = CARTESIAN_POINT ( 'NONE',  ( -18.41452686919999593, 1437.075586301560179, 192.6723155837979959 ) ) ;
#38575 = DIRECTION ( 'NONE',  ( 0.000000000000000000, 0.000000000000000000, -1.000000000000000000 ) ) ;
#38576 = CARTESIAN_POINT ( 'NONE',  ( -2.427038242517200128, 1449.569853069620194, 183.3138490965509959 ) ) ;
#38577 = ORIENTED_EDGE ( 'NONE', *, *, #17886, .T. ) ;
#38578 = ORIENTED_EDGE ( 'NONE', *, *, #68769, .F. ) ;
#38579 =( BOUNDED_CURVE ( )  B_SPLINE_CURVE ( 3, ( #13603, #39937, #23115, #56746 ),
 .UNSPECIFIED., .F., .F. ) 
 B_SPLINE_CURVE_WITH_KNOTS ( ( 4, 4 ),
 ( 1.307301600140529985, 1.688785180142575060 ),
 .UNSPECIFIED. ) 
 CURVE ( )  GEOMETRIC_REPRESENTATION_ITEM ( )  RATIONAL_B_SPLINE_CURVE ( ( 1.000000000000000000, 0.9879092475434242404, 0.9879092475434242404, 1.000000000000000000 ) ) 
 REPRESENTATION_ITEM ( '' )  );
#38580 = CARTESIAN_POINT ( 'NONE',  ( 19.07966196791819513, 1524.244163922424377, 239.0023935151726562 ) ) ;
#38581 = CARTESIAN_POINT ( 'NONE',  ( -11.34486004996399977, 1415.059973085260026, 195.5756060859239938 ) ) ;
#38582 = CARTESIAN_POINT ( 'NONE',  ( -11.97808853149999919, 1435.413056357760070, 151.1931547270979763 ) ) ;
#38583 = ADVANCED_FACE ( 'NONE', ( #59013 ), #7998, .F. ) ;
#38584 = CARTESIAN_POINT ( 'NONE',  ( -6.119344404807989421E-10, 1468.772255180760112, 250.5908485024660024 ) ) ;
#38585 = CARTESIAN_POINT ( 'NONE',  ( -3.430374836980000008, 1431.708658569990121, 216.7924588047190184 ) ) ;
#38586 = CARTESIAN_POINT ( 'NONE',  ( -14.83290890009999963, 1420.352728576609934, 213.2060141321290132 ) ) ;
#38587 = CARTESIAN_POINT ( 'NONE',  ( -1.793335950739999962, 1419.496365638530051, 185.6406336190979971 ) ) ;
#38588 = CARTESIAN_POINT ( 'NONE',  ( -0.1926035411919999885, 1484.826485890729828, 181.8486164389979933 ) ) ;
#38589 = CARTESIAN_POINT ( 'NONE',  ( -10.48932666274678205, 1367.017575692817445, 210.6218459617030021 ) ) ;
#38590 = FACE_OUTER_BOUND ( 'NONE', #55599, .T. ) ;
#38591 = ADVANCED_FACE ( 'NONE', ( #79130 ), #90158, .F. ) ;
#38592 = CARTESIAN_POINT ( 'NONE',  ( 2.596261494520241353, 1525.907212628473644, 177.4701144822246874 ) ) ;
#38593 = CARTESIAN_POINT ( 'NONE',  ( -5.013429394184999666, 1517.123342927159911, 207.9998951881570122 ) ) ;
#38594 = FACE_OUTER_BOUND ( 'NONE', #79429, .T. ) ;
#38595 = CARTESIAN_POINT ( 'NONE',  ( 11.27110984222679946, 1434.117046727379829, 151.5594388631620006 ) ) ;
#38596 = CARTESIAN_POINT ( 'NONE',  ( -13.95840997858960009, 1435.352809884700264, 149.6697649492990081 ) ) ;
#38597 = CARTESIAN_POINT ( 'NONE',  ( -7.543140222519999938, 1385.044701444139946, 219.0850215955189810 ) ) ;
#38598 = CARTESIAN_POINT ( 'NONE',  ( 20.92457304854260158, 1409.643762579499935, 205.0061533375680085 ) ) ;
#38599 = CARTESIAN_POINT ( 'NONE',  ( 1.037960838350000081, 1497.036773399490130, 197.1546544923990041 ) ) ;
#38600 = CARTESIAN_POINT ( 'NONE',  ( -16.70268422512909723, 1500.167277360910020, 229.9148981415720243 ) ) ;
#38601 = AXIS2_PLACEMENT_3D ( 'NONE', #40152, #13826, #31196 ) ;
#38602 = EDGE_LOOP ( 'NONE', ( #41762, #69786, #15339 ) ) ;
#38603 = CARTESIAN_POINT ( 'NONE',  ( 32.03901053599999926, 1430.123112397830027, 250.0966427502979741 ) ) ;
#38604 = CYLINDRICAL_SURFACE ( 'NONE', #93996, 2.000000000000000000 ) ;
#38607 = CARTESIAN_POINT ( 'NONE',  ( -17.84692918829999897, 1410.032953027829990, 195.3924022816980255 ) ) ;
#38606 = CIRCLE ( 'NONE', #108322, 0.2999999999999669598 ) ;
#38605 = CARTESIAN_POINT ( 'NONE',  ( 0.4635522705379999664, 1504.645434567829852, 181.0404501616980042 ) ) ;
#38608 = CARTESIAN_POINT ( 'NONE',  ( 1.861700016370000164E-09, 1407.650947845630071, 270.1377426662980383 ) ) ;
#38609 = CARTESIAN_POINT ( 'NONE',  ( -23.75152772239999877, 1432.714080072660181, 220.8246967967979799 ) ) ;
#38610 = CARTESIAN_POINT ( 'NONE',  ( 2.418224342909999880, 1485.303415267289893, 220.3436431501990000 ) ) ;
#38611 = EDGE_CURVE ( 'NONE', #61362, #21533, #4074, .T. ) ;
#38612 = CARTESIAN_POINT ( 'NONE',  ( -7.734617125744999377, 1516.863303996349941, 216.9435780305869912 ) ) ;
#38613 = CARTESIAN_POINT ( 'NONE',  ( 30.24133951009999777, 1451.857592286530007, 135.2575210613979948 ) ) ;
#38614 = ORIENTED_EDGE ( 'NONE', *, *, #110148, .T. ) ;
#38615 = DIRECTION ( 'NONE',  ( -0.8672669759446604010, 0.000000000000000000, 0.4978433412588780804 ) ) ;
#38616 = CARTESIAN_POINT ( 'NONE',  ( 14.30575996553655038, 1514.201209518706264, 225.6492543780247502 ) ) ;
#38617 = EDGE_CURVE ( 'NONE', #100495, #34701, #81521, .T. ) ;
#38618 = CARTESIAN_POINT ( 'NONE',  ( 2.905289237559999904, 1509.014515323130126, 238.4132587644979822 ) ) ;
#38619 = ORIENTED_EDGE ( 'NONE', *, *, #71701, .F. ) ;
#38620 = ORIENTED_EDGE ( 'NONE', *, *, #4133, .F. ) ;
#38621 = CARTESIAN_POINT ( 'NONE',  ( 9.176823589263729986, 1451.591198660380087, 210.4727899134140046 ) ) ;
#38622 = CARTESIAN_POINT ( 'NONE',  ( -23.91153463986099936, 1410.421621703130086, 208.6572241185120049 ) ) ;
#38623 = EDGE_CURVE ( 'NONE', #42280, #64279, #71861, .T. ) ;
#38624 = ORIENTED_EDGE ( 'NONE', *, *, #5898, .F. ) ;
#38625 = CARTESIAN_POINT ( 'NONE',  ( 5.923682464646780943, 1522.051704408389924, 194.3813127491490036 ) ) ;
#38626 = CARTESIAN_POINT ( 'NONE',  ( 20.69751568230000061, 1495.539250102490087, 213.2323776579090122 ) ) ;
#38627 = ADVANCED_FACE ( 'NONE', ( #95909 ), #75045, .T. ) ;
#38628 = CARTESIAN_POINT ( 'NONE',  ( -4.375055004340000053, 1479.770299212029840, 235.2382511805980130 ) ) ;
#38630 = VECTOR ( 'NONE', #50227, 1000.000000000000000 ) ;
#38629 = CARTESIAN_POINT ( 'NONE',  ( 3.601839739459999912, 1444.840594719589944, 200.9001243581789993 ) ) ;
#38631 = ORIENTED_EDGE ( 'NONE', *, *, #25557, .F. ) ;
#38632 = CARTESIAN_POINT ( 'NONE',  ( 11.15480544429999910, 1425.160630053029990, 144.1619436902979885 ) ) ;
#38633 = CARTESIAN_POINT ( 'NONE',  ( -12.16511160556770044, 1414.971513442450032, 220.6991975209760142 ) ) ;
#38634 = CARTESIAN_POINT ( 'NONE',  ( -8.316669917960000546, 1425.055151526479904, 204.9623398779190211 ) ) ;
#38635 = CARTESIAN_POINT ( 'NONE',  ( -3.263521942484999716, 1516.676340709600026, 203.3494421577970002 ) ) ;
#38636 = ORIENTED_EDGE ( 'NONE', *, *, #2908, .F. ) ;
#38637 = CARTESIAN_POINT ( 'NONE',  ( 9.010607138093890356, 1482.289598254839802, 216.7687604371109842 ) ) ;
#38638 = CARTESIAN_POINT ( 'NONE',  ( 13.27015362366167217, 1443.199215167730699, 187.6658312763560446 ) ) ;
#38639 = ORIENTED_EDGE ( 'NONE', *, *, #31522, .F. ) ;
#38640 = EDGE_LOOP ( 'NONE', ( #49747, #104606, #51538, #96494 ) ) ;
#38641 = CARTESIAN_POINT ( 'NONE',  ( 0.8350686643532179154, 1526.382868172863937, 177.3106345060153046 ) ) ;
#38642 = DIRECTION ( 'NONE',  ( 0.9991156149436395406, 0.000000000000000000, -0.04204744909971582650 ) ) ;
#38643 = CARTESIAN_POINT ( 'NONE',  ( -4.363122647530000009, 1409.354802298930053, 146.1721969590979882 ) ) ;
#38644 = CARTESIAN_POINT ( 'NONE',  ( -14.56186263597409969, 1513.645442088330128, 194.0527955301810152 ) ) ;
#38645 = CARTESIAN_POINT ( 'NONE',  ( -4.459046139639999851, 1425.240413237929943, 186.1432435763979925 ) ) ;
#38646 = CARTESIAN_POINT ( 'NONE',  ( 11.21940781969999890, 1420.554733691869842, 198.7349279449990149 ) ) ;
#38647 = ADVANCED_FACE ( 'NONE', ( #58318 ), #7350, .T. ) ;
#38648 = CARTESIAN_POINT ( 'NONE',  ( 0.9567324420246190453, 1475.057211051239847, 220.5008870814820057 ) ) ;
#38649 = CARTESIAN_POINT ( 'NONE',  ( -7.566646731243020341, 1494.041882933070156, 199.4137124706639952 ) ) ;
#38650 = CARTESIAN_POINT ( 'NONE',  ( -10.97268961956110012, 1432.538086023540245, 151.7700193388709806 ) ) ;
#38651 = CARTESIAN_POINT ( 'NONE',  ( 0.03704823030615916196, 1409.672459229776450, 233.0526395660594972 ) ) ;
#38653 = CARTESIAN_POINT ( 'NONE',  ( -105.4653038608459923, 1391.248269531060259, 304.9316119955079785 ) ) ;
#38652 = CARTESIAN_POINT ( 'NONE',  ( 29.41653895341896074, 1525.790286462512086, 196.6777156381645284 ) ) ;
#38654 = CARTESIAN_POINT ( 'NONE',  ( 12.01697534725119887, 1421.833474732869945, 207.3587116575859852 ) ) ;
#38655 = CARTESIAN_POINT ( 'NONE',  ( -9.835593549186530282, 1439.958152553570017, 207.2549332851669988 ) ) ;
#38656 = ADVANCED_FACE ( 'NONE', ( #91366 ), #73476, .F. ) ;
#38657 = CARTESIAN_POINT ( 'NONE',  ( -7.101217506704999849, 1512.693483295299984, 200.8135970150769936 ) ) ;
#38658 = ORIENTED_EDGE ( 'NONE', *, *, #20435, .F. ) ;
#38659 = CARTESIAN_POINT ( 'NONE',  ( 17.24149055319999846, 1434.891998881070094, 209.1218459616979999 ) ) ;
#38660 = CARTESIAN_POINT ( 'NONE',  ( -0.04714347637158690374, 1424.289205137260069, 227.6285544301180153 ) ) ;
#38661 = CARTESIAN_POINT ( 'NONE',  ( -88.41096488174009949, 1384.973236710020046, 308.1529525611489930 ) ) ;
#38662 = CARTESIAN_POINT ( 'NONE',  ( -10.43611966299999949, 1387.704879639269848, 201.2730187963089747 ) ) ;
#38663 = ADVANCED_FACE ( 'NONE', ( #82954 ), #67021, .F. ) ;
#38664 = CARTESIAN_POINT ( 'NONE',  ( -14.87918216340000122, 1415.865102033119911, 212.9009079005989804 ) ) ;
#38666 = ORIENTED_EDGE ( 'NONE', *, *, #74806, .F. ) ;
#38665 = CARTESIAN_POINT ( 'NONE',  ( -9.183711187100000117, 1463.569275765890097, 202.8257126108990178 ) ) ;
#38667 = CARTESIAN_POINT ( 'NONE',  ( 4.110418388699999426, 1430.160170311989987, 217.2245068817190088 ) ) ;
#38668 = CARTESIAN_POINT ( 'NONE',  ( -1.661536740469999884, 1441.600846913620217, 150.6803463261979914 ) ) ;
#38669 = CARTESIAN_POINT ( 'NONE',  ( -13.79565920049999939, 1416.830001024129842, 221.9088573472979817 ) ) ;
#38670 = CARTESIAN_POINT ( 'NONE',  ( 0.2961798576886189305, 1430.492998182000065, 199.6993750702310138 ) ) ;
#38671 = CARTESIAN_POINT ( 'NONE',  ( 14.56792383663499990, 1513.484013041540038, 224.4367011526669842 ) ) ;
#38672 = DIRECTION ( 'NONE',  ( 0.9996573249755569268, 0.02617694830788839730, 1.176140869340470334E-16 ) ) ;
#38673 = CARTESIAN_POINT ( 'NONE',  ( 4.830146310314740177, 1458.041703014179802, 200.3202911288479982 ) ) ;
#38674 = CARTESIAN_POINT ( 'NONE',  ( -108.4218473026954257, 1388.739376737770726, 298.0879157462472335 ) ) ;
#38675 = CARTESIAN_POINT ( 'NONE',  ( 15.98031816559999996, 1422.108692535729915, 227.4722591969980101 ) ) ;
#38676 = CARTESIAN_POINT ( 'NONE',  ( -21.38516915557942255, 1522.382868172863937, 237.8497028174240313 ) ) ;
#38677 = CARTESIAN_POINT ( 'NONE',  ( -6.563595907815000352, 1517.154223579619838, 206.8322214998769937 ) ) ;
#38678 = CARTESIAN_POINT ( 'NONE',  ( 45.66301396820000491, 1436.924929342960013, 268.7619381858979750 ) ) ;
#38679 = CARTESIAN_POINT ( 'NONE',  ( -19.06484846609999906, 1410.501627938029969, 222.8115755776980222 ) ) ;
#38680 = CARTESIAN_POINT ( 'NONE',  ( 18.47698316009999786, 1435.143056706319840, 145.4054505043980043 ) ) ;
#38681 = CARTESIAN_POINT ( 'NONE',  ( -0.7130142950260000001, 1416.844618646229947, 227.9191939115979721 ) ) ;
#38682 = PRODUCT_DEFINITION_FORMATION_WITH_SPECIFIED_SOURCE ( 'ANY', '', #71492, .NOT_KNOWN. ) ;
#38683 = CARTESIAN_POINT ( 'NONE',  ( -15.94338848148980148, 1409.469815784339971, 192.9752912694130202 ) ) ;
#38684 = CARTESIAN_POINT ( 'NONE',  ( 12.61618830369999955, 1416.831305870130109, 223.3237475159979795 ) ) ;
#38685 = CARTESIAN_POINT ( 'NONE',  ( -31.34137657934000387, 1523.382868172864164, 221.9025654077414345 ) ) ;
#38686 = CARTESIAN_POINT ( 'NONE',  ( -36.72317469411459712, 1436.720746570669917, 136.2687545549769936 ) ) ;
#38687 = CARTESIAN_POINT ( 'NONE',  ( 0.2120850959947599979, 1456.177984629059893, 183.1170619906590105 ) ) ;
#38688 = CARTESIAN_POINT ( 'NONE',  ( -8.260959520976138393, 1408.154429929020125, 220.0006158248199881 ) ) ;
#38689 = CARTESIAN_POINT ( 'NONE',  ( 8.637121918412720589, 1428.330124385589897, 213.2627993150280190 ) ) ;
#38690 = CARTESIAN_POINT ( 'NONE',  ( 16.68062049856716555, 1526.382868172863709, 181.4122394607864521 ) ) ;
#38691 = CARTESIAN_POINT ( 'NONE',  ( 0.9281737935813634266, 1484.584957263379692, 198.4507462532201032 ) ) ;
#38692 = CARTESIAN_POINT ( 'NONE',  ( 12.40435961620000072, 1434.419950087150255, 147.6244959444979941 ) ) ;
#38693 = CARTESIAN_POINT ( 'NONE',  ( -39.18506236317279701, 1437.902641090850011, 134.0999999975949777 ) ) ;
#38694 = CARTESIAN_POINT ( 'NONE',  ( 4.781276783620000081, 1452.020048942890071, 190.5513815401990030 ) ) ;
#38695 = ORIENTED_EDGE ( 'NONE', *, *, #22655, .F. ) ;
#38696 = CARTESIAN_POINT ( 'NONE',  ( 0.9988581265890018601, 1485.909730274089952, 197.9875094714990098 ) ) ;
#38697 = CARTESIAN_POINT ( 'NONE',  ( 4.229221492309999775, 1477.633992664089874, 199.3656528811089856 ) ) ;
#38698 = CARTESIAN_POINT ( 'NONE',  ( -9.025147011466630786, 1409.228225465760033, 221.0552217307139813 ) ) ;
#38699 = CARTESIAN_POINT ( 'NONE',  ( -11.81485801620000053, 1490.683346627590026, 208.7791644193250136 ) ) ;
#38700 = CARTESIAN_POINT ( 'NONE',  ( 1.543581094750000160, 1464.188004283289956, 202.2270558697589991 ) ) ;
#38701 = CARTESIAN_POINT ( 'NONE',  ( 14.46831308334499866, 1508.704177307590044, 232.8351181552330047 ) ) ;
#38702 = CARTESIAN_POINT ( 'NONE',  ( 31.94087964542345048, 1416.502482517117869, 269.3169482426198442 ) ) ;
#38703 = CARTESIAN_POINT ( 'NONE',  ( -17.84338787571900298, 1523.382868172864164, 237.8836641337663309 ) ) ;
#38704 = CARTESIAN_POINT ( 'NONE',  ( -12.29258316900000025, 1378.290984699069895, 210.0372636615540216 ) ) ;
#38705 = CARTESIAN_POINT ( 'NONE',  ( -86.03463923215619502, 1384.626609384469930, 307.1684108349550115 ) ) ;
#38706 = CARTESIAN_POINT ( 'NONE',  ( -28.43854200076519945, 1384.965860001799911, 204.7629818153700114 ) ) ;
#38707 = CARTESIAN_POINT ( 'NONE',  ( -18.37487226820823949, 1526.382868172863937, 235.7398599686418663 ) ) ;
#38708 = DIRECTION ( 'NONE',  ( -5.980589973904019347E-17, 1.000000000000000000, -1.736889445713099699E-16 ) ) ;
#38709 = CARTESIAN_POINT ( 'NONE',  ( -28.46393112459029950, 1508.969040165770139, 208.7960455483320175 ) ) ;
#38710 = TOROIDAL_SURFACE ( 'NONE', #76291, 24.69926344187880929, 1.000000000000000000 ) ;
#38711 = CARTESIAN_POINT ( 'NONE',  ( 2.745142294599053567, 1419.769955103634175, 137.0999999980979567 ) ) ;
#38713 = VERTEX_POINT ( 'NONE', #31861 ) ;
#38712 = DIRECTION ( 'NONE',  ( -1.755985294532469921E-16, 1.000000000000000000, -1.338183447452831989E-16 ) ) ;
#38714 = CARTESIAN_POINT ( 'NONE',  ( -109.1308226289999936, 1384.913202581150017, 311.2647286892589591 ) ) ;
#38715 = CARTESIAN_POINT ( 'NONE',  ( 5.191014570674193251, 1422.191164659828701, 138.4291919130531880 ) ) ;
#38716 = CARTESIAN_POINT ( 'NONE',  ( -10.81752260999999926, 1499.346262163689971, 213.0012804442189918 ) ) ;
#38717 = CARTESIAN_POINT ( 'NONE',  ( 3.487592431178331953, 1508.551704408389469, 204.2634855480304452 ) ) ;
#38718 = CARTESIAN_POINT ( 'NONE',  ( -2.472546475879999761, 1422.360492461289823, 192.6709265613989999 ) ) ;
#38719 = B_SPLINE_CURVE_WITH_KNOTS ( 'NONE', 3,
 ( #9361, #102841, #60324, #43525 ),
 .UNSPECIFIED., .F., .F.,
 ( 4, 4 ),
 ( 5.115887024574549358, 6.089794067229999719 ),
 .UNSPECIFIED. ) ;
#38720 = CARTESIAN_POINT ( 'NONE',  ( 20.90914698570000141, 1409.807713502029856, 217.2189215442579950 ) ) ;
#38721 = FACE_OUTER_BOUND ( 'NONE', #107334, .T. ) ;
#38722 = CARTESIAN_POINT ( 'NONE',  ( -16.53936930417849993, 1465.413251900429941, 220.7146308235560070 ) ) ;
#38723 = CARTESIAN_POINT ( 'NONE',  ( -17.86815066140000141, 1424.407639920930023, 228.2372701936979809 ) ) ;
#38725 = CARTESIAN_POINT ( 'NONE',  ( -11.82847241660000037, 1380.969823483590062, 203.0484502812290089 ) ) ;
#38724 = CARTESIAN_POINT ( 'NONE',  ( -3.547807590152150414, 1511.610022727348223, 201.0686036343854539 ) ) ;
#38726 = CARTESIAN_POINT ( 'NONE',  ( -11.39126005979999867, 1381.496251003520001, 216.9356158229890070 ) ) ;
#38727 = AXIS2_PLACEMENT_3D ( 'NONE', #57795, #49381, #40411 ) ;
#38728 = LINE ( 'NONE', #72902, #103842 ) ;
#38729 = CARTESIAN_POINT ( 'NONE',  ( 17.84338787571943641, 1523.382868172864164, 237.8836641337660467 ) ) ;
#38730 = CARTESIAN_POINT ( 'NONE',  ( -1.831354244299999934, 1416.588294615730092, 233.3593385782979794 ) ) ;
#38731 = CARTESIAN_POINT ( 'NONE',  ( 9.813910351400000565, 1364.017814053649772, 210.6218459616991936 ) ) ;
#38732 = CARTESIAN_POINT ( 'NONE',  ( 2.865911516645000212, 1516.906233342200039, 205.6598507734169914 ) ) ;
#38733 = CARTESIAN_POINT ( 'NONE',  ( -10.33648297811009975, 1485.164656460750166, 184.8983750646000033 ) ) ;
#38734 = ORIENTED_EDGE ( 'NONE', *, *, #71960, .T. ) ;
#38735 = CARTESIAN_POINT ( 'NONE',  ( 8821.610583169964229, 5182.767774292105059, -2585.458545683866305 ) ) ;
#38736 = CARTESIAN_POINT ( 'NONE',  ( 18.89905511659999959, 1416.828040475729949, 210.6687957193779823 ) ) ;
#38738 = ORIENTED_EDGE ( 'NONE', *, *, #43461, .F. ) ;
#38737 = CARTESIAN_POINT ( 'NONE',  ( -67.67707935839548838, 1379.746493294780066, 278.9722144515000082 ) ) ;
#38739 = ORIENTED_EDGE ( 'NONE', *, *, #59080, .F. ) ;
#38740 = CARTESIAN_POINT ( 'NONE',  ( 27.46146691510000082, 1508.600904575230061, 213.3784942867079906 ) ) ;
#38741 = ORIENTED_EDGE ( 'NONE', *, *, #17901, .F. ) ;
#38742 = CARTESIAN_POINT ( 'NONE',  ( 3.214223995087363672, 1507.157967210614061, 181.4588691370872482 ) ) ;
#38743 = CARTESIAN_POINT ( 'NONE',  ( -109.1316882649999940, 1384.947817856130087, 311.2645137162589890 ) ) ;
#38745 = CARTESIAN_POINT ( 'NONE',  ( 20.89213389120000031, 1453.805113726430136, 224.2163675376980052 ) ) ;
#38744 = CARTESIAN_POINT ( 'NONE',  ( 15.94629373821300078, 1419.829628885949887, 191.2397526529200036 ) ) ;
#38746 = CARTESIAN_POINT ( 'NONE',  ( -5.000330033664999618, 1516.770163853809890, 209.8779366980180328 ) ) ;
#38747 = ADVANCED_FACE ( 'NONE', ( #15039 ), #38604, .F. ) ;
#38748 = CARTESIAN_POINT ( 'NONE',  ( -24.31234282530909852, 1452.048309861259895, 136.6059775254549891 ) ) ;
#38749 = CARTESIAN_POINT ( 'NONE',  ( -107.8376371489249976, 1378.913060387289988, 308.2679488075570475 ) ) ;
#38750 = CARTESIAN_POINT ( 'NONE',  ( 12.52086369699999935, 1410.723690760830095, 228.7769307124980003 ) ) ;
#38752 = EDGE_CURVE ( 'NONE', #60554, #62929, #69022, .T. ) ;
#38751 = LINE ( 'NONE', #72928, #63477 ) ;
#38753 = CARTESIAN_POINT ( 'NONE',  ( 0.000000000000000000, 0.000000000000000000, 0.000000000000000000 ) ) ;
#38754 = B_SPLINE_CURVE_WITH_KNOTS ( 'NONE', 3,
 ( #99652, #99104, #57147, #66103, #38660, #40314 ),
 .UNSPECIFIED., .F., .F.,
 ( 4, 2, 4 ),
 ( -0.03264310120058740161, -0.01583012587366310064, -2.621721704315627122E-08 ),
 .UNSPECIFIED. ) ;
#38755 = CARTESIAN_POINT ( 'NONE',  ( 41.59656558032850171, 1442.666623284490015, 134.0999999980969903 ) ) ;
#38756 = CARTESIAN_POINT ( 'NONE',  ( -40.10831975841819741, 1442.142396374759983, 136.9487569356429901 ) ) ;
#38757 = ORIENTED_EDGE ( 'NONE', *, *, #5526, .F. ) ;
#38758 = CARTESIAN_POINT ( 'NONE',  ( 14.55552041736240021, 1435.948062197440095, 149.7943142905429852 ) ) ;
#38759 = CARTESIAN_POINT ( 'NONE',  ( -11.15007135000000105, 1391.248055150329947, 203.8486859877390032 ) ) ;
#38760 = EDGE_LOOP ( 'NONE', ( #12939, #52816, #97841, #91776 ) ) ;
#38761 = VERTEX_POINT ( 'NONE', #65491 ) ;
#38762 = CARTESIAN_POINT ( 'NONE',  ( -6.439137473055000171, 1514.557408760799945, 217.0653694116970200 ) ) ;
#38763 = CARTESIAN_POINT ( 'NONE',  ( 16.52212291317280446, 1514.209381233948534, 194.8043297302063195 ) ) ;
#38764 = CARTESIAN_POINT ( 'NONE',  ( -0.07105538368350000633, 1451.175970991930171, 182.5309677413980012 ) ) ;
#38765 = CARTESIAN_POINT ( 'NONE',  ( -16.87183719374050028, 1508.551704427820141, 210.1079651444619856 ) ) ;
#38766 = B_SPLINE_CURVE_WITH_KNOTS ( 'NONE', 5,
 ( #65167, #14739, #47256, #107149, #73013, #99839 ),
 .UNSPECIFIED., .F., .F.,
 ( 6, 6 ),
 ( -1.999999800030170194, 0.000000000000000000 ),
 .UNSPECIFIED. ) ;
#38767 = CIRCLE ( 'NONE', #11929, 2.000000000000001776 ) ;
#38768 = CARTESIAN_POINT ( 'NONE',  ( -16.20118746261578835, 1450.456937708418309, 221.2434354958739675 ) ) ;
#38769 = CARTESIAN_POINT ( 'NONE',  ( -68.43664974299086623, 1379.747301587279026, 279.3461838679465927 ) ) ;
#38770 = CARTESIAN_POINT ( 'NONE',  ( -3.138284008646738954, 1369.929752808247940, 210.4427501191478882 ) ) ;
#38771 = CARTESIAN_POINT ( 'NONE',  ( 28.13497766429999913, 1508.084884363030142, 208.3112646548739804 ) ) ;
#38772 = CARTESIAN_POINT ( 'NONE',  ( 8.218608085730000568, 1415.425433635630043, 193.5610124803980057 ) ) ;
#38773 = CARTESIAN_POINT ( 'NONE',  ( -50.68086562047950139, 1384.622718412899758, 226.3488145558480085 ) ) ;
#38774 = ORIENTED_EDGE ( 'NONE', *, *, #29579, .F. ) ;
#38775 = FACE_OUTER_BOUND ( 'NONE', #109156, .T. ) ;
#38776 = CARTESIAN_POINT ( 'NONE',  ( -7.338753868364999988, 1517.184383877180153, 206.8309596656170015 ) ) ;
#38777 = ORIENTED_EDGE ( 'NONE', *, *, #44604, .F. ) ;
#38778 = CARTESIAN_POINT ( 'NONE',  ( 35.59427720072490331, 1440.913060387330006, 261.7132250683009715 ) ) ;
#38779 = CARTESIAN_POINT ( 'NONE',  ( 19.03110457520000054, 1457.047041247629977, 226.1578386330979811 ) ) ;
#38780 = EDGE_LOOP ( 'NONE', ( #35318, #96769, #16546, #10098 ) ) ;
#38781 = CARTESIAN_POINT ( 'NONE',  ( -0.1198308412573760029, 1451.168734167799812, 182.5321973637160227 ) ) ;
#38782 = CARTESIAN_POINT ( 'NONE',  ( 8.427480802527020032, 1428.383621637630085, 213.4646598519510121 ) ) ;
#38783 = CARTESIAN_POINT ( 'NONE',  ( -108.7285119980398207, 1383.837283289873085, 311.1015258184347658 ) ) ;
#38784 = CARTESIAN_POINT ( 'NONE',  ( -24.49718675060000095, 1441.226578766219973, 211.0033545095979832 ) ) ;
#38785 = CARTESIAN_POINT ( 'NONE',  ( 22.46374799362600072, 1410.651871220149815, 206.2118963477199998 ) ) ;
#38786 = CARTESIAN_POINT ( 'NONE',  ( -5.943999059570199250, 1511.034527886640262, 201.5415479481260093 ) ) ;
#38787 = LINE ( 'NONE', #99784, #38792 ) ;
#38788 = DIRECTION ( 'NONE',  ( -0.7414773880254666993, 0.000000000000000000, 0.6709778558543727511 ) ) ;
#38789 = CARTESIAN_POINT ( 'NONE',  ( 11.40383981496231591, 1425.336178278838133, 144.1583008349757336 ) ) ;
#38791 = CARTESIAN_POINT ( 'NONE',  ( 0.1205199568272290050, 1457.838980749249913, 229.0211416662100135 ) ) ;
#38790 = CARTESIAN_POINT ( 'NONE',  ( 4.627533690799999988, 1466.419777224029986, 233.9118733120979812 ) ) ;
#38792 = VECTOR ( 'NONE', #74618, 1000.000000000000000 ) ;
#38793 = EDGE_CURVE ( 'NONE', #758, #75410, #31735, .T. ) ;
#38794 = CARTESIAN_POINT ( 'NONE',  ( -5.002593397454999646, 1516.960844870249957, 215.6810146069769871 ) ) ;
#38795 = CARTESIAN_POINT ( 'NONE',  ( -22.71594008370638562, 1409.706314096660435, 209.0156538452060317 ) ) ;
#38796 = CARTESIAN_POINT ( 'NONE',  ( -10.40779544903779197, 1480.508706840727882, 207.4968371392113795 ) ) ;
#38797 = CARTESIAN_POINT ( 'NONE',  ( 2.414383718323408257, 1516.533281679525544, 216.8308509075874611 ) ) ;
#38798 = CARTESIAN_POINT ( 'NONE',  ( 2.491188358395000080, 1516.733363207009916, 213.1488973760370129 ) ) ;
#38799 = CARTESIAN_POINT ( 'NONE',  ( 2.329939114882360052, 1515.551844914359890, 213.1055637607790061 ) ) ;
#38800 = EDGE_CURVE ( 'NONE', #74706, #109446, #38606, .T. ) ;
#38801 = CARTESIAN_POINT ( 'NONE',  ( -17.17241001986523941, 1512.187213306747481, 181.6185504016045797 ) ) ;
#38803 = ORIENTED_EDGE ( 'NONE', *, *, #9743, .T. ) ;
#38802 = CARTESIAN_POINT ( 'NONE',  ( -113.4000000000000057, 1384.913060387289988, 311.2218459572590064 ) ) ;
#38804 = CARTESIAN_POINT ( 'NONE',  ( -2.131986625821266745, 1526.000688113749902, 177.5511380990283499 ) ) ;
#38805 = CARTESIAN_POINT ( 'NONE',  ( 24.36881673870000142, 1444.160329039040107, 213.3381660858680107 ) ) ;
#38806 = CARTESIAN_POINT ( 'NONE',  ( -11.76319757070000094, 1431.851246079359953, 150.7944596534980235 ) ) ;
#38807 = CARTESIAN_POINT ( 'NONE',  ( -14.53748718939999840, 1415.677402282210096, 205.0892928880890054 ) ) ;
#38808 = CARTESIAN_POINT ( 'NONE',  ( 32.02808312589922224, 1511.187213306747708, 219.9649204700462235 ) ) ;
#38809 = CARTESIAN_POINT ( 'NONE',  ( -15.06652045519958349, 1415.677402202029953, 210.6308072257622541 ) ) ;
#38810 = CARTESIAN_POINT ( 'NONE',  ( 12.22832369420000020, 1445.155617767419926, 186.6170932793979773 ) ) ;
#38812 = CARTESIAN_POINT ( 'NONE',  ( 5.386599516782380803, 1432.386091107299762, 154.6080078439310057 ) ) ;
#38811 = CARTESIAN_POINT ( 'NONE',  ( -19.46735787119999728, 1444.804550784760067, 225.1090302134979879 ) ) ;
#38814 = CARTESIAN_POINT ( 'NONE',  ( -1.622337697689999914, 1484.281053948429872, 182.6410747883979866 ) ) ;
#38813 = AXIS2_PLACEMENT_3D ( 'NONE', #106033, #93870, #71918 ) ;
#38815 = EDGE_LOOP ( 'NONE', ( #41394, #47198, #33048, #30592 ) ) ;
#38816 = CARTESIAN_POINT ( 'NONE',  ( 2.479246847704999812, 1516.983612918759945, 205.0778556245070092 ) ) ;
#38817 = CARTESIAN_POINT ( 'NONE',  ( 0.8877057929439999828, 1405.849110591630051, 267.2346354947979989 ) ) ;
#38818 = CARTESIAN_POINT ( 'NONE',  ( 1.842963640640000067, 1515.372048646890107, 213.3835825195990026 ) ) ;
#38819 = CARTESIAN_POINT ( 'NONE',  ( 10.79528402730720060, 1489.628194868570063, 207.4012257063180016 ) ) ;
#38820 = CARTESIAN_POINT ( 'NONE',  ( 22.96977252851270990, 1432.194948239369296, 216.1620617374289850 ) ) ;
#38821 = CARTESIAN_POINT ( 'NONE',  ( 1.356372325302582782, 1463.975736616651602, 199.4023338319472884 ) ) ;
#38822 = DIRECTION ( 'NONE',  ( -1.000000000000000000, 0.000000000000000000, 0.000000000000000000 ) ) ;
#38823 = CARTESIAN_POINT ( 'NONE',  ( -4.817207246935718779, 1440.943601040120939, 201.7191942600521202 ) ) ;
#38824 = CARTESIAN_POINT ( 'NONE',  ( -1.179291431074050100, 1450.813351930680028, 155.3354871613740045 ) ) ;
#38825 = CARTESIAN_POINT ( 'NONE',  ( -1.624815496279135241, 1451.579047725773080, 184.0101596272184565 ) ) ;
#38826 = CARTESIAN_POINT ( 'NONE',  ( 2.496316844175979544, 1449.223786328959932, 155.0643092729569901 ) ) ;
#38827 = CARTESIAN_POINT ( 'NONE',  ( -13.94822761416910240, 1415.393085341430151, 220.8713811350969820 ) ) ;
#38828 = CARTESIAN_POINT ( 'NONE',  ( -4.175269160410000069, 1515.456655180189955, 210.6055574401990214 ) ) ;
#38829 = CARTESIAN_POINT ( 'NONE',  ( -28.52406122560000057, 1430.067484667830058, 255.3819207682979595 ) ) ;
#38830 = VECTOR ( 'NONE', #53016, 1000.000000000000000 ) ;
#38831 = DIRECTION ( 'NONE',  ( -1.000000000000000000, 0.000000000000000000, 0.000000000000000000 ) ) ;
#38832 = CARTESIAN_POINT ( 'NONE',  ( 2.499999926920000171, 1440.210289421680045, 168.7266379278979969 ) ) ;
#38833 = CARTESIAN_POINT ( 'NONE',  ( -6.209676061589999740, 1475.800420687429778, 267.8376408680979921 ) ) ;
#38834 = DIRECTION ( 'NONE',  ( -0.7067700363771036720, 0.03085824620770448792, -0.7067700363771036720 ) ) ;
#38835 = CARTESIAN_POINT ( 'NONE',  ( -9.526128307108560733, 1440.436522615020067, 205.9995050262249947 ) ) ;
#38836 = CARTESIAN_POINT ( 'NONE',  ( 6.232532001854651504, 1405.413060387330006, 220.5304192662728440 ) ) ;
#38837 = CARTESIAN_POINT ( 'NONE',  ( -41.36494379132859223, 1384.781339806650067, 244.5749991835589867 ) ) ;
#38838 = CARTESIAN_POINT ( 'NONE',  ( -4.994663984927831812, 1391.700789716822328, 214.7093307040285026 ) ) ;
#38839 = AXIS2_PLACEMENT_3D ( 'NONE', #465, #86644, #78811 ) ;
#38840 = CARTESIAN_POINT ( 'NONE',  ( -24.61293950550089704, 1444.770188684140066, 210.8869336946189890 ) ) ;
#38841 = CARTESIAN_POINT ( 'NONE',  ( -105.4633420800000039, 1378.947304614410086, 304.0408918711589763 ) ) ;
#38842 = CARTESIAN_POINT ( 'NONE',  ( 31.52384429374465569, 1525.730671948511599, 217.0357143952193724 ) ) ;
#38843 = CARTESIAN_POINT ( 'NONE',  ( -10.72715585175719966, 1396.287660924140027, 211.8461252756880242 ) ) ;
#38844 = B_SPLINE_CURVE_WITH_KNOTS ( 'NONE', 3,
 ( #59656, #37611, #45492, #60775 ),
 .UNSPECIFIED., .F., .F.,
 ( 4, 4 ),
 ( 0.000000000000000000, 1.000000000000000000 ),
 .UNSPECIFIED. ) ;
#38845 = CARTESIAN_POINT ( 'NONE',  ( -2.910436537626309939, 1508.551704408389924, 204.1692697258259841 ) ) ;
#38846 = CARTESIAN_POINT ( 'NONE',  ( 19.29701624502764190, 1455.937115892289057, 225.2550683788775814 ) ) ;
#38847 = ORIENTED_EDGE ( 'NONE', *, *, #96968, .T. ) ;
#38848 = LINE ( 'NONE', #75238, #98208 ) ;
#38849 = CARTESIAN_POINT ( 'NONE',  ( -7.530701528224715169, 1510.600498159482868, 214.9792805877740420 ) ) ;
#38850 = DIRECTION ( 'NONE',  ( 0.4229618813980365877, 0.9061474752402244315, 4.354426617128452806E-10 ) ) ;
#38852 = CARTESIAN_POINT ( 'NONE',  ( -12.73246623696499924, 1512.053076656670100, 193.2925894132669953 ) ) ;
#38851 = CARTESIAN_POINT ( 'NONE',  ( 10.52899685699999921, 1425.090219727929934, 126.2876617244979798 ) ) ;
#38853 = DIRECTION ( 'NONE',  ( 1.000000000000000000, 0.000000000000000000, 0.000000000000000000 ) ) ;
#38854 = CARTESIAN_POINT ( 'NONE',  ( -4.360511200180000380, 1454.978814463989920, 200.7714289439389859 ) ) ;
#38855 = CARTESIAN_POINT ( 'NONE',  ( 1.708747624254999931, 1517.213554313520035, 202.1696795498070003 ) ) ;
#38856 = CARTESIAN_POINT ( 'NONE',  ( 12.68801083313210043, 1500.413651417279880, 208.6561539661539939 ) ) ;
#38858 = CARTESIAN_POINT ( 'NONE',  ( 9.738317565070000015, 1493.400072498489862, 188.2659980885989910 ) ) ;
#38857 = AXIS2_PLACEMENT_3D ( 'NONE', #107133, #72997, #39381 ) ;
#38859 = CARTESIAN_POINT ( 'NONE',  ( 2.336427541990000023, 1507.413612230230001, 181.2610990600980188 ) ) ;
#38860 = FACE_BOUND ( 'NONE', #15687, .T. ) ;
#38861 = CARTESIAN_POINT ( 'NONE',  ( -93.69296856029690446, 1378.179795124779957, 305.3712508567500095 ) ) ;
#38862 = CARTESIAN_POINT ( 'NONE',  ( 4.724978704057813061, 1366.967019841526962, 208.3718459617061285 ) ) ;
#38864 = ORIENTED_EDGE ( 'NONE', *, *, #69224, .T. ) ;
#38863 = CARTESIAN_POINT ( 'NONE',  ( 17.22670715777832839, 1410.879751196339157, 192.2060273682096749 ) ) ;
#38865 = ORIENTED_EDGE ( 'NONE', *, *, #99821, .F. ) ;
#38866 = CARTESIAN_POINT ( 'NONE',  ( -14.45727104390000051, 1444.967096565130078, 188.7843282767979929 ) ) ;
#38867 = CARTESIAN_POINT ( 'NONE',  ( 2.871070354779960088, 1409.266853455240152, 231.0074625432760058 ) ) ;
#38868 = CARTESIAN_POINT ( 'NONE',  ( -1.159637561150000051, 1415.063410489829948, 226.6648382762980134 ) ) ;
#38869 = CARTESIAN_POINT ( 'NONE',  ( -0.0001401872352955277768, 1395.950288251542815, 220.5864547455709044 ) ) ;
#38870 = CARTESIAN_POINT ( 'NONE',  ( -14.28311008799576065, 1434.994877684804578, 148.2389552663005077 ) ) ;
#38871 = CARTESIAN_POINT ( 'NONE',  ( -7.583791944165000132, 1511.751588929339960, 211.4475770739170173 ) ) ;
#38873 = CARTESIAN_POINT ( 'NONE',  ( 16.74784213730000104, 1413.534413880030115, 226.5806976118979890 ) ) ;
#38872 = CARTESIAN_POINT ( 'NONE',  ( -103.5807003099999974, 1389.940341032420065, 304.1776946944589781 ) ) ;
#38874 = CARTESIAN_POINT ( 'NONE',  ( 14.16563741459999903, 1410.295047179630046, 191.3811060272979887 ) ) ;
#38875 = CARTESIAN_POINT ( 'NONE',  ( -2.384849065066879881, 1464.024019744329962, 199.4598481641620253 ) ) ;
#38876 = CARTESIAN_POINT ( 'NONE',  ( 8.445405620969070881, 1396.207980526650090, 201.9858892368549732 ) ) ;
#38877 = CARTESIAN_POINT ( 'NONE',  ( -39.61513715173970240, 1439.514898078000215, 136.6561437647560240 ) ) ;
#38878 = CARTESIAN_POINT ( 'NONE',  ( 10.81519956410000027, 1424.921090988229935, 144.1714224093980192 ) ) ;
#38879 = CARTESIAN_POINT ( 'NONE',  ( 41.48884051969999831, 1443.959437935279993, 136.5760756673980154 ) ) ;
#38880 = ORIENTED_EDGE ( 'NONE', *, *, #35506, .T. ) ;
#38881 = CARTESIAN_POINT ( 'NONE',  ( 3.842196749729999805, 1424.768327057229953, 185.0917902076980113 ) ) ;
#38882 = CARTESIAN_POINT ( 'NONE',  ( 1.857330175695710350, 1450.366835696837143, 181.8689242810781366 ) ) ;
#38883 = ORIENTED_EDGE ( 'NONE', *, *, #14136, .T. ) ;
#38884 = ORIENTED_EDGE ( 'NONE', *, *, #42812, .F. ) ;
#38885 = CARTESIAN_POINT ( 'NONE',  ( -17.95163359629999533, 1488.038499059930018, 229.1097482272980130 ) ) ;
#38886 = DIRECTION ( 'NONE',  ( -0.6736849260863841948, 0.000000000000000000, 0.7390186874254148774 ) ) ;
#38887 = CIRCLE ( 'NONE', #71141, 1.999999999999999556 ) ;
#38888 = CARTESIAN_POINT ( 'NONE',  ( -109.4005255434914972, 1387.066694983333036, 311.0856849982282029 ) ) ;
#38889 = CARTESIAN_POINT ( 'NONE',  ( 6.556651371285000529, 1516.858146885269889, 215.6747433371770057 ) ) ;
#38890 = CARTESIAN_POINT ( 'NONE',  ( -12.34596455585159980, 1378.847116221920032, 209.2104869998679817 ) ) ;
#38891 = ORIENTED_EDGE ( 'NONE', *, *, #104881, .F. ) ;
#38892 = CARTESIAN_POINT ( 'NONE',  ( -17.18922504907660098, 1508.551704422510056, 212.4816474524029957 ) ) ;
#38893 = CARTESIAN_POINT ( 'NONE',  ( -8.942586000020730452, 1509.338997363079898, 180.2808501620069990 ) ) ;
#38894 = CARTESIAN_POINT ( 'NONE',  ( -50.14839348009999753, 1380.010081756269983, 242.5009839091590038 ) ) ;
#38895 = ADVANCED_FACE ( 'NONE', ( #73327 ), #49113, .T. ) ;
#38896 = CARTESIAN_POINT ( 'NONE',  ( -15.42462372342430932, 1461.099982565929849, 228.7269502612183771 ) ) ;
#38897 = CARTESIAN_POINT ( 'NONE',  ( -1.714334285315000095, 1516.699825673279975, 205.0952314524469955 ) ) ;
#38898 = ORIENTED_EDGE ( 'NONE', *, *, #30443, .F. ) ;
#38899 = CARTESIAN_POINT ( 'NONE',  ( -8.509555873503130030, 1452.079233855630036, 205.3893997472640081 ) ) ;
#38900 = EDGE_CURVE ( 'NONE', #64568, #74476, #18441, .T. ) ;
#38901 = CARTESIAN_POINT ( 'NONE',  ( -35.14253230574213660, 1424.207438634963864, 269.5334840037577351 ) ) ;
#38902 = CARTESIAN_POINT ( 'NONE',  ( -1.637939388229999960, 1410.349266066630207, 232.9014652880979952 ) ) ;
#38904 = VERTEX_POINT ( 'NONE', #2096 ) ;
#38903 = CARTESIAN_POINT ( 'NONE',  ( -10.78330898009999927, 1453.313060387329870, 191.8873814369979982 ) ) ;
#38905 = DIRECTION ( 'NONE',  ( 0.000000000000000000, 0.000000000000000000, -1.000000000000000000 ) ) ;
#38906 = CARTESIAN_POINT ( 'NONE',  ( -35.38730834711080320, 1440.913060388089889, 251.6904557940889902 ) ) ;
#38907 = CARTESIAN_POINT ( 'NONE',  ( -49.58793988690000276, 1384.741903095260113, 260.9101892837590526 ) ) ;
#38908 = CARTESIAN_POINT ( 'NONE',  ( -0.3690490828443839799, 1465.421766398420004, 236.2943576644740062 ) ) ;
#38909 = CARTESIAN_POINT ( 'NONE',  ( 15.30542547920000018, 1410.181902236829728, 270.3573229405980101 ) ) ;
#38910 = CARTESIAN_POINT ( 'NONE',  ( -6.547881413045000265, 1516.647534046129977, 212.5778533554070293 ) ) ;
#38911 = CARTESIAN_POINT ( 'NONE',  ( -50.79448650070000326, 1379.685520326630012, 241.2356115758589965 ) ) ;
#38912 = VECTOR ( 'NONE', #57218, 1000.000000000000000 ) ;
#38913 = CARTESIAN_POINT ( 'NONE',  ( 23.05752159060000039, 1409.824208518830119, 208.4404237973319880 ) ) ;
#38914 = CARTESIAN_POINT ( 'NONE',  ( 28.27139721233031722, 1526.382868172864164, 198.6830693683572235 ) ) ;
#38915 = CARTESIAN_POINT ( 'NONE',  ( 12.72813482502530036, 1426.626821931249879, 196.2928140043740086 ) ) ;
#38916 = CIRCLE ( 'NONE', #46164, 7.975189853890007896 ) ;
#38917 = CARTESIAN_POINT ( 'NONE',  ( -7.709047995734989556, 1516.534924556719943, 211.5762535550240102 ) ) ;
#38918 = CARTESIAN_POINT ( 'NONE',  ( 1.717139084115000047, 1516.949031626070109, 210.2396860569670025 ) ) ;
#38919 = CARTESIAN_POINT ( 'NONE',  ( 4.267709349675449459, 1420.674582551029971, 185.5795260963529927 ) ) ;
#38920 = CARTESIAN_POINT ( 'NONE',  ( -8.480871446589999252, 1420.439733004030131, 230.9234419115979904 ) ) ;
#38921 =( BOUNDED_SURFACE ( )  B_SPLINE_SURFACE ( 3, 2, ( 
 ( #100369, #23654, #93058 ),
 ( #91963, #14701, #49973 ),
 ( #6846, #39915, #15239 ),
 ( #75185, #41007, #32619 ),
 ( #24191, #58378, #65131 ),
 ( #109874, #92504, #49431 ),
 ( #84109, #7409, #41574 ),
 ( #58927, #67342, #74084 ),
 ( #101440, #24730, #108213 ),
 ( #16332, #7954, #73535 ),
 ( #31501, #107671, #30956 ),
 ( #91426, #48890, #83018 ) ),
 .UNSPECIFIED., .F., .F., .F. ) 
 B_SPLINE_SURFACE_WITH_KNOTS ( ( 4, 2, 2, 2, 2, 4 ),
 ( 3, 3 ),
 ( -4.818654156246715559E-13, 0.0004428215754125967830, 0.0008856431513070589815, 0.001328464727201521126, 0.001549875515148752252, 0.001771286303095983379 ),
 ( 0.000000000000000000, 1.000000000000000000 ),
 .UNSPECIFIED. ) 
 GEOMETRIC_REPRESENTATION_ITEM ( )  RATIONAL_B_SPLINE_SURFACE ( (
 ( 1.000000000000000000, 0.8676549166461677842, 1.000000000000000000),
 ( 1.000000000000000000, 0.8796972043940699537, 1.000000000000000000),
 ( 1.000000000000000000, 0.8923052904408216301, 1.000000000000000000),
 ( 1.000000000000000000, 0.9171311462241392709, 1.000000000000000000),
 ( 1.000000000000000000, 0.9293640644949126006, 1.000000000000000000),
 ( 1.000000000000000000, 0.9509457646758097127, 1.000000000000000000),
 ( 1.000000000000000000, 0.9602070476915617325, 1.000000000000000000),
 ( 1.000000000000000000, 0.9693527540417160582, 1.000000000000000000),
 ( 1.000000000000000000, 0.9716220080584853092, 1.000000000000000000),
 ( 1.000000000000000000, 0.9742788806458316797, 1.000000000000000000),
 ( 1.000000000000000000, 0.9746510992719278343, 1.000000000000000000),
 ( 1.000000000000000000, 0.9740160527066915597, 1.000000000000000000) ) ) 
 REPRESENTATION_ITEM ( '' )  SURFACE ( )  );
#38922 = CARTESIAN_POINT ( 'NONE',  ( 10.49818696109023186, 1422.381269827019423, 137.0999999980981272 ) ) ;
#38923 = ORIENTED_EDGE ( 'NONE', *, *, #6278, .T. ) ;
#38924 = CARTESIAN_POINT ( 'NONE',  ( -30.72941576718060119, 1385.230165571390216, 228.8128147210159966 ) ) ;
#38925 = DIRECTION ( 'NONE',  ( -0.6736849260863837507, 0.000000000000000000, 0.7390186874254154326 ) ) ;
#38926 = CARTESIAN_POINT ( 'NONE',  ( 0.9892016712189999339, 1417.304970919730067, 235.7878985900979956 ) ) ;
#38927 = LINE ( 'NONE', #4781, #55789 ) ;
#38928 = CARTESIAN_POINT ( 'NONE',  ( 7.572192850525000019, 1511.308638870219966, 206.5572121486769959 ) ) ;
#38929 = CARTESIAN_POINT ( 'NONE',  ( 11.54684311930000007, 1425.837099041209967, 203.6587523742389862 ) ) ;
#38930 = FACE_OUTER_BOUND ( 'NONE', #92111, .T. ) ;
#38932 = CARTESIAN_POINT ( 'NONE',  ( 18.06717587838990013, 1416.826860677879949, 208.8995450462120118 ) ) ;
#38931 = CARTESIAN_POINT ( 'NONE',  ( 0.01126491619350150110, 1516.939530130779985, 216.0663127125970107 ) ) ;
#38933 = DIRECTION ( 'NONE',  ( 0.000000000000000000, 0.000000000000000000, -1.000000000000000000 ) ) ;
#38934 = CARTESIAN_POINT ( 'NONE',  ( 11.19499699576850027, 1470.359902562939851, 207.1673228584000128 ) ) ;
#38935 = VERTEX_POINT ( 'NONE', #55253 ) ;
#38936 = CARTESIAN_POINT ( 'NONE',  ( -3.454748846324999789, 1516.609912606490070, 201.7988116581369979 ) ) ;
#38937 = CARTESIAN_POINT ( 'NONE',  ( 29.22958591724099975, 1509.933780020319773, 206.4713313096740137 ) ) ;
#38938 = ORIENTED_EDGE ( 'NONE', *, *, #15873, .F. ) ;
#38939 = CARTESIAN_POINT ( 'NONE',  ( 21.84020450222056908, 1523.382868172864164, 234.9798068779740277 ) ) ;
#38940 = CARTESIAN_POINT ( 'NONE',  ( 20.46232921600000054, 1454.237003251030046, 223.5521112539979924 ) ) ;
#38941 = CARTESIAN_POINT ( 'NONE',  ( 8.057909095891742979, 1438.036219788864173, 153.6519697238730942 ) ) ;
#38942 = CARTESIAN_POINT ( 'NONE',  ( 7.550412389219739673, 1510.476657126699820, 203.5713960734849763 ) ) ;
#38943 = CARTESIAN_POINT ( 'NONE',  ( 2.663026065689999999, 1442.012083350790135, 217.9487819464190181 ) ) ;
#38944 = CARTESIAN_POINT ( 'NONE',  ( -27.24127397847530219, 1509.605191577599953, 201.1898831551650062 ) ) ;
#38945 = CARTESIAN_POINT ( 'NONE',  ( -10.10004869885203682, 1411.254281879943164, 135.5999999980979851 ) ) ;
#38946 = CARTESIAN_POINT ( 'NONE',  ( -19.15018216310000199, 1426.147315663830113, 224.7566274145979719 ) ) ;
#38947 = CARTESIAN_POINT ( 'NONE',  ( -31.74245818353665172, 1465.468252347056250, 269.3210959786474064 ) ) ;
#38948 = CARTESIAN_POINT ( 'NONE',  ( -103.5806803890000083, 1389.940350142260058, 304.1776731731589507 ) ) ;
#38949 = CARTESIAN_POINT ( 'NONE',  ( -3.061616997868380553E-17, 1389.413060387289988, 209.1218459616989946 ) ) ;
#38950 = B_SPLINE_CURVE_WITH_KNOTS ( 'NONE', 4,
 ( #96377, #96936, #53859, #29711, #45448 ),
 .UNSPECIFIED., .F., .F.,
 ( 5, 5 ),
 ( 0.000000000000000000, 1.000000000000000000 ),
 .UNSPECIFIED. ) ;
#38952 = CARTESIAN_POINT ( 'NONE',  ( -18.31626795570251076, 1436.062568559702640, 213.5329773601903298 ) ) ;
#38951 = CARTESIAN_POINT ( 'NONE',  ( -106.5381113420000077, 1391.812866088840110, 301.3072072504589869 ) ) ;
#38953 = CARTESIAN_POINT ( 'NONE',  ( -9.946114271644979965, 1472.218658670100012, 211.2590325883199966 ) ) ;
#38954 = ORIENTED_EDGE ( 'NONE', *, *, #96530, .F. ) ;
#38955 = FACE_OUTER_BOUND ( 'NONE', #54913, .T. ) ;
#38956 = CARTESIAN_POINT ( 'NONE',  ( -14.36727199889999973, 1508.541240743890057, 215.8627312463090107 ) ) ;
#38957 = CARTESIAN_POINT ( 'NONE',  ( 3.350338079455601026, 1523.604703353109699, 242.0808062845893289 ) ) ;
#38958 = AXIS2_PLACEMENT_3D ( 'NONE', #85958, #78664, #86503 ) ;
#38959 = CARTESIAN_POINT ( 'NONE',  ( -17.19739463999606599, 1525.960063244516959, 236.2603809477411971 ) ) ;
#38960 = CARTESIAN_POINT ( 'NONE',  ( -113.4000000000000057, 1384.913060387289988, 304.2218459572590064 ) ) ;
#38961 = CARTESIAN_POINT ( 'NONE',  ( 1.469130622283230103, 1487.271942394239886, 181.9786426215879942 ) ) ;
#38962 = CARTESIAN_POINT ( 'NONE',  ( -3.355802132529050574, 1523.843271061949963, 242.0624703644778606 ) ) ;
#38963 = CARTESIAN_POINT ( 'NONE',  ( -12.92553196027594176, 1442.905430701026944, 186.4482871715469514 ) ) ;
#38964 = CARTESIAN_POINT ( 'NONE',  ( -7.500000019064999357, 1516.934643012909874, 209.1218459511669892 ) ) ;
#38965 = CARTESIAN_POINT ( 'NONE',  ( -8.313145311751080513, 1507.316772571419961, 235.1568484389069909 ) ) ;
#38966 = CYLINDRICAL_SURFACE ( 'NONE', #11006, 33.13701971169416538 ) ;
#38967 = CARTESIAN_POINT ( 'NONE',  ( -14.61097672478990006, 1415.677402205059934, 205.8812875983110189 ) ) ;
#38968 = EDGE_CURVE ( 'NONE', #7623, #94000, #65417, .T. ) ;
#38969 = FACE_OUTER_BOUND ( 'NONE', #64404, .T. ) ;
#38970 = CARTESIAN_POINT ( 'NONE',  ( 6.938871378149999991, 1427.890279811890196, 213.8982594654290210 ) ) ;
#38972 = ORIENTED_EDGE ( 'NONE', *, *, #24827, .F. ) ;
#38971 = CARTESIAN_POINT ( 'NONE',  ( 19.35628570429999940, 1496.398810548190113, 218.7515486585290034 ) ) ;
#38973 = DIRECTION ( 'NONE',  ( -0.6736849260863841948, 0.000000000000000000, 0.7390186874254148774 ) ) ;
#38974 = EDGE_CURVE ( 'NONE', #99156, #42052, #17076, .T. ) ;
#38975 = CARTESIAN_POINT ( 'NONE',  ( 12.72383573552339975, 1512.260118274589786, 224.2302556167890089 ) ) ;
#38976 = ORIENTED_EDGE ( 'NONE', *, *, #108860, .F. ) ;
#38977 = ORIENTED_EDGE ( 'NONE', *, *, #84249, .T. ) ;
#38978 = EDGE_CURVE ( 'NONE', #17947, #84814, #70807, .T. ) ;
#38979 = CARTESIAN_POINT ( 'NONE',  ( 18.05542472024740164, 1416.825783990419950, 208.7596433786079899 ) ) ;
#38980 = CARTESIAN_POINT ( 'NONE',  ( -109.7177012239999954, 1384.912553384849843, 297.0861780560589978 ) ) ;
#38981 = CARTESIAN_POINT ( 'NONE',  ( -11.42312749683812356, 1378.600463633266827, 204.4622889030064243 ) ) ;
#38983 = CARTESIAN_POINT ( 'NONE',  ( -31.18244400280000050, 1447.044067085910001, 244.2061907774979943 ) ) ;
#38982 = CARTESIAN_POINT ( 'NONE',  ( 38.80991273106157280, 1429.204819279143976, 269.5897298496287817 ) ) ;
#38984 = CARTESIAN_POINT ( 'NONE',  ( -20.14249648099999845, 1499.094827274529962, 189.7136622036979929 ) ) ;
#38985 = AXIS2_PLACEMENT_3D ( 'NONE', #94711, #45443, #86864 ) ;
#38986 = CARTESIAN_POINT ( 'NONE',  ( -11.21637391500000192, 1433.532588004509989, 151.5878911200980212 ) ) ;
#38987 = CARTESIAN_POINT ( 'NONE',  ( -5.134308048384249940E-13, 1492.051704408390151, 209.1218459616989946 ) ) ;
#38988 = CARTESIAN_POINT ( 'NONE',  ( -19.52948423790000021, 1485.515647422730126, 190.0633780688980039 ) ) ;
#38989 = CARTESIAN_POINT ( 'NONE',  ( 9.554826419470950682, 1464.136006249749926, 211.3862083144839801 ) ) ;
#38990 = CARTESIAN_POINT ( 'NONE',  ( 0.6516344981559789584, 1515.134688985610182, 213.4494644436790054 ) ) ;
#38991 = CARTESIAN_POINT ( 'NONE',  ( 8.778727692719998643, 1440.670317412140093, 153.7060891647979872 ) ) ;
#38992 = CARTESIAN_POINT ( 'NONE',  ( 13.13254582842679774, 1428.645359689489851, 223.2771978780310178 ) ) ;
#38993 = VECTOR ( 'NONE', #81379, 1000.000000000000000 ) ;
#38994 = CARTESIAN_POINT ( 'NONE',  ( -4.280544930714631491, 1362.872105239078792, 209.6218459617148824 ) ) ;
#38995 = CARTESIAN_POINT ( 'NONE',  ( 30.99338347247808656, 1526.382868172863937, 199.8717226395764044 ) ) ;
#38997 = ORIENTED_EDGE ( 'NONE', *, *, #44750, .F. ) ;
#38996 = CARTESIAN_POINT ( 'NONE',  ( 5.267020990686269920E-09, 1406.060656444949927, 266.8269676183700199 ) ) ;
#38998 = VERTEX_POINT ( 'NONE', #27826 ) ;
#38999 = CARTESIAN_POINT ( 'NONE',  ( -11.86610048948770135, 1432.336024750160050, 149.9824232984959735 ) ) ;
#39000 = CARTESIAN_POINT ( 'NONE',  ( -18.74924298070000006, 1506.108474969089912, 222.6729604708989996 ) ) ;
#39001 = CARTESIAN_POINT ( 'NONE',  ( -24.89782654780000115, 1466.147263882030074, 269.9192101110980389 ) ) ;
#39002 = CARTESIAN_POINT ( 'NONE',  ( 13.08557583159999993, 1509.198239579430037, 234.3544144791979988 ) ) ;
#39003 = CARTESIAN_POINT ( 'NONE',  ( 9.421550853199999409, 1433.443826258700028, 153.1575888881980063 ) ) ;
#39004 = CARTESIAN_POINT ( 'NONE',  ( -11.52816659857622561, 1414.661898229710005, 206.9304423160286888 ) ) ;
#39005 = CARTESIAN_POINT ( 'NONE',  ( 0.2165510715247410123, 1452.950780108749996, 183.2553406918169969 ) ) ;
#39006 = CARTESIAN_POINT ( 'NONE',  ( -9.849896899200842881, 1519.913060387329779, 185.5490084180013923 ) ) ;
#39007 = DIRECTION ( 'NONE',  ( -1.000000000000000000, 0.000000000000000000, 0.000000000000000000 ) ) ;
#39008 = CARTESIAN_POINT ( 'NONE',  ( -3.345499056600000021, 1457.924539801389983, 218.8450915141490043 ) ) ;
#39009 = CARTESIAN_POINT ( 'NONE',  ( 10.13733714734278024, 1367.141848830506206, 207.6218459616987673 ) ) ;
#39010 = CARTESIAN_POINT ( 'NONE',  ( -41.85400445561560190, 1426.437045596680036, 268.8779146404949643 ) ) ;
#39011 = ORIENTED_EDGE ( 'NONE', *, *, #66682, .F. ) ;
#39012 = CARTESIAN_POINT ( 'NONE',  ( -11.45492292490000175, 1391.035318004910096, 204.4802647352790075 ) ) ;
#39013 = ORIENTED_EDGE ( 'NONE', *, *, #17992, .T. ) ;
#39014 = EDGE_LOOP ( 'NONE', ( #81117, #59701, #35013, #70948 ) ) ;
#39015 = CARTESIAN_POINT ( 'NONE',  ( -3.251394400264999707, 1516.757508073510053, 210.8375504612070017 ) ) ;
#39016 = CARTESIAN_POINT ( 'NONE',  ( 17.11714618744286653, 1444.740067931808881, 162.7561046190442369 ) ) ;
#39017 = AXIS2_PLACEMENT_3D ( 'NONE', #86123, #11086, #96182 ) ;
#39019 = CARTESIAN_POINT ( 'NONE',  ( 0.000000000000000000, 1523.382868172864164, 209.1218459616979999 ) ) ;
#39018 = CARTESIAN_POINT ( 'NONE',  ( 3.267603515704999850, 1516.858171774179937, 212.3749871074670068 ) ) ;
#39020 = CARTESIAN_POINT ( 'NONE',  ( -13.16389777740000078, 1440.431676128409890, 188.3426591800980248 ) ) ;
#39021 = CARTESIAN_POINT ( 'NONE',  ( -15.90881031062220075, 1461.182782413890209, 228.4097491243460070 ) ) ;
#39022 = ORIENTED_EDGE ( 'NONE', *, *, #107501, .T. ) ;
#39023 = CARTESIAN_POINT ( 'NONE',  ( 9.803834995107230554, 1517.051704408389924, 221.6221720662910002 ) ) ;
#39024 = CARTESIAN_POINT ( 'NONE',  ( -5.004442077115000664, 1516.690345681169902, 201.4087281291169802 ) ) ;
#39025 = ADVANCED_FACE ( 'NONE', ( #21050 ), #7091, .T. ) ;
#39026 = DIRECTION ( 'NONE',  ( 0.000000000000000000, -0.8237382389120454507, 0.5669702935375731112 ) ) ;
#39027 = CARTESIAN_POINT ( 'NONE',  ( -27.30026132067300182, 1384.549843020650087, 204.2521262686249770 ) ) ;
#39028 = CARTESIAN_POINT ( 'NONE',  ( -39.91390632348250023, 1425.727616005299978, 270.2554194705400050 ) ) ;
#39029 = DIRECTION ( 'NONE',  ( 3.828568698926945984E-16, 0.000000000000000000, -1.000000000000000000 ) ) ;
#39030 = CARTESIAN_POINT ( 'NONE',  ( -2.403335121230000038, 1396.180591763030179, 197.3371931114980100 ) ) ;
#39032 = EDGE_LOOP ( 'NONE', ( #30173, #105285, #12396, #24556 ) ) ;
#39031 = CARTESIAN_POINT ( 'NONE',  ( -9.516636888329999877, 1366.309137899869938, 207.6218459616989946 ) ) ;
#39033 = ORIENTED_EDGE ( 'NONE', *, *, #68675, .F. ) ;
#39034 = LINE ( 'NONE', #82151, #942 ) ;
#39035 = CARTESIAN_POINT ( 'NONE',  ( 1.476582328747939821, 1467.059268612629921, 220.0911334793899812 ) ) ;
#39036 = CARTESIAN_POINT ( 'NONE',  ( 3.005276066430000448, 1369.205039411269809, 210.6218459616989946 ) ) ;
#39037 = CARTESIAN_POINT ( 'NONE',  ( -0.03715205675588980488, 1409.647736300129964, 185.2081566933059946 ) ) ;
#39038 = CARTESIAN_POINT ( 'NONE',  ( -4.610079871555000430, 1516.713079096360161, 210.2553629353369899 ) ) ;
#39039 = CARTESIAN_POINT ( 'NONE',  ( 6.006124716077446024, 1460.017935509939662, 201.5831662601001995 ) ) ;
#39040 = CARTESIAN_POINT ( 'NONE',  ( 9.906408661899998691, 1453.734930172990062, 213.0153772767789917 ) ) ;
#39041 = CARTESIAN_POINT ( 'NONE',  ( 4.124003890242169845, 1440.791985383939846, 218.1323065870639937 ) ) ;
#39042 = CARTESIAN_POINT ( 'NONE',  ( 12.78690713350000152, 1416.828040475229955, 222.7042044314979989 ) ) ;
#39043 = CARTESIAN_POINT ( 'NONE',  ( 7.635834362694999378, 1511.005930286180046, 205.1946200654369932 ) ) ;
#39044 = VERTEX_POINT ( 'NONE', #70410 ) ;
#39045 = CARTESIAN_POINT ( 'NONE',  ( -6.564578723344999922, 1517.199196846569976, 207.4137433428170141 ) ) ;
#39046 = EDGE_LOOP ( 'NONE', ( #70811, #106379, #52505, #87191, #36416 ) ) ;
#39047 = CARTESIAN_POINT ( 'NONE',  ( -33.91369104902859988, 1451.728768199629940, 135.6928041595160153 ) ) ;
#39049 = B_SPLINE_CURVE_WITH_KNOTS ( 'NONE', 5,
 ( #8736, #27215, #384, #35054, #69797, #7644 ),
 .UNSPECIFIED., .F., .F.,
 ( 6, 6 ),
 ( -167.9874969530119984, -30.64195154390000653 ),
 .UNSPECIFIED. ) ;
#39048 = CARTESIAN_POINT ( 'NONE',  ( -23.50051618060902570, 1448.308771251206053, 215.7218330829513775 ) ) ;
#39050 = ORIENTED_EDGE ( 'NONE', *, *, #22759, .T. ) ;
#39051 = CARTESIAN_POINT ( 'NONE',  ( 9.531827753298708572, 1455.676400814010321, 226.7632778638479465 ) ) ;
#39052 = CARTESIAN_POINT ( 'NONE',  ( 24.84980271777819993, 1451.808520470279973, 136.8918982205989892 ) ) ;
#39053 = CARTESIAN_POINT ( 'NONE',  ( 13.46339118210000052, 1415.263254644529979, 197.1639476829979856 ) ) ;
#39054 = CARTESIAN_POINT ( 'NONE',  ( -11.68639022133180028, 1416.948096802419968, 211.2488954177810001 ) ) ;
#39055 = CARTESIAN_POINT ( 'NONE',  ( 19.75836274200000275, 1410.963915033830062, 196.8094767124980251 ) ) ;
#39056 = B_SPLINE_CURVE_WITH_KNOTS ( 'NONE', 3,
 ( #42759, #36021, #44426, #60127, #76920, #53382, #1316, #1884, #43864, #10818, #86958, #68529, #78569, #25375, #9696, #44988, #16960, #85857, #36559, #70211, #52829, #27609 ),
 .UNSPECIFIED., .F., .F.,
 ( 4, 3, 3, 3, 3, 3, 3, 4 ),
 ( -2.000000000000000000, -1.902662651915229874, -1.582520240992760119, -1.259666668549479951, -0.9395862512417130219, -0.6254581966034109541, -0.3129536411610209790, 0.000000000000000000 ),
 .UNSPECIFIED. ) ;
#39057 = CARTESIAN_POINT ( 'NONE',  ( 16.66094735740000132, 1410.867388120730084, 226.5061907895980085 ) ) ;
#39058 = CARTESIAN_POINT ( 'NONE',  ( -14.08275829279420499, 1379.695270052737214, 211.5466488430092795 ) ) ;
#39059 = DIRECTION ( 'NONE',  ( -0.8090169943749422332, 0.000000000000000000, 0.5877852522924802425 ) ) ;
#39060 = CARTESIAN_POINT ( 'NONE',  ( 22.36671582959205651, 1452.044573827695331, 219.5114896727811811 ) ) ;
#39061 = EDGE_CURVE ( 'NONE', #103217, #108761, #61354, .T. ) ;
#39062 = CARTESIAN_POINT ( 'NONE',  ( 2.500000000000000000, 1439.615672362369878, 170.5246407131980106 ) ) ;
#39063 = CIRCLE ( 'NONE', #26600, 1.999999999999999556 ) ;
#39064 = CARTESIAN_POINT ( 'NONE',  ( 4.618749068485000109, 1516.729202374750002, 215.6716084172169872 ) ) ;
#39065 = VERTEX_POINT ( 'NONE', #63660 ) ;
#39066 = CARTESIAN_POINT ( 'NONE',  ( 7.709271376012959642, 1516.543456561459834, 206.4978234970299980 ) ) ;
#39067 = B_SPLINE_SURFACE_WITH_KNOTS ( 'NONE', 5, 5, ( 
 ( #50360, #65503, #49249, #22896, #99612, #91774, #48701, #75557, #100717 ),
 ( #41939, #101254, #74458, #16157, #75004, #39731, #109154, #100185, #84486 ),
 ( #92323, #57105, #7773, #83372, #22343, #23999, #24553, #108023, #32438 ),
 ( #6117, #109691, #31872, #108586, #110233, #23468, #15052, #14511, #90671 ),
 ( #6673, #40826, #82825, #64950, #99064, #56543, #57662, #66614, #48144 ),
 ( #15594, #83930, #82283, #7232, #41392, #32967, #60974, #68820, #511 ),
 ( #34636, #61522, #26786, #59315, #60410, #50896, #95099, #35187, #1060 ),
 ( #10543, #94528, #18365, #95650, #67708, #110789, #85026, #8867, #17802 ),
 ( #25111, #35744, #76637, #77751, #52003, #18917, #102921, #43600, #85570 ),
 ( #43051, #52560, #69931, #104044, #8319, #44717, #69372, #78869, #53115 ),
 ( #26221, #86693, #42480, #77208, #33507, #101817, #103481, #93427, #34082 ),
 ( #86143, #16696, #9436, #9987, #25664, #68275, #102382, #44157, #78293 ),
 ( #87252, #59857, #93981, #17247, #51440, #1607, #27336, #70483, #55875 ),
 ( #71602, #88357, #20035, #12187, #4360, #11646, #19480, #105723, #29006 ),
 ( #53682, #106255, #13271, #87824, #46380, #3273, #47462, #29541, #80512 ) ),
 .UNSPECIFIED., .F., .F., .F.,
 ( 6, 3, 3, 3, 6 ),
 ( 6, 3, 6 ),
 ( 71.01177471054140256, 77.03401477149999721, 87.95300694690000398, 98.87199912229999654, 105.5884550614849928 ),
 ( 0.000000000000000000, 1.000000000000000000, 2.000579642670969882 ),
 .UNSPECIFIED. ) ;
#39068 = CARTESIAN_POINT ( 'NONE',  ( -44.50818758269999620, 1445.910501413080055, 269.6919245774980141 ) ) ;
#39069 = CIRCLE ( 'NONE', #6955, 5.133097426430088817 ) ;
#39070 = CARTESIAN_POINT ( 'NONE',  ( -3.609371144360000283, 1448.978751989720195, 184.9854825331979953 ) ) ;
#39071 = AXIS2_PLACEMENT_3D ( 'NONE', #4655, #75180, #91421 ) ;
#39072 = DIRECTION ( 'NONE',  ( 0.000000000000000000, 0.000000000000000000, -1.000000000000000000 ) ) ;
#39073 = CARTESIAN_POINT ( 'NONE',  ( -40.26396455803409680, 1444.186530478750001, 137.1012301494149881 ) ) ;
#39074 = CARTESIAN_POINT ( 'NONE',  ( 11.60004869885203682, 1425.898600695503546, 137.5181336713743292 ) ) ;
#39075 = CARTESIAN_POINT ( 'NONE',  ( -4.500000000000000000, 1425.929641636930000, 127.2892455880980123 ) ) ;
#39076 = CARTESIAN_POINT ( 'NONE',  ( -2.500000000000000000, 1419.454841297830171, 146.2312480424980095 ) ) ;
#39077 = CARTESIAN_POINT ( 'NONE',  ( -1.165022167831349931, 1455.263797152349980, 198.6710384306789763 ) ) ;
#39078 = CARTESIAN_POINT ( 'NONE',  ( -22.08622291488090639, 1523.456924617336426, 184.4183880513689928 ) ) ;
#39079 = CARTESIAN_POINT ( 'NONE',  ( 32.01195192442499859, 1440.913060383300035, 244.1429064951479972 ) ) ;
#39080 = CARTESIAN_POINT ( 'NONE',  ( -10.07722745004169873, 1471.911775314289798, 210.4363667124119672 ) ) ;
#39081 = CARTESIAN_POINT ( 'NONE',  ( -103.4000000000000057, 1378.913060387289988, 304.2218459572590064 ) ) ;
#39082 = VERTEX_POINT ( 'NONE', #47391 ) ;
#39083 = ORIENTED_EDGE ( 'NONE', *, *, #56184, .F. ) ;
#39084 = CARTESIAN_POINT ( 'NONE',  ( 10.55265553690759894, 1480.891686322609985, 208.8870839355319902 ) ) ;
#39085 = CARTESIAN_POINT ( 'NONE',  ( 45.67177343720949523, 1440.913060382069943, 266.1885934449759930 ) ) ;
#39086 = CARTESIAN_POINT ( 'NONE',  ( -4.553268120680000308, 1442.065311926689901, 201.3752710187589798 ) ) ;
#39087 = CARTESIAN_POINT ( 'NONE',  ( -14.17772861730700207, 1379.591530685439920, 207.8208986668599891 ) ) ;
#39088 = CIRCLE ( 'NONE', #33737, 2.000000000000001776 ) ;
#39089 = CARTESIAN_POINT ( 'NONE',  ( 15.08448175589999884, 1409.953164874830009, 191.7150831455979869 ) ) ;
#39090 = CARTESIAN_POINT ( 'NONE',  ( -30.60461244942468184, 1523.621879633028584, 221.8232741897821541 ) ) ;
#39091 = CARTESIAN_POINT ( 'NONE',  ( -50.45191962221719706, 1383.811169775679900, 262.2738409289869992 ) ) ;
#39092 = ADVANCED_FACE ( 'NONE', ( #4815 ), #91088, .T. ) ;
#39093 = CARTESIAN_POINT ( 'NONE',  ( -3.611462641674999752, 1511.572472350439739, 201.0497519038969756 ) ) ;
#39094 = EDGE_CURVE ( 'NONE', #5500, #52165, #83910, .T. ) ;
#39095 = CARTESIAN_POINT ( 'NONE',  ( -13.41982536019999905, 1453.154034701130058, 193.5350393489979979 ) ) ;
#39096 = CARTESIAN_POINT ( 'NONE',  ( -11.44991336099019819, 1501.249626596179951, 208.6595951068130148 ) ) ;
#39097 = CARTESIAN_POINT ( 'NONE',  ( 1.394897302499999991, 1465.720900699230015, 235.3343340621979962 ) ) ;
#39098 = EDGE_CURVE ( 'NONE', #19743, #69935, #34531, .T. ) ;
#39100 = ORIENTED_EDGE ( 'NONE', *, *, #2268, .F. ) ;
#39099 = CYLINDRICAL_SURFACE ( 'NONE', #24607, 2.000000000000001776 ) ;
#39101 = CARTESIAN_POINT ( 'NONE',  ( -0.6413067440629999227, 1451.969509408830163, 183.1830565138979807 ) ) ;
#39102 = CARTESIAN_POINT ( 'NONE',  ( -19.23736494940000341, 1383.854422637459948, 220.3626903602589948 ) ) ;
#39103 = EDGE_CURVE ( 'NONE', #50508, #105303, #76188, .T. ) ;
#39104 = CARTESIAN_POINT ( 'NONE',  ( 3.219327822800559957, 1508.551704408389924, 204.2443104558009850 ) ) ;
#39106 = ORIENTED_EDGE ( 'NONE', *, *, #22963, .T. ) ;
#39105 = CARTESIAN_POINT ( 'NONE',  ( -18.09118544614330304, 1416.225364278609959, 209.0355310070899861 ) ) ;
#39107 = CARTESIAN_POINT ( 'NONE',  ( -18.32378034181390092, 1464.077664432049914, 217.4721294711199846 ) ) ;
#39108 = ORIENTED_EDGE ( 'NONE', *, *, #47457, .T. ) ;
#39109 = EDGE_CURVE ( 'NONE', #1227, #68445, #35017, .T. ) ;
#39110 = CARTESIAN_POINT ( 'NONE',  ( -10.91935502263179991, 1388.739090993680065, 216.4564496294659932 ) ) ;
#39111 = FACE_OUTER_BOUND ( 'NONE', #87954, .T. ) ;
#39112 = CARTESIAN_POINT ( 'NONE',  ( -6.754078978114156584, 1512.913060387330006, 184.4732361498326156 ) ) ;
#39113 = EDGE_CURVE ( 'NONE', #36273, #104141, #54602, .T. ) ;
#39114 = CARTESIAN_POINT ( 'NONE',  ( 1.771001175045461284, 1526.211523310372513, 177.6852190580647459 ) ) ;
#39115 = CARTESIAN_POINT ( 'NONE',  ( 3.347801439296141712, 1523.382868172864164, 242.0893193391992497 ) ) ;
#39116 = CARTESIAN_POINT ( 'NONE',  ( 13.31407495111609940, 1409.377998129700018, 202.3408434151739925 ) ) ;
#39117 = CARTESIAN_POINT ( 'NONE',  ( 18.80463393750000023, 1425.801073282529842, 225.6039001781980176 ) ) ;
#39118 = CARTESIAN_POINT ( 'NONE',  ( -109.0556933945980091, 1385.242281295139946, 297.1439643352929920 ) ) ;
#39119 = CARTESIAN_POINT ( 'NONE',  ( -18.52955747089999861, 1440.801523186710028, 192.1682810942980097 ) ) ;
#39120 = CARTESIAN_POINT ( 'NONE',  ( 11.86550948949999906, 1432.301448183290177, 150.3971867778979856 ) ) ;
#39121 = AXIS2_PLACEMENT_3D ( 'NONE', #82591, #15358, #22637 ) ;
#39122 = CARTESIAN_POINT ( 'NONE',  ( -4.038223998531310421, 1450.278802180569983, 185.0006718053259647 ) ) ;
#39123 = ORIENTED_EDGE ( 'NONE', *, *, #3501, .T. ) ;
#39124 = ORIENTED_EDGE ( 'NONE', *, *, #60421, .T. ) ;
#39126 = EDGE_CURVE ( 'NONE', #73912, #8321, #94617, .T. ) ;
#39125 = CARTESIAN_POINT ( 'NONE',  ( 13.74310390781900004, 1522.051704408389924, 217.0905615615409943 ) ) ;
#39127 = CARTESIAN_POINT ( 'NONE',  ( -2.499989269620250809, 1419.524750234567819, 137.1000002976804808 ) ) ;
#39128 = CARTESIAN_POINT ( 'NONE',  ( -11.96704581050000016, 1433.884959444120113, 150.6597764172979907 ) ) ;
#39129 = CARTESIAN_POINT ( 'NONE',  ( 29.75012120190000076, 1509.993914123429931, 209.6841247587719863 ) ) ;
#39130 = CARTESIAN_POINT ( 'NONE',  ( -20.02005738860690087, 1489.080029727439978, 190.9336551125319943 ) ) ;
#39131 = CARTESIAN_POINT ( 'NONE',  ( -15.86088303929999910, 1419.980596273840092, 210.7344905958990182 ) ) ;
#39132 = CARTESIAN_POINT ( 'NONE',  ( -108.9389063659999977, 1385.729741725900112, 311.1830050262590248 ) ) ;
#39133 = ADVANCED_FACE ( 'NONE', ( #76523 ), #83274, .T. ) ;
#39134 = CARTESIAN_POINT ( 'NONE',  ( -7.444284933535620041, 1510.876154134890157, 215.3695507499089956 ) ) ;
#39135 = CARTESIAN_POINT ( 'NONE',  ( -9.516636888325759713, 1366.309137899864027, 210.6218459616991936 ) ) ;
#39136 = CARTESIAN_POINT ( 'NONE',  ( 13.55421397129999939, 1497.816254223590022, 226.3870761728989862 ) ) ;
#39137 = CARTESIAN_POINT ( 'NONE',  ( -18.64672481365220236, 1416.851343896850040, 208.5597484336410048 ) ) ;
#39138 = EDGE_CURVE ( 'NONE', #89175, #97581, #52947, .T. ) ;
#39139 = B_SPLINE_CURVE_WITH_KNOTS ( 'NONE', 5,
 ( #70913, #23210, #74202, #106670, #13142, #38361, #99358, #4761, #29959, #107781, #100479, #47326, #66360, #22632, #47877, #64707, #57948, #56281, #14260, #81456, #23761 ),
 .UNSPECIFIED., .F., .F.,
 ( 6, 3, 3, 3, 3, 3, 6 ),
 ( 122.5631238770533997, 122.5666549750004037, 128.3589772970003082, 134.1528038510001863, 139.9378092970001148, 146.0761118390000206, 146.2079031070000212 ),
 .UNSPECIFIED. ) ;
#39140 = CARTESIAN_POINT ( 'NONE',  ( 5.772978278544999675, 1516.659138130710289, 207.9900491214870044 ) ) ;
#39141 = DIRECTION ( 'NONE',  ( 0.000000000000000000, 0.000000000000000000, 1.000000000000000000 ) ) ;
#39142 = CARTESIAN_POINT ( 'NONE',  ( 2.590873905056420234, 1407.641759256400064, 222.0240870714810058 ) ) ;
#39143 = CIRCLE ( 'NONE', #101718, 1.000000000000000000 ) ;
#39144 = CARTESIAN_POINT ( 'NONE',  ( -13.84691416458350055, 1435.860713939990092, 150.1842040648199941 ) ) ;
#39145 = CARTESIAN_POINT ( 'NONE',  ( -7.776723803980000405, 1385.308312221739925, 218.8990009525190317 ) ) ;
#39146 = CARTESIAN_POINT ( 'NONE',  ( 6.840648518365643582, 1425.417253097355342, 226.3025326348858073 ) ) ;
#39147 = CARTESIAN_POINT ( 'NONE',  ( 7.085131439273410159, 1424.907808281010148, 213.0594611446600197 ) ) ;
#39148 = AXIS2_PLACEMENT_3D ( 'NONE', #17131, #78742, #36190 ) ;
#39149 = ADVANCED_FACE ( 'NONE', ( #6572 ), #55312, .F. ) ;
#39150 = ORIENTED_EDGE ( 'NONE', *, *, #92875, .T. ) ;
#39151 = AXIS2_PLACEMENT_3D ( 'NONE', #40867, #47627, #21832 ) ;
#39152 = CARTESIAN_POINT ( 'NONE',  ( 27.24390624950000372, 1427.221042094929999, 244.3119003951980233 ) ) ;
#39153 = CARTESIAN_POINT ( 'NONE',  ( -3.709420335830000415, 1414.325355622289862, 206.4743713944289709 ) ) ;
#39155 = CARTESIAN_POINT ( 'NONE',  ( -1.045121690502980094, 1507.562507687170182, 232.0280612577400063 ) ) ;
#39154 = CARTESIAN_POINT ( 'NONE',  ( -11.97564940980980097, 1491.173717386239787, 206.6759772995580136 ) ) ;
#39156 = CARTESIAN_POINT ( 'NONE',  ( 21.76163503289691903, 1506.366982240506104, 206.1367291981587186 ) ) ;
#39157 = CARTESIAN_POINT ( 'NONE',  ( -29.14244551250000015, 1435.145987499609873, 238.0755264353980181 ) ) ;
#39158 = CARTESIAN_POINT ( 'NONE',  ( -1.840591215909999967, 1487.831606858690066, 219.8181691253990095 ) ) ;
#39159 = CARTESIAN_POINT ( 'NONE',  ( -0.4878038053971470167, 1452.896025903080044, 152.5254486361209842 ) ) ;
#39160 = CARTESIAN_POINT ( 'NONE',  ( 28.26596675839999762, 1451.065831357529987, 136.3389790085980167 ) ) ;
#39161 = ORIENTED_EDGE ( 'NONE', *, *, #79640, .T. ) ;
#39162 = CARTESIAN_POINT ( 'NONE',  ( 11.07444841881259912, 1415.954755716080172, 222.2791099274719784 ) ) ;
#39163 = CARTESIAN_POINT ( 'NONE',  ( -24.41186848580399982, 1440.913060429360030, 212.0284777848129920 ) ) ;
#39164 = CARTESIAN_POINT ( 'NONE',  ( 8.917823571280001360, 1509.304539168530027, 237.8784254626980044 ) ) ;
#39165 = EDGE_LOOP ( 'NONE', ( #54504, #99069, #52384, #62998 ) ) ;
#39166 = ORIENTED_EDGE ( 'NONE', *, *, #96051, .T. ) ;
#39167 = CARTESIAN_POINT ( 'NONE',  ( -10.23170511530682525, 1422.701956246408599, 137.1234386916033827 ) ) ;
#39168 = CARTESIAN_POINT ( 'NONE',  ( -23.92933769846699832, 1410.421755315850078, 208.7355662265979959 ) ) ;
#39169 = ORIENTED_EDGE ( 'NONE', *, *, #63840, .F. ) ;
#39170 = CARTESIAN_POINT ( 'NONE',  ( 3.801734722905379726, 1509.034524749680031, 204.6344874870430317 ) ) ;
#39171 = AXIS2_PLACEMENT_3D ( 'NONE', #22213, #5441, #90540 ) ;
#39172 = CARTESIAN_POINT ( 'NONE',  ( -1.906500024517750053E-08, 1508.551704408389924, 202.1089243866269953 ) ) ;
#39173 = CARTESIAN_POINT ( 'NONE',  ( -4.395186754550000074, 1489.059423926730005, 235.6527567464979995 ) ) ;
#39174 = EDGE_CURVE ( 'NONE', #35107, #47910, #18931, .T. ) ;
#39175 = CARTESIAN_POINT ( 'NONE',  ( 2.531901238200000126, 1444.224916984790070, 200.5256934874690273 ) ) ;
#39176 = ORIENTED_EDGE ( 'NONE', *, *, #78940, .F. ) ;
#39177 = CARTESIAN_POINT ( 'NONE',  ( 45.67158849016559685, 1441.839016858149989, 266.1883947468940050 ) ) ;
#39178 = CARTESIAN_POINT ( 'NONE',  ( -11.70695556590979969, 1414.913057860449953, 220.6083897370939724 ) ) ;
#39179 = EDGE_CURVE ( 'NONE', #36663, #42670, #53195, .T. ) ;
#39180 = CARTESIAN_POINT ( 'NONE',  ( -0.1035703829190000036, 1420.452886222830102, 182.7051921315980110 ) ) ;
#39181 = CARTESIAN_POINT ( 'NONE',  ( 2.480813884984999884, 1517.051603658920158, 204.1089070683270279 ) ) ;
#39182 = EDGE_LOOP ( 'NONE', ( #63984, #33107, #75082, #92151, #25954 ) ) ;
#39183 = CARTESIAN_POINT ( 'NONE',  ( 10.23003872437689843, 1481.533373258429947, 215.0139943380300167 ) ) ;
#39184 = CARTESIAN_POINT ( 'NONE',  ( 12.64536475901971890, 1442.792007884521581, 186.5960024392706487 ) ) ;
#39185 = EDGE_LOOP ( 'NONE', ( #78034, #44025, #52083, #107847, #76796 ) ) ;
#39186 = ORIENTED_EDGE ( 'NONE', *, *, #91388, .T. ) ;
#39187 = CARTESIAN_POINT ( 'NONE',  ( 0.4151546846821905778, 1522.382868172863937, 173.3106345060153046 ) ) ;
#39188 = CARTESIAN_POINT ( 'NONE',  ( 4.487249753806469954, 1509.038615938009798, 205.6342535008409982 ) ) ;
#39189 = CARTESIAN_POINT ( 'NONE',  ( 0.4863421998530879642, 1418.702335047680208, 184.7127968358159933 ) ) ;
#39190 = CARTESIAN_POINT ( 'NONE',  ( -12.18971938666500066, 1512.123542805230272, 194.3960765485670095 ) ) ;
#39191 = CARTESIAN_POINT ( 'NONE',  ( 8.160491664018758584, 1452.628089738999961, 151.2681714364080108 ) ) ;
#39192 = CARTESIAN_POINT ( 'NONE',  ( 11.29246402500000102, 1420.389623373509721, 198.6444918639989794 ) ) ;
#39193 = CARTESIAN_POINT ( 'NONE',  ( 6.141424742704666428, 1511.655929346004314, 217.9160887146131245 ) ) ;
#39194 = CARTESIAN_POINT ( 'NONE',  ( -108.6053824472246561, 1381.341894323206361, 297.9344204043421769 ) ) ;
#39195 = DIRECTION ( 'NONE',  ( 5.980589973904019347E-17, -1.000000000000000000, 1.736889445713099699E-16 ) ) ;
#39196 = CARTESIAN_POINT ( 'NONE',  ( 0.01602020491292198423, 1408.960543678336762, 232.1618151973992497 ) ) ;
#39198 = CARTESIAN_POINT ( 'NONE',  ( -106.7386023904570038, 1391.793764057960061, 307.5809146916449777 ) ) ;
#39197 = CARTESIAN_POINT ( 'NONE',  ( -13.54609157666829944, 1434.953585316950011, 148.7557093113670135 ) ) ;
#39199 = CARTESIAN_POINT ( 'NONE',  ( 10.74318624240480169, 1423.607808323160043, 206.7556458220460058 ) ) ;
#39200 = ADVANCED_FACE ( 'NONE', ( #54670 ), #76879, .F. ) ;
#39201 = CARTESIAN_POINT ( 'NONE',  ( -24.83471925681290315, 1509.481687055530074, 222.6988703109550158 ) ) ;
#39202 = CARTESIAN_POINT ( 'NONE',  ( -7.649034438594999763, 1514.243099272629934, 203.4721261815869866 ) ) ;
#39203 = VERTEX_POINT ( 'NONE', #92640 ) ;
#39204 = CARTESIAN_POINT ( 'NONE',  ( 11.40468314536590100, 1414.972329067380088, 222.2791104303979921 ) ) ;
#39205 = AXIS2_PLACEMENT_3D ( 'NONE', #44325, #35356, #70102 ) ;
#39206 = CARTESIAN_POINT ( 'NONE',  ( -16.85557438000711272, 1417.264140369140478, 207.1097720217920255 ) ) ;
#39207 = CARTESIAN_POINT ( 'NONE',  ( -95.82886112073660456, 1384.956069587409957, 310.2164913438589906 ) ) ;
#39208 = B_SPLINE_SURFACE_WITH_KNOTS ( 'NONE', 5, 3, ( 
 ( #50328, #67124, #76058, #110201 ),
 ( #32934, #24523, #110756, #49217 ),
 ( #101224, #83343, #108551, #31841 ),
 ( #74973, #15019, #58712, #50858 ),
 ( #92845, #33475, #57627, #49765 ),
 ( #74424, #83896, #66026, #67677 ) ),
 .UNSPECIFIED., .F., .F., .F.,
 ( 6, 6 ),
 ( 4, 4 ),
 ( 0.000000000000000000, 11.48858425020000062 ),
 ( 37.69911184309999896, 40.20365518519999881 ),
 .UNSPECIFIED. ) ;
#39209 = CARTESIAN_POINT ( 'NONE',  ( -10.60441893339999986, 1387.604333835939997, 201.2306567222790363 ) ) ;
#39210 = CARTESIAN_POINT ( 'NONE',  ( 9.058157503864009641, 1423.689293625850041, 210.6374908749079964 ) ) ;
#39212 = ORIENTED_EDGE ( 'NONE', *, *, #48928, .T. ) ;
#39211 = CARTESIAN_POINT ( 'NONE',  ( -16.14864212301420210, 1419.744746607639854, 210.0472711449799874 ) ) ;
#39213 = CARTESIAN_POINT ( 'NONE',  ( 4.329898783340000001, 1430.328825655489936, 217.5774781053490017 ) ) ;
#39214 = CARTESIAN_POINT ( 'NONE',  ( -2.455820327400000114, 1434.541746329560056, 150.3615916412979914 ) ) ;
#39215 = TOROIDAL_SURFACE ( 'NONE', #21375, 30.13701971169416538, 3.000000000000000000 ) ;
#39216 = ADVANCED_FACE ( 'NONE', ( #40038, #41139 ), #42251, .T. ) ;
#39217 = CARTESIAN_POINT ( 'NONE',  ( -14.00898869779999956, 1416.833018181429907, 221.8520907042980070 ) ) ;
#39218 = CARTESIAN_POINT ( 'NONE',  ( 11.70028423970000020, 1433.720629087699990, 151.0079596410979832 ) ) ;
#39219 = CARTESIAN_POINT ( 'NONE',  ( 15.05391205133499888, 1514.225267046429963, 225.1144834937670112 ) ) ;
#39220 = CARTESIAN_POINT ( 'NONE',  ( 13.01671764799699993, 1416.842625005220043, 196.3343525426479914 ) ) ;
#39221 = B_SPLINE_CURVE_WITH_KNOTS ( 'NONE', 5,
 ( #38736, #63980, #12977, #20279, #98642, #21364, #89696, #55572, #47160 ),
 .UNSPECIFIED., .F., .F.,
 ( 6, 3, 6 ),
 ( 0.7655572723410000169, 2.316155491860000026, 3.835724788519999429 ),
 .UNSPECIFIED. ) ;
#39222 = EDGE_CURVE ( 'NONE', #56035, #20284, #74371, .T. ) ;
#39223 = CARTESIAN_POINT ( 'NONE',  ( 2.921915679247010011, 1414.085076703340064, 231.7960692163919703 ) ) ;
#39224 = CARTESIAN_POINT ( 'NONE',  ( -12.86224528119999988, 1519.913060387329779, 228.0025448475979886 ) ) ;
#39225 = CARTESIAN_POINT ( 'NONE',  ( 16.45032630069999868, 1417.430338871630056, 226.9554082569979983 ) ) ;
#39226 = CARTESIAN_POINT ( 'NONE',  ( -22.03465957473791192, 1522.644714754857205, 235.4136513321467987 ) ) ;
#39227 = CARTESIAN_POINT ( 'NONE',  ( 19.53786426059039982, 1501.977400791986611, 236.7197124308265188 ) ) ;
#39228 = CARTESIAN_POINT ( 'NONE',  ( -19.07843485409999928, 1410.941104706429996, 222.8264070888980086 ) ) ;
#39229 = FACE_OUTER_BOUND ( 'NONE', #99203, .T. ) ;
#39230 = TOROIDAL_SURFACE ( 'NONE', #24905, 6.868727599660000571, 1.000000000000000000 ) ;
#39231 = CARTESIAN_POINT ( 'NONE',  ( 19.79807428129999991, 1508.018205000529861, 188.8464914106980075 ) ) ;
#39232 = CARTESIAN_POINT ( 'NONE',  ( -25.24617298109999908, 1450.838013018590118, 137.6080363986979762 ) ) ;
#39233 = CARTESIAN_POINT ( 'NONE',  ( 20.87481493262672672, 1525.712830164893376, 184.1764553469176633 ) ) ;
#39234 = CARTESIAN_POINT ( 'NONE',  ( -0.7050289745649990225, 1515.139588934790027, 204.7943557892189972 ) ) ;
#39235 = CARTESIAN_POINT ( 'NONE',  ( -14.20525283303160080, 1416.384016890880048, 203.1489016136929706 ) ) ;
#39236 = EDGE_CURVE ( 'NONE', #61659, #34791, #27791, .T. ) ;
#39237 =( BOUNDED_SURFACE ( )  B_SPLINE_SURFACE ( 3, 2, ( 
 ( #61203, #76309, #51667 ),
 ( #52229, #16912, #9102 ),
 ( #69039, #67931, #69595 ),
 ( #109910, #33191, #101479 ),
 ( #24766, #93096, #16368 ),
 ( #25325, #50566, #84692 ),
 ( #87481, #53906, #44941 ),
 ( #29216, #35968, #3486 ),
 ( #27558, #105938, #71817 ),
 ( #2941, #79638, #52774 ),
 ( #37615, #89115, #63406 ),
 ( #70159, #10203, #1834 ),
 ( #11325, #45497, #11866 ),
 ( #88041, #86912, #37061 ) ),
 .UNSPECIFIED., .F., .F., .F. ) 
 B_SPLINE_SURFACE_WITH_KNOTS ( ( 4, 2, 2, 2, 2, 2, 4 ),
 ( 3, 3 ),
 ( 0.000000000000000000, 0.0009440840677145004387, 0.001416126101571750767, 0.001888168135429000877, 0.002360210169286251422, 0.002832252203143501533, 0.003776336270858001755 ),
 ( 0.000000000000000000, 1.000000000000000000 ),
 .UNSPECIFIED. ) 
 GEOMETRIC_REPRESENTATION_ITEM ( )  RATIONAL_B_SPLINE_SURFACE ( (
 ( 1.000000000000000000, 0.8070209408750090851, 1.000000000000000000),
 ( 1.000000000000000000, 0.8215603905292898634, 1.000000000000000000),
 ( 1.000000000000000000, 0.8340988699049266542, 1.000000000000000000),
 ( 1.000000000000000000, 0.8516751610464631250, 1.000000000000000000),
 ( 1.000000000000000000, 0.8573697395152763967, 1.000000000000000000),
 ( 1.000000000000000000, 0.8683586635663552711, 1.000000000000000000),
 ( 1.000000000000000000, 0.8736518481708266393, 1.000000000000000000),
 ( 1.000000000000000000, 0.8840377753030468355, 1.000000000000000000),
 ( 1.000000000000000000, 0.8891294171307794203, 1.000000000000000000),
 ( 1.000000000000000000, 0.8992456600573223158, 1.000000000000000000),
 ( 1.000000000000000000, 0.9042785869249978514, 1.000000000000000000),
 ( 1.000000000000000000, 0.9189749222844358911, 1.000000000000000000),
 ( 1.000000000000000000, 0.9283978182344505559, 1.000000000000000000),
 ( 1.000000000000000000, 0.9376006582765954445, 1.000000000000000000) ) ) 
 REPRESENTATION_ITEM ( '' )  SURFACE ( )  );
#39238 = CARTESIAN_POINT ( 'NONE',  ( 18.38166058516359769, 1428.164368163260178, 201.4944004331299823 ) ) ;
#39239 = CARTESIAN_POINT ( 'NONE',  ( -9.435157404909999102, 1414.913060387329779, 222.1292708042979882 ) ) ;
#39240 = CARTESIAN_POINT ( 'NONE',  ( 0.2100116478871839887, 1457.341752983120159, 183.0671337708849933 ) ) ;
#39241 = CARTESIAN_POINT ( 'NONE',  ( -14.17767550720000003, 1409.408155725629967, 203.0979980328280021 ) ) ;
#39242 = CARTESIAN_POINT ( 'NONE',  ( 9.070710170037548536, 1428.247707153859892, 212.8796129129519841 ) ) ;
#39243 = CARTESIAN_POINT ( 'NONE',  ( 18.00465857451045792, 1523.390106123591067, 180.2140906788903862 ) ) ;
#39244 = EDGE_CURVE ( 'NONE', #77737, #70841, #47825, .T. ) ;
#39245 = CARTESIAN_POINT ( 'NONE',  ( -8.178500771994089646, 1441.152429774469965, 153.9860759686779943 ) ) ;
#39246 = CARTESIAN_POINT ( 'NONE',  ( 12.40410385870000098, 1434.420076928460048, 149.1896426101980069 ) ) ;
#39247 = DIRECTION ( 'NONE',  ( -2.473221764039894783E-17, 0.000000000000000000, -1.000000000000000000 ) ) ;
#39248 = CARTESIAN_POINT ( 'NONE',  ( -2.847678236428970333, 1430.845636561999981, 201.2564352187889938 ) ) ;
#39249 = ORIENTED_EDGE ( 'NONE', *, *, #35506, .F. ) ;
#39250 = CARTESIAN_POINT ( 'NONE',  ( -17.10337015679643713, 1524.478200376951008, 180.9725626400690146 ) ) ;
#39251 = CARTESIAN_POINT ( 'NONE',  ( 6.105460688195506691, 1510.769285161600010, 216.6036268165167940 ) ) ;
#39252 = CARTESIAN_POINT ( 'NONE',  ( -103.9670040342639794, 1380.172649198307454, 306.3874380259700274 ) ) ;
#39253 = CARTESIAN_POINT ( 'NONE',  ( -12.07906408490000061, 1491.053577648989858, 206.9546736298989913 ) ) ;
#39255 = EDGE_CURVE ( 'NONE', #101013, #105289, #95848, .T. ) ;
#39254 = CARTESIAN_POINT ( 'NONE',  ( -0.5038386193489999831, 1452.963758663529916, 183.2902632327979973 ) ) ;
#39256 = CARTESIAN_POINT ( 'NONE',  ( 0.1681681984989999989, 1420.016189442530049, 171.1670476502980023 ) ) ;
#39257 = CARTESIAN_POINT ( 'NONE',  ( 44.74173090250090468, 1434.085289301948251, 268.9999157369318823 ) ) ;
#39258 = CIRCLE ( 'NONE', #85690, 1.999999999999999556 ) ;
#39259 = CARTESIAN_POINT ( 'NONE',  ( -19.73881298686153229, 1499.102984487484946, 189.2247233355559501 ) ) ;
#39260 = CARTESIAN_POINT ( 'NONE',  ( -12.50373372780000025, 1379.339414555010080, 210.6530944808689867 ) ) ;
#39261 = CARTESIAN_POINT ( 'NONE',  ( -108.2169316518169921, 1384.585047728120117, 311.2483635071519643 ) ) ;
#39262 = CARTESIAN_POINT ( 'NONE',  ( -55.20995173741290074, 1385.039367042840013, 234.2426462848850122 ) ) ;
#39263 = CARTESIAN_POINT ( 'NONE',  ( -12.09091630672140028, 1491.024750413429956, 207.0451805009280122 ) ) ;
#39264 = CARTESIAN_POINT ( 'NONE',  ( -4.174206985259830027, 1508.551704408389924, 204.7881409777949955 ) ) ;
#39265 = CARTESIAN_POINT ( 'NONE',  ( -27.03405988099999746, 1451.512678451430020, 136.1495578053979614 ) ) ;
#39266 = EDGE_CURVE ( 'NONE', #55879, #109101, #10552, .T. ) ;
#39267 = ADVANCED_FACE ( 'NONE', ( #69695 ), #84702, .F. ) ;
#39268 = CARTESIAN_POINT ( 'NONE',  ( 1.439851189671143228, 1526.382868172864164, 178.7402778767489906 ) ) ;
#39269 = CARTESIAN_POINT ( 'NONE',  ( -16.33510206972449907, 1410.578254075250015, 226.6050706015539902 ) ) ;
#39271 = ORIENTED_EDGE ( 'NONE', *, *, #51179, .F. ) ;
#39270 = CARTESIAN_POINT ( 'NONE',  ( 0.5133626083067620582, 1410.311097044259895, 185.0719925509139898 ) ) ;
#39272 = CARTESIAN_POINT ( 'NONE',  ( -12.00508716839999934, 1508.989785511929995, 182.7232473457980007 ) ) ;
#39273 = CARTESIAN_POINT ( 'NONE',  ( 9.623281588457949454, 1470.012648596069994, 212.1148972040010108 ) ) ;
#39274 = DIRECTION ( 'NONE',  ( 0.01802056537744943510, 0.000000000000000000, -0.9998376164275263323 ) ) ;
#39275 = CARTESIAN_POINT ( 'NONE',  ( -109.4870104200000043, 1384.778285814570154, 311.2819397492589815 ) ) ;
#39276 = CARTESIAN_POINT ( 'NONE',  ( -0.1980063625633159963, 1419.359867767670039, 184.4979803712249975 ) ) ;
#39277 = CARTESIAN_POINT ( 'NONE',  ( -2.265100829110000102, 1421.884435632049872, 193.4623859336989824 ) ) ;
#39278 = CIRCLE ( 'NONE', #76855, 1.000000000000000888 ) ;
#39279 = CARTESIAN_POINT ( 'NONE',  ( 19.54316991260000336, 1410.091339499530022, 220.4324682491979956 ) ) ;
#39280 = CARTESIAN_POINT ( 'NONE',  ( -1.804128457859720092, 1410.345740199939883, 186.0509510551849814 ) ) ;
#39281 = CARTESIAN_POINT ( 'NONE',  ( -18.30458809710689749, 1465.267267787470018, 217.6413456689680004 ) ) ;
#39282 = CARTESIAN_POINT ( 'NONE',  ( -18.14246331760000075, 1424.695492789029913, 227.8876255367979979 ) ) ;
#39284 = CARTESIAN_POINT ( 'NONE',  ( 16.63178568020000014, 1409.493855139530069, 223.7919630844980077 ) ) ;
#39283 = CARTESIAN_POINT ( 'NONE',  ( -4.487172950141123273, 1511.405761256467713, 200.7686181660011471 ) ) ;
#39285 = CARTESIAN_POINT ( 'NONE',  ( 19.60792669039999936, 1475.100271358290229, 204.3343059087790152 ) ) ;
#39286 = CARTESIAN_POINT ( 'NONE',  ( -118.8461440515266929, 1348.229899472570651, 301.2466039018671609 ) ) ;
#39287 = CARTESIAN_POINT ( 'NONE',  ( 0.000000000000000000, 1522.051704408389924, 209.1218459616979999 ) ) ;
#39288 = EDGE_CURVE ( 'NONE', #18748, #97154, #90651, .T. ) ;
#39289 = CARTESIAN_POINT ( 'NONE',  ( -14.55659802589999963, 1503.856184377289992, 208.7749621606049857 ) ) ;
#39290 = CARTESIAN_POINT ( 'NONE',  ( 7.818221670729999850, 1367.736483592530021, 210.6218459616991936 ) ) ;
#39291 = CARTESIAN_POINT ( 'NONE',  ( -7.335901033725000353, 1517.068717944079935, 205.0869373723870126 ) ) ;
#39292 = CARTESIAN_POINT ( 'NONE',  ( -11.57752524527410110, 1486.021447801480008, 184.4692410163380032 ) ) ;
#39293 = ORIENTED_EDGE ( 'NONE', *, *, #65928, .F. ) ;
#39294 = ADVANCED_FACE ( 'NONE', ( #98712 ), #63505, .T. ) ;
#39295 = CARTESIAN_POINT ( 'NONE',  ( -8765.422060425717063, 5182.767774292095964, 3175.242030490383513 ) ) ;
#39296 = CARTESIAN_POINT ( 'NONE',  ( -4.234119969708030951, 1441.492840331990010, 163.8906307119239898 ) ) ;
#39298 = EDGE_LOOP ( 'NONE', ( #22862, #89108, #6361, #53623 ) ) ;
#39297 = CARTESIAN_POINT ( 'NONE',  ( -68.30538991723700804, 1379.747268421340095, 279.8418067756310279 ) ) ;
#39299 = ORIENTED_EDGE ( 'NONE', *, *, #50184, .T. ) ;
#39300 = CARTESIAN_POINT ( 'NONE',  ( 28.70345850190000192, 1509.590240593130147, 210.2487084362280143 ) ) ;
#39301 = ORIENTED_EDGE ( 'NONE', *, *, #105536, .F. ) ;
#39302 = CARTESIAN_POINT ( 'NONE',  ( -3.558358604862239982, 1455.955982659530036, 200.3550966546550001 ) ) ;
#39303 = DIRECTION ( 'NONE',  ( 0.000000000000000000, 0.000000000000000000, -1.000000000000000000 ) ) ;
#39305 = CARTESIAN_POINT ( 'NONE',  ( 1.152385366779999920, 1508.177879779530031, 180.8347444588980011 ) ) ;
#39304 = CARTESIAN_POINT ( 'NONE',  ( -11.39350426579230025, 1425.508008078089915, 141.1901541546949943 ) ) ;
#39306 = CARTESIAN_POINT ( 'NONE',  ( -3.447128498755000159, 1516.778853242349896, 210.2570310142770040 ) ) ;
#39307 = AXIS2_PLACEMENT_3D ( 'NONE', #96621, #21529, #90398 ) ;
#39309 = B_SPLINE_CURVE_WITH_KNOTS ( 'NONE', 5,
 ( #36875, #86178, #10582, #95687, #69408, #36321 ),
 .UNSPECIFIED., .F., .F.,
 ( 6, 6 ),
 ( 0.000000000000000000, 1.000000000000000000 ),
 .UNSPECIFIED. ) ;
#39308 = CARTESIAN_POINT ( 'NONE',  ( -24.14079447473799789, 1452.054257227049902, 136.9211370085970145 ) ) ;
#39310 = CARTESIAN_POINT ( 'NONE',  ( -11.73645620750000163, 1426.280382981230105, 144.1655706660979774 ) ) ;
#39311 = CARTESIAN_POINT ( 'NONE',  ( -14.53473304376390018, 1379.710786975620067, 208.2794084638009906 ) ) ;
#39312 = CARTESIAN_POINT ( 'NONE',  ( 10.43358895521959973, 1481.587437876299873, 210.8843897139930164 ) ) ;
#39313 = APPLICATION_PROTOCOL_DEFINITION ( 'draft international standard', 'automotive_design', 1998, #20555 ) ;
#39314 = PRODUCT ( 'Handle Grip', 'Handle Grip', '', ( #73484 ) ) ;
#39315 = CARTESIAN_POINT ( 'NONE',  ( 36.53452253882689860, 1451.194196174300032, 134.0999999986999853 ) ) ;
#39316 = CARTESIAN_POINT ( 'NONE',  ( -40.26434707082469799, 1443.230809785309930, 137.0716638627269788 ) ) ;
#39317 = CARTESIAN_POINT ( 'NONE',  ( 13.95068308120620060, 1435.004429209999898, 148.7713137966129864 ) ) ;
#39318 = AXIS2_PLACEMENT_3D ( 'NONE', #104448, #96047, #54086 ) ;
#39319 = CARTESIAN_POINT ( 'NONE',  ( -16.73628186595804479, 1526.382868172863937, 234.1845039693045862 ) ) ;
#39320 = ORIENTED_EDGE ( 'NONE', *, *, #18926, .T. ) ;
#39321 = EDGE_LOOP ( 'NONE', ( #72411, #67173, #97037, #103076, #90432, #65110 ) ) ;
#39322 = CARTESIAN_POINT ( 'NONE',  ( -5.649719788644999241, 1514.243099272629934, 216.7708803706970002 ) ) ;
#39323 = CARTESIAN_POINT ( 'NONE',  ( 16.68633773671889742, 1513.912053497473607, 195.2582997944726060 ) ) ;
#39324 = CARTESIAN_POINT ( 'NONE',  ( 0.09653062418259999999, 1451.692067920030013, 183.0365772874980053 ) ) ;
#39325 = CARTESIAN_POINT ( 'NONE',  ( -20.36287103150000277, 1507.711394158289977, 209.4617748114379765 ) ) ;
#39326 = CARTESIAN_POINT ( 'NONE',  ( -2.864888263985923444, 1368.214942817532346, 207.6218459616988241 ) ) ;
#39327 = AXIS2_PLACEMENT_3D ( 'NONE', #81679, #108554, #31844 ) ;
#39328 = CARTESIAN_POINT ( 'NONE',  ( -26.35475552313950232, 1507.985742420310089, 201.5462045797129917 ) ) ;
#39329 = CARTESIAN_POINT ( 'NONE',  ( 5.551188673975000043, 1510.480349266450048, 216.6723492941569873 ) ) ;
#39330 = CARTESIAN_POINT ( 'NONE',  ( -9277.788495362316098, 2833.746317950420689, 5939.014819763676314 ) ) ;
#39331 = CARTESIAN_POINT ( 'NONE',  ( -10613.67162176269994, 54.28084076250828360, 5061.882847083795241 ) ) ;
#39332 = CARTESIAN_POINT ( 'NONE',  ( 11.80290349340000056, 1415.088016306429836, 196.9360299734980231 ) ) ;
#39333 = CARTESIAN_POINT ( 'NONE',  ( -67.88352385773819719, 1384.723690489739965, 261.4186645314100588 ) ) ;
#39334 = ORIENTED_EDGE ( 'NONE', *, *, #29653, .F. ) ;
#39335 = CARTESIAN_POINT ( 'NONE',  ( 4.487358949475809489, 1509.034510030706997, 205.3201214368218359 ) ) ;
#39336 = CARTESIAN_POINT ( 'NONE',  ( 7.323390407215000231, 1516.613712827999962, 207.9924597298270044 ) ) ;
#39337 = ORIENTED_EDGE ( 'NONE', *, *, #88581, .T. ) ;
#39338 = DIRECTION ( 'NONE',  ( 0.000000000000000000, 1.000000000000000000, 0.000000000000000000 ) ) ;
#39339 = CARTESIAN_POINT ( 'NONE',  ( 19.65890388680000100, 1477.381973150129852, 226.7576334579979971 ) ) ;
#39340 = ORIENTED_EDGE ( 'NONE', *, *, #72907, .F. ) ;
#39341 = CARTESIAN_POINT ( 'NONE',  ( -17.78793056501397984, 1523.919943579690425, 180.4102122295458059 ) ) ;
#39342 = CARTESIAN_POINT ( 'NONE',  ( -16.31589243200000183, 1410.414964140629991, 191.5459822045979763 ) ) ;
#39343 = CARTESIAN_POINT ( 'NONE',  ( -18.05280916457315143, 1508.456971748121987, 211.8086596262961621 ) ) ;
#39344 = LINE ( 'NONE', #66778, #100775 ) ;
#39345 = CARTESIAN_POINT ( 'NONE',  ( -7.465741425504200279, 1435.823992893209834, 215.3776685733120075 ) ) ;
#39346 = CARTESIAN_POINT ( 'NONE',  ( -5.395039083132619595, 1511.384172056590160, 200.9623232297749666 ) ) ;
#39347 = CARTESIAN_POINT ( 'NONE',  ( -2.158139092959999950, 1508.640225114429995, 180.2987574298980178 ) ) ;
#39348 = CARTESIAN_POINT ( 'NONE',  ( -13.19883015649999969, 1434.900409594529947, 147.8554851810979756 ) ) ;
#39349 = CARTESIAN_POINT ( 'NONE',  ( -7.734617125744999377, 1513.613303996360173, 216.9435780305869912 ) ) ;
#39351 = CARTESIAN_POINT ( 'NONE',  ( -11.60004869885203682, 1423.973206102585664, 135.9381536973014590 ) ) ;
#39350 = CARTESIAN_POINT ( 'NONE',  ( 16.58228743579999787, 1460.774766522529944, 229.0346157100979951 ) ) ;
#39352 = CARTESIAN_POINT ( 'NONE',  ( 6.555273148870000455, 1470.255836705890033, 211.2211195251889819 ) ) ;
#39353 = AXIS2_PLACEMENT_3D ( 'NONE', #33607, #84577, #92416 ) ;
#39354 = B_SPLINE_SURFACE_WITH_KNOTS ( 'NONE', 5, 5, ( 
 ( #97314, #97854, #20583, #12201, #46396, #29021, #105174, #69944, #20051 ),
 ( #106270, #62094, #36859, #87839, #79427, #11127, #87266, #80527, #2738 ),
 ( #37970, #29556, #62658, #63741, #96780, #54245, #88371, #21129, #27351 ),
 ( #11661, #10560, #78309, #45837, #86708, #1624, #35760, #104058, #3288 ),
 ( #61535, #78884, #79970, #95665, #44734, #27912, #2190, #36303, #70499 ),
 ( #104616, #73224, #73789, #90560, #13839, #31209, #23353, #65943, #100067 ) ),
 .UNSPECIFIED., .F., .F., .F.,
 ( 6, 6 ),
 ( 6, 3, 6 ),
 ( 9.202839167560000533, 20.64174078209999763 ),
 ( 0.000000000000000000, 1.000000000000000000, 2.000000000000000000 ),
 .UNSPECIFIED. ) ;
#39355 = CARTESIAN_POINT ( 'NONE',  ( 0.01073129396420149928, 1516.939491476980038, 216.4539099096770087 ) ) ;
#39356 = CARTESIAN_POINT ( 'NONE',  ( -0.08725294298748798028, 1486.463441972811779, 181.7930006954420037 ) ) ;
#39357 = CARTESIAN_POINT ( 'NONE',  ( -10.33191382005590953, 1480.649815741992597, 207.0399858577212910 ) ) ;
#39358 = CARTESIAN_POINT ( 'NONE',  ( 3.163495553606223254, 1467.481610648900414, 218.5739468055329837 ) ) ;
#39359 = CARTESIAN_POINT ( 'NONE',  ( -2.479246885834999858, 1516.983612918759945, 213.1658362778269691 ) ) ;
#39360 = CARTESIAN_POINT ( 'NONE',  ( 18.70459388869999628, 1509.566239198929907, 186.5372755795979742 ) ) ;
#39361 = CARTESIAN_POINT ( 'NONE',  ( -3.631597801648350110, 1483.402419362059845, 199.0973728678349914 ) ) ;
#39363 = ORIENTED_EDGE ( 'NONE', *, *, #102828, .F. ) ;
#39362 = CARTESIAN_POINT ( 'NONE',  ( -11.25664976887165203, 1508.421381615256678, 207.6010284851684276 ) ) ;
#39364 = CARTESIAN_POINT ( 'NONE',  ( -7.966175666139999834, 1384.907333411119907, 199.4893255676990123 ) ) ;
#39365 = TOROIDAL_SURFACE ( 'NONE', #98340, 2.000000000000000000, 1.000000000000000000 ) ;
#39366 = CARTESIAN_POINT ( 'NONE',  ( 2.911802205209999883, 1507.562757914290160, 220.4805861716990023 ) ) ;
#39367 = CARTESIAN_POINT ( 'NONE',  ( -11.29610511779999982, 1431.916778257889973, 151.5105990156980056 ) ) ;
#39368 = CARTESIAN_POINT ( 'NONE',  ( -15.75672504909999816, 1415.912232267690115, 208.9316401283900291 ) ) ;
#39369 = CARTESIAN_POINT ( 'NONE',  ( -6.711227830452440202, 1442.278139609789832, 201.5834457825660024 ) ) ;
#39370 = CARTESIAN_POINT ( 'NONE',  ( 27.01856162345059786, 1451.963899306131680, 135.0861192397252069 ) ) ;
#39371 = CARTESIAN_POINT ( 'NONE',  ( 8.725351515859999907, 1420.892103511989944, 196.4178243839989761 ) ) ;
#39372 = CARTESIAN_POINT ( 'NONE',  ( -9.522388363570000180, 1439.330054399390065, 208.4250942545799887 ) ) ;
#39373 = B_SPLINE_CURVE_WITH_KNOTS ( 'NONE', 3,
 ( #26548, #100619, #59617, #14954 ),
 .UNSPECIFIED., .F., .F.,
 ( 4, 4 ),
 ( 0.000000000000000000, 1.000000000000000000 ),
 .UNSPECIFIED. ) ;
#39375 = CARTESIAN_POINT ( 'NONE',  ( -9.482852257741408053, 1424.109967149583326, 139.1406704986484044 ) ) ;
#39374 = CARTESIAN_POINT ( 'NONE',  ( -21.23607560820000018, 1470.084651651229933, 224.2120819598980006 ) ) ;
#39376 = CARTESIAN_POINT ( 'NONE',  ( -13.48561026711389843, 1379.693410661539929, 211.4566350483709982 ) ) ;
#39377 = ORIENTED_EDGE ( 'NONE', *, *, #82409, .T. ) ;
#39378 = CARTESIAN_POINT ( 'NONE',  ( 4.029572640705000985, 1516.858649670339901, 205.0803734583570019 ) ) ;
#39379 = CARTESIAN_POINT ( 'NONE',  ( 3.757756526780000161, 1406.106055978829772, 266.9554538344980301 ) ) ;
#39380 = CARTESIAN_POINT ( 'NONE',  ( 18.51436573157356946, 1511.187213306747708, 181.1015051776552696 ) ) ;
#39381 = DIRECTION ( 'NONE',  ( 0.000000000000000000, 0.000000000000000000, 1.000000000000000000 ) ) ;
#39382 = CARTESIAN_POINT ( 'NONE',  ( 21.09445956586550608, 1428.283637055626286, 219.6230929203899507 ) ) ;
#39383 = CARTESIAN_POINT ( 'NONE',  ( 0.1095232733706122119, 1463.638598533493223, 199.3170435800446398 ) ) ;
#39384 = CARTESIAN_POINT ( 'NONE',  ( 9.545351305817721510, 1500.533481294277635, 228.7109972438295813 ) ) ;
#39385 = CARTESIAN_POINT ( 'NONE',  ( 11.73709356406289928, 1426.695943121369965, 144.1748013758129900 ) ) ;
#39386 = TOROIDAL_SURFACE ( 'NONE', #59152, 8.000000000000000000, 2.000000000000000000 ) ;
#39387 = CARTESIAN_POINT ( 'NONE',  ( -2.441038202540000146, 1449.508741061479896, 155.6080925163979884 ) ) ;
#39388 = CARTESIAN_POINT ( 'NONE',  ( -11.95968169409999859, 1446.500037956690221, 187.4450202269979968 ) ) ;
#39389 = EDGE_CURVE ( 'NONE', #56949, #62022, #40369, .T. ) ;
#39390 = CARTESIAN_POINT ( 'NONE',  ( -19.88407671807765809, 1485.200176455136216, 190.7915739009804099 ) ) ;
#39391 = CARTESIAN_POINT ( 'NONE',  ( -106.4020496450190052, 1391.913060387289988, 304.2007955189830568 ) ) ;
#39392 = CARTESIAN_POINT ( 'NONE',  ( -4.045201229639999951, 1515.528102034789981, 210.6102411367990328 ) ) ;
#39393 = CIRCLE ( 'NONE', #92, 2.000000000000001776 ) ;
#39394 = CARTESIAN_POINT ( 'NONE',  ( -23.42675388609999843, 1438.250513045190246, 234.3916895488980003 ) ) ;
#39395 = CARTESIAN_POINT ( 'NONE',  ( -1.073240929390329958E-18, 1414.661898229710005, 209.1218459616989946 ) ) ;
#39396 = CARTESIAN_POINT ( 'NONE',  ( -3.246772394788723481, 1511.187213306747708, 177.1492560608742224 ) ) ;
#39397 = CARTESIAN_POINT ( 'NONE',  ( -4.969071879919999546, 1475.566901209930165, 269.0361176487980401 ) ) ;
#39398 = FACE_OUTER_BOUND ( 'NONE', #105044, .T. ) ;
#39399 = CARTESIAN_POINT ( 'NONE',  ( -9.240621257877769779, 1384.939706531919910, 197.9480711716310282 ) ) ;
#39400 = CARTESIAN_POINT ( 'NONE',  ( -8.636908121861750942, 1486.516023803749704, 183.0083597854972766 ) ) ;
#39401 = CARTESIAN_POINT ( 'NONE',  ( -24.10034866325270286, 1384.849111676500115, 223.0989387258899797 ) ) ;
#39402 = CARTESIAN_POINT ( 'NONE',  ( -106.4135441880139865, 1391.913060387269979, 303.8057445950980195 ) ) ;
#39403 = CIRCLE ( 'NONE', #82324, 15.40132948099999943 ) ;
#39404 = CARTESIAN_POINT ( 'NONE',  ( 12.26355851476349912, 1416.702560753930129, 223.5733017519110035 ) ) ;
#39405 = EDGE_CURVE ( 'NONE', #57510, #60349, #68855, .T. ) ;
#39406 = CARTESIAN_POINT ( 'NONE',  ( -105.4748444820000088, 1379.159997331010118, 302.2473400626589637 ) ) ;
#39407 = CARTESIAN_POINT ( 'NONE',  ( 32.54505059146715951, 1524.547395018737916, 217.0833365843165268 ) ) ;
#39408 = CARTESIAN_POINT ( 'NONE',  ( 24.69959627108774924, 1509.552018375699618, 195.6047270735438701 ) ) ;
#39409 = CARTESIAN_POINT ( 'NONE',  ( -17.57263694559999934, 1409.691668941730086, 195.6049344922980140 ) ) ;
#39410 = CARTESIAN_POINT ( 'NONE',  ( -15.81192270634400288, 1421.036774565764063, 227.0412074172699874 ) ) ;
#39411 = CARTESIAN_POINT ( 'NONE',  ( 19.59345072173944757, 1455.474483766830417, 225.8838923643688474 ) ) ;
#39412 = ORIENTED_EDGE ( 'NONE', *, *, #33553, .F. ) ;
#39413 = DIRECTION ( 'NONE',  ( 0.000000000000000000, 0.000000000000000000, -1.000000000000000000 ) ) ;
#39414 = CARTESIAN_POINT ( 'NONE',  ( -7.548036999711751349, 1510.518062821254716, 214.7935333685385615 ) ) ;
#39415 = CARTESIAN_POINT ( 'NONE',  ( -19.86464710129909861, 1441.435714616360201, 212.6459466280339825 ) ) ;
#39417 = CARTESIAN_POINT ( 'NONE',  ( -14.46755554256499998, 1513.509764667529907, 193.9550704101670249 ) ) ;
#39416 = CARTESIAN_POINT ( 'NONE',  ( -15.92986207429999901, 1416.139014782290133, 209.7537124246929920 ) ) ;
#39418 = CARTESIAN_POINT ( 'NONE',  ( 2.564995765565520003, 1366.156374150979900, 209.1218459575829911 ) ) ;
#39419 = CARTESIAN_POINT ( 'NONE',  ( -8.045651973969999204, 1451.834176107089888, 203.9611725415890078 ) ) ;
#39420 = CIRCLE ( 'NONE', #5453, 1.000000000000000888 ) ;
#39421 = CARTESIAN_POINT ( 'NONE',  ( -4.617490504904999682, 1516.685667699390024, 201.7969310139470167 ) ) ;
#39422 = CARTESIAN_POINT ( 'NONE',  ( 7.213731313499999409, 1426.540065858099979, 212.9766447227389961 ) ) ;
#39423 = CARTESIAN_POINT ( 'NONE',  ( 0.000000000000000000, 1523.382868172864164, 209.1218459616979999 ) ) ;
#39424 = CARTESIAN_POINT ( 'NONE',  ( 16.11904262073499794, 1512.169992403149990, 197.6534206206669921 ) ) ;
#39425 = FACE_BOUND ( 'NONE', #70786, .T. ) ;
#39426 = CARTESIAN_POINT ( 'NONE',  ( -3.220674668504990290, 1433.265634988960073, 218.1214075394389909 ) ) ;
#39428 = EDGE_CURVE ( 'NONE', #57302, #44714, #24983, .T. ) ;
#39427 = EDGE_CURVE ( 'NONE', #48513, #91956, #50932, .T. ) ;
#39429 = CARTESIAN_POINT ( 'NONE',  ( 5.721861508758420811, 1366.657167162936048, 208.3718459617061285 ) ) ;
#39431 = VERTEX_POINT ( 'NONE', #54002 ) ;
#39430 = CARTESIAN_POINT ( 'NONE',  ( -16.64413823199859976, 1379.585478419799983, 212.2328527173980035 ) ) ;
#39432 = ORIENTED_EDGE ( 'NONE', *, *, #60401, .F. ) ;
#39433 = CARTESIAN_POINT ( 'NONE',  ( -11.96158875949999967, 1396.389701308929943, 207.5433552565580158 ) ) ;
#39434 = CARTESIAN_POINT ( 'NONE',  ( -22.33897111659999979, 1410.187224098330034, 212.0108098173379858 ) ) ;
#39436 = CARTESIAN_POINT ( 'NONE',  ( -1.441539353560000070, 1414.983773854429955, 226.5042058782979666 ) ) ;
#39435 = B_SPLINE_CURVE_WITH_KNOTS ( 'NONE', 5,
 ( #35491, #36061, #78606, #61291, #104354, #62959 ),
 .UNSPECIFIED., .F., .F.,
 ( 6, 6 ),
 ( -2.000000000000000000, -3.509303492243986966E-08 ),
 .UNSPECIFIED. ) ;
#39437 = CARTESIAN_POINT ( 'NONE',  ( -13.51164583954868448, 1444.016856206453213, 169.3518408349974322 ) ) ;
#39438 = CARTESIAN_POINT ( 'NONE',  ( -26.37683243140000044, 1508.582706621130228, 201.5299903364179954 ) ) ;
#39439 = CARTESIAN_POINT ( 'NONE',  ( 2.329939107268570009, 1515.551844914359890, 205.1381281622049926 ) ) ;
#39442 = EDGE_CURVE ( 'NONE', #73345, #65239, #914, .T. ) ;
#39441 = CARTESIAN_POINT ( 'NONE',  ( 17.26703884499999830, 1419.032847617429979, 226.5196259762979878 ) ) ;
#39440 = CARTESIAN_POINT ( 'NONE',  ( 3.279726280340000244, 1445.963863862890094, 200.3213861966889908 ) ) ;
#39443 = AXIS2_PLACEMENT_3D ( 'NONE', #46006, #20219, #4004 ) ;
#39444 = CARTESIAN_POINT ( 'NONE',  ( -32.85805783624315524, 1523.678648413191922, 201.0453875934059340 ) ) ;
#39445 = DIRECTION ( 'NONE',  ( 1.755985294532469921E-16, -1.000000000000000000, 1.338183447452831989E-16 ) ) ;
#39446 = CARTESIAN_POINT ( 'NONE',  ( -41.56522242718469329, 1445.106110315470005, 135.9524270544380045 ) ) ;
#39447 = SHAPE_REPRESENTATION_RELATIONSHIP ( 'NONE' , 'NONE' ,  #72299, #19969 ) ;
#39448 = CARTESIAN_POINT ( 'NONE',  ( 6.447394074667360364, 1396.138208400039957, 200.1593900886609845 ) ) ;
#39449 = CARTESIAN_POINT ( 'NONE',  ( 1.138464810440000141, 1416.254459047329874, 190.2411719155979881 ) ) ;
#39450 = CARTESIAN_POINT ( 'NONE',  ( 11.43741207009999883, 1425.481177415629872, 144.1677667564979970 ) ) ;
#39451 = CARTESIAN_POINT ( 'NONE',  ( 7.316722005465000400, 1511.382498894329956, 202.5414830215270001 ) ) ;
#39452 = VERTEX_POINT ( 'NONE', #97623 ) ;
#39453 = CARTESIAN_POINT ( 'NONE',  ( 3.713785113579999742, 1424.815349392029930, 185.0498344327979794 ) ) ;
#39454 = CARTESIAN_POINT ( 'NONE',  ( 21.50863349123601509, 1524.374142163904253, 234.1185027681734709 ) ) ;
#39455 = ORIENTED_EDGE ( 'NONE', *, *, #42486, .T. ) ;
#39456 = VERTEX_POINT ( 'NONE', #5208 ) ;
#39457 = CARTESIAN_POINT ( 'NONE',  ( 10.96561470309999820, 1490.902452854290004, 209.8193876016359809 ) ) ;
#39458 = CARTESIAN_POINT ( 'NONE',  ( 8.726849315049999944, 1367.111769039820047, 207.6218459616989946 ) ) ;
#39459 = CARTESIAN_POINT ( 'NONE',  ( -109.1939007313264369, 1387.425512231509856, 310.9496258952415246 ) ) ;
#39460 = DIRECTION ( 'NONE',  ( 0.000000000000000000, 0.000000000000000000, 1.000000000000000000 ) ) ;
#39461 = CARTESIAN_POINT ( 'NONE',  ( -6.941100315875000426, 1516.858069504249897, 216.0654486236869900 ) ) ;
#39462 = CARTESIAN_POINT ( 'NONE',  ( -12.32664172942340031, 1378.996309998719880, 209.7960268208129833 ) ) ;
#39463 = B_SPLINE_CURVE_WITH_KNOTS ( 'NONE', 3,
 ( #102529, #50514, #101420, #110399, #75710, #33679, #40988, #42103, #68427, #67871 ),
 .UNSPECIFIED., .F., .F.,
 ( 4, 2, 2, 2, 4 ),
 ( 0.000000000000000000, 0.2500000000000000000, 0.5000000000000000000, 0.7500000000000000000, 1.000000000000000000 ),
 .UNSPECIFIED. ) ;
#39464 = VERTEX_POINT ( 'NONE', #56164 ) ;
#39465 = CARTESIAN_POINT ( 'NONE',  ( -11.41188801179999857, 1502.809396336989948, 207.5688504535389995 ) ) ;
#39466 = CARTESIAN_POINT ( 'NONE',  ( 2.500000000000000000, 1448.482477207059901, 160.8482066586829831 ) ) ;
#39467 = CARTESIAN_POINT ( 'NONE',  ( -42.70366651140000158, 1375.424979822739942, 226.7036006363589991 ) ) ;
#39468 = FACE_OUTER_BOUND ( 'NONE', #20516, .T. ) ;
#39469 = CARTESIAN_POINT ( 'NONE',  ( -1.135185082175000026, 1516.778853242349896, 205.6747174714770097 ) ) ;
#39470 = VERTEX_POINT ( 'NONE', #13033 ) ;
#39471 = CARTESIAN_POINT ( 'NONE',  ( 3.261652286895000419, 1516.939580991450157, 209.1085619926769823 ) ) ;
#39472 = CIRCLE ( 'NONE', #105584, 451.3741471861067680 ) ;
#39473 = CARTESIAN_POINT ( 'NONE',  ( -8.599604059879169426, 1451.952372034600103, 205.6084899554880110 ) ) ;
#39474 = B_SPLINE_SURFACE_WITH_KNOTS ( 'NONE', 5, 5, ( 
 ( #11493, #56246, #98787, #96598, #19869, #71440 ),
 ( #73051, #71982, #62478, #20412, #20962, #4193 ),
 ( #12585, #90375, #38326, #72505, #3112, #13653 ),
 ( #81976, #54073, #88749, #5284, #64114, #45668 ),
 ( #70880, #79807, #104992, #21504, #28283, #98235 ),
 ( #63573, #12033, #105555, #37241, #46766, #28842 ),
 ( #63038, #55718, #89837, #97144, #46214, #81417 ),
 ( #80348, #37794, #106095, #29373, #97689, #55166 ),
 ( #89290, #13110, #47293, #40538, #31029, #99875 ) ),
 .UNSPECIFIED., .F., .F., .F.,
 ( 6, 3, 6 ),
 ( 6, 6 ),
 ( 24.41308947359999948, 25.74260990720000208, 27.07213034080000114 ),
 ( 0.000000000000000000, 2.000000000000000000 ),
 .UNSPECIFIED. ) ;
#39475 = CARTESIAN_POINT ( 'NONE',  ( -35.60174245805101378, 1424.724877476223128, 269.5399423230903722 ) ) ;
#39476 = CARTESIAN_POINT ( 'NONE',  ( -1.069820623280000049, 1408.950419346429953, 232.0160439753980199 ) ) ;
#39478 = EDGE_LOOP ( 'NONE', ( #95080, #25523, #60146, #42896, #31052 ) ) ;
#39477 = CARTESIAN_POINT ( 'NONE',  ( -31.32995031131208918, 1523.678648413191695, 196.3423562208917872 ) ) ;
#39479 = CARTESIAN_POINT ( 'NONE',  ( -0.01305586186176959859, 1452.917665869470056, 183.2406260983729851 ) ) ;
#39480 = CARTESIAN_POINT ( 'NONE',  ( -33.74865851176389953, 1440.913060389799966, 248.3065938399680022 ) ) ;
#39481 = CARTESIAN_POINT ( 'NONE',  ( -89.65362972180000156, 1384.619809472219913, 308.7387643915590161 ) ) ;
#39482 = CARTESIAN_POINT ( 'NONE',  ( -0.6059102731196839287, 1465.006891891870055, 237.7143419758519940 ) ) ;
#39483 = CARTESIAN_POINT ( 'NONE',  ( 10.53025398842429894, 1410.959292425960030, 269.8740791142779472 ) ) ;
#39485 = CARTESIAN_POINT ( 'NONE',  ( -4.609673279564999504, 1516.754149861460064, 212.3872530880769887 ) ) ;
#39484 = CIRCLE ( 'NONE', #55657, 32.13701971169416538 ) ;
#39486 = CARTESIAN_POINT ( 'NONE',  ( -47.65858604169999779, 1379.688530322980114, 235.3355530128589805 ) ) ;
#39487 = CARTESIAN_POINT ( 'NONE',  ( 23.30720214069999940, 1409.831584714629798, 208.9977026400509885 ) ) ;
#39488 = CARTESIAN_POINT ( 'NONE',  ( 1.984413551915469975, 1517.151704408390060, 198.9129232538419956 ) ) ;
#39489 = CARTESIAN_POINT ( 'NONE',  ( 17.25714853236529933, 1428.491813688779757, 203.4901169056299750 ) ) ;
#39490 = CARTESIAN_POINT ( 'NONE',  ( -7.710086906866910006, 1516.574598972179956, 210.5804421991259971 ) ) ;
#39491 = CARTESIAN_POINT ( 'NONE',  ( -1.119592219845000125, 1516.958737650239982, 210.2577447559170025 ) ) ;
#39492 = CARTESIAN_POINT ( 'NONE',  ( 4.207967578379720130, 1420.996416529009821, 185.4063400840479972 ) ) ;
#39493 = CARTESIAN_POINT ( 'NONE',  ( 0.1277302730189999735, 1419.774434123929950, 184.3736332935979760 ) ) ;
#39494 = CARTESIAN_POINT ( 'NONE',  ( -19.63722818134010240, 1517.051704408389924, 200.0074286634620364 ) ) ;
#39496 = ORIENTED_EDGE ( 'NONE', *, *, #61029, .T. ) ;
#39495 = CARTESIAN_POINT ( 'NONE',  ( -45.21221387570000161, 1388.283329091300175, 219.7150970607590068 ) ) ;
#39497 = CARTESIAN_POINT ( 'NONE',  ( -42.52088808034810086, 1385.167360014890164, 246.7025410803429963 ) ) ;
#39498 = CARTESIAN_POINT ( 'NONE',  ( 18.79647803339999967, 1416.822694190429729, 209.8352280844500228 ) ) ;
#39499 = CARTESIAN_POINT ( 'NONE',  ( 0.3099421919009999749, 1416.442944220429808, 233.6989699818980171 ) ) ;
#39500 = AXIS2_PLACEMENT_3D ( 'NONE', #100650, #58131, #25039 ) ;
#39501 = CARTESIAN_POINT ( 'NONE',  ( -21.63548603055769703, 1509.707618109219993, 229.5065455109210006 ) ) ;
#39502 = CARTESIAN_POINT ( 'NONE',  ( 1.451113133880000072, 1499.806239416590188, 230.3830668976989955 ) ) ;
#39503 = CARTESIAN_POINT ( 'NONE',  ( 12.91459300150000011, 1421.176040162410118, 204.7063101998089962 ) ) ;
#39504 = DIRECTION ( 'NONE',  ( 0.000000000000000000, -1.000000000000000000, 6.123233995736769734E-17 ) ) ;
#39505 = AXIS2_PLACEMENT_3D ( 'NONE', #105248, #86786, #61608 ) ;
#39507 = CARTESIAN_POINT ( 'NONE',  ( 21.53712143570556137, 1523.621879633028811, 183.9400870382961841 ) ) ;
#39506 = CARTESIAN_POINT ( 'NONE',  ( -0.7391220051939990654, 1517.130100026000036, 216.0715493048870144 ) ) ;
#39508 = CARTESIAN_POINT ( 'NONE',  ( 7.294923546887015497, 1458.268531074105567, 201.0098627031420904 ) ) ;
#39509 = CARTESIAN_POINT ( 'NONE',  ( 33.93019615848559312, 1522.906561336852974, 220.5829544588082740 ) ) ;
#39510 = ORIENTED_EDGE ( 'NONE', *, *, #97190, .F. ) ;
#39511 = CARTESIAN_POINT ( 'NONE',  ( 3.453544825624999870, 1517.106845464700200, 201.7850012896870169 ) ) ;
#39512 = CARTESIAN_POINT ( 'NONE',  ( 10.44087869485973030, 1517.051704408389924, 212.8912867333128531 ) ) ;
#39513 = ORIENTED_EDGE ( 'NONE', *, *, #10703, .T. ) ;
#39514 = CARTESIAN_POINT ( 'NONE',  ( -0.2751659205230000405, 1506.798305149130101, 231.4088083078979992 ) ) ;
#39515 = CARTESIAN_POINT ( 'NONE',  ( 21.15356505109999929, 1453.179070293830137, 222.9746448834980015 ) ) ;
#39516 = CARTESIAN_POINT ( 'NONE',  ( 6.026450563690831430, 1440.073360909948860, 154.5831774296489129 ) ) ;
#39517 = CARTESIAN_POINT ( 'NONE',  ( 8.950879146035706668, 1424.989091137386595, 195.6957624501638406 ) ) ;
#39518 = CARTESIAN_POINT ( 'NONE',  ( 1.480262881429999844, 1443.955256524790002, 217.9442098410289930 ) ) ;
#39519 = CARTESIAN_POINT ( 'NONE',  ( -26.56916871408720127, 1508.840664607660074, 201.4539126542630072 ) ) ;
#39520 = AXIS2_PLACEMENT_3D ( 'NONE', #65573, #99684, #22977 ) ;
#39521 = CARTESIAN_POINT ( 'NONE',  ( 19.52205342210000083, 1473.076230373790168, 204.3554439105789982 ) ) ;
#39522 = CARTESIAN_POINT ( 'NONE',  ( -19.05596984009999773, 1425.010854422730063, 224.1379177625979935 ) ) ;
#39523 = CARTESIAN_POINT ( 'NONE',  ( -23.61227025210000008, 1435.322036687620084, 137.2858276859979867 ) ) ;
#39524 = CARTESIAN_POINT ( 'NONE',  ( -104.1029534810000001, 1389.819474454779993, 301.8406320987589879 ) ) ;
#39525 = CARTESIAN_POINT ( 'NONE',  ( 19.64045971950000080, 1507.861171870530143, 188.7866432982980029 ) ) ;
#39526 = DIRECTION ( 'NONE',  ( 0.000000000000000000, 6.123233995736769734E-17, 1.000000000000000000 ) ) ;
#39527 = CARTESIAN_POINT ( 'NONE',  ( -15.89197043703675583, 1469.153657686127644, 269.3685434817093665 ) ) ;
#39528 = EDGE_LOOP ( 'NONE', ( #26588, #55188, #56508, #31154 ) ) ;
#39529 = CARTESIAN_POINT ( 'NONE',  ( -104.5268087689999987, 1379.723412970779918, 303.3030969148589975 ) ) ;
#39530 = CARTESIAN_POINT ( 'NONE',  ( -16.59176436839999980, 1508.492920114390017, 213.6703949458789964 ) ) ;
#39531 = CARTESIAN_POINT ( 'NONE',  ( 11.87227031139999944, 1435.412617320299887, 147.6610825172980128 ) ) ;
#39532 = CARTESIAN_POINT ( 'NONE',  ( -29.99620953741502660, 1526.382868172863937, 198.4974435154502999 ) ) ;
#39533 = CARTESIAN_POINT ( 'NONE',  ( -12.54268436849999979, 1408.913060387329779, 221.6645303301980050 ) ) ;
#39534 = CARTESIAN_POINT ( 'NONE',  ( 1.468394784813899845, 1487.955722966210033, 181.9488289805979946 ) ) ;
#39535 = CARTESIAN_POINT ( 'NONE',  ( -15.43159309022804493, 1451.439643999777445, 222.6302084244509842 ) ) ;
#39536 = CARTESIAN_POINT ( 'NONE',  ( -13.19336125707238061, 1444.715447408086675, 186.5675026392735276 ) ) ;
#39537 = LINE ( 'NONE', #99418, #80673 ) ;
#39538 = DIRECTION ( 'NONE',  ( 0.9996573249755569268, -0.02617694830788839730, 1.602875797835060866E-18 ) ) ;
#39539 = CARTESIAN_POINT ( 'NONE',  ( -3.835404308833623155, 1405.413060387330006, 202.1011854665750036 ) ) ;
#39541 = EDGE_CURVE ( 'NONE', #40681, #92786, #59895, .T. ) ;
#39540 = CARTESIAN_POINT ( 'NONE',  ( -14.82123553143790140, 1415.677402202029953, 206.6677478258380063 ) ) ;
#39542 = CARTESIAN_POINT ( 'NONE',  ( -9.643323296948050682, 1460.351442354390201, 209.5911327240870037 ) ) ;
#39543 = CARTESIAN_POINT ( 'NONE',  ( 6.687468864090000409, 1429.390509083689949, 215.9663958518090112 ) ) ;
#39545 = ORIENTED_EDGE ( 'NONE', *, *, #78085, .F. ) ;
#39544 = DIRECTION ( 'NONE',  ( -0.3363363969979658030, -0.9417419115949056119, 0.000000000000000000 ) ) ;
#39546 = CARTESIAN_POINT ( 'NONE',  ( -89.86981536200001131, 1382.337715003790208, 308.1217387938589809 ) ) ;
#39547 = CARTESIAN_POINT ( 'NONE',  ( 12.49443849680770136, 1512.179780174510142, 224.0980365015450104 ) ) ;
#39548 = EDGE_CURVE ( 'NONE', #77826, #32575, #26395, .T. ) ;
#39549 = VERTEX_POINT ( 'NONE', #33153 ) ;
#39550 = VERTEX_POINT ( 'NONE', #5771 ) ;
#39551 = CARTESIAN_POINT ( 'NONE',  ( -12.78592627679999971, 1502.554352260989845, 209.5469753058839899 ) ) ;
#39552 = CARTESIAN_POINT ( 'NONE',  ( 6.100701914535983761, 1516.739200664758528, 204.7580812289224355 ) ) ;
#39554 = CARTESIAN_POINT ( 'NONE',  ( 4.634283904179999078E-09, 1465.695272584029908, 240.4142140037979800 ) ) ;
#39553 = CARTESIAN_POINT ( 'NONE',  ( 1.991751356299999776, 1454.627457338589920, 218.3211767913890071 ) ) ;
#39555 = CARTESIAN_POINT ( 'NONE',  ( 9.339431960871671379, 1436.245858615840007, 210.2893693010520053 ) ) ;
#39556 = CARTESIAN_POINT ( 'NONE',  ( -11.31301446079999984, 1433.586356650280095, 151.4935912186979863 ) ) ;
#39557 = CARTESIAN_POINT ( 'NONE',  ( -3.116134665872564380, 1509.034509761476556, 213.6092032002669328 ) ) ;
#39558 = CARTESIAN_POINT ( 'NONE',  ( 11.69439630328679947, 1426.723912090049907, 141.1194945047550107 ) ) ;
#39559 = DIRECTION ( 'NONE',  ( -0.7063774289747313251, 0.04540766091858271930, -0.7063774289747313251 ) ) ;
#39560 = FACE_OUTER_BOUND ( 'NONE', #104710, .T. ) ;
#39561 = CARTESIAN_POINT ( 'NONE',  ( -1.273031542849370146, 1515.087982642930001, 213.4506874923570194 ) ) ;
#39562 = CARTESIAN_POINT ( 'NONE',  ( -107.3811187542021912, 1379.376395203810944, 309.1054750742122224 ) ) ;
#39563 = CARTESIAN_POINT ( 'NONE',  ( -5.619035311959510004, 1477.367051216990149, 219.2138315790730019 ) ) ;
#39564 =( GEOMETRIC_REPRESENTATION_CONTEXT ( 3 ) GLOBAL_UNCERTAINTY_ASSIGNED_CONTEXT ( ( #25572 ) ) GLOBAL_UNIT_ASSIGNED_CONTEXT ( ( #80901, #20417, #88204 ) ) REPRESENTATION_CONTEXT ( 'NONE', 'WORKASPACE' ) );
#39565 = CARTESIAN_POINT ( 'NONE',  ( -4.745098151869999725, 1360.923919868640041, 207.6218459616989946 ) ) ;
#39566 = CARTESIAN_POINT ( 'NONE',  ( 34.09079054514428719, 1524.667648926107404, 200.3377533957251728 ) ) ;
#39568 = ORIENTED_EDGE ( 'NONE', *, *, #93623, .F. ) ;
#39567 = CARTESIAN_POINT ( 'NONE',  ( -1.430581255003579772E-09, 1413.383262237239933, 249.6119133123739857 ) ) ;
#39569 = ORIENTED_EDGE ( 'NONE', *, *, #836, .T. ) ;
#39570 = CARTESIAN_POINT ( 'NONE',  ( -11.86398566780919950, 1432.188216858459782, 149.9803512562860135 ) ) ;
#39571 = CARTESIAN_POINT ( 'NONE',  ( 19.12714126967820150, 1496.834737738279955, 222.0421931355600123 ) ) ;
#39572 = CARTESIAN_POINT ( 'NONE',  ( -3.400296248400000110, 1471.337052564629857, 269.3361249056980000 ) ) ;
#39573 = CARTESIAN_POINT ( 'NONE',  ( -1.555569193359999991, 1415.296882296330068, 227.2022622829979639 ) ) ;
#39576 = EDGE_CURVE ( 'NONE', #10869, #41956, #23093, .T. ) ;
#39575 = CIRCLE ( 'NONE', #75318, 0.9999999999999976685 ) ;
#39574 = CARTESIAN_POINT ( 'NONE',  ( -113.4000000000000057, 1377.418846546390114, 315.3996670310589820 ) ) ;
#39577 = CARTESIAN_POINT ( 'NONE',  ( 35.89837063142969953, 1451.292665198759778, 135.5646561065310038 ) ) ;
#39578 = CARTESIAN_POINT ( 'NONE',  ( 4.326999254989379651, 1515.158336317459998, 209.1856212445070184 ) ) ;
#39579 = CARTESIAN_POINT ( 'NONE',  ( -8.602704958620000397, 1384.751806508920026, 199.8723417454790194 ) ) ;
#39580 = CARTESIAN_POINT ( 'NONE',  ( 10.00058476560569964, 1468.846443592369724, 208.4342511431520109 ) ) ;
#39581 = CARTESIAN_POINT ( 'NONE',  ( -5.024929782580000115, 1457.083462483489939, 217.2019913456090308 ) ) ;
#39582 = CARTESIAN_POINT ( 'NONE',  ( 10.91522438530139638, 1365.730702465838704, 207.6218459616987673 ) ) ;
#39583 = CARTESIAN_POINT ( 'NONE',  ( -42.26673233833929544, 1426.182016276979994, 267.7309908727469860 ) ) ;
#39584 = ORIENTED_EDGE ( 'NONE', *, *, #98917, .T. ) ;
#39585 = CARTESIAN_POINT ( 'NONE',  ( -24.89775034519999863, 1442.835538705840008, 210.5176537872779932 ) ) ;
#39586 = VERTEX_POINT ( 'NONE', #74632 ) ;
#39587 = ORIENTED_EDGE ( 'NONE', *, *, #81068, .F. ) ;
#39588 = CARTESIAN_POINT ( 'NONE',  ( 1.717432448265000078, 1516.836638729160086, 211.4041475482669910 ) ) ;
#39589 = AXIS2_PLACEMENT_3D ( 'NONE', #79221, #98197, #55133 ) ;
#39590 = CARTESIAN_POINT ( 'NONE',  ( -8.993785038736740844, 1447.472150739280096, 212.1283412365259835 ) ) ;
#39591 = CARTESIAN_POINT ( 'NONE',  ( 41.11865450958669754, 1444.162607370569958, 136.7833858997449852 ) ) ;
#39592 = CARTESIAN_POINT ( 'NONE',  ( -1.702406023195000007, 1516.999105586269934, 212.3918307515370145 ) ) ;
#39593 = CARTESIAN_POINT ( 'NONE',  ( -15.72029972270000009, 1440.436594279349947, 189.7121662737980046 ) ) ;
#39594 = CARTESIAN_POINT ( 'NONE',  ( -2.133905332862266135, 1450.047792930902915, 182.8895505775221295 ) ) ;
#39595 = ORIENTED_EDGE ( 'NONE', *, *, #49377, .T. ) ;
#39596 = CARTESIAN_POINT ( 'NONE',  ( 10.10004869885203682, 1411.254281879943164, 135.5999999980979851 ) ) ;
#39597 =( BOUNDED_CURVE ( )  B_SPLINE_CURVE ( 3, ( #36165, #79279, #75985, #26111 ),
 .UNSPECIFIED., .F., .T. ) 
 B_SPLINE_CURVE_WITH_KNOTS ( ( 4, 4 ),
 ( 1.424829929282025898, 1.707080582674059821 ),
 .UNSPECIFIED. ) 
 CURVE ( )  GEOMETRIC_REPRESENTATION_ITEM ( )  RATIONAL_B_SPLINE_CURVE ( ( 1.000000000000000000, 0.9933722251124278424, 0.9933722251124278424, 1.000000000000000000 ) ) 
 REPRESENTATION_ITEM ( '' )  );
#39598 = CARTESIAN_POINT ( 'NONE',  ( -2.872700555325000238, 1516.559109716219837, 201.4121646638069763 ) ) ;
#39599 = VECTOR ( 'NONE', #46133, 1000.000000000000114 ) ;
#39600 = CARTESIAN_POINT ( 'NONE',  ( -2.038847259689231084, 1501.977400791986611, 244.9330574173806951 ) ) ;
#39601 = CARTESIAN_POINT ( 'NONE',  ( -13.70478788754319943, 1384.519254815689919, 200.4442307571110007 ) ) ;
#39602 = AXIS2_PLACEMENT_3D ( 'NONE', #97343, #87301, #61024 ) ;
#39603 = CARTESIAN_POINT ( 'NONE',  ( -44.93140264801330375, 1435.581069431369997, 269.6837702837809729 ) ) ;
#39604 = DIRECTION ( 'NONE',  ( -1.755985294532469921E-16, 1.000000000000000000, -1.338183447452831989E-16 ) ) ;
#39605 = CARTESIAN_POINT ( 'NONE',  ( -1.171291564450000156, 1396.015411382230013, 197.4876103079979828 ) ) ;
#39607 = ORIENTED_EDGE ( 'NONE', *, *, #23746, .F. ) ;
#39606 = CARTESIAN_POINT ( 'NONE',  ( -9.011061020611320416, 1364.914693253510450, 207.6218459616988241 ) ) ;
#39608 = VERTEX_POINT ( 'NONE', #100894 ) ;
#39609 = CARTESIAN_POINT ( 'NONE',  ( 0.3350112074000000106, 1452.978120002730066, 183.2691759946980028 ) ) ;
#39610 = CARTESIAN_POINT ( 'NONE',  ( 27.49569038830730605, 1468.273487270390888, 269.4050666718689513 ) ) ;
#39611 = CARTESIAN_POINT ( 'NONE',  ( -11.38166339569999863, 1381.807649517150139, 201.7589817661390157 ) ) ;
#39612 = CARTESIAN_POINT ( 'NONE',  ( -2.500000000000000000, 1419.414122305159026, 142.6947176393313441 ) ) ;
#39613 = CARTESIAN_POINT ( 'NONE',  ( -0.03584877448754099361, 1410.017694336640034, 185.0604024924950011 ) ) ;
#39614 = CARTESIAN_POINT ( 'NONE',  ( -3.447128498755000159, 1516.778853242349896, 210.2570310142770040 ) ) ;
#39615 = CIRCLE ( 'NONE', #102185, 1.999999999999998668 ) ;
#39616 = DIRECTION ( 'NONE',  ( -2.274506543718548102E-15, -0.7071067811865474617, -0.7071067811865474617 ) ) ;
#39617 = CARTESIAN_POINT ( 'NONE',  ( -0.2694122078740051607, 1452.981479858197417, 183.2530805312008511 ) ) ;
#39618 = CARTESIAN_POINT ( 'NONE',  ( 4.363122647530000009, 1407.471318475732687, 137.0999999980979851 ) ) ;
#39619 = CARTESIAN_POINT ( 'NONE',  ( 4.283856666023710069, 1440.956247486469920, 155.9231014612180104 ) ) ;
#39620 = CARTESIAN_POINT ( 'NONE',  ( 7.549016763624999626, 1510.423579818979988, 204.6938642082269837 ) ) ;
#39621 = VERTEX_POINT ( 'NONE', #14147 ) ;
#39622 = CARTESIAN_POINT ( 'NONE',  ( 1.700259675955000160, 1516.898441858519845, 207.4036424686470070 ) ) ;
#39623 = VERTEX_POINT ( 'NONE', #65681 ) ;
#39624 = CARTESIAN_POINT ( 'NONE',  ( -38.81202643698959776, 1450.612734567539974, 134.7398511103019985 ) ) ;
#39625 = CARTESIAN_POINT ( 'NONE',  ( -10.19411843490000003, 1472.876058185389866, 208.6040583671850186 ) ) ;
#39626 = CARTESIAN_POINT ( 'NONE',  ( -23.37010607166610043, 1448.870807780643645, 216.3500970213881089 ) ) ;
#39627 = ORIENTED_EDGE ( 'NONE', *, *, #108252, .F. ) ;
#39628 = CARTESIAN_POINT ( 'NONE',  ( 9.265501621498845708, 1455.798605834726004, 226.8760981150780935 ) ) ;
#39629 = CARTESIAN_POINT ( 'NONE',  ( -2.813821217590033452, 1367.641464860482529, 209.3838672787736641 ) ) ;
#39630 = CARTESIAN_POINT ( 'NONE',  ( 13.47470376080000065, 1415.128105756529976, 197.4143262845979905 ) ) ;
#39631 = LINE ( 'NONE', #65403, #86050 ) ;
#39632 = CARTESIAN_POINT ( 'NONE',  ( 10.41132050455482982, 1519.551704408389924, 228.7775216444308342 ) ) ;
#39633 = CARTESIAN_POINT ( 'NONE',  ( 17.50305786550000064, 1410.885931832129927, 225.6206267369979912 ) ) ;
#39634 = CARTESIAN_POINT ( 'NONE',  ( 32.86802468363470098, 1523.481610118012213, 201.0396662541351986 ) ) ;
#39635 = CARTESIAN_POINT ( 'NONE',  ( 13.89869200000000049, 1452.835253893030085, 223.8385666725980059 ) ) ;
#39636 = CARTESIAN_POINT ( 'NONE',  ( 4.247012561190310009, 1441.378048274870025, 161.6132208113730258 ) ) ;
#39637 = DIRECTION ( 'NONE',  ( 0.000000000000000000, -6.123233995736769734E-17, -1.000000000000000000 ) ) ;
#39638 = DIRECTION ( 'NONE',  ( -0.4794255386042042266, 2.935634756405672795E-17, 0.8775825618903720926 ) ) ;
#39639 = CARTESIAN_POINT ( 'NONE',  ( -3.259101837015000225, 1517.102359858469754, 216.0714209178769920 ) ) ;
#39640 = ORIENTED_EDGE ( 'NONE', *, *, #106213, .T. ) ;
#39641 = CARTESIAN_POINT ( 'NONE',  ( -17.48275921970000013, 1417.637981030829906, 206.6019964927289720 ) ) ;
#39642 = STYLED_ITEM ( 'NONE', ( #55041 ), #67999 ) ;
#39643 = CARTESIAN_POINT ( 'NONE',  ( -41.12099125829999480, 1454.819569115930108, 269.7572481037980197 ) ) ;
#39644 = CARTESIAN_POINT ( 'NONE',  ( -11.71997758781537868, 1414.913060387329779, 220.1971170300299434 ) ) ;
#39645 = CARTESIAN_POINT ( 'NONE',  ( -3.047791110882830168, 1421.605825503799906, 133.5222801187929917 ) ) ;
#39646 = CARTESIAN_POINT ( 'NONE',  ( -2.702426668010000199, 1474.936083011690016, 219.0658163223389749 ) ) ;
#39647 = CARTESIAN_POINT ( 'NONE',  ( 7.722580313994999557, 1517.051704397749972, 213.7119064319370239 ) ) ;
#39648 = CARTESIAN_POINT ( 'NONE',  ( 2.095694667039108339, 1417.379259930220314, 233.2286282754426168 ) ) ;
#39649 = CARTESIAN_POINT ( 'NONE',  ( -2.500000000000000000, 1432.180584051779761, 157.4911758378979982 ) ) ;
#39650 = CARTESIAN_POINT ( 'NONE',  ( -2.139976072801630380, 1454.838776466839818, 198.8441892363819932 ) ) ;
#39651 = CARTESIAN_POINT ( 'NONE',  ( -21.84020450222075738, 1523.382868172864164, 183.2638850454220858 ) ) ;
#39652 = CARTESIAN_POINT ( 'NONE',  ( 28.49669390769100374, 1440.913060387309997, 233.1064013253619862 ) ) ;
#39654 = CARTESIAN_POINT ( 'NONE',  ( -7.980162481601299262, 1424.786834349992887, 210.5240428619318322 ) ) ;
#39653 = DIRECTION ( 'NONE',  ( -1.755985294532469921E-16, 1.000000000000000000, -1.338183447452831989E-16 ) ) ;
#39655 = CARTESIAN_POINT ( 'NONE',  ( 13.21447417100000088, 1422.962187270429922, 221.8217804547979881 ) ) ;
#39656 = VERTEX_POINT ( 'NONE', #108767 ) ;
#39658 = ORIENTED_EDGE ( 'NONE', *, *, #91727, .F. ) ;
#39657 = B_SPLINE_CURVE_WITH_KNOTS ( 'NONE', 5,
 ( #91344, #48812, #83477, #5695, #82935, #15698, #65609, #99167, #49350 ),
 .UNSPECIFIED., .F., .F.,
 ( 6, 3, 6 ),
 ( 0.000000000000000000, 0.4798557570286712815, 1.000000000000000000 ),
 .UNSPECIFIED. ) ;
#39659 = CARTESIAN_POINT ( 'NONE',  ( 13.51610093808350221, 1442.913060377700731, 150.6358704321319237 ) ) ;
#39660 = CARTESIAN_POINT ( 'NONE',  ( 1.248319867352440049, 1432.832940376729994, 200.7627304351539976 ) ) ;
#39661 = AXIS2_PLACEMENT_3D ( 'NONE', #16780, #69459, #49882 ) ;
#39662 = CARTESIAN_POINT ( 'NONE',  ( -0.5085492386525418684, 1408.930820210946422, 186.5021863892519320 ) ) ;
#39663 = CARTESIAN_POINT ( 'NONE',  ( 11.35500377106789927, 1502.899977923620099, 211.0831124703279897 ) ) ;
#39664 = FACE_OUTER_BOUND ( 'NONE', #110313, .T. ) ;
#39665 = CARTESIAN_POINT ( 'NONE',  ( -17.73406580063780069, 1423.343214054229975, 226.1884525926029994 ) ) ;
#39666 = CARTESIAN_POINT ( 'NONE',  ( -1.398163373145720145, 1508.551704408389924, 220.0821830793859704 ) ) ;
#39667 = CARTESIAN_POINT ( 'NONE',  ( -45.07337503762840214, 1383.820054821190070, 251.3008954162190207 ) ) ;
#39668 = CARTESIAN_POINT ( 'NONE',  ( -16.09728575562460051, 1496.785509464440111, 224.3774119518249961 ) ) ;
#39669 = CARTESIAN_POINT ( 'NONE',  ( -15.03004244010000079, 1489.480617680229898, 193.2534437250980091 ) ) ;
#39670 = CARTESIAN_POINT ( 'NONE',  ( -11.55818388030770016, 1501.591350514780061, 208.7507439016920046 ) ) ;
#39671 = CARTESIAN_POINT ( 'NONE',  ( 2.219216292930000112, 1464.733825611330076, 235.9342693422979949 ) ) ;
#39673 = ORIENTED_EDGE ( 'NONE', *, *, #84652, .T. ) ;
#39672 = CARTESIAN_POINT ( 'NONE',  ( 31.29224244793351417, 1525.661276915132476, 216.2849148480870838 ) ) ;
#39674 = CARTESIAN_POINT ( 'NONE',  ( -0.7219500573439999735, 1452.548174062430007, 183.3754457303979848 ) ) ;
#39675 = VECTOR ( 'NONE', #107677, 1000.000000000000000 ) ;
#39676 = CARTESIAN_POINT ( 'NONE',  ( -29.04720760670000246, 1380.913020375419819, 224.0879423276590217 ) ) ;
#39677 = CARTESIAN_POINT ( 'NONE',  ( 3.384752633832900148, 1508.551704408389924, 204.2997876064260083 ) ) ;
#39679 = ORIENTED_EDGE ( 'NONE', *, *, #18018, .F. ) ;
#39678 = CARTESIAN_POINT ( 'NONE',  ( -19.66678637224480397, 1517.151704408390060, 215.8936635741279986 ) ) ;
#39680 = CARTESIAN_POINT ( 'NONE',  ( 10.37957671256920023, 1453.090566707049902, 190.0119522185410119 ) ) ;
#39681 = VERTEX_POINT ( 'NONE', #6310 ) ;
#39682 = CARTESIAN_POINT ( 'NONE',  ( -8.945497862365648700, 1385.615016313520073, 218.6252861300649784 ) ) ;
#39683 = CARTESIAN_POINT ( 'NONE',  ( -3.368571795366160249, 1515.551842517600107, 205.3433056528259897 ) ) ;
#39684 = CARTESIAN_POINT ( 'NONE',  ( -11.60004869884828338, 1426.501519354271977, 135.6460154492365575 ) ) ;
#39685 = CARTESIAN_POINT ( 'NONE',  ( -106.5042781940000083, 1381.696109913969849, 298.6533303033589846 ) ) ;
#39686 = CARTESIAN_POINT ( 'NONE',  ( 2.745142294599053567, 1419.769955103634175, 137.0999999980979567 ) ) ;
#39687 = B_SPLINE_CURVE_WITH_KNOTS ( 'NONE', 3,
 ( #5637, #75058, #14566, #57162, #82879, #82337, #40326, #31925, #81223, #4538, #91829, #66118, #22393 ),
 .UNSPECIFIED., .F., .F.,
 ( 4, 3, 3, 3, 4 ),
 ( -6.921059206559499799, -6.378283243919759649, -5.323661303994230209, -4.287854170524850517, -3.271576390819999958 ),
 .UNSPECIFIED. ) ;
#39688 = CARTESIAN_POINT ( 'NONE',  ( 10.34831838578470098, 1409.274431628310140, 198.3247425477780155 ) ) ;
#39689 = CARTESIAN_POINT ( 'NONE',  ( 18.52259794967000062, 1425.592554617246151, 225.5483412146120088 ) ) ;
#39690 = FACE_OUTER_BOUND ( 'NONE', #47725, .T. ) ;
#39691 = CARTESIAN_POINT ( 'NONE',  ( -19.91456662359999896, 1485.663097783829926, 191.2402015274980158 ) ) ;
#39692 = CARTESIAN_POINT ( 'NONE',  ( 11.76903984429999994, 1432.302179532869786, 150.8119321890980018 ) ) ;
#39693 = TOROIDAL_SURFACE ( 'NONE', #61159, 25.96906897330000064, 0.5000000000000000000 ) ;
#39694 = CARTESIAN_POINT ( 'NONE',  ( -3.615177284590409990, 1449.532947440919997, 184.9113150316539986 ) ) ;
#39695 = EDGE_LOOP ( 'NONE', ( #108215, #93011, #32933, #20457 ) ) ;
#39696 = CARTESIAN_POINT ( 'NONE',  ( 19.39983987835423918, 1522.382868172863937, 239.2921289694223503 ) ) ;
#39697 = CARTESIAN_POINT ( 'NONE',  ( -7.826748708962336210, 1427.837793894468859, 134.0999999980979851 ) ) ;
#39698 = AXIS2_PLACEMENT_3D ( 'NONE', #30056, #72637, #64247 ) ;
#39699 = DIRECTION ( 'NONE',  ( -0.8090169943749507819, 0.000000000000000000, -0.5877852522924685852 ) ) ;
#39700 = CARTESIAN_POINT ( 'NONE',  ( 12.82316716488450048, 1420.870306943950027, 202.5884333197170122 ) ) ;
#39701 = CARTESIAN_POINT ( 'NONE',  ( -20.23330171276339939, 1495.987187365530190, 190.7338839421090313 ) ) ;
#39702 = CARTESIAN_POINT ( 'NONE',  ( -14.76729556169999924, 1420.459770328189734, 213.1799085011889758 ) ) ;
#39703 = CARTESIAN_POINT ( 'NONE',  ( -109.2173541970000059, 1385.843882786750100, 311.1794573962590107 ) ) ;
#39704 = CARTESIAN_POINT ( 'NONE',  ( -0.1904153588180000078, 1483.383698146929873, 181.9103537380979958 ) ) ;
#39705 = CARTESIAN_POINT ( 'NONE',  ( -8.052217410967335454, 1361.074664824414413, 207.6218459616987673 ) ) ;
#39706 = CARTESIAN_POINT ( 'NONE',  ( -46.04570283003550202, 1440.250595516199837, 266.6772069938360232 ) ) ;
#39707 = CARTESIAN_POINT ( 'NONE',  ( -19.80431309490000302, 1426.801393628430105, 224.9940485357979867 ) ) ;
#39708 = CARTESIAN_POINT ( 'NONE',  ( -22.39107471859139764, 1501.813592682170110, 208.5249304223659976 ) ) ;
#39709 = B_SPLINE_CURVE_WITH_KNOTS ( 'NONE', 3,
 ( #43533, #35669, #96130, #44084, #70413, #26710, #96697, #11034, #53044, #36781, #18848, #10471, #9370, #44644, #79896, #60336, #103405, #60904, #45201, #78224, #70973, #95579 ),
 .UNSPECIFIED., .F., .F.,
 ( 4, 3, 3, 3, 3, 3, 3, 4 ),
 ( -7.319250909075099898, -7.125925300183699740, -6.024000583945539944, -5.159116688310800392, -5.076639483430359867, -4.351712499397559775, -3.635277218665780019, -2.998981459959999540 ),
 .UNSPECIFIED. ) ;
#39710 = EDGE_CURVE ( 'NONE', #100597, #43261, #15771, .T. ) ;
#39711 = CARTESIAN_POINT ( 'NONE',  ( -6.564578723344999922, 1517.199196846569976, 207.4137433428170141 ) ) ;
#39712 = CARTESIAN_POINT ( 'NONE',  ( -9.044119212145819375, 1448.868168609049917, 210.5545963948329984 ) ) ;
#39713 = CARTESIAN_POINT ( 'NONE',  ( 3.897533513563200103, 1407.987765282759938, 221.8195319916089829 ) ) ;
#39714 = CARTESIAN_POINT ( 'NONE',  ( -14.08841074084159928, 1436.255549608840056, 150.1863611090900008 ) ) ;
#39715 = SURFACE_SIDE_STYLE ('',( #66042 ) ) ;
#39716 = CARTESIAN_POINT ( 'NONE',  ( 2.977092784659999936, 1421.750417338729903, 122.8790358596979928 ) ) ;
#39717 = CARTESIAN_POINT ( 'NONE',  ( 7.301066274272970169, 1425.020808777460161, 212.6544105784089993 ) ) ;
#39718 = ORIENTED_EDGE ( 'NONE', *, *, #70193, .T. ) ;
#39719 = CARTESIAN_POINT ( 'NONE',  ( 33.66409354169999801, 1434.352089750400182, 250.0355534229980492 ) ) ;
#39720 = CARTESIAN_POINT ( 'NONE',  ( -27.66125109240000057, 1508.130528727329875, 205.7926023901279677 ) ) ;
#39722 = CARTESIAN_POINT ( 'NONE',  ( -17.06941237829999736, 1409.674943312830010, 194.0661809782980072 ) ) ;
#39721 = CARTESIAN_POINT ( 'NONE',  ( 0.4840505593630000103, 1486.443749368729868, 181.8234518676980258 ) ) ;
#39723 = CARTESIAN_POINT ( 'NONE',  ( -5.513435590433334532, 1508.551704408459500, 216.2634855482666012 ) ) ;
#39724 = CARTESIAN_POINT ( 'NONE',  ( -21.29137176940000131, 1428.105725915830135, 225.2483481452979959 ) ) ;
#39725 = CARTESIAN_POINT ( 'NONE',  ( -4.633397098031163175, 1377.913060387290216, 214.0697612255490014 ) ) ;
#39726 = CARTESIAN_POINT ( 'NONE',  ( -2.967187434369539911, 1452.809443918890111, 152.3758103778500015 ) ) ;
#39727 = CARTESIAN_POINT ( 'NONE',  ( 27.44739306059999961, 1451.807595801730031, 135.7772701328979963 ) ) ;
#39728 = ORIENTED_EDGE ( 'NONE', *, *, #52842, .T. ) ;
#39729 = CARTESIAN_POINT ( 'NONE',  ( -107.7967585290650021, 1378.913060387369796, 300.1988973161450076 ) ) ;
#39730 = CARTESIAN_POINT ( 'NONE',  ( 21.12212911287032213, 1511.187213306747708, 235.8226600804184159 ) ) ;
#39731 = CARTESIAN_POINT ( 'NONE',  ( 16.34718949245090158, 1423.188823444010040, 228.3968466436469953 ) ) ;
#39732 = CARTESIAN_POINT ( 'NONE',  ( 17.33645362950000290, 1414.996442546130083, 210.3925741896480304 ) ) ;
#39733 = ORIENTED_EDGE ( 'NONE', *, *, #72659, .T. ) ;
#39734 = VERTEX_POINT ( 'NONE', #82473 ) ;
#39735 = CARTESIAN_POINT ( 'NONE',  ( -9.853078183510000088, 1384.932634673870098, 199.8720430995890069 ) ) ;
#39736 = CARTESIAN_POINT ( 'NONE',  ( -22.87714078023959985, 1409.721603508060070, 209.3742144960980056 ) ) ;
#39737 = ORIENTED_EDGE ( 'NONE', *, *, #70715, .T. ) ;
#39738 = CARTESIAN_POINT ( 'NONE',  ( -0.1620123092989999847, 1416.817366565030170, 227.3670020742980284 ) ) ;
#39739 = CARTESIAN_POINT ( 'NONE',  ( -17.68237282055029880, 1522.051704408389924, 205.6847408665509818 ) ) ;
#39740 = CARTESIAN_POINT ( 'NONE',  ( -1.545769114060000060, 1507.641667498930019, 237.1363977266979930 ) ) ;
#39741 = CARTESIAN_POINT ( 'NONE',  ( 0.4151546846821903003, 1512.187213306747481, 173.3106345060153046 ) ) ;
#39742 = VERTEX_POINT ( 'NONE', #57300 ) ;
#39743 = EDGE_CURVE ( 'NONE', #47552, #47062, #104560, .T. ) ;
#39744 = CARTESIAN_POINT ( 'NONE',  ( 43.12262697494430341, 1452.630018548870112, 266.2617581945530105 ) ) ;
#39745 = ADVANCED_FACE ( 'NONE', ( #66249 ), #38921, .T. ) ;
#39746 = CARTESIAN_POINT ( 'NONE',  ( -12.87305953236479894, 1416.529254608160045, 221.9220372573969939 ) ) ;
#39747 = CARTESIAN_POINT ( 'NONE',  ( -7.604266383829999754, 1426.735969319010110, 206.0920978162889980 ) ) ;
#39748 = CARTESIAN_POINT ( 'NONE',  ( -6.559798094425000059, 1516.987478262539980, 204.5068286042669854 ) ) ;
#39749 = ORIENTED_EDGE ( 'NONE', *, *, #17863, .F. ) ;
#39751 = EDGE_CURVE ( 'NONE', #99599, #52697, #30365, .T. ) ;
#39750 = CARTESIAN_POINT ( 'NONE',  ( 11.15342146135749957, 1480.750365135299944, 212.9722137386380041 ) ) ;
#39752 = AXIS2_PLACEMENT_3D ( 'NONE', #53178, #80573, #87321 ) ;
#39753 = CARTESIAN_POINT ( 'NONE',  ( 13.48661114156805496, 1443.650664694040188, 188.0188052989198582 ) ) ;
#39754 = ORIENTED_EDGE ( 'NONE', *, *, #17320, .F. ) ;
#39755 = ORIENTED_EDGE ( 'NONE', *, *, #90583, .F. ) ;
#39756 = CARTESIAN_POINT ( 'NONE',  ( -10.70297910787769879, 1480.941407630280082, 209.2201545748799845 ) ) ;
#39757 = ADVANCED_FACE ( 'NONE', ( #69000 ), #78481, .T. ) ;
#39758 = DIRECTION ( 'NONE',  ( 0.7071067811865490160, 0.000000000000000000, 0.7071067811865461294 ) ) ;
#39759 = EDGE_CURVE ( 'NONE', #23029, #97372, #83139, .T. ) ;
#39760 = CARTESIAN_POINT ( 'NONE',  ( -14.02477542606970040, 1513.114148093550057, 193.8538915311939661 ) ) ;
#39761 = CARTESIAN_POINT ( 'NONE',  ( 2.865104109652619524, 1452.813008747159756, 152.3914803971919980 ) ) ;
#39762 = CARTESIAN_POINT ( 'NONE',  ( 9.570877374229999290, 1420.722443590560033, 197.0571623609990297 ) ) ;
#39763 = CARTESIAN_POINT ( 'NONE',  ( -2.039945179225050254, 1475.967660246570176, 220.3917608611429841 ) ) ;
#39764 = CARTESIAN_POINT ( 'NONE',  ( 19.02174849391997924, 1456.743990138540767, 225.7168055990159985 ) ) ;
#39765 = CARTESIAN_POINT ( 'NONE',  ( -4.873188877689999643, 1496.854351603390114, 198.9825648115990191 ) ) ;
#39766 = FACE_OUTER_BOUND ( 'NONE', #20039, .T. ) ;
#39768 = CARTESIAN_POINT ( 'NONE',  ( 16.06975285769999928, 1489.474306033529956, 194.0919983873980073 ) ) ;
#39767 = CARTESIAN_POINT ( 'NONE',  ( -13.63839190360340048, 1434.968068183459991, 148.6805963842519986 ) ) ;
#39769 = CARTESIAN_POINT ( 'NONE',  ( 8.486023334060121215, 1517.051704408389924, 207.2139745301958271 ) ) ;
#39770 = CARTESIAN_POINT ( 'NONE',  ( -24.04775057459589860, 1508.134858764150067, 222.3238671512500275 ) ) ;
#39771 = CARTESIAN_POINT ( 'NONE',  ( 9.559188306630000298, 1428.004395111430085, 145.6094494780980142 ) ) ;
#39772 = EDGE_LOOP ( 'NONE', ( #107485, #30911, #50088, #55230, #54741 ) ) ;
#39773 = CARTESIAN_POINT ( 'NONE',  ( 6.454036439679999404, 1470.375359702289870, 211.5526527559590022 ) ) ;
#39774 = CIRCLE ( 'NONE', #73766, 12.49965726619999984 ) ;
#39775 = CARTESIAN_POINT ( 'NONE',  ( -3.274320305756030160E-16, 1450.913060387229962, 154.2476693630359819 ) ) ;
#39776 = CARTESIAN_POINT ( 'NONE',  ( -82.94653126506901231, 1384.986406227859788, 305.6412706045470600 ) ) ;
#39777 = CARTESIAN_POINT ( 'NONE',  ( -8.083309084479999740, 1385.702140206949935, 199.6133739923190262 ) ) ;
#39778 = CARTESIAN_POINT ( 'NONE',  ( -12.39573405564623165, 1517.051704408389924, 199.6750929870061668 ) ) ;
#39779 = EDGE_CURVE ( 'NONE', #38412, #20993, #69556, .T. ) ;
#39781 = EDGE_LOOP ( 'NONE', ( #47852, #4562, #64531, #50305 ) ) ;
#39780 = CARTESIAN_POINT ( 'NONE',  ( 11.07287788601909995, 1424.672578760980059, 203.0822791269380332 ) ) ;
#39782 = CARTESIAN_POINT ( 'NONE',  ( 2.529870311359999846, 1429.478213350389979, 217.0523039979090072 ) ) ;
#39783 = CARTESIAN_POINT ( 'NONE',  ( -7.544821708607240218, 1384.901423427800182, 219.0876899943770013 ) ) ;
#39784 = CARTESIAN_POINT ( 'NONE',  ( 1.110223024629999949E-15, 1377.913060387289988, 209.1218459616989946 ) ) ;
#39785 = CARTESIAN_POINT ( 'NONE',  ( 11.92647681149999883, 1433.523782385620052, 150.2359986513980061 ) ) ;
#39786 = CARTESIAN_POINT ( 'NONE',  ( 12.15345567070000143, 1468.554006627229910, 265.6112251771979800 ) ) ;
#39787 = CARTESIAN_POINT ( 'NONE',  ( -22.86388144358860330, 1435.295931049460023, 134.1000000049170069 ) ) ;
#39788 = ADVANCED_FACE ( 'NONE', ( #43232 ), #40138, .T. ) ;
#39789 = CARTESIAN_POINT ( 'NONE',  ( 8.559858904628349308, 1437.030483964089854, 207.9845584131589931 ) ) ;
#39790 = CARTESIAN_POINT ( 'NONE',  ( -109.4257410045153165, 1387.211591992306467, 297.3482829929823765 ) ) ;
#39791 = ADVANCED_FACE ( 'NONE', ( #86871 ), #27516, .T. ) ;
#39792 = CARTESIAN_POINT ( 'NONE',  ( 14.90141943649999945, 1419.765491606529849, 227.9873096972980022 ) ) ;
#39793 = CARTESIAN_POINT ( 'NONE',  ( 0.5359454300520634096, 1410.309919237011854, 233.1502810298127883 ) ) ;
#39794 = DIRECTION ( 'NONE',  ( 0.000000000000000000, 1.000000000000000000, 0.000000000000000000 ) ) ;
#39795 = CARTESIAN_POINT ( 'NONE',  ( -18.08242730619999605, 1410.468575122029733, 224.5973926771980018 ) ) ;
#39796 = CARTESIAN_POINT ( 'NONE',  ( 28.96738428617755190, 1526.189899547014647, 220.8024311359775425 ) ) ;
#39797 = CARTESIAN_POINT ( 'NONE',  ( -20.06562366400000030, 1485.934169092390221, 214.0282076738189971 ) ) ;
#39798 = CARTESIAN_POINT ( 'NONE',  ( 9.862951377130659836, 1521.951704408389787, 189.8497022437369708 ) ) ;
#39799 = CARTESIAN_POINT ( 'NONE',  ( -17.13435691658580140, 1410.007868545600104, 192.3884277009809978 ) ) ;
#39800 = CARTESIAN_POINT ( 'NONE',  ( 1.842962231260000028, 1515.219201591190085, 204.7964405199890336 ) ) ;
#39801 = CARTESIAN_POINT ( 'NONE',  ( -14.45615645293159979, 1417.226029900110007, 203.2557612791789836 ) ) ;
#39802 = CARTESIAN_POINT ( 'NONE',  ( -10.96946876072200006, 1432.347663854339999, 151.7701362700559855 ) ) ;
#39803 = CARTESIAN_POINT ( 'NONE',  ( -8.469419501860000921, 1416.216252248530054, 225.1067773946980139 ) ) ;
#39804 = CARTESIAN_POINT ( 'NONE',  ( 0.2169929020791310226, 1453.438874170419922, 183.2345656878090097 ) ) ;
#39805 = CARTESIAN_POINT ( 'NONE',  ( -9.740725139009999367, 1409.193360974830057, 198.3895369463979819 ) ) ;
#39806 = CARTESIAN_POINT ( 'NONE',  ( -12.18581598819999989, 1415.088016306429836, 197.3189424682980189 ) ) ;
#39807 = CARTESIAN_POINT ( 'NONE',  ( -28.44549777152819914, 1509.607982451979979, 211.0864871972310084 ) ) ;
#39808 = CARTESIAN_POINT ( 'NONE',  ( 13.50119150350000119, 1434.968975554210147, 147.9458048916980033 ) ) ;
#39809 = CARTESIAN_POINT ( 'NONE',  ( -35.52558520677190046, 1435.900183204640143, 134.0999999974749812 ) ) ;
#39810 = CARTESIAN_POINT ( 'NONE',  ( 8.765894577279999211, 1440.430470941899785, 186.4520186125980103 ) ) ;
#39811 = ORIENTED_EDGE ( 'NONE', *, *, #109532, .T. ) ;
#39812 = CARTESIAN_POINT ( 'NONE',  ( -16.86500409606249562, 1525.697947650550304, 181.8505186805997482 ) ) ;
#39813 = CARTESIAN_POINT ( 'NONE',  ( -32.97913964219424088, 1512.187213306747481, 220.2739374644216355 ) ) ;
#39814 = CARTESIAN_POINT ( 'NONE',  ( -107.6855514720864306, 1382.839660080642034, 310.6340048910524274 ) ) ;
#39815 = DIRECTION ( 'NONE',  ( -0.9455185755993178454, 0.000000000000000000, 0.3255681544571539243 ) ) ;
#39816 = CARTESIAN_POINT ( 'NONE',  ( -1.033934541210000058, 1452.678099303230056, 183.5143811305979966 ) ) ;
#39817 = DIRECTION ( 'NONE',  ( -0.9996573249755569268, -0.02617694830788819954, 0.000000000000000000 ) ) ;
#39818 = CARTESIAN_POINT ( 'NONE',  ( -109.1314732179999965, 1384.943873489550015, 311.2645625782590173 ) ) ;
#39819 = CARTESIAN_POINT ( 'NONE',  ( -19.90347714819266400, 1504.417445143046052, 189.0711003657198148 ) ) ;
#39820 = FACE_OUTER_BOUND ( 'NONE', #20854, .T. ) ;
#39821 = CARTESIAN_POINT ( 'NONE',  ( 2.500000000000000000, 1425.929641631630147, 183.3886485112979869 ) ) ;
#39822 = CARTESIAN_POINT ( 'NONE',  ( -50.05828054499940549, 1385.019276194180065, 225.3411702308840177 ) ) ;
#39823 = CARTESIAN_POINT ( 'NONE',  ( -12.25193733536140073, 1490.464065053120066, 208.8495834660220112 ) ) ;
#39824 = CARTESIAN_POINT ( 'NONE',  ( -4.239735416363259901, 1508.551704408389924, 204.8502244740350022 ) ) ;
#39825 = CARTESIAN_POINT ( 'NONE',  ( -28.53735979761090036, 1509.098833409579811, 208.7800982448970046 ) ) ;
#39826 = CARTESIAN_POINT ( 'NONE',  ( -15.81239850789610202, 1409.465374018880084, 225.3821397894910206 ) ) ;
#39828 = EDGE_LOOP ( 'NONE', ( #38954, #92577, #21794, #76364 ) ) ;
#39827 = CARTESIAN_POINT ( 'NONE',  ( -21.84020450222019250, 1523.382868172864164, 234.9798068779743403 ) ) ;
#39829 = DIRECTION ( 'NONE',  ( -0.8386695113602914420, -0.4884709562386498338, -0.2408932868014154460 ) ) ;
#39830 = CARTESIAN_POINT ( 'NONE',  ( 11.39055221683119967, 1471.191658448979979, 209.8979774520730075 ) ) ;
#39831 = CARTESIAN_POINT ( 'NONE',  ( 18.07341264884579957, 1430.225308298370010, 211.4628600911939884 ) ) ;
#39832 = PRESENTATION_STYLE_ASSIGNMENT (( #57210 ) ) ;
#39833 = CARTESIAN_POINT ( 'NONE',  ( -113.4000000000000057, 1389.413060387289988, 304.2218459572590064 ) ) ;
#39834 = CARTESIAN_POINT ( 'NONE',  ( 0.2860585402580000380, 1466.760278681229920, 235.6133694232979963 ) ) ;
#39835 = CARTESIAN_POINT ( 'NONE',  ( 20.46412024869999868, 1410.988662584130225, 219.2699858747980102 ) ) ;
#39836 = CARTESIAN_POINT ( 'NONE',  ( -2.418217451635309878, 1419.517398164420001, 186.0902754504199947 ) ) ;
#39837 = CARTESIAN_POINT ( 'NONE',  ( -20.45989939420000425, 1467.733552288090095, 211.3272550349789753 ) ) ;
#39838 = CARTESIAN_POINT ( 'NONE',  ( -16.07129795299999842, 1423.037556925630042, 229.0666284455979849 ) ) ;
#39840 = LINE ( 'NONE', #14626, #45086 ) ;
#39839 = CARTESIAN_POINT ( 'NONE',  ( -4.076752252616049788, 1511.455710048287301, 200.9017954071260021 ) ) ;
#39841 = CARTESIAN_POINT ( 'NONE',  ( 24.98278806157259879, 1430.498769693610029, 208.7705283626380037 ) ) ;
#39842 = CARTESIAN_POINT ( 'NONE',  ( -102.7365228771000574, 1314.643966242390661, 306.9446787514269204 ) ) ;
#39843 = CARTESIAN_POINT ( 'NONE',  ( 10.22570915140000025, 1431.113060387329824, 225.5143498067979806 ) ) ;
#39844 = CARTESIAN_POINT ( 'NONE',  ( -23.45859897689999940, 1430.822343046630067, 211.7813861080580011 ) ) ;
#39845 = CARTESIAN_POINT ( 'NONE',  ( -3.982247585420000124, 1360.759224656429978, 210.6218459616991936 ) ) ;
#39846 = ADVANCED_FACE ( 'NONE', ( #53295 ), #82136, .F. ) ;
#39847 = CARTESIAN_POINT ( 'NONE',  ( -4.623788007495000407, 1516.947419719950176, 205.6726967363569827 ) ) ;
#39849 = EDGE_CURVE ( 'NONE', #48271, #82569, #3994, .T. ) ;
#39848 = CARTESIAN_POINT ( 'NONE',  ( 19.53786426059019021, 1501.977400791986611, 181.5239794925693388 ) ) ;
#39850 = CARTESIAN_POINT ( 'NONE',  ( -32.20549126534956486, 1524.425415513989947, 216.0989951694419346 ) ) ;
#39851 = CARTESIAN_POINT ( 'NONE',  ( -4.221362096953909848, 1441.596168439879875, 170.5366494805969921 ) ) ;
#39853 = ORIENTED_EDGE ( 'NONE', *, *, #36136, .F. ) ;
#39852 = CARTESIAN_POINT ( 'NONE',  ( -68.69425754540708340, 1379.747748063760127, 280.2977437733629813 ) ) ;
#39854 = ORIENTED_EDGE ( 'NONE', *, *, #72068, .T. ) ;
#39855 = CARTESIAN_POINT ( 'NONE',  ( -17.43675326300159867, 1417.688629928019964, 206.2161178420579972 ) ) ;
#39856 = EDGE_LOOP ( 'NONE', ( #58781, #8908, #62370, #77585, #9239 ) ) ;
#39857 = CARTESIAN_POINT ( 'NONE',  ( 3.262212153180289675, 1484.802729046160039, 220.5136830109310040 ) ) ;
#39858 = CARTESIAN_POINT ( 'NONE',  ( 12.09108845230000107, 1500.238058980090045, 207.1892423451589877 ) ) ;
#39860 = CARTESIAN_POINT ( 'NONE',  ( 15.94106684230400184, 1410.432583999669760, 191.5989877904739842 ) ) ;
#39859 = CARTESIAN_POINT ( 'NONE',  ( -11.63960718312326748, 1425.863102008939904, 144.3731951731623440 ) ) ;
#39861 = CARTESIAN_POINT ( 'NONE',  ( -3.449647478144999724, 1516.829948096479939, 209.8791439064560223 ) ) ;
#39862 = EDGE_CURVE ( 'NONE', #65641, #83271, #15170, .T. ) ;
#39863 = CARTESIAN_POINT ( 'NONE',  ( -106.7579877504269916, 1378.913060387289988, 306.8343690171730032 ) ) ;
#39864 = CARTESIAN_POINT ( 'NONE',  ( 10.80507665935240169, 1480.918775577479892, 212.7532992060299932 ) ) ;
#39865 = DIRECTION ( 'NONE',  ( 1.000000000000000000, 0.000000000000000000, 0.000000000000000000 ) ) ;
#39866 = CARTESIAN_POINT ( 'NONE',  ( 34.54825073197359586, 1451.683981886209949, 134.0999999981819713 ) ) ;
#39867 = DIRECTION ( 'NONE',  ( 0.3363363969979660806, 0.9417419115949053898, 0.000000000000000000 ) ) ;
#39868 = VERTEX_POINT ( 'NONE', #28066 ) ;
#39869 = CARTESIAN_POINT ( 'NONE',  ( -2.775555821850000271, 1468.867611631090085, 187.4507004057990116 ) ) ;
#39870 = CARTESIAN_POINT ( 'NONE',  ( -3.666694481987490040, 1509.114858341099989, 179.5219341129400163 ) ) ;
#39871 = ORIENTED_EDGE ( 'NONE', *, *, #109651, .F. ) ;
#39872 = VERTEX_POINT ( 'NONE', #47088 ) ;
#39873 = CARTESIAN_POINT ( 'NONE',  ( 5.485270235611575451, 1410.482254480975371, 231.1776710310072644 ) ) ;
#39874 = CARTESIAN_POINT ( 'NONE',  ( -20.71343476517555615, 1524.726013923371283, 179.9059455038196802 ) ) ;
#39875 = APPLICATION_CONTEXT ( 'automotive_design' ) ;
#39876 = CARTESIAN_POINT ( 'NONE',  ( 0.1718821611349999889, 1452.986277132529949, 183.2483320761980110 ) ) ;
#39877 = CARTESIAN_POINT ( 'NONE',  ( -2.330134126681665752, 1515.193466806617153, 213.4479252923928243 ) ) ;
#39878 = CARTESIAN_POINT ( 'NONE',  ( -2.500000000000000000, 1439.624608411989811, 169.5728731851750126 ) ) ;
#39879 = CARTESIAN_POINT ( 'NONE',  ( -3.348647037815654315, 1523.530870145311155, 242.0864809827354520 ) ) ;
#39880 = CARTESIAN_POINT ( 'NONE',  ( 33.91369111058539687, 1451.728768197430099, 135.0591089875200055 ) ) ;
#39881 = CARTESIAN_POINT ( 'NONE',  ( -1.423096497750000022, 1465.102360927890004, 198.1952834721990087 ) ) ;
#39882 = EDGE_CURVE ( 'NONE', #110373, #5142, #16914, .T. ) ;
#39883 = CARTESIAN_POINT ( 'NONE',  ( 26.05603448480000139, 1437.546877748950010, 137.0232845100980228 ) ) ;
#39884 = CARTESIAN_POINT ( 'NONE',  ( 12.13987719790000064, 1415.426210663629945, 196.5375171025980023 ) ) ;
#39885 = CARTESIAN_POINT ( 'NONE',  ( -81.16297568175110655, 1384.800030316710036, 284.5901439566409863 ) ) ;
#39886 = EDGE_LOOP ( 'NONE', ( #24664, #60739, #51287, #48651 ) ) ;
#39887 = CARTESIAN_POINT ( 'NONE',  ( -5.005071046424999892, 1516.710692850270107, 201.7963041449669959 ) ) ;
#39888 = CARTESIAN_POINT ( 'NONE',  ( 4.028611221114998919, 1516.744381837270112, 207.9874879615069858 ) ) ;
#39889 = EDGE_LOOP ( 'NONE', ( #6138, #65966, #14752, #34729, #63140 ) ) ;
#39890 = CARTESIAN_POINT ( 'NONE',  ( 39.99774708740250162, 1440.913060387330006, 267.3729947719869529 ) ) ;
#39891 = CARTESIAN_POINT ( 'NONE',  ( -0.0002224978450532523575, 1452.169907037069606, 153.8711149815915462 ) ) ;
#39892 = ORIENTED_EDGE ( 'NONE', *, *, #55661, .T. ) ;
#39893 = CARTESIAN_POINT ( 'NONE',  ( -0.01304300853801059965, 1452.999749671699874, 183.2385070597169943 ) ) ;
#39894 = CARTESIAN_POINT ( 'NONE',  ( 8.186040751612090105, 1428.551989710240150, 213.9112982126329996 ) ) ;
#39895 = CARTESIAN_POINT ( 'NONE',  ( -5.013435694540000043, 1375.426148861440197, 209.1218459569879826 ) ) ;
#39896 = DIRECTION ( 'NONE',  ( -0.3090169943749515036, -0.000000000000000000, -0.9510565162951521989 ) ) ;
#39897 = CARTESIAN_POINT ( 'NONE',  ( -12.79518584150000038, 1426.055539333530078, 222.4327048618980029 ) ) ;
#39898 = CARTESIAN_POINT ( 'NONE',  ( -20.32975018110188259, 1508.870389951621746, 229.0186712996133735 ) ) ;
#39899 = CARTESIAN_POINT ( 'NONE',  ( 45.48702082709758798, 1436.948629695928048, 266.1936686269212942 ) ) ;
#39900 = CARTESIAN_POINT ( 'NONE',  ( -5.671687354363034395, 1510.518062792044475, 201.5738089661925017 ) ) ;
#39901 = CARTESIAN_POINT ( 'NONE',  ( -22.03465957474590908, 1522.382868172863937, 182.8300405912331144 ) ) ;
#39902 = EDGE_CURVE ( 'NONE', #44275, #78311, #28624, .T. ) ;
#39904 = CARTESIAN_POINT ( 'NONE',  ( -23.54657453824519919, 1420.952714651539964, 210.9134052879049648 ) ) ;
#39903 = CARTESIAN_POINT ( 'NONE',  ( 12.71492891619999988, 1463.042985206030153, 231.2054259453979910 ) ) ;
#39905 = DIRECTION ( 'NONE',  ( 0.000000000000000000, -0.9990482215818579093, -0.04361938736533144123 ) ) ;
#39906 = CARTESIAN_POINT ( 'NONE',  ( -7.716878941104999612, 1516.833976295079992, 216.4517711926369827 ) ) ;
#39907 = ORIENTED_EDGE ( 'NONE', *, *, #56606, .T. ) ;
#39908 = EDGE_CURVE ( 'NONE', #110254, #54705, #93822, .T. ) ;
#39909 = CARTESIAN_POINT ( 'NONE',  ( -10.22078022364619976, 1448.827725899079724, 207.2905427559460065 ) ) ;
#39910 = DIRECTION ( 'NONE',  ( 5.980589973904019347E-17, -1.000000000000000000, 1.736889445713099699E-16 ) ) ;
#39911 = CARTESIAN_POINT ( 'NONE',  ( 17.43217232700621722, 1448.245005021945417, 217.7414174091619259 ) ) ;
#39912 = CARTESIAN_POINT ( 'NONE',  ( 7.724423394095000894, 1517.122088787240045, 212.5760185856570104 ) ) ;
#39913 = CARTESIAN_POINT ( 'NONE',  ( 18.64061438810000126, 1509.327891197830013, 187.7640544359979913 ) ) ;
#39914 =( BOUNDED_CURVE ( )  B_SPLINE_CURVE ( 3, ( #49629, #41758, #33902, #8146 ),
 .UNSPECIFIED., .F., .F. ) 
 B_SPLINE_CURVE_WITH_KNOTS ( ( 4, 4 ),
 ( 1.006680279111034082, 2.134912272047150061 ),
 .UNSPECIFIED. ) 
 CURVE ( )  GEOMETRIC_REPRESENTATION_ITEM ( )  RATIONAL_B_SPLINE_CURVE ( ( 1.000000000000000000, 0.8967077198847258623, 0.8967077198847258623, 1.000000000000000000 ) ) 
 REPRESENTATION_ITEM ( '' )  );
#39915 = CARTESIAN_POINT ( 'NONE',  ( -11.60004869884502732, 1425.372347710274653, 138.1236363301591439 ) ) ;
#39917 = ORIENTED_EDGE ( 'NONE', *, *, #26110, .F. ) ;
#39916 = CARTESIAN_POINT ( 'NONE',  ( 3.802992195031519973, 1508.880967439349888, 213.6144902172630111 ) ) ;
#39918 = CARTESIAN_POINT ( 'NONE',  ( -17.19757137884673526, 1524.059547553519224, 237.3738383026851011 ) ) ;
#39919 = CARTESIAN_POINT ( 'NONE',  ( 25.66618467929999881, 1444.303020621219957, 221.6515381826980047 ) ) ;
#39920 = CARTESIAN_POINT ( 'NONE',  ( -11.84270513390000090, 1430.621905942929970, 150.1494318102980117 ) ) ;
#39921 = CARTESIAN_POINT ( 'NONE',  ( -1.315891021949999962, 1430.627222964690191, 214.6815279436889909 ) ) ;
#39922 = CARTESIAN_POINT ( 'NONE',  ( -68.77278092737650184, 1379.747928288920093, 280.3133413970129482 ) ) ;
#39923 = CARTESIAN_POINT ( 'NONE',  ( -5.329063471891149685E-15, 1428.868807534159941, 155.3340205489109849 ) ) ;
#39924 = CARTESIAN_POINT ( 'NONE',  ( 9.197260543180000525, 1420.703589484819986, 196.7538032495989739 ) ) ;
#39925 = ADVANCED_FACE ( 'NONE', ( #64451 ), #23136, .F. ) ;
#39926 = CARTESIAN_POINT ( 'NONE',  ( 12.84295322920000082, 1444.979964823190130, 186.6187016747979897 ) ) ;
#39928 = CARTESIAN_POINT ( 'NONE',  ( -20.24460045326980051, 1505.070898157219972, 209.5321939871419943 ) ) ;
#39927 = CARTESIAN_POINT ( 'NONE',  ( -18.38271312340000208, 1444.809750369289759, 226.8202415501980056 ) ) ;
#39929 = CARTESIAN_POINT ( 'NONE',  ( -2.496620389599999879, 1485.857485423129901, 182.3495326893979893 ) ) ;
#39930 = VERTEX_POINT ( 'NONE', #49843 ) ;
#39931 = CARTESIAN_POINT ( 'NONE',  ( 0.7360974386200019870, 1517.045004075700035, 205.0794574309270217 ) ) ;
#39932 = CARTESIAN_POINT ( 'NONE',  ( 9.769670128800001407, 1407.519369601530116, 269.6204844436979897 ) ) ;
#39933 = EDGE_CURVE ( 'NONE', #81697, #9577, #45074, .T. ) ;
#39934 = CARTESIAN_POINT ( 'NONE',  ( 0.5238745688090000741, 1409.870337461830104, 185.0929766115979760 ) ) ;
#39935 = CARTESIAN_POINT ( 'NONE',  ( 17.66554091740000132, 1410.882309102730005, 192.9158045799980243 ) ) ;
#39936 = CARTESIAN_POINT ( 'NONE',  ( 21.71754518174779491, 1429.404468804660610, 218.5691086971039283 ) ) ;
#39937 = CARTESIAN_POINT ( 'NONE',  ( 15.82489611782290240, 1509.465677942714137, 184.1612054350828203 ) ) ;
#39938 = CARTESIAN_POINT ( 'NONE',  ( -0.5021741993441900531, 1413.729074630699870, 233.3179678917850026 ) ) ;
#39939 = CARTESIAN_POINT ( 'NONE',  ( -10.32330663897819889, 1447.671776642609984, 209.9210912389999919 ) ) ;
#39940 = CARTESIAN_POINT ( 'NONE',  ( -2.307020840992839883, 1449.832034867059974, 154.5197370804639831 ) ) ;
#39941 = CARTESIAN_POINT ( 'NONE',  ( -12.42428048090000026, 1445.297595047380128, 186.7045969743979867 ) ) ;
#39942 = CARTESIAN_POINT ( 'NONE',  ( 1.462738438227520144, 1450.687750484019944, 155.0630772167459952 ) ) ;
#39943 = CARTESIAN_POINT ( 'NONE',  ( -14.20217057992160115, 1415.778512723650010, 221.1297441146029712 ) ) ;
#39944 = CARTESIAN_POINT ( 'NONE',  ( -10.21665424470000083, 1499.224423270490206, 214.5746271585690010 ) ) ;
#39945 = CARTESIAN_POINT ( 'NONE',  ( -7.991890656415680638, 1409.192143358779958, 196.4723718539459867 ) ) ;
#39946 = CARTESIAN_POINT ( 'NONE',  ( 10.72994439777698439, 1424.980258667470935, 138.6335552007459455 ) ) ;
#39947 = CARTESIAN_POINT ( 'NONE',  ( 3.696739103780000146, 1440.987872693469853, 157.0266763811980013 ) ) ;
#39948 = CARTESIAN_POINT ( 'NONE',  ( -4.933848679039999574, 1475.129223611229918, 269.4903295208979443 ) ) ;
#39949 = CARTESIAN_POINT ( 'NONE',  ( -4.235648567922631003, 1446.341758401669949, 163.6974501593520017 ) ) ;
#39950 = DIRECTION ( 'NONE',  ( 0.000000000000000000, -1.000000000000000000, 6.123233995736769734E-17 ) ) ;
#39951 = CARTESIAN_POINT ( 'NONE',  ( -14.91306988694542923, 1486.499853230188137, 185.9738472613629199 ) ) ;
#39952 = CARTESIAN_POINT ( 'NONE',  ( -58.27305785222070256, 1384.702705549079838, 277.9433341154070263 ) ) ;
#39953 = CARTESIAN_POINT ( 'NONE',  ( -29.86461515634900010, 1525.960063244516959, 220.9690070206027031 ) ) ;
#39954 = CARTESIAN_POINT ( 'NONE',  ( -17.60627216660330063, 1410.895669502700230, 193.4350316886979897 ) ) ;
#39955 = CARTESIAN_POINT ( 'NONE',  ( 12.14869142895439857, 1491.529512745250031, 207.2247900540259877 ) ) ;
#39956 = CARTESIAN_POINT ( 'NONE',  ( -19.98413504154930109, 1526.143142182166912, 184.9530087057032119 ) ) ;
#39957 = CARTESIAN_POINT ( 'NONE',  ( 25.78167222729700114, 1509.813387082529971, 195.1140727163279962 ) ) ;
#39958 = CARTESIAN_POINT ( 'NONE',  ( -19.22980863180000100, 1409.584580101929987, 199.6886479387179918 ) ) ;
#39959 = CARTESIAN_POINT ( 'NONE',  ( 2.500000000000000000, 1448.210448409899982, 182.3842139592889851 ) ) ;
#39960 = CARTESIAN_POINT ( 'NONE',  ( 10.92186379062459878, 1478.901561184230104, 206.2239204151590286 ) ) ;
#39961 = VERTEX_POINT ( 'NONE', #39778 ) ;
#39962 = CARTESIAN_POINT ( 'NONE',  ( -2.297865873822824145, 1410.371582420674713, 232.7246199332096239 ) ) ;
#39963 = CARTESIAN_POINT ( 'NONE',  ( -3.317807041231336485E-31, 1414.677402202029953, 209.1218459616989946 ) ) ;
#39964 = CARTESIAN_POINT ( 'NONE',  ( -19.04700360162490114, 1444.155872992060040, 199.5980005314840184 ) ) ;
#39966 = CARTESIAN_POINT ( 'NONE',  ( -14.83035617076499868, 1514.570049710740022, 192.8394949842669917 ) ) ;
#39965 = CARTESIAN_POINT ( 'NONE',  ( 11.72669663920000005, 1426.286371213729808, 143.4670320514979949 ) ) ;
#39967 = FACE_OUTER_BOUND ( 'NONE', #75467, .T. ) ;
#39968 = CARTESIAN_POINT ( 'NONE',  ( 10.94233749380000020, 1409.295175233830150, 190.2941314834980062 ) ) ;
#39969 = CARTESIAN_POINT ( 'NONE',  ( -5.735785620560000631, 1454.599929374689964, 201.6482604689090010 ) ) ;
#39970 = VECTOR ( 'NONE', #59519, 1000.000000000000000 ) ;
#39971 = EDGE_CURVE ( 'NONE', #50471, #101391, #85082, .T. ) ;
#39972 = CARTESIAN_POINT ( 'NONE',  ( 2.290256263724999908, 1517.170721208160103, 202.1706708033170230 ) ) ;
#39973 = CARTESIAN_POINT ( 'NONE',  ( 7.143956740810000205, 1426.607338919389804, 213.1092222816089929 ) ) ;
#39974 = CARTESIAN_POINT ( 'NONE',  ( -14.94707557629999961, 1464.413060387330006, 223.3779789887979916 ) ) ;
#39975 = CARTESIAN_POINT ( 'NONE',  ( 15.78436436263500120, 1512.151624459629829, 197.9925267198669872 ) ) ;
#39976 = FACE_BOUND ( 'NONE', #59428, .T. ) ;
#39977 = CARTESIAN_POINT ( 'NONE',  ( -25.65044697828639997, 1380.250345453750015, 213.2121384338130099 ) ) ;
#39978 = CARTESIAN_POINT ( 'NONE',  ( 20.00897032557049826, 1508.357423559000154, 229.1242640148969940 ) ) ;
#39980 = VERTEX_POINT ( 'NONE', #73387 ) ;
#39979 = CARTESIAN_POINT ( 'NONE',  ( 3.958649409925110163, 1508.551704408389924, 204.1347675188470134 ) ) ;
#39981 = ORIENTED_EDGE ( 'NONE', *, *, #55052, .F. ) ;
#39982 = CARTESIAN_POINT ( 'NONE',  ( -12.38667194039999941, 1397.378208682429886, 212.8773238670779904 ) ) ;
#39983 = CARTESIAN_POINT ( 'NONE',  ( -21.12354134859999988, 1409.814880802030075, 216.2513170893979861 ) ) ;
#39984 = ORIENTED_EDGE ( 'NONE', *, *, #28880, .F. ) ;
#39985 = CARTESIAN_POINT ( 'NONE',  ( -12.64444544987818020, 1445.030967319847377, 169.4649881375822247 ) ) ;
#39986 = CARTESIAN_POINT ( 'NONE',  ( 22.47005530878909241, 1509.697731202374825, 228.0526691234717873 ) ) ;
#39987 = CARTESIAN_POINT ( 'NONE',  ( -7.780733106055000903, 1512.320675624280057, 211.9528311838369916 ) ) ;
#39989 = CYLINDRICAL_SURFACE ( 'NONE', #63011, 1.999999999999999556 ) ;
#39988 = FACE_OUTER_BOUND ( 'NONE', #14912, .T. ) ;
#39990 = ADVANCED_FACE ( 'NONE', ( #109733 ), #38292, .T. ) ;
#39991 = CARTESIAN_POINT ( 'NONE',  ( 9.052748310100000140, 1449.229322941700048, 186.1672263551980109 ) ) ;
#39992 = CARTESIAN_POINT ( 'NONE',  ( -4.458786532230819333, 1463.138397474430121, 200.4163687677220196 ) ) ;
#39993 = CARTESIAN_POINT ( 'NONE',  ( 44.70565337623089874, 1440.913053082580063, 269.9105772721819676 ) ) ;
#39994 = CARTESIAN_POINT ( 'NONE',  ( 11.04255400179049929, 1396.298674870250125, 209.9401464633739920 ) ) ;
#39995 = CARTESIAN_POINT ( 'NONE',  ( 14.36283523568019937, 1416.196255300799976, 196.9494022668550031 ) ) ;
#39996 = CARTESIAN_POINT ( 'NONE',  ( 11.83663831039999970, 1430.188662621430012, 150.0176914616980071 ) ) ;
#39997 = CARTESIAN_POINT ( 'NONE',  ( 6.917574163163576095, 1509.156500478879025, 180.5619989194156005 ) ) ;
#39998 = VERTEX_POINT ( 'NONE', #7815 ) ;
#39999 = CARTESIAN_POINT ( 'NONE',  ( 13.00321027915850003, 1435.856774820759711, 150.7051697245010189 ) ) ;
#40000 = CARTESIAN_POINT ( 'NONE',  ( 21.83550407203923527, 1523.678648413191922, 234.9693198511250785 ) ) ;
#40001 = ORIENTED_EDGE ( 'NONE', *, *, #16691, .F. ) ;
#40002 = ORIENTED_EDGE ( 'NONE', *, *, #69911, .T. ) ;
#40003 = CARTESIAN_POINT ( 'NONE',  ( -6.466996272939999457, 1422.019461440550231, 192.0563668886989888 ) ) ;
#40004 = CARTESIAN_POINT ( 'NONE',  ( -15.42294715779999947, 1459.506347036930038, 230.2271999085980099 ) ) ;
#40005 = CARTESIAN_POINT ( 'NONE',  ( -108.4178825058906170, 1388.553815689287148, 310.3588190281001857 ) ) ;
#40006 = CARTESIAN_POINT ( 'NONE',  ( 2.292307230374999616, 1516.548716157039962, 216.0554627912370051 ) ) ;
#40007 = CARTESIAN_POINT ( 'NONE',  ( -12.33756948541939913, 1378.984672000980254, 209.5697532986669671 ) ) ;
#40008 = B_SPLINE_SURFACE_WITH_KNOTS ( 'NONE', 5, 5, ( 
 ( #106973, #37575, #12360, #54408, #72301, #71212 ),
 ( #72840, #30260, #64453, #98567, #21836, #106432 ),
 ( #11824, #105334, #80126, #28625, #29716, #64991 ),
 ( #30814, #98015, #63900, #5064, #47632, #45995 ),
 ( #21287, #90161, #81761, #62827, #71776, #39211 ),
 ( #73388, #107524, #105895, #99109, #3445, #56586 ) ),
 .UNSPECIFIED., .F., .F., .F.,
 ( 6, 6 ),
 ( 6, 6 ),
 ( 27.35438305753609711, 59.36386366779180435 ),
 ( -0.0006425587617316530107, 0.5000000000000000000 ),
 .UNSPECIFIED. ) ;
#40009 = ORIENTED_EDGE ( 'NONE', *, *, #34584, .F. ) ;
#40010 = CARTESIAN_POINT ( 'NONE',  ( -11.42324330920000008, 1503.135554566890050, 207.5366435103790081 ) ) ;
#40011 = CARTESIAN_POINT ( 'NONE',  ( 2.500000000000000000, 1448.563435859630090, 159.6568317789180185 ) ) ;
#40012 = CARTESIAN_POINT ( 'NONE',  ( -42.05438492420000074, 1380.117442312619914, 227.1521432528590196 ) ) ;
#40013 = CARTESIAN_POINT ( 'NONE',  ( -2.298048961635000165, 1516.764084769670262, 205.6764383981169715 ) ) ;
#40014 = VERTEX_POINT ( 'NONE', #93464 ) ;
#40015 = CARTESIAN_POINT ( 'NONE',  ( 7.332063939445000678, 1516.939491476980038, 209.1111146381379911 ) ) ;
#40016 = CARTESIAN_POINT ( 'NONE',  ( -8.890910552086271679, 1451.447161361959843, 206.5067915207390001 ) ) ;
#40017 = EDGE_CURVE ( 'NONE', #102115, #20461, #16736, .T. ) ;
#40018 = CARTESIAN_POINT ( 'NONE',  ( -19.01751557161993134, 1413.711985803739708, 269.3842094040881534 ) ) ;
#40019 = CARTESIAN_POINT ( 'NONE',  ( 6.013893971085000345, 1511.644799026709961, 217.0731095806869746 ) ) ;
#40020 = EDGE_CURVE ( 'NONE', #72991, #80364, #106393, .T. ) ;
#40022 = ORIENTED_EDGE ( 'NONE', *, *, #97876, .F. ) ;
#40021 = CARTESIAN_POINT ( 'NONE',  ( 0.2033579075311599815, 1416.218865267220053, 227.1056941053959974 ) ) ;
#40023 = CARTESIAN_POINT ( 'NONE',  ( 24.65284846710000011, 1440.998862877870124, 212.5088464049680113 ) ) ;
#40024 = CARTESIAN_POINT ( 'NONE',  ( -32.33429779520879777, 1440.913060389619886, 244.9699471617589950 ) ) ;
#40025 = CARTESIAN_POINT ( 'NONE',  ( -62.07136965400000150, 1384.687060561920134, 284.7656473558590164 ) ) ;
#40026 = FACE_OUTER_BOUND ( 'NONE', #102767, .T. ) ;
#40027 = EDGE_CURVE ( 'NONE', #27217, #35721, #77786, .T. ) ;
#40028 = CARTESIAN_POINT ( 'NONE',  ( 14.76285304363459794, 1412.136382785999785, 269.6387137786039716 ) ) ;
#40029 = CARTESIAN_POINT ( 'NONE',  ( 1.713317409674999903, 1516.660388280709867, 213.7298676393670291 ) ) ;
#40030 = EDGE_CURVE ( 'NONE', #73642, #86033, #28747, .T. ) ;
#40031 = CARTESIAN_POINT ( 'NONE',  ( 23.94662184079999889, 1410.398902072829969, 209.3165411815660093 ) ) ;
#40032 = CARTESIAN_POINT ( 'NONE',  ( 0.02095502431091895990, 1507.112669616160019, 237.3523204869388792 ) ) ;
#40033 = CARTESIAN_POINT ( 'NONE',  ( -1.693092047772239983, 1443.235800395060096, 218.9922115469449864 ) ) ;
#40034 = CARTESIAN_POINT ( 'NONE',  ( -11.60004869885203682, 1425.456763142306272, 136.9372401164825703 ) ) ;
#40035 = CARTESIAN_POINT ( 'NONE',  ( 0.7559394982620020187, 1516.972341476009888, 210.2438793621770117 ) ) ;
#40036 = CARTESIAN_POINT ( 'NONE',  ( -22.07680818022615910, 1523.847248782568613, 233.7985790283582901 ) ) ;
#40037 = CARTESIAN_POINT ( 'NONE',  ( 15.09682228229999978, 1409.610690924630035, 192.0685155598980032 ) ) ;
#40038 = FACE_BOUND ( 'NONE', #63461, .T. ) ;
#40040 = VERTEX_POINT ( 'NONE', #3025 ) ;
#40039 = CARTESIAN_POINT ( 'NONE',  ( -50.80916825539999593, 1386.657926508519949, 226.1996310703590041 ) ) ;
#40041 = CARTESIAN_POINT ( 'NONE',  ( -53.36249814381680068, 1385.102014360260227, 268.5762821108210119 ) ) ;
#40042 = CARTESIAN_POINT ( 'NONE',  ( 17.60627508980000044, 1410.895669370830092, 224.8086596393980017 ) ) ;
#40043 = DIRECTION ( 'NONE',  ( 0.8775825618903732028, 0.000000000000000000, 0.4794255386042021172 ) ) ;
#40044 =( BOUNDED_CURVE ( )  B_SPLINE_CURVE ( 3, ( #14941, #93313, #23891, #50770 ),
 .UNSPECIFIED., .F., .F. ) 
 B_SPLINE_CURVE_WITH_KNOTS ( ( 4, 4 ),
 ( 3.141592653589793116, 4.712388980384689674 ),
 .UNSPECIFIED. ) 
 CURVE ( )  GEOMETRIC_REPRESENTATION_ITEM ( )  RATIONAL_B_SPLINE_CURVE ( ( 1.000000000000000000, 0.8047378541243649375, 0.8047378541243649375, 1.000000000000000000 ) ) 
 REPRESENTATION_ITEM ( '' )  );
#40045 = CARTESIAN_POINT ( 'NONE',  ( -1.908953967214899405, 1494.973776298109669, 220.1229886510380140 ) ) ;
#40046 = CARTESIAN_POINT ( 'NONE',  ( 33.28034951413924603, 1512.187213306747481, 200.8029765415137717 ) ) ;
#40047 = CARTESIAN_POINT ( 'NONE',  ( 12.85698489369999997, 1421.301446356600081, 205.5386183585989954 ) ) ;
#40048 = CARTESIAN_POINT ( 'NONE',  ( -11.87823649874709986, 1433.207008023099888, 147.6493504979379736 ) ) ;
#40049 = AXIS2_PLACEMENT_3D ( 'NONE', #15048, #91227, #66057 ) ;
#40051 = CARTESIAN_POINT ( 'NONE',  ( -8.297772639310000642, 1384.896939720920045, 218.7035975184890049 ) ) ;
#40050 = CARTESIAN_POINT ( 'NONE',  ( 4.036119644515000715, 1516.647924054489977, 216.4458205765370167 ) ) ;
#40052 = CARTESIAN_POINT ( 'NONE',  ( -27.01380866140000236, 1450.681584507220123, 136.4483241423979791 ) ) ;
#40053 = CARTESIAN_POINT ( 'NONE',  ( 33.34040796508655546, 1523.342713519622293, 222.1177029624608110 ) ) ;
#40054 = ORIENTED_EDGE ( 'NONE', *, *, #82268, .T. ) ;
#40055 = CARTESIAN_POINT ( 'NONE',  ( 6.554151426245000245, 1516.906641539930206, 201.7900338461269882 ) ) ;
#40056 = EDGE_CURVE ( 'NONE', #11858, #44698, #100413, .T. ) ;
#40057 = CARTESIAN_POINT ( 'NONE',  ( -15.07517731296499974, 1511.972232048389969, 221.4259079178670220 ) ) ;
#40058 = ORIENTED_EDGE ( 'NONE', *, *, #16119, .F. ) ;
#40059 = CARTESIAN_POINT ( 'NONE',  ( 0.2288628776169999990, 1457.825816290129751, 228.9826145029980182 ) ) ;
#40060 = VECTOR ( 'NONE', #52718, 1000.000000000000114 ) ;
#40061 = CARTESIAN_POINT ( 'NONE',  ( 23.90525189569999753, 1446.959187819619956, 216.4132176579479960 ) ) ;
#40062 = CARTESIAN_POINT ( 'NONE',  ( 8.952338953416104417, 1437.015053605790399, 153.1552784082401786 ) ) ;
#40063 = EDGE_CURVE ( 'NONE', #41473, #85993, #62378, .T. ) ;
#40064 = CARTESIAN_POINT ( 'NONE',  ( 9.592729112698087590, 1425.412518091523225, 195.5100996857470932 ) ) ;
#40065 = CARTESIAN_POINT ( 'NONE',  ( 4.647891285400000072, 1467.686421235989883, 217.9474878197889893 ) ) ;
#40066 = CARTESIAN_POINT ( 'NONE',  ( 15.23801107490102247, 1420.745564912765531, 227.8424191170523443 ) ) ;
#40067 = CARTESIAN_POINT ( 'NONE',  ( 6.251976625090000184, 1423.636347555029943, 186.2373219085980054 ) ) ;
#40068 = CARTESIAN_POINT ( 'NONE',  ( -18.82070097289999921, 1425.548023863429989, 224.8286763900980247 ) ) ;
#40069 = CARTESIAN_POINT ( 'NONE',  ( 10.16029637529024399, 1488.802298484208677, 205.1479740240232275 ) ) ;
#40070 = CARTESIAN_POINT ( 'NONE',  ( -106.3702501619999907, 1389.389845767869929, 299.7163509613590122 ) ) ;
#40071 = CARTESIAN_POINT ( 'NONE',  ( 17.47858465850000087, 1445.355796517389990, 190.5483357571979752 ) ) ;
#40072 = CARTESIAN_POINT ( 'NONE',  ( -106.5052939700000110, 1391.913060387289988, 302.8727176574589635 ) ) ;
#40073 = CARTESIAN_POINT ( 'NONE',  ( -29.82992791574873337, 1462.373732266217303, 269.4690031617170121 ) ) ;
#40074 = ORIENTED_EDGE ( 'NONE', *, *, #105782, .F. ) ;
#40075 = CARTESIAN_POINT ( 'NONE',  ( 3.330134165755000097, 1515.051704408389924, 213.4516374609670208 ) ) ;
#40076 = CARTESIAN_POINT ( 'NONE',  ( -39.43000968072596635, 1423.549647405266114, 269.1442499132564876 ) ) ;
#40077 = CARTESIAN_POINT ( 'NONE',  ( 10.14180306839999801, 1422.829400496329981, 209.7690176243060023 ) ) ;
#40078 = CARTESIAN_POINT ( 'NONE',  ( 9.722207004026980570, 1428.114070666289763, 212.2005352792010058 ) ) ;
#40079 = CARTESIAN_POINT ( 'NONE',  ( -0.1544391217869999777, 1417.354636897429828, 235.2106466983979942 ) ) ;
#40080 = CARTESIAN_POINT ( 'NONE',  ( -12.88287017495675180, 1442.882806527179127, 186.3955768649811944 ) ) ;
#40081 = AXIS2_PLACEMENT_3D ( 'NONE', #39019, #83794, #41244 ) ;
#40082 = CARTESIAN_POINT ( 'NONE',  ( 4.500000000000000000, 1425.929641636930000, 183.3886486283980162 ) ) ;
#40083 = CARTESIAN_POINT ( 'NONE',  ( 5.400240006326249897, 1493.509531614239904, 218.8212082968839809 ) ) ;
#40084 = CARTESIAN_POINT ( 'NONE',  ( -2.372055168030982930, 1415.656490859390487, 232.9357013292204215 ) ) ;
#40085 = CARTESIAN_POINT ( 'NONE',  ( -15.08212675520640111, 1415.677402202029953, 207.7871099719839947 ) ) ;
#40086 = CARTESIAN_POINT ( 'NONE',  ( 18.80464302510000252, 1425.801049065629968, 225.6039134470979945 ) ) ;
#40087 = CARTESIAN_POINT ( 'NONE',  ( -12.77015161775204177, 1442.833871923525749, 169.4527266999588733 ) ) ;
#40089 = ORIENTED_EDGE ( 'NONE', *, *, #23541, .F. ) ;
#40088 = CARTESIAN_POINT ( 'NONE',  ( -15.09681984919999920, 1409.610690840030202, 226.1751760239980058 ) ) ;
#40090 = CARTESIAN_POINT ( 'NONE',  ( -103.3000534650000048, 1379.387642428310073, 303.1956711788589587 ) ) ;
#40091 = CARTESIAN_POINT ( 'NONE',  ( 12.89209530779459989, 1512.335564144490036, 224.3027625489149841 ) ) ;
#40092 = EDGE_LOOP ( 'NONE', ( #9144, #20018, #71301, #82952, #70487 ) ) ;
#40093 = EDGE_LOOP ( 'NONE', ( #97349, #1081, #11739, #106345 ) ) ;
#40094 = CARTESIAN_POINT ( 'NONE',  ( 16.67301258007090325, 1414.971349104640012, 208.8753071508930077 ) ) ;
#40095 = CYLINDRICAL_SURFACE ( 'NONE', #11686, 2.000000000000003553 ) ;
#40097 = CARTESIAN_POINT ( 'NONE',  ( 1.844551928739080138, 1456.521385733330135, 219.5817337447860211 ) ) ;
#40096 = CARTESIAN_POINT ( 'NONE',  ( 4.355885920510000453, 1455.333275423389978, 217.9418639333990200 ) ) ;
#40098 = CARTESIAN_POINT ( 'NONE',  ( -8.102264060359999576, 1447.655834216490121, 213.4872354334590057 ) ) ;
#40099 = CARTESIAN_POINT ( 'NONE',  ( -11.87899302940000013, 1433.117272603449919, 149.9761280929979819 ) ) ;
#40100 = DIRECTION ( 'NONE',  ( 9.156846217086110244E-47, -1.000000000000000000, 1.836970198721029688E-16 ) ) ;
#40101 = CARTESIAN_POINT ( 'NONE',  ( 17.41346973679999977, 1410.020394403929913, 224.1775087769979962 ) ) ;
#40102 = CARTESIAN_POINT ( 'NONE',  ( -25.85694180069999959, 1436.522598591890073, 136.9096217434980360 ) ) ;
#40103 = CARTESIAN_POINT ( 'NONE',  ( -14.68424190075857894, 1429.954736308614429, 222.0400034816578057 ) ) ;
#40104 = FACE_BOUND ( 'NONE', #70573, .T. ) ;
#40105 = CARTESIAN_POINT ( 'NONE',  ( 1.324218434260000077, 1452.129555781629961, 183.4093038337979920 ) ) ;
#40106 = CARTESIAN_POINT ( 'NONE',  ( 5.072810769355130311, 1362.944312259176513, 208.3718459617061285 ) ) ;
#40107 = CARTESIAN_POINT ( 'NONE',  ( -20.41791317763336622, 1509.743963675110081, 231.1018990513161668 ) ) ;
#40109 = EDGE_LOOP ( 'NONE', ( #106403, #70070, #86429, #53246 ) ) ;
#40108 = CARTESIAN_POINT ( 'NONE',  ( -1.656929189209940043E-09, 1413.545274745300048, 249.1207792992729821 ) ) ;
#40110 = EDGE_LOOP ( 'NONE', ( #15375, #95082, #59407, #15387 ) ) ;
#40111 = CARTESIAN_POINT ( 'NONE',  ( -11.85755111573270071, 1431.739894570919887, 149.9497684120179883 ) ) ;
#40112 = CARTESIAN_POINT ( 'NONE',  ( -13.90061082261569858, 1502.276449099379988, 227.4029592858559852 ) ) ;
#40113 = CARTESIAN_POINT ( 'NONE',  ( -7.240565274249999739, 1470.982841272730184, 269.3413375565979777 ) ) ;
#40114 = CARTESIAN_POINT ( 'NONE',  ( -2.389513320580931577, 1474.347589592441182, 219.1042510813949775 ) ) ;
#40115 = CARTESIAN_POINT ( 'NONE',  ( -103.5905391456986706, 1377.418846546389432, 309.5807788459800349 ) ) ;
#40116 = FACE_OUTER_BOUND ( 'NONE', #948, .T. ) ;
#40117 = CARTESIAN_POINT ( 'NONE',  ( 0.2487136076107180072, 1451.379526256489953, 182.5560867144160113 ) ) ;
#40118 = CARTESIAN_POINT ( 'NONE',  ( -8.617791468060000071, 1384.526991232059800, 199.8918045177789793 ) ) ;
#40119 = CARTESIAN_POINT ( 'NONE',  ( 9.905242068095489572, 1468.560492227489931, 207.6656469818879884 ) ) ;
#40120 = CARTESIAN_POINT ( 'NONE',  ( -3.060197654820000057, 1457.550371045389966, 218.5492501106489840 ) ) ;
#40121 = CARTESIAN_POINT ( 'NONE',  ( 9.842969107809999230, 1365.740588703660023, 207.6218459616989946 ) ) ;
#40122 = CARTESIAN_POINT ( 'NONE',  ( -39.51545107973109339, 1423.010726206650133, 266.3651880554039622 ) ) ;
#40123 = VERTEX_POINT ( 'NONE', #80807 ) ;
#40124 = CARTESIAN_POINT ( 'NONE',  ( 0.000000000000000000, 1518.913060387330006, 209.1218459616979999 ) ) ;
#40125 = B_SPLINE_SURFACE_WITH_KNOTS ( 'NONE', 5, 5, ( 
 ( #101988, #51614, #16862, #93585, #9045, #85749 ),
 ( #85195, #42656, #43219, #68432, #84643, #102534 ),
 ( #77368, #60584, #17980, #52175, #75172, #100881 ),
 ( #15758, #24175, #7396, #70648, #43761, #96925 ),
 ( #28609, #104766, #44323, #62809, #20192, #45435 ),
 ( #2338, #79037, #26960, #53281, #54390, #37002 ),
 ( #2883, #28050, #95810, #77913, #86858, #78467 ),
 ( #87420, #1780, #1219, #35917, #10150, #45977 ),
 ( #62240, #35354, #88523, #10716, #69541, #103662 ) ),
 .UNSPECIFIED., .F., .F., .F.,
 ( 6, 3, 6 ),
 ( 6, 6 ),
 ( 0.000000000000000000, 7.189919518870000026, 14.37983903770000005 ),
 ( 0.000000000000000000, 2.000000000000000000 ),
 .UNSPECIFIED. ) ;
#40126 = B_SPLINE_CURVE_WITH_KNOTS ( 'NONE', 3,
 ( #57259, #13548, #83515, #108731, #39877, #23615 ),
 .UNSPECIFIED., .F., .F.,
 ( 4, 2, 4 ),
 ( 0.000000000000000000, 0.5000000000000000000, 1.000000000000000000 ),
 .UNSPECIFIED. ) ;
#40127 = VECTOR ( 'NONE', #107494, 1000.000000000000000 ) ;
#40128 = ORIENTED_EDGE ( 'NONE', *, *, #58613, .T. ) ;
#40129 = ORIENTED_EDGE ( 'NONE', *, *, #52970, .F. ) ;
#40130 = CARTESIAN_POINT ( 'NONE',  ( 7.725372132234999967, 1517.158319634930194, 211.9946825927569876 ) ) ;
#40131 = CARTESIAN_POINT ( 'NONE',  ( -107.2899050854710055, 1379.886892357829993, 309.1794776302379546 ) ) ;
#40132 = CARTESIAN_POINT ( 'NONE',  ( -2.500000000000000000, 1434.141256042250006, 183.7754221751980026 ) ) ;
#40134 = CARTESIAN_POINT ( 'NONE',  ( -17.63951784556396163, 1419.668342365388753, 207.0221617922962878 ) ) ;
#40133 = CARTESIAN_POINT ( 'NONE',  ( 2.878693249144999466, 1516.766397346390022, 213.1495431961470217 ) ) ;
#40135 = CARTESIAN_POINT ( 'NONE',  ( -16.72084742370000043, 1440.439203200979819, 190.3227648696979770 ) ) ;
#40136 = AXIS2_PLACEMENT_3D ( 'NONE', #24819, #84198, #102631 ) ;
#40137 = CARTESIAN_POINT ( 'NONE',  ( -2.129012891770579508, 1450.054690635432507, 182.8874644828513283 ) ) ;
#40138 = B_SPLINE_SURFACE_WITH_KNOTS ( 'NONE', 5, 5, ( 
 ( #60597, #34261, #1231, #68443, #8496, #103103 ),
 ( #104228, #76270, #33698, #52189, #67893, #86319 ),
 ( #85763, #9603, #34813, #26405, #25286, #16874 ),
 ( #94159, #17428, #61164, #9061, #77380, #43773 ),
 ( #103676, #61702, #59487, #77924, #26975, #95280 ),
 ( #18543, #93597, #51080, #44338, #52737, #35931 ) ),
 .UNSPECIFIED., .F., .F., .F.,
 ( 6, 6 ),
 ( 6, 6 ),
 ( 132.5300310469999943, 134.7130480889999831 ),
 ( 0.000000000000000000, 0.5000000000000000000 ),
 .UNSPECIFIED. ) ;
#40139 = ORIENTED_EDGE ( 'NONE', *, *, #102056, .F. ) ;
#40140 = CARTESIAN_POINT ( 'NONE',  ( -26.21200917470000036, 1435.609253055569980, 136.1127715238980045 ) ) ;
#40141 = CARTESIAN_POINT ( 'NONE',  ( 3.452917022905000355, 1517.089216728169959, 202.1725802860869976 ) ) ;
#40142 = ADVANCED_FACE ( 'NONE', ( #70791 ), #65174, .T. ) ;
#40143 = B_SPLINE_SURFACE_WITH_KNOTS ( 'NONE', 5, 5, ( 
 ( #29908, #98773, #62464, #54061, #20950, #39975, #24796, #14210, #5269 ),
 ( #101510, #65745, #66857, #48396, #99862, #39424, #74150, #84176, #24263 ),
 ( #15305, #57361, #90924, #57898, #82539, #91485, #59001, #99308, #100966 ),
 ( #5835, #58443, #92571, #14765, #66313, #49497, #15842, #108281, #41636 ),
 ( #83622, #56787, #32678, #93129, #31568, #50047, #7474, #75791, #6919 ),
 ( #47830, #92033, #23159, #48952, #81963, #41075, #83083, #23713, #67410 ),
 ( #6376, #73601, #107731, #109943, #31016, #65196, #22582, #40522, #75253 ),
 ( #74700, #33221, #108831, #32128, #100430, #109402, #27048, #1296, #84722 ),
 ( #51144, #52809, #60107, #750, #9137, #70190, #76338, #26471, #33768 ) ),
 .UNSPECIFIED., .F., .F., .F.,
 ( 6, 3, 6 ),
 ( 6, 3, 6 ),
 ( 9.902195898180000455, 12.38020728900000123, 16.40090783169999966 ),
 ( 0.000000000000000000, 0.5000000000000000000, 1.000000000000000000 ),
 .UNSPECIFIED. ) ;
#40144 = FACE_OUTER_BOUND ( 'NONE', #97577, .T. ) ;
#40145 = CARTESIAN_POINT ( 'NONE',  ( 45.63712937690380755, 1440.913060387330006, 268.9747523971630017 ) ) ;
#40146 = CARTESIAN_POINT ( 'NONE',  ( 0.06764684832619999311, 1408.848989329930191, 194.7501694690980116 ) ) ;
#40147 = DIRECTION ( 'NONE',  ( -0.9455185755993178454, 0.000000000000000000, 0.3255681544571537578 ) ) ;
#40148 = CARTESIAN_POINT ( 'NONE',  ( -3.586209743369999980, 1396.221085749330086, 197.6373087627979714 ) ) ;
#40150 = EDGE_LOOP ( 'NONE', ( #74322, #108399, #25939, #12911 ) ) ;
#40149 = CARTESIAN_POINT ( 'NONE',  ( -7.940837552955301248, 1365.055256626819073, 209.6218459617148824 ) ) ;
#40151 = VERTEX_POINT ( 'NONE', #104904 ) ;
#40152 = CARTESIAN_POINT ( 'NONE',  ( -1.906499846882070084E-08, 1508.551704408389924, 209.1218459511669892 ) ) ;
#40153 = CARTESIAN_POINT ( 'NONE',  ( -29.36007807473448139, 1526.208281990539263, 220.5288989449499866 ) ) ;
#40154 = CARTESIAN_POINT ( 'NONE',  ( 10.89952677771999845, 1460.763933248429794, 208.1481502120179812 ) ) ;
#40155 = CARTESIAN_POINT ( 'NONE',  ( 2.836810703502730568, 1368.016923498806136, 210.6218459617142003 ) ) ;
#40156 = DIRECTION ( 'NONE',  ( 0.9125304618753961039, 0.000000000000000000, -0.4090087482554332632 ) ) ;
#40157 = CIRCLE ( 'NONE', #34807, 1.000010375718257460 ) ;
#40158 = CARTESIAN_POINT ( 'NONE',  ( 6.950833530105000158, 1517.156142772249950, 211.6057959108269984 ) ) ;
#40159 = CARTESIAN_POINT ( 'NONE',  ( -68.77190080519999071, 1379.747925807450201, 280.3125203366930123 ) ) ;
#40160 = CARTESIAN_POINT ( 'NONE',  ( 5.436747755899999923, 1437.112761795790220, 154.7095357218980212 ) ) ;
#40161 = EDGE_CURVE ( 'NONE', #83258, #1325, #4113, .T. ) ;
#40162 = CARTESIAN_POINT ( 'NONE',  ( -14.76761537580000017, 1430.144808017329979, 221.9970169696979667 ) ) ;
#40163 = CARTESIAN_POINT ( 'NONE',  ( 18.80463395749418609, 1425.801070877558004, 225.6039093632070376 ) ) ;
#40164 = CARTESIAN_POINT ( 'NONE',  ( 7.622960486734998931, 1511.191277613550028, 205.7361320510769929 ) ) ;
#40165 = CARTESIAN_POINT ( 'NONE',  ( -0.7579844201469989606, 1516.883361325900069, 206.8353730456769881 ) ) ;
#40166 = VERTEX_POINT ( 'NONE', #2477 ) ;
#40167 = DIRECTION ( 'NONE',  ( 0.9149707217702669482, 0.000000000000000000, 0.4035202328300239172 ) ) ;
#40168 = CARTESIAN_POINT ( 'NONE',  ( -11.15268071913589942, 1425.700850061899928, 101.7510819996820004 ) ) ;
#40169 = CIRCLE ( 'NONE', #51133, 1.999999999999999556 ) ;
#40170 = CARTESIAN_POINT ( 'NONE',  ( -19.36207330082412881, 1457.403296974644263, 226.2910419354238343 ) ) ;
#40171 = EDGE_LOOP ( 'NONE', ( #39432, #82182, #12869, #38022 ) ) ;
#40172 = CARTESIAN_POINT ( 'NONE',  ( -5.614653854145000622, 1512.956339156650074, 203.5071921160869977 ) ) ;
#40174 = EDGE_CURVE ( 'NONE', #77339, #47552, #29496, .T. ) ;
#40173 = CARTESIAN_POINT ( 'NONE',  ( -24.41826286173580840, 1509.769384798847341, 225.6085766216700677 ) ) ;
#40175 = CARTESIAN_POINT ( 'NONE',  ( -4.141637188104014378, 1439.809767520328933, 185.4878219303663229 ) ) ;
#40176 = CARTESIAN_POINT ( 'NONE',  ( -6.964057390120000690, 1413.857113999770036, 207.9404136278890007 ) ) ;
#40177 = CARTESIAN_POINT ( 'NONE',  ( 11.58478124470000026, 1415.063410489829948, 222.3466023727980030 ) ) ;
#40178 = CARTESIAN_POINT ( 'NONE',  ( 1.530052826864370052, 1452.704406626560058, 183.4894965714629791 ) ) ;
#40179 = CARTESIAN_POINT ( 'NONE',  ( 3.735758962120000248, 1487.094197141789891, 198.1822665823990235 ) ) ;
#40180 = CARTESIAN_POINT ( 'NONE',  ( 24.29980230545161746, 1445.714648955952498, 214.3234337815786716 ) ) ;
#40181 = CARTESIAN_POINT ( 'NONE',  ( -4.390466737189999691, 1449.947854720489886, 190.5483265708990075 ) ) ;
#40182 = FACE_OUTER_BOUND ( 'NONE', #2212, .T. ) ;
#40183 = CARTESIAN_POINT ( 'NONE',  ( -1.709384611084999950, 1517.224900789629828, 216.4615953054470197 ) ) ;
#40184 = ORIENTED_EDGE ( 'NONE', *, *, #94649, .F. ) ;
#40185 = CARTESIAN_POINT ( 'NONE',  ( 7.708854789774719940, 1516.527547774869845, 206.9824925634590045 ) ) ;
#40186 = DIRECTION ( 'NONE',  ( 0.9995237695669298983, 0.03085829012780005876, 1.050424002118616340E-06 ) ) ;
#40187 = CARTESIAN_POINT ( 'NONE',  ( -17.55780571682349844, 1508.551704408389924, 211.7873504713069792 ) ) ;
#40188 = CARTESIAN_POINT ( 'NONE',  ( 1.132427485120000064E-14, 1421.588970873729977, 90.97065375769790307 ) ) ;
#40189 = DIRECTION ( 'NONE',  ( -0.4090087482554183862, 0.000000000000000000, 0.9125304618754026542 ) ) ;
#40190 = ADVANCED_FACE ( 'NONE', ( #97063 ), #108605, .F. ) ;
#40191 = CARTESIAN_POINT ( 'NONE',  ( -0.04898095367366699787, 1508.952069630370033, 179.4017721621569876 ) ) ;
#40192 = CARTESIAN_POINT ( 'NONE',  ( -11.36241000037609972, 1471.019701088729789, 208.0608489626829964 ) ) ;
#40193 = CARTESIAN_POINT ( 'NONE',  ( -4.300067920883310357, 1508.175884720887780, 220.6014452582427339 ) ) ;
#40194 = CARTESIAN_POINT ( 'NONE',  ( 18.02093535799999913, 1424.326836137830014, 225.1991050518980160 ) ) ;
#40195 = CARTESIAN_POINT ( 'NONE',  ( 1.351404204432949729, 1456.215857334650082, 198.6335368618340169 ) ) ;
#40196 = CARTESIAN_POINT ( 'NONE',  ( 5.157704406284129827E-09, 1406.911841301380036, 222.1218459627310153 ) ) ;
#40197 = CARTESIAN_POINT ( 'NONE',  ( 34.82401208279389948, 1440.913060385709969, 250.5797988201090050 ) ) ;
#40199 = CARTESIAN_POINT ( 'NONE',  ( -5.742877853539999577, 1477.404484404390132, 219.2478600367990111 ) ) ;
#40198 = CARTESIAN_POINT ( 'NONE',  ( -9.899088691764880821, 1472.173087826980009, 211.4694681913989882 ) ) ;
#40200 = CARTESIAN_POINT ( 'NONE',  ( 12.93261679809999976, 1416.825245919230156, 221.7399671197980240 ) ) ;
#40201 = EDGE_LOOP ( 'NONE', ( #97333, #6312, #98853, #31996 ) ) ;
#40202 = ORIENTED_EDGE ( 'NONE', *, *, #56349, .F. ) ;
#40203 = AXIS2_PLACEMENT_3D ( 'NONE', #97317, #9453, #20587 ) ;
#40204 = CARTESIAN_POINT ( 'NONE',  ( 6.223484587698222548, 1441.168272379637301, 215.3989590944712234 ) ) ;
#40205 = CARTESIAN_POINT ( 'NONE',  ( -1.514738108749209999, 1507.606285622480073, 232.0384771855580084 ) ) ;
#40206 = CARTESIAN_POINT ( 'NONE',  ( -3.261844206600000184, 1443.084586291889991, 200.4064849727489843 ) ) ;
#40207 = CARTESIAN_POINT ( 'NONE',  ( 11.35583702168310083, 1503.040203525480138, 211.0426724955169959 ) ) ;
#40208 = CARTESIAN_POINT ( 'NONE',  ( -13.01671764799590036, 1416.842625005220043, 221.9093393807470136 ) ) ;
#40209 = AXIS2_PLACEMENT_3D ( 'NONE', #10164, #95824, #19092 ) ;
#40210 = CARTESIAN_POINT ( 'NONE',  ( 9.345710454894810226, 1422.635914553260136, 212.8840094578699791 ) ) ;
#40211 = CARTESIAN_POINT ( 'NONE',  ( -17.52327301342160126, 1415.836208884639973, 225.9446061863119724 ) ) ;
#40212 = CARTESIAN_POINT ( 'NONE',  ( 0.2964407352292510178, 1508.551704408389924, 219.9776655330169888 ) ) ;
#40213 = CARTESIAN_POINT ( 'NONE',  ( -41.29375914184250007, 1383.826143227880038, 244.0855120829130271 ) ) ;
#40214 = CARTESIAN_POINT ( 'NONE',  ( -15.93370838064100248, 1491.571823434650014, 224.2164500899540087 ) ) ;
#40215 = CARTESIAN_POINT ( 'NONE',  ( -251.6678281593879944, 1855.626960278319984, 173.9672998193020135 ) ) ;
#40216 = CARTESIAN_POINT ( 'NONE',  ( -12.07091066857769945, 1502.301112229150021, 208.9299697958410036 ) ) ;
#40217 = CARTESIAN_POINT ( 'NONE',  ( 10.61162123832369986, 1490.998599246300273, 212.0041548266819973 ) ) ;
#40219 = ORIENTED_EDGE ( 'NONE', *, *, #31563, .F. ) ;
#40218 = CARTESIAN_POINT ( 'NONE',  ( -0.1769726758110010123, 1455.698884654190124, 218.5933451010789952 ) ) ;
#40220 = CARTESIAN_POINT ( 'NONE',  ( -1.304523669740000225, 1451.773061479729904, 183.6942222515980063 ) ) ;
#40221 = CARTESIAN_POINT ( 'NONE',  ( -31.91391880200000131, 1384.560375756019766, 206.3213236589990061 ) ) ;
#40222 = CARTESIAN_POINT ( 'NONE',  ( 3.053241897432329655, 1508.551704408389924, 204.1980707054060247 ) ) ;
#40223 = ORIENTED_EDGE ( 'NONE', *, *, #53740, .F. ) ;
#40224 = ORIENTED_EDGE ( 'NONE', *, *, #33002, .T. ) ;
#40225 = CARTESIAN_POINT ( 'NONE',  ( -7.924974002880879276, 1385.447079371110021, 218.8285693757050012 ) ) ;
#40226 = CARTESIAN_POINT ( 'NONE',  ( -2.898099067781480187, 1515.492902831140100, 204.9850961401090217 ) ) ;
#40228 = CARTESIAN_POINT ( 'NONE',  ( 11.89193436271280113, 1434.276600485830159, 147.6498533937430011 ) ) ;
#40227 = CARTESIAN_POINT ( 'NONE',  ( -11.63679813930000151, 1439.363771630820111, 147.7934734181980048 ) ) ;
#40229 = CARTESIAN_POINT ( 'NONE',  ( -5.727657026459999301, 1464.121933083889871, 200.1990060710790260 ) ) ;
#40230 = CARTESIAN_POINT ( 'NONE',  ( -103.9810530660000012, 1379.936289390329875, 302.8711362071589974 ) ) ;
#40231 = FACE_OUTER_BOUND ( 'NONE', #217, .T. ) ;
#40232 = CARTESIAN_POINT ( 'NONE',  ( -15.83041352305280114, 1508.551704408389924, 214.0237305288890184 ) ) ;
#40233 = DIRECTION ( 'NONE',  ( 0.000000000000000000, 0.000000000000000000, 1.000000000000000000 ) ) ;
#40234 = CARTESIAN_POINT ( 'NONE',  ( 18.28846457996500163, 1425.324642923450028, 225.4724497386589803 ) ) ;
#40235 = DIRECTION ( 'NONE',  ( 1.755985294532469921E-16, -1.000000000000000000, 1.338183447452831989E-16 ) ) ;
#40236 = CARTESIAN_POINT ( 'NONE',  ( 7.319715941259939740, 1435.586172999379869, 204.5315301320030130 ) ) ;
#40237 = CARTESIAN_POINT ( 'NONE',  ( 10.96941897920000031, 1432.344069363209883, 151.7701285250979879 ) ) ;
#40238 = CARTESIAN_POINT ( 'NONE',  ( -2.545475536568049701, 1449.267405237600087, 183.6438597093680016 ) ) ;
#40239 = EDGE_LOOP ( 'NONE', ( #1766, #82991, #108841, #46116 ) ) ;
#40240 = AXIS2_PLACEMENT_3D ( 'NONE', #98252, #5300, #46783 ) ;
#40241 = CARTESIAN_POINT ( 'NONE',  ( 2.512783080302469774, 1509.132906964770200, 239.1218459480490139 ) ) ;
#40242 = CARTESIAN_POINT ( 'NONE',  ( 19.07243531070609777, 1456.493896479490104, 226.7047778378099849 ) ) ;
#40243 =( BOUNDED_CURVE ( )  B_SPLINE_CURVE ( 3, ( #10124, #19618, #85720, #95236 ),
 .UNSPECIFIED., .F., .T. ) 
 B_SPLINE_CURVE_WITH_KNOTS ( ( 4, 4 ),
 ( 4.150443908561925355, 5.274333949474359962 ),
 .UNSPECIFIED. ) 
 CURVE ( )  GEOMETRIC_REPRESENTATION_ITEM ( )  RATIONAL_B_SPLINE_CURVE ( ( 1.000000000000000000, 0.8974802273446612633, 0.8974802273446612633, 1.000000000000000000 ) ) 
 REPRESENTATION_ITEM ( '' )  );
#40244 = CARTESIAN_POINT ( 'NONE',  ( -12.12002620680000042, 1433.961363555340085, 150.1912452130979716 ) ) ;
#40245 = CARTESIAN_POINT ( 'NONE',  ( 8.296490667357130383E-11, 1466.080307989299854, 241.7690657028170165 ) ) ;
#40246 = CARTESIAN_POINT ( 'NONE',  ( -20.25904020392970040, 1496.820878093550164, 190.7097365830209981 ) ) ;
#40247 = DIRECTION ( 'NONE',  ( 0.000000000000000000, 0.000000000000000000, 1.000000000000000000 ) ) ;
#40248 = DIRECTION ( 'NONE',  ( -0.6906235817280228506, 0.2466512791305629781, 0.6798545541984799545 ) ) ;
#40249 = CIRCLE ( 'NONE', #92129, 30.00000000000000000 ) ;
#40250 = CARTESIAN_POINT ( 'NONE',  ( -0.5453392599249999861, 1476.674368370930097, 182.2373881275980239 ) ) ;
#40251 = CARTESIAN_POINT ( 'NONE',  ( -8.910387285859998840, 1362.858511851210096, 207.6218459616989946 ) ) ;
#40252 = CARTESIAN_POINT ( 'NONE',  ( -46.16777166034429314, 1440.913065320969963, 266.9714496862470128 ) ) ;
#40253 = CARTESIAN_POINT ( 'NONE',  ( -3.076366055149999834, 1424.853903601579987, 191.3970713258989917 ) ) ;
#40254 = CARTESIAN_POINT ( 'NONE',  ( -20.18543317628819977, 1451.730021516360011, 208.5438760233379867 ) ) ;
#40255 = CARTESIAN_POINT ( 'NONE',  ( 4.995623452895000760, 1516.636036526019780, 207.4092012159470073 ) ) ;
#40256 = CARTESIAN_POINT ( 'NONE',  ( 6.244762012776079452, 1407.784308379980075, 220.5925233722940106 ) ) ;
#40257 = CARTESIAN_POINT ( 'NONE',  ( 29.00779973304117831, 1526.382868172864164, 200.9494832830835378 ) ) ;
#40258 = B_SPLINE_SURFACE_WITH_KNOTS ( 'NONE', 5, 5, ( 
 ( #107897, #98395, #40146, #56967, #74329, #91099, #14377, #48570, #17671 ),
 ( #24429, #41797, #44022, #383, #84892, #69234, #51300, #94391, #16561 ),
 ( #85437, #8735, #67028, #101683, #59179, #24973, #7643, #76505, #75957 ),
 ( #25530, #78158, #42918, #103343, #17112, #26645, #43472, #77617, #33946 ),
 ( #51873, #77074, #110109, #93299, #33381, #102787, #60843, #59720, #101135 ),
 ( #86009, #60273, #34504, #50755, #8184, #929, #1470, #93840, #84352 ) ),
 .UNSPECIFIED., .F., .F., .F.,
 ( 6, 6 ),
 ( 6, 3, 6 ),
 ( 52.45005585730000064, 62.38124646570000209 ),
 ( 0.000000000000000000, 1.000000000000000000, 2.000000000000000000 ),
 .UNSPECIFIED. ) ;
#40259 = CARTESIAN_POINT ( 'NONE',  ( -15.72751745975079984, 1522.051704408389924, 211.3620530696679793 ) ) ;
#40260 = CARTESIAN_POINT ( 'NONE',  ( 7.376085248378010384, 1425.097779052370015, 212.5030054048039858 ) ) ;
#40261 = ORIENTED_EDGE ( 'NONE', *, *, #104271, .T. ) ;
#40262 = CARTESIAN_POINT ( 'NONE',  ( 39.40331993399999533, 1435.955742673169880, 259.1105269787980205 ) ) ;
#40263 = CARTESIAN_POINT ( 'NONE',  ( -27.70206559600000062, 1508.130759164429946, 205.9664600262279919 ) ) ;
#40265 = CARTESIAN_POINT ( 'NONE',  ( 4.363122647530000009, 1432.413060387330006, 146.1721969590979882 ) ) ;
#40264 = CARTESIAN_POINT ( 'NONE',  ( -0.5320368101529999727, 1499.383640133830113, 181.1599537584980055 ) ) ;
#40266 = CARTESIAN_POINT ( 'NONE',  ( -19.18813880309999931, 1465.797355387890093, 204.3301597990889888 ) ) ;
#40267 = CARTESIAN_POINT ( 'NONE',  ( -18.28167441760000145, 1423.284962468630056, 231.7606941460979897 ) ) ;
#40268 = CARTESIAN_POINT ( 'NONE',  ( -1.335447573599999993, 1487.231578949990080, 220.0114897263989917 ) ) ;
#40269 = CARTESIAN_POINT ( 'NONE',  ( -21.70213619864250276, 1452.155205091640028, 140.9573533261639966 ) ) ;
#40270 = EDGE_LOOP ( 'NONE', ( #101257, #85104 ) ) ;
#40271 = CARTESIAN_POINT ( 'NONE',  ( -5.360340255521029995, 1422.242729809129969, 144.1582390553999744 ) ) ;
#40272 = DIRECTION ( 'NONE',  ( 0.1403878024439506045, 0.9900965937346509760, 0.000000000000000000 ) ) ;
#40273 = FACE_OUTER_BOUND ( 'NONE', #17459, .T. ) ;
#40274 = CARTESIAN_POINT ( 'NONE',  ( -105.0428569062679145, 1378.913060387289988, 308.7873740373456144 ) ) ;
#40275 = ORIENTED_EDGE ( 'NONE', *, *, #28124, .F. ) ;
#40276 = ORIENTED_EDGE ( 'NONE', *, *, #16149, .F. ) ;
#40277 = CARTESIAN_POINT ( 'NONE',  ( -68.71403817000000913, 1384.980557972010047, 263.4288273180590068 ) ) ;
#40278 = CARTESIAN_POINT ( 'NONE',  ( -23.90704851129999753, 1410.421101986430131, 209.5356727241129988 ) ) ;
#40279 = ORIENTED_EDGE ( 'NONE', *, *, #56320, .F. ) ;
#40280 = CARTESIAN_POINT ( 'NONE',  ( 4.159863633235049818, 1508.728286123109910, 204.6953547332600181 ) ) ;
#40281 = CARTESIAN_POINT ( 'NONE',  ( -8.753854093810092607, 1516.720891557477444, 204.9704016331489811 ) ) ;
#40282 = CARTESIAN_POINT ( 'NONE',  ( -4.992349863779999453, 1391.620913471789891, 203.8075142969990168 ) ) ;
#40283 = CARTESIAN_POINT ( 'NONE',  ( -22.25208704810000171, 1415.845517319630062, 214.9433210100679901 ) ) ;
#40284 = ORIENTED_EDGE ( 'NONE', *, *, #29579, .T. ) ;
#40285 = EDGE_CURVE ( 'NONE', #42643, #76367, #94399, .T. ) ;
#40286 = CARTESIAN_POINT ( 'NONE',  ( 45.19053312608840400, 1446.052362190220265, 268.9873881031790006 ) ) ;
#40287 = AXIS2_PLACEMENT_3D ( 'NONE', #76586, #110737, #34028 ) ;
#40288 = CARTESIAN_POINT ( 'NONE',  ( -4.364191184633019915, 1509.032029208890208, 205.0059634122790158 ) ) ;
#40289 = CARTESIAN_POINT ( 'NONE',  ( -0.02608006148170000094, 1419.743832528429948, 184.3822973806979917 ) ) ;
#40290 = CARTESIAN_POINT ( 'NONE',  ( -4.040527342105000308, 1516.815231249920089, 204.5109077207270047 ) ) ;
#40291 = ORIENTED_EDGE ( 'NONE', *, *, #24196, .F. ) ;
#40292 = CARTESIAN_POINT ( 'NONE',  ( 12.53380745427929988, 1442.773887455719887, 186.4115735415020083 ) ) ;
#40293 = CARTESIAN_POINT ( 'NONE',  ( 15.08187215528230141, 1512.240709848920005, 196.4484943621689865 ) ) ;
#40294 = CARTESIAN_POINT ( 'NONE',  ( 12.96698787743724424, 1442.929322678499602, 187.1422095272347121 ) ) ;
#40295 = ORIENTED_EDGE ( 'NONE', *, *, #93471, .T. ) ;
#40296 = ORIENTED_EDGE ( 'NONE', *, *, #83249, .F. ) ;
#40297 = CARTESIAN_POINT ( 'NONE',  ( 3.932773640260000203, 1448.980696606500032, 184.2693352687979882 ) ) ;
#40299 = EDGE_CURVE ( 'NONE', #79128, #60672, #83702, .T. ) ;
#40298 = CARTESIAN_POINT ( 'NONE',  ( 26.83637367288270070, 1451.055154343129971, 136.3626532266509628 ) ) ;
#40300 = CARTESIAN_POINT ( 'NONE',  ( -13.31081197707080044, 1512.571279492550048, 193.8315606877860091 ) ) ;
#40301 = CARTESIAN_POINT ( 'NONE',  ( 3.605245751538479926, 1452.787162431489833, 152.2996838318599941 ) ) ;
#40302 = CARTESIAN_POINT ( 'NONE',  ( 10.42801528889999929, 1420.646855367029957, 197.8923855931989806 ) ) ;
#40303 = CARTESIAN_POINT ( 'NONE',  ( 0.2117397328861620187, 1431.756573977249900, 218.6125798781350227 ) ) ;
#40304 = CARTESIAN_POINT ( 'NONE',  ( -10.45765233029969998, 1492.595238526010007, 202.6675476240720002 ) ) ;
#40305 = CARTESIAN_POINT ( 'NONE',  ( -5.046753363489999700, 1496.785717051189977, 199.0711811026990006 ) ) ;
#40306 = CARTESIAN_POINT ( 'NONE',  ( 2.902343876856320115, 1466.632250330839952, 234.1422825383600070 ) ) ;
#40308 = DIRECTION ( 'NONE',  ( 1.836970198721029688E-16, 1.000000000000000000, -1.793662034335764721E-47 ) ) ;
#40307 = CARTESIAN_POINT ( 'NONE',  ( -16.69647987924599875, 1411.957873142359858, 191.7070286008739970 ) ) ;
#40309 = CARTESIAN_POINT ( 'NONE',  ( 2.801329332423560636, 1440.706061933215551, 170.5311005724319955 ) ) ;
#40310 = CARTESIAN_POINT ( 'NONE',  ( -24.03880222912709996, 1508.063415561920237, 222.3187217912339975 ) ) ;
#40311 = CARTESIAN_POINT ( 'NONE',  ( 0.1681681984982243971, 1405.973120458232188, 137.0999999980979851 ) ) ;
#40312 = EDGE_LOOP ( 'NONE', ( #5518, #46664, #72241, #110352, #28017 ) ) ;
#40313 = CARTESIAN_POINT ( 'NONE',  ( 9.562842933049999772, 1427.428384358229778, 219.6133831119979902 ) ) ;
#40314 = CARTESIAN_POINT ( 'NONE',  ( 3.203789175851970288E-09, 1424.294192408320214, 227.6053815985079893 ) ) ;
#40315 = CARTESIAN_POINT ( 'NONE',  ( -82.57267637850920039, 1384.987339562300122, 305.4358940477329725 ) ) ;
#40316 = VECTOR ( 'NONE', #62000, 1000.000000000000000 ) ;
#40317 = CARTESIAN_POINT ( 'NONE',  ( -8.716424698579999131, 1385.235525592430122, 199.8893934550389986 ) ) ;
#40318 = CARTESIAN_POINT ( 'NONE',  ( 10.68268295506589993, 1422.301575183460045, 211.2623176957549731 ) ) ;
#40320 = ORIENTED_EDGE ( 'NONE', *, *, #25538, .T. ) ;
#40319 = CARTESIAN_POINT ( 'NONE',  ( 11.10553610726389984, 1424.766439379950270, 203.0669930095579900 ) ) ;
#40321 = CARTESIAN_POINT ( 'NONE',  ( 2.113384585539999971, 1431.103683422689983, 218.3861821563190233 ) ) ;
#40322 = CARTESIAN_POINT ( 'NONE',  ( -1.650293394300000216, 1438.194204504490017, 150.5634062101979964 ) ) ;
#40323 = CARTESIAN_POINT ( 'NONE',  ( -7.595251018561734568, 1476.838993603164909, 216.1895794634047832 ) ) ;
#40324 = DIRECTION ( 'NONE',  ( 0.6709778558543625371, 0.000000000000000000, -0.7414773880254761362 ) ) ;
#40325 = CARTESIAN_POINT ( 'NONE',  ( 9.005216046220072101, 1434.097723414891789, 205.2808641047390665 ) ) ;
#40326 = CARTESIAN_POINT ( 'NONE',  ( 0.8608076301245028983, 1450.861566175740109, 181.3854559141449840 ) ) ;
#40327 = AXIS2_PLACEMENT_3D ( 'NONE', #43342, #77490, #36042 ) ;
#40328 = CARTESIAN_POINT ( 'NONE',  ( 0.6301902189002333010, 1467.066691292220639, 235.5390148699710835 ) ) ;
#40329 = CARTESIAN_POINT ( 'NONE',  ( -9.519812938348620079, 1460.017558366200092, 210.6311618255110147 ) ) ;
#40330 = CARTESIAN_POINT ( 'NONE',  ( 0.1681674884180490159, 1420.473121907760060, 182.7464979049940155 ) ) ;
#40331 = CARTESIAN_POINT ( 'NONE',  ( 11.41285014610000026, 1422.099025052029901, 229.8069411653980012 ) ) ;
#40332 = CARTESIAN_POINT ( 'NONE',  ( 13.02322703161950024, 1416.825784015089994, 221.6328457863429833 ) ) ;
#40333 = DIRECTION ( 'NONE',  ( 1.836970198721029688E-16, 1.000000000000000000, -2.953460612019999929E-19 ) ) ;
#40334 = CARTESIAN_POINT ( 'NONE',  ( -16.81208394469999945, 1409.500151295429987, 223.9875056278980026 ) ) ;
#40335 = CARTESIAN_POINT ( 'NONE',  ( -7.762930123710000352, 1492.073939571090023, 209.9113589376980258 ) ) ;
#40336 = CARTESIAN_POINT ( 'NONE',  ( 27.69925877688100258, 1441.434395746940027, 137.3015763641899980 ) ) ;
#40337 = CARTESIAN_POINT ( 'NONE',  ( -17.40901011393470199, 1410.017888045460040, 193.0747045748870221 ) ) ;
#40338 = CARTESIAN_POINT ( 'NONE',  ( 1.192550336225690098E-06, 1408.657067415270149, 195.1347666596020076 ) ) ;
#40339 = CARTESIAN_POINT ( 'NONE',  ( -0.7251570665222376588, 1526.278758871496848, 176.2636429491666945 ) ) ;
#40340 = CARTESIAN_POINT ( 'NONE',  ( 11.27339687608339958, 1433.557990205359829, 225.8166789818299947 ) ) ;
#40341 = CARTESIAN_POINT ( 'NONE',  ( -1.160956870409999953, 1414.971439108430104, 226.6888194207980121 ) ) ;
#40342 = CARTESIAN_POINT ( 'NONE',  ( 0.1701966656071439987, 1480.214123346120232, 182.0851929733079828 ) ) ;
#40344 = ORIENTED_EDGE ( 'NONE', *, *, #55584, .T. ) ;
#40343 = CARTESIAN_POINT ( 'NONE',  ( 5.012117609890212044, 1465.268517957009635, 200.5744003840434857 ) ) ;
#40345 = CARTESIAN_POINT ( 'NONE',  ( -24.49842486978874945, 1451.934881895486114, 137.2711189102183198 ) ) ;
#40346 = CARTESIAN_POINT ( 'NONE',  ( -33.28034951413921760, 1501.977400791986611, 217.4407153818824838 ) ) ;
#40347 = CARTESIAN_POINT ( 'NONE',  ( 12.91297502169999944, 1434.774370803509782, 149.0259275850980032 ) ) ;
#40348 = CARTESIAN_POINT ( 'NONE',  ( -40.21460569546650277, 1439.107902997820020, 134.0999999981339954 ) ) ;
#40349 = CARTESIAN_POINT ( 'NONE',  ( 3.846235792629999928, 1440.870317293109792, 184.3772602386979997 ) ) ;
#40350 = EDGE_LOOP ( 'NONE', ( #20957, #27801, #35031, #110648, #46789 ) ) ;
#40351 = CARTESIAN_POINT ( 'NONE',  ( -16.50400130224779360, 1525.907212628473644, 181.9890130758379030 ) ) ;
#40352 = DIRECTION ( 'NONE',  ( 0.7071067802247986700, -0.01693885153322989556, 0.7069038666387766900 ) ) ;
#40353 = CARTESIAN_POINT ( 'NONE',  ( -103.9934435520329572, 1380.191563112924086, 306.4628881227609440 ) ) ;
#40354 = CARTESIAN_POINT ( 'NONE',  ( -10.97842496009999991, 1492.884872791990119, 207.6491268858789851 ) ) ;
#40355 = CARTESIAN_POINT ( 'NONE',  ( 18.63567692469789705, 1430.070545818819937, 208.7560837280540227 ) ) ;
#40356 = CARTESIAN_POINT ( 'NONE',  ( 36.28172795142912577, 1420.161297467323493, 269.2207334997069665 ) ) ;
#40357 = CARTESIAN_POINT ( 'NONE',  ( 21.04915883790000208, 1471.323284331829882, 209.7080812325230283 ) ) ;
#40358 = CARTESIAN_POINT ( 'NONE',  ( -13.06039920679999966, 1380.082784840310069, 210.0204466537629742 ) ) ;
#40359 = CARTESIAN_POINT ( 'NONE',  ( -22.03465957474591619, 1522.382868172863937, 182.8300405912331144 ) ) ;
#40360 = CARTESIAN_POINT ( 'NONE',  ( -65.65150386709079555, 1385.090028818440032, 256.4968730652950057 ) ) ;
#40361 = CARTESIAN_POINT ( 'NONE',  ( -5.512208796550629231, 1374.913060387289988, 214.9365724502839896 ) ) ;
#40362 = CARTESIAN_POINT ( 'NONE',  ( -26.81029715973576444, 1436.081135210529737, 136.5370857271699663 ) ) ;
#40363 = EDGE_LOOP ( 'NONE', ( #23491, #45192, #67559, #18498 ) ) ;
#40364 = CARTESIAN_POINT ( 'NONE',  ( -29.47598808667450143, 1509.906165461940191, 208.6054833806550164 ) ) ;
#40365 = CARTESIAN_POINT ( 'NONE',  ( -16.01078298560119961, 1409.497709431180056, 225.5354710659109969 ) ) ;
#40367 = VERTEX_POINT ( 'NONE', #16340 ) ;
#40366 = DIRECTION ( 'NONE',  ( 0.000000000000000000, 0.000000000000000000, 1.000000000000000000 ) ) ;
#40368 = CARTESIAN_POINT ( 'NONE',  ( 3.984158188860000394, 1472.833767862289960, 218.5211933959089947 ) ) ;
#40370 = CARTESIAN_POINT ( 'NONE',  ( 9.968391131921531922, 1469.521124705179773, 210.4613160911150089 ) ) ;
#40369 = CIRCLE ( 'NONE', #75944, 2.000048419052109061 ) ;
#40371 = EDGE_CURVE ( 'NONE', #41801, #100706, #69564, .T. ) ;
#40372 = CARTESIAN_POINT ( 'NONE',  ( 23.95042262499999808, 1509.749427575030040, 225.5182035443980055 ) ) ;
#40373 = CARTESIAN_POINT ( 'NONE',  ( -109.4760068020000006, 1384.604117400059977, 311.2718567032590045 ) ) ;
#40374 = FACE_OUTER_BOUND ( 'NONE', #15606, .T. ) ;
#40375 = CARTESIAN_POINT ( 'NONE',  ( 0.8662027080590000150, 1465.087949259730067, 238.0466396433980094 ) ) ;
#40376 = EDGE_CURVE ( 'NONE', #94371, #87953, #101144, .T. ) ;
#40377 = CARTESIAN_POINT ( 'NONE',  ( 18.87422689890000171, 1410.495332323530192, 221.7757844262980029 ) ) ;
#40378 = CARTESIAN_POINT ( 'NONE',  ( -2.189223485552659998, 1414.936483310510084, 186.1778520092960036 ) ) ;
#40379 = ADVANCED_FACE ( 'NONE', ( #34820 ), #50538, .F. ) ;
#40380 = CARTESIAN_POINT ( 'NONE',  ( -17.73407118999999810, 1423.343216095329808, 226.1884512641980223 ) ) ;
#40381 = CARTESIAN_POINT ( 'NONE',  ( -3.000855178852367633, 1512.041030487102034, 201.2259107305448822 ) ) ;
#40382 = CARTESIAN_POINT ( 'NONE',  ( 24.05147185178290314, 1411.090383835510011, 208.4115470962599943 ) ) ;
#40383 = CARTESIAN_POINT ( 'NONE',  ( -125.0414468819076461, 1320.102705746891161, 297.8620945402992106 ) ) ;
#40384 = CARTESIAN_POINT ( 'NONE',  ( 7.326859461719999800, 1453.313060387329870, 227.7771414719979930 ) ) ;
#40385 = CARTESIAN_POINT ( 'NONE',  ( 7.877099145829999038, 1362.118768394180051, 210.6218459616991936 ) ) ;
#40386 = CARTESIAN_POINT ( 'NONE',  ( 7.322709686834999232, 1516.596789218710001, 205.8608388005369818 ) ) ;
#40387 = CARTESIAN_POINT ( 'NONE',  ( -5.490999923311999709, 1485.816407977019935, 182.9198330246910018 ) ) ;
#40388 = DIRECTION ( 'NONE',  ( 0.000000000000000000, 1.000000000000000000, 0.000000000000000000 ) ) ;
#40389 = CARTESIAN_POINT ( 'NONE',  ( -4.221515794169249602, 1441.604558287980126, 168.7334682647589830 ) ) ;
#40391 = ORIENTED_EDGE ( 'NONE', *, *, #15820, .T. ) ;
#40390 = CARTESIAN_POINT ( 'NONE',  ( -68.54637881447411019, 1379.747431728610081, 280.1644567549890326 ) ) ;
#40392 = ORIENTED_EDGE ( 'NONE', *, *, #106560, .T. ) ;
#40393 = CARTESIAN_POINT ( 'NONE',  ( -9.431129421125392653, 1380.292824618373061, 217.1402169329579692 ) ) ;
#40394 = ORIENTED_EDGE ( 'NONE', *, *, #38519, .T. ) ;
#40395 = CARTESIAN_POINT ( 'NONE',  ( 1.448679645196929933, 1507.129709964000085, 181.1126013477120011 ) ) ;
#40396 = AXIS2_PLACEMENT_3D ( 'NONE', #63390, #47658, #29201 ) ;
#40397 = CARTESIAN_POINT ( 'NONE',  ( -21.30585458279999855, 1410.903636193130069, 200.5893642190180231 ) ) ;
#40399 = CARTESIAN_POINT ( 'NONE',  ( 16.42012968119449923, 1410.579620556590044, 191.6756617717020106 ) ) ;
#40398 = CARTESIAN_POINT ( 'NONE',  ( 2.205156445730000137, 1428.435894572430016, 91.31218443469779800 ) ) ;
#40400 = CARTESIAN_POINT ( 'NONE',  ( 3.463767257884999839, 1517.014196759610059, 210.8246003415769962 ) ) ;
#40401 = CARTESIAN_POINT ( 'NONE',  ( 41.52362570818139886, 1442.051313831599828, 135.5055742887579981 ) ) ;
#40402 = CARTESIAN_POINT ( 'NONE',  ( -107.1548411235229992, 1378.913060387289988, 307.3968287292940431 ) ) ;
#40403 = CARTESIAN_POINT ( 'NONE',  ( 20.20959865099491992, 1501.977400791986611, 236.2316688286738611 ) ) ;
#40404 = CARTESIAN_POINT ( 'NONE',  ( 11.47334203980808276, 1464.061491388687273, 231.7760070827772552 ) ) ;
#40405 = DIRECTION ( 'NONE',  ( 0.000000000000000000, 0.000000000000000000, 1.000000000000000000 ) ) ;
#40406 = EDGE_CURVE ( 'NONE', #44333, #38120, #91836, .T. ) ;
#40408 = AXIS2_PLACEMENT_3D ( 'NONE', #89483, #107931, #21698 ) ;
#40407 = CARTESIAN_POINT ( 'NONE',  ( -30.90487439922522483, 1525.907212628473872, 216.4335774778785151 ) ) ;
#40409 = CYLINDRICAL_SURFACE ( 'NONE', #9592, 1.436538049339996181 ) ;
#40410 = CARTESIAN_POINT ( 'NONE',  ( -0.3862240863000029889, 1500.063269133189806, 233.1571802061990013 ) ) ;
#40411 = DIRECTION ( 'NONE',  ( 0.000000000000000000, 0.000000000000000000, -1.000000000000000000 ) ) ;
#40412 = VERTEX_POINT ( 'NONE', #60604 ) ;
#40413 = ORIENTED_EDGE ( 'NONE', *, *, #9898, .T. ) ;
#40414 = CARTESIAN_POINT ( 'NONE',  ( -2.155023191118941472, 1370.176848074955160, 211.3933356164083364 ) ) ;
#40415 = CARTESIAN_POINT ( 'NONE',  ( -17.59268554400000184, 1410.455475221230017, 194.0661810319979850 ) ) ;
#40416 = CARTESIAN_POINT ( 'NONE',  ( 0.02280772265270000071, 1450.912263924099989, 181.2411195727979702 ) ) ;
#40417 = CARTESIAN_POINT ( 'NONE',  ( -3.236612797780000328, 1484.261208539930067, 183.3592960838980161 ) ) ;
#40418 = CARTESIAN_POINT ( 'NONE',  ( -3.763781937373404052, 1369.097489338571904, 210.6218459616987957 ) ) ;
#40419 = CARTESIAN_POINT ( 'NONE',  ( 2.330134126090002145, 1515.499673595019885, 205.0355315948771988 ) ) ;
#40420 = B_SPLINE_CURVE_WITH_KNOTS ( 'NONE', 3,
 ( #78701, #42333, #2014, #77598 ),
 .UNSPECIFIED., .F., .F.,
 ( 4, 4 ),
 ( 0.000000000000000000, 1.000000000000000000 ),
 .UNSPECIFIED. ) ;
#40421 = B_SPLINE_CURVE_WITH_KNOTS ( 'NONE', 3,
 ( #32275, #92720, #7073, #59153 ),
 .UNSPECIFIED., .F., .F.,
 ( 4, 4 ),
 ( -47.20273799956279959, -29.43575841650000058 ),
 .UNSPECIFIED. ) ;
#40422 = CARTESIAN_POINT ( 'NONE',  ( -3.487592467065220081, 1508.551704408389924, 204.1347675093749956 ) ) ;
#40423 = CARTESIAN_POINT ( 'NONE',  ( 33.91369114129039986, 1435.681798693210112, 134.7402661674759941 ) ) ;
#40424 = CARTESIAN_POINT ( 'NONE',  ( 6.186741257861129384, 1516.987734611904671, 213.4228617371842063 ) ) ;
#40425 = DIRECTION ( 'NONE',  ( 1.836970198721029688E-16, 1.000000000000000000, 0.000000000000000000 ) ) ;
#40426 = CARTESIAN_POINT ( 'NONE',  ( 33.98103710425687041, 1443.913060387329324, 154.9319925572100942 ) ) ;
#40427 = CARTESIAN_POINT ( 'NONE',  ( -67.46733395234829800, 1384.720989913540052, 260.5131342236279579 ) ) ;
#40428 = ORIENTED_EDGE ( 'NONE', *, *, #33855, .F. ) ;
#40429 = CARTESIAN_POINT ( 'NONE',  ( 7.329303077985000137, 1516.857992118400034, 201.7912917986770083 ) ) ;
#40430 = CARTESIAN_POINT ( 'NONE',  ( -0.7559395363919990674, 1516.972341476009888, 207.9998125401569951 ) ) ;
#40431 = ORIENTED_EDGE ( 'NONE', *, *, #68566, .F. ) ;
#40432 = CARTESIAN_POINT ( 'NONE',  ( 41.55687132039510345, 1440.913060387330006, 269.1110027756790259 ) ) ;
#40433 = CARTESIAN_POINT ( 'NONE',  ( -0.0002577169993026165776, 1452.568168760216622, 153.5123052302506892 ) ) ;
#40434 = ORIENTED_EDGE ( 'NONE', *, *, #104226, .F. ) ;
#40435 = CARTESIAN_POINT ( 'NONE',  ( -0.3202584381410000236, 1451.681415889429900, 183.0549383082980057 ) ) ;
#40436 = ADVANCED_FACE ( 'NONE', ( #33705 ), #50019, .F. ) ;
#40437 = CARTESIAN_POINT ( 'NONE',  ( -15.35486504390000029, 1409.449264088030077, 192.1003565319979884 ) ) ;
#40438 = CARTESIAN_POINT ( 'NONE',  ( -16.79867715692278907, 1508.454973776049201, 213.5438332828385626 ) ) ;
#40439 = CARTESIAN_POINT ( 'NONE',  ( -9.457322321504838314, 1462.148587934049829, 206.2709873367270177 ) ) ;
#40440 = CARTESIAN_POINT ( 'NONE',  ( -4.474042835350000580, 1420.726059067829965, 186.3567251020980109 ) ) ;
#40441 = CARTESIAN_POINT ( 'NONE',  ( -5.384056492903469326, 1511.434805660039956, 200.4695677088149921 ) ) ;
#40442 = CARTESIAN_POINT ( 'NONE',  ( 7.054183505060000137, 1406.398142208129912, 266.9413180379979735 ) ) ;
#40443 = CARTESIAN_POINT ( 'NONE',  ( -12.06132760070000032, 1433.903324594730066, 147.1502524840979902 ) ) ;
#40444 = CARTESIAN_POINT ( 'NONE',  ( 26.86204993032690069, 1508.007394616730153, 206.2315948942269870 ) ) ;
#40446 = CARTESIAN_POINT ( 'NONE',  ( -10.75958976553603819, 1424.480348114876506, 137.8583268508966739 ) ) ;
#40445 = CARTESIAN_POINT ( 'NONE',  ( 16.31715900080000026, 1460.257358923430047, 229.2418418610980098 ) ) ;
#40447 = CARTESIAN_POINT ( 'NONE',  ( 6.639614474480000084, 1470.122678494290085, 210.8877727176889891 ) ) ;
#40448 = CARTESIAN_POINT ( 'NONE',  ( -5.003848160104999998, 1517.005755693489846, 216.4561742428970206 ) ) ;
#40449 = EDGE_LOOP ( 'NONE', ( #52859, #71504, #40828, #57233 ) ) ;
#40450 = CARTESIAN_POINT ( 'NONE',  ( 20.50000000000000000, 1442.773887286369927, 169.0968414572980123 ) ) ;
#40451 = CARTESIAN_POINT ( 'NONE',  ( -0.1001984567280549965, 1508.308975277190029, 180.4408595641159820 ) ) ;
#40452 = CARTESIAN_POINT ( 'NONE',  ( -4.682234856550000046, 1438.893385222290135, 227.1256850459990062 ) ) ;
#40453 = CARTESIAN_POINT ( 'NONE',  ( -1.120543735785000106, 1517.073005577650065, 213.1661658574570026 ) ) ;
#40454 = B_SPLINE_CURVE_WITH_KNOTS ( 'NONE', 3,
 ( #10353, #101217, #86511, #109650, #61900, #16113, #96017 ),
 .UNSPECIFIED., .F., .F.,
 ( 4, 3, 4 ),
 ( -20.59614224704469976, -18.01294953900849904, -15.04010021667880004 ),
 .UNSPECIFIED. ) ;
#40455 = CARTESIAN_POINT ( 'NONE',  ( 2.936817763032770312, 1515.374151778960140, 213.3816236606869836 ) ) ;
#40456 = CARTESIAN_POINT ( 'NONE',  ( -1.894502717228039979, 1483.831863175760191, 198.6119618997200007 ) ) ;
#40458 = EDGE_LOOP ( 'NONE', ( #101412, #105868, #74292, #27885, #38300, #59500 ) ) ;
#40457 = CARTESIAN_POINT ( 'NONE',  ( -12.10387469771020008, 1501.702042382700029, 211.4972372465589956 ) ) ;
#40459 = B_SPLINE_CURVE_WITH_KNOTS ( 'NONE', 3,
 ( #53767, #61597, #45354, #1689 ),
 .UNSPECIFIED., .F., .F.,
 ( 4, 4 ),
 ( 0.000000000000000000, 0.0002220129587134777205 ),
 .UNSPECIFIED. ) ;
#40460 = CARTESIAN_POINT ( 'NONE',  ( -1.191524307911313807, 1526.382868172864164, 179.0083900503168479 ) ) ;
#40461 = CARTESIAN_POINT ( 'NONE',  ( 3.303701760970000123, 1508.421385209789833, 219.9897194252990005 ) ) ;
#40462 = CARTESIAN_POINT ( 'NONE',  ( -11.29829825160000034, 1432.080963479299953, 151.5184116568979960 ) ) ;
#40463 = CARTESIAN_POINT ( 'NONE',  ( 2.448891952219999890, 1435.321209562490139, 227.4386027112989836 ) ) ;
#40464 = CARTESIAN_POINT ( 'NONE',  ( -61.49666415160000099, 1379.841752510579909, 267.0938153646590649 ) ) ;
#40465 = CARTESIAN_POINT ( 'NONE',  ( 6.305024129259999555, 1422.156209412130011, 144.1468801376980196 ) ) ;
#40466 = B_SPLINE_CURVE_WITH_KNOTS ( 'NONE', 3,
 ( #103026, #59966, #52658, #25767, #35290, #95200, #17351, #93527, #94638, #34186, #84583, #75657, #8980, #61085, #34736, #69476, #52109, #50459, #41497, #26896, #110341, #18461, #109797, #7874, #42042, #26323, #25210, #17913, #33613, #67266, #7333, #67810, #77308, #94081, #101924, #43151, #51546, #102478, #33075, #76194, #59415, #606, #24648, #101358, #103596, #86239, #58850, #92982, #16796, #16256, #51000, #85131, #8418, #85683 ),
 .UNSPECIFIED., .F., .F.,
 ( 4, 2, 2, 1, 1, 1, 1, 1, 2, 2, 2, 2, 1, 1, 1, 1, 1, 2, 2, 2, 2, 1, 1, 1, 1, 1, 2, 2, 2, 2, 1, 1, 1, 2, 2, 4 ),
 ( 0.000000000000000000, 0.1250000000035015324, 0.1875000000052515492, 0.2187500000061264882, 0.2343750000065650818, 0.2421875000067657546, 0.2460937500068673678, 0.2480468750069194372, 0.2490234375069441952, 0.2500000000069689809, 0.3750000000063240524, 0.4375000000060016991, 0.4687500000058259508, 0.4843750000057260863, 0.4921875000056777916, 0.4960937500056679661, 0.4980468750056630256, 0.4990234375056590843, 0.5000000000056551430, 0.6250000000030080383, 0.6875000000016828761, 0.7187500000010204060, 0.7343750000006781242, 0.7421875000004977130, 0.7460937500003983480, 0.7480468750003566036, 0.7490234375003448353, 0.7500000000003329559, 0.8125000000003542722, 0.8437500000003754774, 0.8593750000003955725, 0.8671875000003966827, 0.8710937500003971268, 0.8730468750003963496, 0.8750000000003955725, 1.000000000000000000 ),
 .UNSPECIFIED. ) ;
#40467 = DIRECTION ( 'NONE',  ( 0.000000000000000000, 1.000000000000000000, 0.000000000000000000 ) ) ;
#40468 = CARTESIAN_POINT ( 'NONE',  ( 12.44069282309999913, 1446.394401557849960, 188.1775352768979701 ) ) ;
#40469 = ADVANCED_FACE ( 'NONE', ( #38127 ), #20530, .T. ) ;
#40471 = LINE ( 'NONE', #14714, #99809 ) ;
#40470 = CARTESIAN_POINT ( 'NONE',  ( -20.21251411980000157, 1470.087779964230094, 225.9614712067979951 ) ) ;
#40472 = CARTESIAN_POINT ( 'NONE',  ( 19.37001854000000023, 1457.793959969789967, 211.0198531007490033 ) ) ;
#40473 = ORIENTED_EDGE ( 'NONE', *, *, #44865, .F. ) ;
#40474 = CARTESIAN_POINT ( 'NONE',  ( -2.492130661305000050, 1516.778761582560037, 205.6761608547170113 ) ) ;
#40475 = CARTESIAN_POINT ( 'NONE',  ( 3.744464175900000136, 1406.377798150230092, 269.2893938024980116 ) ) ;
#40476 = EDGE_CURVE ( 'NONE', #96461, #48130, #69066, .T. ) ;
#40477 = CARTESIAN_POINT ( 'NONE',  ( 0.08329622130249998702, 1408.915969163729869, 186.0161422112979892 ) ) ;
#40478 = DIRECTION ( 'NONE',  ( -0.1141463326676888657, -0.5076720045192847364, -0.8539553563072771469 ) ) ;
#40479 = AXIS2_PLACEMENT_3D ( 'NONE', #23877, #109568, #92750 ) ;
#40480 = VECTOR ( 'NONE', #99015, 1000.000000000000114 ) ;
#40481 = CARTESIAN_POINT ( 'NONE',  ( 22.78255286321940076, 1431.711273479132842, 216.5513474728326457 ) ) ;
#40482 = CARTESIAN_POINT ( 'NONE',  ( -8.894733913401703163, 1388.790479115094513, 217.7593060885732825 ) ) ;
#40483 = CARTESIAN_POINT ( 'NONE',  ( 26.63183758487663155, 1507.995768146901355, 215.9641994103228058 ) ) ;
#40484 = LINE ( 'NONE', #50554, #12092 ) ;
#40485 = CARTESIAN_POINT ( 'NONE',  ( -1.174890917327530149, 1450.814461561099961, 154.7899053676320023 ) ) ;
#40486 = CARTESIAN_POINT ( 'NONE',  ( -1.556661572576635955, 1451.024750845122753, 183.5973180285813271 ) ) ;
#40487 = CARTESIAN_POINT ( 'NONE',  ( -17.49001816009999999, 1408.913060387329779, 212.4168409189479974 ) ) ;
#40488 = DIRECTION ( 'NONE',  ( 0.02617694830785712717, 0.9996573249755577040, 1.162500616384811670E-17 ) ) ;
#40489 = CARTESIAN_POINT ( 'NONE',  ( 5.277460848200000498, 1426.742654866309977, 191.8370381630989812 ) ) ;
#40490 = CARTESIAN_POINT ( 'NONE',  ( -10.13264865422269878, 1409.266900275340049, 198.1207111944070220 ) ) ;
#40491 = CARTESIAN_POINT ( 'NONE',  ( 20.46625090740818109, 1507.818616722226807, 228.4183586287386447 ) ) ;
#40492 = CARTESIAN_POINT ( 'NONE',  ( 3.116763890020000094, 1441.234358967379876, 170.5448746976979919 ) ) ;
#40493 = CARTESIAN_POINT ( 'NONE',  ( -1.779266724299999991, 1476.084642096830066, 267.8527211508980486 ) ) ;
#40494 = CARTESIAN_POINT ( 'NONE',  ( -11.19904275380046599, 1425.025785267508354, 138.1878544111817462 ) ) ;
#40495 = CARTESIAN_POINT ( 'NONE',  ( -17.60627216660330063, 1410.895669502700230, 193.4350316886979897 ) ) ;
#40496 = EDGE_CURVE ( 'NONE', #69919, #44698, #102773, .T. ) ;
#40497 = DIRECTION ( 'NONE',  ( -0.9980318515193558060, 0.000000000000000000, -0.06270903725019710828 ) ) ;
#40498 = CARTESIAN_POINT ( 'NONE',  ( -47.50847041448220409, 1384.752078445960024, 256.6134531784289834 ) ) ;
#40499 = CARTESIAN_POINT ( 'NONE',  ( -106.7778451161910169, 1391.913060387289988, 302.2346433575910396 ) ) ;
#40500 = CARTESIAN_POINT ( 'NONE',  ( -20.87069991009999725, 1506.658021081189872, 214.5368842940590071 ) ) ;
#40501 = CARTESIAN_POINT ( 'NONE',  ( 2.760778564396810353, 1409.009468899150079, 230.1977509304229841 ) ) ;
#40502 = CARTESIAN_POINT ( 'NONE',  ( 0.000000000000000000, 1518.913060387330006, 209.1218459616979999 ) ) ;
#40503 = CARTESIAN_POINT ( 'NONE',  ( 7.445037983834265738, 1508.731359867039373, 203.6084103738589022 ) ) ;
#40504 = EDGE_CURVE ( 'NONE', #77737, #22920, #28632, .T. ) ;
#40505 = CARTESIAN_POINT ( 'NONE',  ( -22.38836670029999709, 1410.616270142430039, 203.1479786175279969 ) ) ;
#40506 = ADVANCED_FACE ( 'NONE', ( #55502 ), #89081, .T. ) ;
#40507 = CARTESIAN_POINT ( 'NONE',  ( 12.89505231660000106, 1420.989630775359956, 203.4267439564690108 ) ) ;
#40508 = CARTESIAN_POINT ( 'NONE',  ( -3.298498094659999769, 1407.650947899530138, 270.1377426963979929 ) ) ;
#40509 = ORIENTED_EDGE ( 'NONE', *, *, #83167, .F. ) ;
#40510 = CARTESIAN_POINT ( 'NONE',  ( 31.32995031131198616, 1523.678648413191695, 221.9013357025044115 ) ) ;
#40511 = CARTESIAN_POINT ( 'NONE',  ( -13.59430914469499996, 1507.912413286850096, 209.4080442005970042 ) ) ;
#40512 = CARTESIAN_POINT ( 'NONE',  ( 10.37958006579530057, 1453.090549329029727, 190.0119551464189840 ) ) ;
#40514 = CARTESIAN_POINT ( 'NONE',  ( -12.24109810896139905, 1378.509644311850025, 210.6652527242490009 ) ) ;
#40513 = DIRECTION ( 'NONE',  ( -0.7067700363771036720, 0.03085824620770448792, -0.7067700363771036720 ) ) ;
#40515 = CARTESIAN_POINT ( 'NONE',  ( 16.49279218151955462, 1525.408327360769590, 236.9553615728405589 ) ) ;
#40516 = CARTESIAN_POINT ( 'NONE',  ( -7.065869411249059873, 1517.051704406860154, 205.0465358202790185 ) ) ;
#40517 = CARTESIAN_POINT ( 'NONE',  ( -29.00779973304142345, 1526.382868172863937, 200.9494832830838789 ) ) ;
#40518 = EDGE_CURVE ( 'NONE', #101372, #23634, #23613, .T. ) ;
#40519 = CARTESIAN_POINT ( 'NONE',  ( -2.292307268505000106, 1516.548716157039962, 202.1882291110970300 ) ) ;
#40520 = CARTESIAN_POINT ( 'NONE',  ( -8.788663597526685578, 1511.593711396709296, 215.1384066147768976 ) ) ;
#40521 = CARTESIAN_POINT ( 'NONE',  ( -9.534219445089998857, 1428.030197386430018, 144.1938086916980239 ) ) ;
#40522 = CARTESIAN_POINT ( 'NONE',  ( 16.51584604633499964, 1514.088841912139969, 194.6296875079669917 ) ) ;
#40523 = CARTESIAN_POINT ( 'NONE',  ( -23.17200737914519948, 1417.287767808789795, 209.8650901584490214 ) ) ;
#40524 = CARTESIAN_POINT ( 'NONE',  ( -3.771520279010110333, 1379.944275571289836, 211.0169301715230006 ) ) ;
#40525 = CARTESIAN_POINT ( 'NONE',  ( 20.85715114138509918, 1508.960603666100042, 227.8108728366430000 ) ) ;
#40526 = EDGE_CURVE ( 'NONE', #104582, #36010, #97441, .T. ) ;
#40529 = EDGE_LOOP ( 'NONE', ( #103987, #42079, #31117, #82167, #50797 ) ) ;
#40528 = CARTESIAN_POINT ( 'NONE',  ( -48.00211451008600250, 1379.678745322079976, 241.5445238333160205 ) ) ;
#40527 = CIRCLE ( 'NONE', #69169, 24.33258347882036432 ) ;
#40530 = ORIENTED_EDGE ( 'NONE', *, *, #83719, .F. ) ;
#40531 = CARTESIAN_POINT ( 'NONE',  ( 11.85650668279999920, 1434.045051391929974, 150.8704278162979904 ) ) ;
#40532 = CARTESIAN_POINT ( 'NONE',  ( -7.937424474279999309, 1397.838828921930144, 219.9794736354980103 ) ) ;
#40533 = CARTESIAN_POINT ( 'NONE',  ( -19.24584652619999758, 1409.749709703130065, 221.2367099497979837 ) ) ;
#40534 = ORIENTED_EDGE ( 'NONE', *, *, #92242, .F. ) ;
#40535 = CARTESIAN_POINT ( 'NONE',  ( -13.31737298010640380, 1444.561816739103051, 169.3769464296262299 ) ) ;
#40536 = CARTESIAN_POINT ( 'NONE',  ( 22.33114268944675018, 1509.698422332540986, 228.3716627733444113 ) ) ;
#40537 = CARTESIAN_POINT ( 'NONE',  ( -7.683494276754999852, 1512.058324472099912, 211.8336161652269993 ) ) ;
#40539 = CARTESIAN_POINT ( 'NONE',  ( 17.85825448869999832, 1419.057470054430041, 225.0456301946979920 ) ) ;
#40538 = CARTESIAN_POINT ( 'NONE',  ( -8.297292677919999804, 1384.885217424229950, 218.7035352471990279 ) ) ;
#40540 = EDGE_CURVE ( 'NONE', #64221, #53037, #47640, .T. ) ;
#40541 = CARTESIAN_POINT ( 'NONE',  ( 14.44949573220000083, 1468.697490635830036, 188.3306200720979859 ) ) ;
#40542 = CARTESIAN_POINT ( 'NONE',  ( -7.191821496720000262, 1414.913060387229962, 194.0837811316980037 ) ) ;
#40543 = CARTESIAN_POINT ( 'NONE',  ( -17.00797328670000397, 1417.537217351680056, 207.7155449971589860 ) ) ;
#40545 = EDGE_CURVE ( 'NONE', #89981, #12260, #39687, .T. ) ;
#40544 = CARTESIAN_POINT ( 'NONE',  ( 10.54395425458129942, 1396.281263384510112, 205.7609669223470235 ) ) ;
#40546 = CARTESIAN_POINT ( 'NONE',  ( 1.149035020129999918, 1415.140114695929924, 191.3456881844979875 ) ) ;
#40547 = CARTESIAN_POINT ( 'NONE',  ( 11.22829442119999932, 1427.193422228129975, 149.5441094775980275 ) ) ;
#40548 = CARTESIAN_POINT ( 'NONE',  ( 7.515087040108598515, 1509.176409119497976, 180.7408218922122387 ) ) ;
#40549 = ORIENTED_EDGE ( 'NONE', *, *, #54943, .F. ) ;
#40550 = CARTESIAN_POINT ( 'NONE',  ( 12.96456176665079951, 1434.782329531799860, 149.4767548373170030 ) ) ;
#40551 = ORIENTED_EDGE ( 'NONE', *, *, #97914, .T. ) ;
#40552 = ADVANCED_FACE ( 'NONE', ( #23520 ), #30823, .T. ) ;
#40553 = VERTEX_POINT ( 'NONE', #39787 ) ;
#40554 = CARTESIAN_POINT ( 'NONE',  ( -18.04049389182639729, 1478.103586370280027, 228.8030285101139896 ) ) ;
#40555 = CARTESIAN_POINT ( 'NONE',  ( -4.153219689960000238, 1466.619231579529924, 234.7255339115979780 ) ) ;
#40556 = CARTESIAN_POINT ( 'NONE',  ( -12.78671360849999772, 1416.817366564930126, 196.1060123485979716 ) ) ;
#40557 = CARTESIAN_POINT ( 'NONE',  ( -3.258474617075000079, 1517.083030555940013, 215.6838419306269827 ) ) ;
#40558 = CARTESIAN_POINT ( 'NONE',  ( -12.31949145670699863, 1378.253786499809848, 209.5105070175480080 ) ) ;
#40559 = EDGE_CURVE ( 'NONE', #9383, #39203, #81760, .T. ) ;
#40560 = ORIENTED_EDGE ( 'NONE', *, *, #3535, .F. ) ;
#40561 = CARTESIAN_POINT ( 'NONE',  ( -11.38797607120000066, 1501.230572076990029, 208.0053829869090123 ) ) ;
#40562 = CARTESIAN_POINT ( 'NONE',  ( 2.500000000000000000, 1448.335387686779995, 163.4889113519770092 ) ) ;
#40563 = CARTESIAN_POINT ( 'NONE',  ( -46.19755678850000180, 1376.012990379910207, 231.0255711751590013 ) ) ;
#40564 =( BOUNDED_SURFACE ( )  B_SPLINE_SURFACE ( 4, 2, ( 
 ( #85054, #51467, #77237, #34662, #68847, #104628, #52035, #76668, #86171, #27925, #103512 ),
 ( #25691, #95129, #26251, #60439, #94557, #104071, #9464, #17832, #43629, #52590, #77778 ),
 ( #61548, #1089, #26816, #61003, #18391, #86723, #44185, #95680, #53142, #87280, #10575 ),
 ( #78896, #44746, #79982, #12776, #96231, #54257, #64304, #88383, #45299, #3301, #2751 ),
 ( #106818, #11673, #96793, #79439, #46407, #89481, #88926, #98424, #63751, #28479, #97865 ) ),
 .UNSPECIFIED., .F., .T., .F. ) 
 B_SPLINE_SURFACE_WITH_KNOTS ( ( 5, 5 ),
 ( 3, 2, 2, 2, 2, 3 ),
 ( 3.613988937050000239, 5.260361675040000407 ),
 ( 5.178099995975939507, 6.283185307179590673, 7.853981633974480125, 9.424777960769379348, 10.99557428756429900, 11.46128530315550087 ),
 .UNSPECIFIED. ) 
 GEOMETRIC_REPRESENTATION_ITEM ( )  RATIONAL_B_SPLINE_SURFACE ( (
 ( 0.8778166930676709612, 0.7939440089458740246, 1.000000000000000000, 0.7071067811865480168, 1.000000000000000000, 0.7071067811865480168, 1.000000000000000000, 0.7071067811865480168, 1.000000000000000000, 0.9131627722406729930, 0.8778166930676709612),
 ( 0.8778166930676709612, 0.7939440089458740246, 1.000000000000000000, 0.7071067811865480168, 1.000000000000000000, 0.7071067811865480168, 1.000000000000000000, 0.7071067811865480168, 1.000000000000000000, 0.9131627722406729930, 0.8778166930676709612),
 ( 0.8778166930676709612, 0.7939440089458740246, 1.000000000000000000, 0.7071067811865480168, 1.000000000000000000, 0.7071067811865480168, 1.000000000000000000, 0.7071067811865480168, 1.000000000000000000, 0.9131627722406729930, 0.8778166930676709612),
 ( 0.8778166930676709612, 0.7939440089458740246, 1.000000000000000000, 0.7071067811865480168, 1.000000000000000000, 0.7071067811865480168, 1.000000000000000000, 0.7071067811865480168, 1.000000000000000000, 0.9131627722406729930, 0.8778166930676709612),
 ( 0.8778166930676709612, 0.7939440089458740246, 1.000000000000000000, 0.7071067811865480168, 1.000000000000000000, 0.7071067811865480168, 1.000000000000000000, 0.7071067811865480168, 1.000000000000000000, 0.9131627722406729930, 0.8778166930676709612) ) ) 
 REPRESENTATION_ITEM ( '' )  SURFACE ( )  );
#40565 = VERTEX_POINT ( 'NONE', #65555 ) ;
#40566 = CARTESIAN_POINT ( 'NONE',  ( -5.786527600464999033, 1517.025653221279981, 205.6708125431369751 ) ) ;
#40567 = VERTEX_POINT ( 'NONE', #57713 ) ;
#40568 = CARTESIAN_POINT ( 'NONE',  ( -2.486220139904999904, 1516.939658295650133, 209.1350829839039989 ) ) ;
#40569 = CARTESIAN_POINT ( 'NONE',  ( -21.02506738559999988, 1509.639958407829909, 229.8460882628980073 ) ) ;
#40570 = CARTESIAN_POINT ( 'NONE',  ( -36.12168399312893996, 1425.338662683803022, 269.5474266120900779 ) ) ;
#40571 = CARTESIAN_POINT ( 'NONE',  ( 6.597706014745000402, 1512.335510084630187, 217.2026964005870013 ) ) ;
#40573 = VERTEX_POINT ( 'NONE', #99665 ) ;
#40572 = FACE_OUTER_BOUND ( 'NONE', #73474, .T. ) ;
#40574 = CARTESIAN_POINT ( 'NONE',  ( 5.513435558228538369, 1508.611350403035431, 216.4436907933061320 ) ) ;
#40575 = CARTESIAN_POINT ( 'NONE',  ( -28.98124970245649834, 1440.913060387189944, 234.8964103687889917 ) ) ;
#40576 = CARTESIAN_POINT ( 'NONE',  ( -32.23247795450000552, 1383.839374993809770, 229.8499276021589992 ) ) ;
#40577 = PLANE ( 'NONE',  #39121 ) ;
#40578 = VECTOR ( 'NONE', #57282, 1000.000000000000000 ) ;
#40579 = CARTESIAN_POINT ( 'NONE',  ( 8.021036561768740469, 1410.327436765469884, 270.0743298054680395 ) ) ;
#40580 = CARTESIAN_POINT ( 'NONE',  ( 5.008848199894999631, 1516.858456333729919, 214.1219297979669989 ) ) ;
#40581 = CARTESIAN_POINT ( 'NONE',  ( 23.31374782499999654, 1409.831799812029885, 209.2655790302239893 ) ) ;
#40582 = ADVANCED_FACE ( 'NONE', ( #73947 ), #15108, .T. ) ;
#40583 = CARTESIAN_POINT ( 'NONE',  ( -20.92767404034479028, 1511.187213306747708, 235.3888156262297571 ) ) ;
#40584 = CARTESIAN_POINT ( 'NONE',  ( 3.001614222390000197, 1441.369934486689999, 218.5760139890790299 ) ) ;
#40585 = CARTESIAN_POINT ( 'NONE',  ( -7.713601987141389671, 1516.708834472129865, 209.9201896328700059 ) ) ;
#40586 = CARTESIAN_POINT ( 'NONE',  ( 1.135898785685000023, 1516.958737650239982, 210.2414381519470226 ) ) ;
#40588 = ADVANCED_FACE ( 'NONE', ( #6722 ), #33010, .F. ) ;
#40587 = CARTESIAN_POINT ( 'NONE',  ( 9.781792257336670460, 1435.212511321700049, 208.3818996341230161 ) ) ;
#40589 = CARTESIAN_POINT ( 'NONE',  ( 0.04809717934580000354, 1420.202363427830051, 183.9005163246980032 ) ) ;
#40590 = CARTESIAN_POINT ( 'NONE',  ( -3.482404828285579956, 1485.996524617339901, 182.2044860649310181 ) ) ;
#40592 = ORIENTED_EDGE ( 'NONE', *, *, #11355, .T. ) ;
#40591 = CARTESIAN_POINT ( 'NONE',  ( -52.53197402710000574, 1389.553010688960057, 259.5557295571589975 ) ) ;
#40593 = CARTESIAN_POINT ( 'NONE',  ( -46.06484833219570163, 1385.146025147649880, 253.6578770933249984 ) ) ;
#40594 = CARTESIAN_POINT ( 'NONE',  ( 18.89924256150000303, 1416.831925117730179, 210.6687426732179631 ) ) ;
#40595 = CARTESIAN_POINT ( 'NONE',  ( -3.323881039096373335, 1370.249599412167072, 210.1653830766376245 ) ) ;
#40596 = AXIS2_PLACEMENT_3D ( 'NONE', #54405, #39638, #54942 ) ;
#40597 = CARTESIAN_POINT ( 'NONE',  ( -18.18137283769999968, 1507.608465321030053, 229.7139307937979993 ) ) ;
#40598 = CARTESIAN_POINT ( 'NONE',  ( -4.925559152112373162, 1409.085064703106355, 194.7584071229671849 ) ) ;
#40599 = CARTESIAN_POINT ( 'NONE',  ( 12.02413026890000047, 1426.614203559159932, 205.4717539480090238 ) ) ;
#40600 = LINE ( 'NONE', #90994, #30809 ) ;
#40601 = ADVANCED_FACE ( 'NONE', ( #1110 ), #16016, .T. ) ;
#40603 = CARTESIAN_POINT ( 'NONE',  ( -7.768947876059999480, 1384.898102977279905, 218.9179155823389920 ) ) ;
#40602 = CARTESIAN_POINT ( 'NONE',  ( -5.003220765204999587, 1516.983995446890049, 216.0685944891870065 ) ) ;
#40604 = CARTESIAN_POINT ( 'NONE',  ( -25.66452594925480923, 1450.796198851616282, 137.0023867642745188 ) ) ;
#40605 = CARTESIAN_POINT ( 'NONE',  ( 31.76119286153743815, 1522.906363951597314, 221.9477464134155866 ) ) ;
#40606 = ORIENTED_EDGE ( 'NONE', *, *, #11781, .F. ) ;
#40607 = CARTESIAN_POINT ( 'NONE',  ( 5.777745395274999751, 1516.908489800550115, 202.5639360494670029 ) ) ;
#40608 = CARTESIAN_POINT ( 'NONE',  ( -15.73511544386499850, 1514.703592237370003, 224.4575895832670085 ) ) ;
#40609 = CARTESIAN_POINT ( 'NONE',  ( 0.2329173765010000285, 1487.216803758130027, 230.2681330600980232 ) ) ;
#40610 = AXIS2_PLACEMENT_3D ( 'NONE', #62033, #93931, #77705 ) ;
#40611 = FACE_OUTER_BOUND ( 'NONE', #85509, .T. ) ;
#40612 = CARTESIAN_POINT ( 'NONE',  ( 10.91793180594200052, 1461.492375007339888, 210.1518181392050053 ) ) ;
#40613 = CARTESIAN_POINT ( 'NONE',  ( 0.000000000000000000, 1518.913060387330006, 209.1218459616979999 ) ) ;
#40614 = CARTESIAN_POINT ( 'NONE',  ( 4.303723356569999936, 1466.891311542389758, 218.2258331277790262 ) ) ;
#40615 = CARTESIAN_POINT ( 'NONE',  ( 7.013597998606249107, 1416.776616305703783, 231.0639749510152399 ) ) ;
#40616 = EDGE_CURVE ( 'NONE', #108592, #80761, #9762, .T. ) ;
#40617 = CARTESIAN_POINT ( 'NONE',  ( 40.18841066169029830, 1444.887014588840202, 136.9828721817030157 ) ) ;
#40618 = CARTESIAN_POINT ( 'NONE',  ( -19.34668267510000206, 1426.404838512529977, 224.4165203646980160 ) ) ;
#40619 = CARTESIAN_POINT ( 'NONE',  ( -24.71654799220000243, 1435.786941262089840, 137.7886789613979772 ) ) ;
#40620 = CARTESIAN_POINT ( 'NONE',  ( -105.9329978819999951, 1390.513368602009905, 301.0435293657589568 ) ) ;
#40621 = CARTESIAN_POINT ( 'NONE',  ( 12.86159104559999911, 1509.362197043529932, 182.9546168079979793 ) ) ;
#40622 = CARTESIAN_POINT ( 'NONE',  ( -106.8917078750000087, 1391.793768397970098, 300.5749944091589896 ) ) ;
#40623 = CARTESIAN_POINT ( 'NONE',  ( -27.62462018541545916, 1463.884133562258057, 269.4472085826375292 ) ) ;
#40624 = VERTEX_POINT ( 'NONE', #12237 ) ;
#40626 = EDGE_CURVE ( 'NONE', #75973, #84881, #86647, .T. ) ;
#40625 = CARTESIAN_POINT ( 'NONE',  ( -4.196074440480000121E-15, 1430.453334911130241, 150.3332009510979788 ) ) ;
#40627 = CARTESIAN_POINT ( 'NONE',  ( -43.11111256194765673, 1429.682096741483065, 269.0454486936832268 ) ) ;
#40628 = CARTESIAN_POINT ( 'NONE',  ( 32.80315919379400214, 1523.919943579690425, 201.0769014459399102 ) ) ;
#40629 = CARTESIAN_POINT ( 'NONE',  ( 10.81714288539756730, 1427.819672987908461, 210.7127296406635537 ) ) ;
#40630 = CARTESIAN_POINT ( 'NONE',  ( -15.24610303002120659, 1451.631057024628035, 222.8112762265741651 ) ) ;
#40631 = AXIS2_PLACEMENT_3D ( 'NONE', #85767, #77384, #109340 ) ;
#40632 = CARTESIAN_POINT ( 'NONE',  ( -13.51709569822251922, 1443.869434758233183, 187.1393552450566915 ) ) ;
#40633 = CARTESIAN_POINT ( 'NONE',  ( -8.639773871640201719, 1437.117077603399821, 209.3259169240039910 ) ) ;
#40634 = CARTESIAN_POINT ( 'NONE',  ( 16.50400130224750583, 1525.907212628473644, 181.9890130758377040 ) ) ;
#40635 = CARTESIAN_POINT ( 'NONE',  ( -1.649050658508506073, 1415.557147993468789, 233.1206746122759341 ) ) ;
#40636 = CARTESIAN_POINT ( 'NONE',  ( -14.86020447212730033, 1415.677402202029953, 206.8262383623809910 ) ) ;
#40637 = CARTESIAN_POINT ( 'NONE',  ( -1.172395513999999869E-13, 1415.677402202029953, 209.1218459616989946 ) ) ;
#40638 = CARTESIAN_POINT ( 'NONE',  ( -12.77345823270095870, 1442.835097972180620, 169.4523692618799657 ) ) ;
#40640 = ORIENTED_EDGE ( 'NONE', *, *, #80072, .T. ) ;
#40639 = CARTESIAN_POINT ( 'NONE',  ( -15.08447935729999934, 1409.953164787530113, 226.5286084827979778 ) ) ;
#40641 = CARTESIAN_POINT ( 'NONE',  ( 0.4068402808920000280, 1415.948532224930204, 190.9215044426980228 ) ) ;
#40642 = EDGE_CURVE ( 'NONE', #92171, #15354, #34330, .T. ) ;
#40643 = CARTESIAN_POINT ( 'NONE',  ( 21.46027241321153411, 1509.101876359112566, 226.4434528296256417 ) ) ;
#40644 = ORIENTED_EDGE ( 'NONE', *, *, #11724, .F. ) ;
#40645 = ORIENTED_EDGE ( 'NONE', *, *, #42077, .T. ) ;
#40646 = CARTESIAN_POINT ( 'NONE',  ( 18.15372975567069957, 1416.529254608160045, 209.1733715860090115 ) ) ;
#40647 = CARTESIAN_POINT ( 'NONE',  ( 19.53786426059019021, 1522.382868172863937, 181.5239794925693388 ) ) ;
#40649 = CARTESIAN_POINT ( 'NONE',  ( -3.935524436840000195, 1461.184553958630204, 220.7697451388980028 ) ) ;
#40648 = CARTESIAN_POINT ( 'NONE',  ( 4.240943730709999748, 1455.710924186590091, 218.4112998676390021 ) ) ;
#40650 = CARTESIAN_POINT ( 'NONE',  ( -20.60158592759999863, 1507.916213491630060, 190.0723952602979807 ) ) ;
#40651 = CARTESIAN_POINT ( 'NONE',  ( -11.87922033200000094, 1433.121278621640158, 150.0748730425980000 ) ) ;
#40652 = EDGE_CURVE ( 'NONE', #19628, #5604, #109111, .T. ) ;
#40653 = CARTESIAN_POINT ( 'NONE',  ( -4.240938128602147472, 1509.032014137962278, 212.8662754392913143 ) ) ;
#40654 = CIRCLE ( 'NONE', #81801, 2.000000000000003997 ) ;
#40655 = CARTESIAN_POINT ( 'NONE',  ( 25.03647985883640104, 1433.346993170209998, 209.5640697471909846 ) ) ;
#40656 = CARTESIAN_POINT ( 'NONE',  ( -26.25026149509999840, 1438.546304523360050, 137.1341921698980002 ) ) ;
#40657 = CARTESIAN_POINT ( 'NONE',  ( -14.58270751444020341, 1429.861807585111592, 222.1210857218158878 ) ) ;
#40658 = DIRECTION ( 'NONE',  ( -5.980589973904019347E-17, 1.000000000000000000, -1.736889445713099699E-16 ) ) ;
#40659 = CARTESIAN_POINT ( 'NONE',  ( 2.675979268209999873, 1451.712890839929969, 183.7935420642980091 ) ) ;
#40660 = CARTESIAN_POINT ( 'NONE',  ( 8.050322358089076147, 1364.710190515749900, 208.3718459617061285 ) ) ;
#40661 = EDGE_CURVE ( 'NONE', #31602, #2577, #101183, .T. ) ;
#40662 = CARTESIAN_POINT ( 'NONE',  ( -27.53680538714794324, 1509.986730036300969, 197.2170476805838177 ) ) ;
#40664 = VERTEX_POINT ( 'NONE', #16074 ) ;
#40663 = CARTESIAN_POINT ( 'NONE',  ( -4.987078454554999318, 1508.551704408389924, 205.6342535004969818 ) ) ;
#40665 = ORIENTED_EDGE ( 'NONE', *, *, #79491, .T. ) ;
#40666 = CARTESIAN_POINT ( 'NONE',  ( -11.75633636577309993, 1426.832617176000213, 145.5136197768400166 ) ) ;
#40667 = CARTESIAN_POINT ( 'NONE',  ( -21.45377186783750290, 1505.623606155929792, 215.8817182770680176 ) ) ;
#40668 = CARTESIAN_POINT ( 'NONE',  ( -5.035691841070000230, 1473.968067415529958, 270.1320510969979978 ) ) ;
#40669 = CARTESIAN_POINT ( 'NONE',  ( 0.6589060341152864764, 1473.309946152746534, 219.3202346236175231 ) ) ;
#40670 = CARTESIAN_POINT ( 'NONE',  ( -103.1624317239240867, 1340.114449826968666, 321.4803018775698433 ) ) ;
#40671 = CARTESIAN_POINT ( 'NONE',  ( 36.52315179513340127, 1449.845863385239909, 136.2557797426800050 ) ) ;
#40672 = LINE ( 'NONE', #70882, #14293 ) ;
#40673 = CARTESIAN_POINT ( 'NONE',  ( -7.304960004490000713, 1480.235071529190009, 209.0219926440400116 ) ) ;
#40674 = CARTESIAN_POINT ( 'NONE',  ( -8.126234285584999384, 1514.923664147150021, 202.9950997886369635 ) ) ;
#40675 = CARTESIAN_POINT ( 'NONE',  ( -3.512275926230000067, 1456.435201441189975, 217.9329361306089936 ) ) ;
#40676 = CARTESIAN_POINT ( 'NONE',  ( 9.925983360904959696, 1364.303202023269932, 210.6218459616991936 ) ) ;
#40677 = CARTESIAN_POINT ( 'NONE',  ( -42.10743620715810209, 1426.274024488540135, 266.8069455525510421 ) ) ;
#40678 = ORIENTED_EDGE ( 'NONE', *, *, #47219, .T. ) ;
#40679 = CARTESIAN_POINT ( 'NONE',  ( -2.109056957580000002, 1421.166295015029846, 183.8085771866980167 ) ) ;
#40680 = EDGE_CURVE ( 'NONE', #64662, #4923, #82535, .T. ) ;
#40681 = VERTEX_POINT ( 'NONE', #32355 ) ;
#40682 = AXIS2_PLACEMENT_3D ( 'NONE', #19106, #10745, #44918 ) ;
#40683 = VERTEX_POINT ( 'NONE', #66534 ) ;
#40684 = CARTESIAN_POINT ( 'NONE',  ( -7.709032175815000443, 1516.534320418310244, 211.6070631641669877 ) ) ;
#40685 = CARTESIAN_POINT ( 'NONE',  ( 4.640563141391067958, 1423.702541937380602, 183.8770172325440058 ) ) ;
#40686 = CARTESIAN_POINT ( 'NONE',  ( -20.69714064973426559, 1525.848198008145346, 184.2818650771049533 ) ) ;
#40687 = EDGE_CURVE ( 'NONE', #4305, #64595, #18697, .T. ) ;
#40689 = CARTESIAN_POINT ( 'NONE',  ( -14.43289921072090110, 1509.539432542180066, 182.8218189571549885 ) ) ;
#40688 = CARTESIAN_POINT ( 'NONE',  ( -4.028630622785000170, 1516.812923327049930, 212.5819478221170016 ) ) ;
#40690 = CARTESIAN_POINT ( 'NONE',  ( -7.546903754000000575, 1440.426785413330208, 186.1739043644979859 ) ) ;
#40691 = AXIS2_PLACEMENT_3D ( 'NONE', #79949, #54221, #28440 ) ;
#40692 = CARTESIAN_POINT ( 'NONE',  ( -15.46699364564850043, 1461.188218472669860, 228.6959131744210083 ) ) ;
#40693 = VERTEX_POINT ( 'NONE', #1522 ) ;
#40694 = CARTESIAN_POINT ( 'NONE',  ( -26.80188213010000098, 1435.454224975739862, 135.5604543457980071 ) ) ;
#40695 = CARTESIAN_POINT ( 'NONE',  ( -6.943602691585000208, 1516.858069504249897, 202.1807456543569685 ) ) ;
#40696 = CARTESIAN_POINT ( 'NONE',  ( -8.648691763575000024, 1514.216922324319739, 203.4721261815869866 ) ) ;
#40697 = CARTESIAN_POINT ( 'NONE',  ( -29.17179959739380379, 1384.554205719389984, 205.1512235203240095 ) ) ;
#40698 =( BOUNDED_CURVE ( )  B_SPLINE_CURVE ( 3, ( #29332, #79763, #87608, #3071 ),
 .UNSPECIFIED., .F., .T. ) 
 B_SPLINE_CURVE_WITH_KNOTS ( ( 4, 4 ),
 ( 1.650548988561060026, 1.665073080160537788 ),
 .UNSPECIFIED. ) 
 CURVE ( )  GEOMETRIC_REPRESENTATION_ITEM ( )  RATIONAL_B_SPLINE_CURVE ( ( 1.000000000000000000, 0.9999824209741901004, 0.9999824209741901004, 1.000000000000000000 ) ) 
 REPRESENTATION_ITEM ( '' )  );
#40699 = CARTESIAN_POINT ( 'NONE',  ( -39.37395162027389972, 1426.108969844229932, 270.3385322152020649 ) ) ;
#40700 = DIRECTION ( 'NONE',  ( 0.06728379684272006722, -0.9969860201949397593, -0.03862338952348245980 ) ) ;
#40701 = CARTESIAN_POINT ( 'NONE',  ( -6.170313877949999970, 1397.182081567729938, 197.8857380414980014 ) ) ;
#40703 = EDGE_LOOP ( 'NONE', ( #69946, #42253, #95654, #81587 ) ) ;
#40702 = CARTESIAN_POINT ( 'NONE',  ( -38.20494153861119457, 1442.993962785479880, 137.1161392804889942 ) ) ;
#40704 = ORIENTED_EDGE ( 'NONE', *, *, #24131, .T. ) ;
#40705 = DIRECTION ( 'NONE',  ( 0.000000000000000000, 0.000000000000000000, 1.000000000000000000 ) ) ;
#40706 = CARTESIAN_POINT ( 'NONE',  ( 3.902542035141590038, 1426.015650130040058, 185.2953857556300079 ) ) ;
#40707 = CARTESIAN_POINT ( 'NONE',  ( 4.520890098355639708, 1426.568512013200007, 191.6274461433459919 ) ) ;
#40708 = CARTESIAN_POINT ( 'NONE',  ( -23.85803262429999805, 1435.336726310830045, 137.1743639523980107 ) ) ;
#40709 = CARTESIAN_POINT ( 'NONE',  ( 0.1595995995380000143, 1486.508831850330125, 181.8147405652979671 ) ) ;
#40710 = AXIS2_PLACEMENT_3D ( 'NONE', #100913, #75203, #5228 ) ;
#40711 = CARTESIAN_POINT ( 'NONE',  ( 7.726331925474999807, 1517.194972660189933, 211.4133602680070112 ) ) ;
#40712 = CARTESIAN_POINT ( 'NONE',  ( -68.78404569073209984, 1379.747969732330148, 280.2963111448109998 ) ) ;
#40713 = DIRECTION ( 'NONE',  ( 0.000000000000000000, 1.000000000000000000, 0.000000000000000000 ) ) ;
#40714 = CARTESIAN_POINT ( 'NONE',  ( 5.200694988025460042, 1440.224034440930154, 217.6292548469920121 ) ) ;
#40715 = CARTESIAN_POINT ( 'NONE',  ( -13.15726447020000123, 1414.996442546230128, 220.4820293380979876 ) ) ;
#40716 = CARTESIAN_POINT ( 'NONE',  ( -4.625693903144999730, 1517.042661899400173, 206.8353996064669786 ) ) ;
#40717 = EDGE_LOOP ( 'NONE', ( #19980, #35327, #32805, #67846 ) ) ;
#40718 = CARTESIAN_POINT ( 'NONE',  ( 21.41971086555086501, 1511.187213306747708, 185.1638823089577670 ) ) ;
#40719 = CARTESIAN_POINT ( 'NONE',  ( -10.13020165310000031, 1472.545330956490034, 208.0133926034690148 ) ) ;
#40720 = CARTESIAN_POINT ( 'NONE',  ( -8.743902791170000910, 1385.175134629190097, 218.5746284983589760 ) ) ;
#40721 = ORIENTED_EDGE ( 'NONE', *, *, #96917, .F. ) ;
#40723 = B_SPLINE_CURVE_WITH_KNOTS ( 'NONE', 5,
 ( #52166, #18517, #103654, #28042, #54382, #43753 ),
 .UNSPECIFIED., .F., .F.,
 ( 6, 6 ),
 ( 0.000000000000000000, 1.000000000000000000 ),
 .UNSPECIFIED. ) ;
#40722 = CARTESIAN_POINT ( 'NONE',  ( 22.08523867432350585, 1523.530870145309564, 233.8225105631262863 ) ) ;
#40724 = CARTESIAN_POINT ( 'NONE',  ( 12.91446205857219987, 1435.737941321880044, 150.7125339207690047 ) ) ;
#40725 = CARTESIAN_POINT ( 'NONE',  ( 13.61423569610000150, 1415.579607672129896, 196.7893798472979938 ) ) ;
#40726 = CARTESIAN_POINT ( 'NONE',  ( 16.31200673029999848, 1449.547814607470173, 190.3222646265980131 ) ) ;
#40727 = CARTESIAN_POINT ( 'NONE',  ( 25.61534012080000267, 1452.018571213930045, 135.1702111959979788 ) ) ;
#40728 = CARTESIAN_POINT ( 'NONE',  ( 10.72219805821039884, 1490.875092374679980, 211.5234845686590006 ) ) ;
#40729 = CARTESIAN_POINT ( 'NONE',  ( 4.798310207610000155, 1486.425997147189946, 199.4446566442690028 ) ) ;
#40730 = CARTESIAN_POINT ( 'NONE',  ( -0.1166470026081705552, 1506.491018783253367, 187.0913018223803874 ) ) ;
#40731 = CARTESIAN_POINT ( 'NONE',  ( 24.45342579656801618, 1444.690443231116660, 213.7192692780448908 ) ) ;
#40732 = AXIS2_PLACEMENT_3D ( 'NONE', #16227, #26295, #42014 ) ;
#40733 = CARTESIAN_POINT ( 'NONE',  ( 33.91369110979999846, 1435.681798629080049, 135.0664268281979901 ) ) ;
#40734 = CARTESIAN_POINT ( 'NONE',  ( 15.55634916703500004, 1516.551704408390151, 193.5654967650670244 ) ) ;
#40735 = CARTESIAN_POINT ( 'NONE',  ( 4.618119666265000589, 1516.706638732659940, 216.0591847158069925 ) ) ;
#40736 = VERTEX_POINT ( 'NONE', #96682 ) ;
#40737 = CARTESIAN_POINT ( 'NONE',  ( -12.78723768810000117, 1416.835809767730098, 195.5393901623979787 ) ) ;
#40738 = CARTESIAN_POINT ( 'NONE',  ( 16.19087789078229989, 1409.478458302130093, 193.2334102746530107 ) ) ;
#40739 = CARTESIAN_POINT ( 'NONE',  ( 1.781954896769999852, 1421.049472850429993, 183.1039533116980067 ) ) ;
#40740 = CARTESIAN_POINT ( 'NONE',  ( -2.609190002560000110, 1475.351101089589974, 219.2386560539989944 ) ) ;
#40741 = DIRECTION ( 'NONE',  ( 5.980589973904019347E-17, -1.000000000000000000, 1.736889445713099699E-16 ) ) ;
#40742 = CARTESIAN_POINT ( 'NONE',  ( -11.40514982007739953, 1470.815891563210016, 208.9000713169049845 ) ) ;
#40743 = CARTESIAN_POINT ( 'NONE',  ( -7.069698889257053587, 1508.382370789888455, 219.7441700735184895 ) ) ;
#40744 = CARTESIAN_POINT ( 'NONE',  ( 18.83207817909999804, 1416.311719782429918, 210.6697760117079952 ) ) ;
#40745 = CARTESIAN_POINT ( 'NONE',  ( 1.779428963082609894, 1456.357349037730046, 198.6855221610310309 ) ) ;
#40746 = CARTESIAN_POINT ( 'NONE',  ( -4.086314431204999487, 1515.499673567537911, 210.9648096920523983 ) ) ;
#40747 = CARTESIAN_POINT ( 'NONE',  ( 36.52292854368440800, 1440.913060387340010, 253.7928692754369706 ) ) ;
#40749 = CARTESIAN_POINT ( 'NONE',  ( -21.31355172039999957, 1471.299568758130135, 207.5959159578679873 ) ) ;
#40748 = CARTESIAN_POINT ( 'NONE',  ( -109.7187103849999943, 1384.936990287839990, 297.0861910508589858 ) ) ;
#40750 = DIRECTION ( 'NONE',  ( -0.000000000000000000, -1.000000000000000000, -0.000000000000000000 ) ) ;
#40751 = ORIENTED_EDGE ( 'NONE', *, *, #13050, .F. ) ;
#40752 = ORIENTED_EDGE ( 'NONE', *, *, #109197, .F. ) ;
#40753 = DIRECTION ( 'NONE',  ( 0.000000000000000000, 0.000000000000000000, 1.000000000000000000 ) ) ;
#40754 = VECTOR ( 'NONE', #12243, 1000.000000000000000 ) ;
#40755 = B_SPLINE_CURVE_WITH_KNOTS ( 'NONE', 5,
 ( #62401, #19230, #61850, #45045, #79190, #2496, #106035, #54553, #97628 ),
 .UNSPECIFIED., .F., .F.,
 ( 6, 3, 6 ),
 ( 0.000000000000000000, 0.5828366913979391439, 1.000000000000000000 ),
 .UNSPECIFIED. ) ;
#40756 = CARTESIAN_POINT ( 'NONE',  ( -1.464162264810000114, 1442.883873453590013, 200.3486113609690165 ) ) ;
#40757 = CARTESIAN_POINT ( 'NONE',  ( 11.76499821370110155, 1501.784643893570092, 211.4691548758199815 ) ) ;
#40758 = AXIS2_PLACEMENT_3D ( 'NONE', #70960, #2640, #35103 ) ;
#40759 = CARTESIAN_POINT ( 'NONE',  ( -12.61823209568500026, 1416.826860677879949, 222.0544590270410197 ) ) ;
#40760 = CARTESIAN_POINT ( 'NONE',  ( -1.906499846882070084E-08, 1517.051704408389924, 209.1218459511669892 ) ) ;
#40761 = TOROIDAL_SURFACE ( 'NONE', #1377, 4.250000000000000000, 0.5000000000000000000 ) ;
#40762 = DIRECTION ( 'NONE',  ( 0.9417419115949053898, -0.3363363969979660806, 9.559255346349054600E-15 ) ) ;
#40763 = CARTESIAN_POINT ( 'NONE',  ( -44.53843405880110140, 1383.820931003150008, 250.2441383139970128 ) ) ;
#40764 = AXIS2_PLACEMENT_3D ( 'NONE', #12721, #20012, #64250 ) ;
#40765 = CARTESIAN_POINT ( 'NONE',  ( -15.10740574596529839, 1465.251597859479944, 223.4038671133249920 ) ) ;
#40766 = CARTESIAN_POINT ( 'NONE',  ( 24.95756467220000019, 1451.613974107930062, 137.4741664119979987 ) ) ;
#40767 = CARTESIAN_POINT ( 'NONE',  ( -12.43173911540150023, 1502.554234090240016, 208.9876481361740161 ) ) ;
#40768 = CARTESIAN_POINT ( 'NONE',  ( 11.81690186861369973, 1492.270327107419917, 210.4669352574049981 ) ) ;
#40770 = ORIENTED_EDGE ( 'NONE', *, *, #68672, .F. ) ;
#40769 = CARTESIAN_POINT ( 'NONE',  ( -14.44303134326499993, 1516.995662938509895, 225.7915129991669971 ) ) ;
#40771 = DIRECTION ( 'NONE',  ( -1.755985294532469921E-16, 1.000000000000000000, -1.338183447452831989E-16 ) ) ;
#40772 = EDGE_CURVE ( 'NONE', #43851, #65447, #95606, .T. ) ;
#40773 = CARTESIAN_POINT ( 'NONE',  ( -47.53302541269999892, 1383.816002435690052, 256.2046081452590442 ) ) ;
#40774 = EDGE_CURVE ( 'NONE', #39431, #76345, #73221, .T. ) ;
#40775 = CARTESIAN_POINT ( 'NONE',  ( 8.559858904628349308, 1437.030483964089854, 207.9845584131589931 ) ) ;
#40776 = ORIENTED_EDGE ( 'NONE', *, *, #9026, .T. ) ;
#40777 = ORIENTED_EDGE ( 'NONE', *, *, #62192, .T. ) ;
#40778 = CARTESIAN_POINT ( 'NONE',  ( -8.951560400169498166, 1386.309576927779972, 218.4184569005070102 ) ) ;
#40779 = CARTESIAN_POINT ( 'NONE',  ( 35.62940004342829781, 1437.304582500250262, 136.5355437598550168 ) ) ;
#40781 = CARTESIAN_POINT ( 'NONE',  ( 1.802301219090000073, 1409.910657985330090, 232.1755723407979985 ) ) ;
#40780 = CARTESIAN_POINT ( 'NONE',  ( 30.51231035492521571, 1526.382868172863937, 218.1578534183718432 ) ) ;
#40782 = CARTESIAN_POINT ( 'NONE',  ( -9.183711187100000117, 1463.569275765890097, 202.8257126108990178 ) ) ;
#40783 = CARTESIAN_POINT ( 'NONE',  ( -106.6208966620000069, 1378.950518748449895, 300.1891795401589320 ) ) ;
#40784 = CARTESIAN_POINT ( 'NONE',  ( -32.38114538885245963, 1523.604703353109699, 216.1203639561433647 ) ) ;
#40785 = CARTESIAN_POINT ( 'NONE',  ( -12.74120642066979947, 1508.551704408389924, 216.7626981741809971 ) ) ;
#40786 = AXIS2_PLACEMENT_3D ( 'NONE', #45787, #12150, #22174 ) ;
#40787 = CARTESIAN_POINT ( 'NONE',  ( 13.00319530123149825, 1409.367141973109938, 201.7590943873260017 ) ) ;
#40788 = DIRECTION ( 'NONE',  ( -1.000000000000000000, 0.000000000000000000, 0.000000000000000000 ) ) ;
#40789 = CYLINDRICAL_SURFACE ( 'NONE', #3593, 1.000000000000000888 ) ;
#40790 = CARTESIAN_POINT ( 'NONE',  ( -6.252266492314999979, 1511.741868877540128, 200.3335294429169835 ) ) ;
#40791 = CARTESIAN_POINT ( 'NONE',  ( 11.30198679499999947, 1432.355652606810054, 151.5220046058980188 ) ) ;
#40792 = EDGE_CURVE ( 'NONE', #98390, #36271, #96834, .T. ) ;
#40793 = CARTESIAN_POINT ( 'NONE',  ( -3.369446259835010338, 1448.970159117820003, 184.7951506743999914 ) ) ;
#40794 = ORIENTED_EDGE ( 'NONE', *, *, #13862, .T. ) ;
#40795 = CARTESIAN_POINT ( 'NONE',  ( -33.23571934791658578, 1511.187213306747708, 219.4842663281467026 ) ) ;
#40796 = CARTESIAN_POINT ( 'NONE',  ( 19.00954907529469651, 1456.857281488789795, 226.5573691136240200 ) ) ;
#40797 = CARTESIAN_POINT ( 'NONE',  ( -12.81107806870000054, 1435.505600523229759, 150.7241902968979730 ) ) ;
#40798 = LINE ( 'NONE', #74977, #3629 ) ;
#40799 = CARTESIAN_POINT ( 'NONE',  ( -0.3104492283789259122, 1515.598602702389826, 213.1604326987470017 ) ) ;
#40800 = CARTESIAN_POINT ( 'NONE',  ( 2.688586027246119947, 1509.006950727750109, 238.2845013960090057 ) ) ;
#40801 = LINE ( 'NONE', #38587, #13883 ) ;
#40802 = CARTESIAN_POINT ( 'NONE',  ( -7.518184220077429814, 1510.874996213040049, 215.1349743772009901 ) ) ;
#40803 = CARTESIAN_POINT ( 'NONE',  ( -9.505471540889999460, 1363.500209798499782, 207.6218459616989946 ) ) ;
#40804 = CARTESIAN_POINT ( 'NONE',  ( -46.05254598119929454, 1440.698150564019898, 266.6769892118650205 ) ) ;
#40805 = CARTESIAN_POINT ( 'NONE',  ( 2.272601175003300167, 1429.102097603389893, 217.0941385727449813 ) ) ;
#40806 = CARTESIAN_POINT ( 'NONE',  ( 19.63722818094939981, 1521.951704408389787, 218.2362632588020119 ) ) ;
#40807 = CARTESIAN_POINT ( 'NONE',  ( 6.556850996575000146, 1516.939568781210028, 209.1101343261499892 ) ) ;
#40808 = AXIS2_PLACEMENT_3D ( 'NONE', #37234, #52942, #103299 ) ;
#40809 = CARTESIAN_POINT ( 'NONE',  ( 4.398715393588610745, 1409.066666913600102, 223.5593897730840069 ) ) ;
#40810 = EDGE_CURVE ( 'NONE', #8175, #75798, #60709, .T. ) ;
#40811 = CARTESIAN_POINT ( 'NONE',  ( 5.684698448500000723, 1422.983443193229959, 101.6537298026979954 ) ) ;
#40812 = CARTESIAN_POINT ( 'NONE',  ( 7.385549640129020155, 1425.110251876329812, 212.4835268894509852 ) ) ;
#40813 = ORIENTED_EDGE ( 'NONE', *, *, #69666, .T. ) ;
#40814 = CARTESIAN_POINT ( 'NONE',  ( 29.63060611060000227, 1437.055399740629809, 238.0637397513980034 ) ) ;
#40816 = CARTESIAN_POINT ( 'NONE',  ( -14.86137038355130002, 1512.142158944850053, 221.4605574290570189 ) ) ;
#40815 = CARTESIAN_POINT ( 'NONE',  ( -1.462006285199999978, 1452.693442003630025, 183.1060772031979980 ) ) ;
#40817 = EDGE_CURVE ( 'NONE', #86466, #23487, #4765, .T. ) ;
#40818 = DIRECTION ( 'NONE',  ( 0.000000000000000000, 0.000000000000000000, 1.000000000000000000 ) ) ;
#40819 = CARTESIAN_POINT ( 'NONE',  ( -26.57890459470000266, 1440.913060377039983, 225.2395996604980155 ) ) ;
#40820 = CARTESIAN_POINT ( 'NONE',  ( -4.636806382847598940, 1378.035560348909030, 214.3314208189594297 ) ) ;
#40821 = CARTESIAN_POINT ( 'NONE',  ( 0.7186111224017516230, 1415.502631355655922, 233.2905737576144247 ) ) ;
#40822 = CARTESIAN_POINT ( 'NONE',  ( 29.24087330780000116, 1451.891771913630237, 134.8528131887979953 ) ) ;
#40823 = ORIENTED_EDGE ( 'NONE', *, *, #29742, .T. ) ;
#40824 = DIRECTION ( 'NONE',  ( -0.8304244096547924725, -0.2476038119107163427, -0.4990868182759106708 ) ) ;
#40825 = LINE ( 'NONE', #22342, #99094 ) ;
#40826 = CARTESIAN_POINT ( 'NONE',  ( 14.52431039145089997, 1420.570648330259928, 228.2522164977820296 ) ) ;
#40827 = CARTESIAN_POINT ( 'NONE',  ( 11.45308832699999968, 1502.277520793189979, 208.2819378797420029 ) ) ;
#40828 = ORIENTED_EDGE ( 'NONE', *, *, #709, .F. ) ;
#40829 = ORIENTED_EDGE ( 'NONE', *, *, #5717, .F. ) ;
#40830 = AXIS2_PLACEMENT_3D ( 'NONE', #96516, #88130, #44468 ) ;
#40831 = CARTESIAN_POINT ( 'NONE',  ( -84.13410175530000856, 1384.933881297359903, 288.0523788940590180 ) ) ;
#40832 = CARTESIAN_POINT ( 'NONE',  ( -22.82803524321889910, 1409.710179317919938, 209.0907902649259995 ) ) ;
#40833 = ORIENTED_EDGE ( 'NONE', *, *, #78317, .F. ) ;
#40834 = CARTESIAN_POINT ( 'NONE',  ( -107.7907090231699954, 1350.849221539110204, 307.2862155841589811 ) ) ;
#40835 = CARTESIAN_POINT ( 'NONE',  ( 20.88002914659999831, 1495.383068942589944, 212.2131686182190151 ) ) ;
#40836 = CIRCLE ( 'NONE', #28302, 1.999999999999999556 ) ;
#40837 = TOROIDAL_SURFACE ( 'NONE', #94453, 32.13701971169416538, 1.000000000000000000 ) ;
#40838 = B_SPLINE_CURVE_WITH_KNOTS ( 'NONE', 3,
 ( #40745, #48055, #92250, #64322, #23384, #40195, #82191, #31789, #65423, #98443, #99530, #23923, #66532, #38535, #57574, #81090, #90036, #55917, #47507, #91148, #91699, #39077, #81631, #74377, #6595, #108503, #74921, #39650, #107948, #64877, #109072, #32353, #100636, #14423, #73255, #26693, #85483 ),
 .UNSPECIFIED., .F., .F.,
 ( 4, 3, 3, 3, 3, 3, 3, 3, 3, 3, 3, 3, 4 ),
 ( -13.00030988960000045, -12.70431845186110031, -12.03435738184399995, -11.32254726432860004, -10.57086120063609869, -9.761044970981449964, -8.781608299062758860, -7.853302061585090144, -7.046341670537930035, -6.091992644973400317, -5.300241650221800604, -4.613009676061491149, -3.966463181889999134 ),
 .UNSPECIFIED. ) ;
#40839 = CARTESIAN_POINT ( 'NONE',  ( -15.47717805819999981, 1507.633541959229888, 231.3088780856980122 ) ) ;
#40840 = CARTESIAN_POINT ( 'NONE',  ( -19.15216164439999957, 1415.854273250330152, 223.1450478733979992 ) ) ;
#40841 = ORIENTED_EDGE ( 'NONE', *, *, #105278, .T. ) ;
#40842 = AXIS2_PLACEMENT_3D ( 'NONE', #62251, #10160, #78477 ) ;
#40843 = CARTESIAN_POINT ( 'NONE',  ( 46.15276881562959943, 1443.753714320680047, 267.5938072023989776 ) ) ;
#40844 = CARTESIAN_POINT ( 'NONE',  ( -4.802232148216890373, 1508.551704408389924, 204.6920728333849979 ) ) ;
#40845 = CARTESIAN_POINT ( 'NONE',  ( 0.1379860871630000096, 1419.157121733429904, 184.6437352945980024 ) ) ;
#40846 = CARTESIAN_POINT ( 'NONE',  ( -3.265407155974999753, 1516.754149861460064, 204.5121726906670006 ) ) ;
#40847 = EDGE_LOOP ( 'NONE', ( #42100, #70051 ) ) ;
#40848 = CARTESIAN_POINT ( 'NONE',  ( 18.75615393743843029, 1458.159782462800649, 227.2589280249185606 ) ) ;
#40849 = CARTESIAN_POINT ( 'NONE',  ( 15.10400614679230102, 1513.569700116999911, 194.6305253545030212 ) ) ;
#40850 = VERTEX_POINT ( 'NONE', #105639 ) ;
#40851 = CARTESIAN_POINT ( 'NONE',  ( 2.500000005229999989, 1448.233542440780184, 182.8968085845980056 ) ) ;
#40852 = CARTESIAN_POINT ( 'NONE',  ( 26.85709460237750079, 1451.975207230750129, 134.9160983460150192 ) ) ;
#40853 = CARTESIAN_POINT ( 'NONE',  ( -13.23930721601690053, 1512.526687531830021, 193.8438098916049910 ) ) ;
#40854 = CARTESIAN_POINT ( 'NONE',  ( 7.214474816066029028, 1504.316466902849925, 219.6367501992550046 ) ) ;
#40855 = CARTESIAN_POINT ( 'NONE',  ( 7.782064256880000030, 1421.606440417200020, 195.8228046871990102 ) ) ;
#40856 = CARTESIAN_POINT ( 'NONE',  ( 1.181149777510320131, 1431.413309031290055, 218.5383434680610151 ) ) ;
#40857 = CARTESIAN_POINT ( 'NONE',  ( 10.65417391917219980, 1479.073446957750093, 205.9772944084500068 ) ) ;
#40858 = CARTESIAN_POINT ( 'NONE',  ( 2.151766400366240006, 1408.988201725800081, 186.9699580838769748 ) ) ;
#40860 = CARTESIAN_POINT ( 'NONE',  ( -18.54538606469993312, 1424.331165113354700, 224.9582236530350769 ) ) ;
#40859 = CARTESIAN_POINT ( 'NONE',  ( -13.46701286011549925, 1434.939967867589985, 148.8194410816790025 ) ) ;
#40861 = CARTESIAN_POINT ( 'NONE',  ( 3.497150990277209104, 1441.358042536442326, 170.5351636937986370 ) ) ;
#40862 = CIRCLE ( 'NONE', #80202, 0.9999999999999880096 ) ;
#40863 = CARTESIAN_POINT ( 'NONE',  ( -12.49949197370000142, 1379.134263153570146, 212.2053367160189907 ) ) ;
#40864 = DIRECTION ( 'NONE',  ( -0.9417419115949662300, -0.2378257470769920556, 0.2378257470769920556 ) ) ;
#40865 = EDGE_LOOP ( 'NONE', ( #3832, #49651, #2740, #6531 ) ) ;
#40866 = FACE_OUTER_BOUND ( 'NONE', #4065, .T. ) ;
#40867 = CARTESIAN_POINT ( 'NONE',  ( -4.491820960670080849E-16, 1519.551704408389924, 209.1218459616989946 ) ) ;
#40868 = CARTESIAN_POINT ( 'NONE',  ( 30.90487439922556945, 1525.907212628473644, 201.8101144455177689 ) ) ;
#40869 = CARTESIAN_POINT ( 'NONE',  ( -9.075511479460001141, 1387.789233278139818, 200.5952413198190243 ) ) ;
#40870 =( BOUNDED_CURVE ( )  B_SPLINE_CURVE ( 3, ( #105239, #80034, #44797, #86220 ),
 .UNSPECIFIED., .F., .F. ) 
 B_SPLINE_CURVE_WITH_KNOTS ( ( 4, 4 ),
 ( 6.207195670891930028, 6.514798957309980487 ),
 .UNSPECIFIED. ) 
 CURVE ( )  GEOMETRIC_REPRESENTATION_ITEM ( )  RATIONAL_B_SPLINE_CURVE ( ( 1.000000000000000000, 0.9921305491659986320, 0.9921305491659986320, 1.000000000000000000 ) ) 
 REPRESENTATION_ITEM ( '' )  );
#40871 = CARTESIAN_POINT ( 'NONE',  ( 9.661937460982130688, 1423.484310766260023, 209.7266508472010003 ) ) ;
#40872 = CARTESIAN_POINT ( 'NONE',  ( 10.99916455748379995, 1424.384112525169940, 203.1270655916410135 ) ) ;
#40873 = CARTESIAN_POINT ( 'NONE',  ( 13.06210717429999946, 1418.073220907129780, 221.6712522191980099 ) ) ;
#40874 = CARTESIAN_POINT ( 'NONE',  ( -40.73184307449999864, 1440.913060387330006, 268.3665355201979992 ) ) ;
#40875 = CARTESIAN_POINT ( 'NONE',  ( -9.087937995490110055, 1383.941172989790175, 218.5505186622879989 ) ) ;
#40876 = CARTESIAN_POINT ( 'NONE',  ( 11.87454696380000030, 1433.566416203000017, 150.5469651275980141 ) ) ;
#40877 = CARTESIAN_POINT ( 'NONE',  ( 38.34143788450000301, 1440.913060387330006, 265.6112250856980381 ) ) ;
#40878 = CARTESIAN_POINT ( 'NONE',  ( 13.15726442949999964, 1415.948532224930204, 196.5399405751979884 ) ) ;
#40879 = CARTESIAN_POINT ( 'NONE',  ( -16.79355120555579717, 1420.470915846049820, 203.2250788671829866 ) ) ;
#40880 = CARTESIAN_POINT ( 'NONE',  ( -109.9515965448952528, 1385.962241300529513, 297.0326770096235691 ) ) ;
#40881 = CARTESIAN_POINT ( 'NONE',  ( 7.600171787371139409, 1465.644562267609899, 215.5555306133580018 ) ) ;
#40882 = CARTESIAN_POINT ( 'NONE',  ( 12.78749341904959991, 1416.842625005220043, 222.1385636096939891 ) ) ;
#40883 = CARTESIAN_POINT ( 'NONE',  ( 5.343927860473110414, 1473.943544974919860, 219.2193853163629740 ) ) ;
#40884 = CARTESIAN_POINT ( 'NONE',  ( -17.48419695489999981, 1410.887768726630156, 225.6235195252980077 ) ) ;
#40885 = CARTESIAN_POINT ( 'NONE',  ( -0.5620977654159999837, 1416.851343902729923, 227.7685710129979952 ) ) ;
#40886 = CARTESIAN_POINT ( 'NONE',  ( -7.083943808717527268, 1442.001743124033055, 184.0116861733216069 ) ) ;
#40887 = CARTESIAN_POINT ( 'NONE',  ( -17.06446529402930068, 1409.673968815769967, 193.1470206694820035 ) ) ;
#40888 = CARTESIAN_POINT ( 'NONE',  ( 1.491420627269999910, 1515.551704408389924, 205.2164164778889983 ) ) ;
#40889 = CARTESIAN_POINT ( 'NONE',  ( -0.8350686643532179154, 1526.382868172863937, 177.3106345060153046 ) ) ;
#40890 = CARTESIAN_POINT ( 'NONE',  ( 1.968601690575629615, 1498.935401749600032, 197.9561509338619771 ) ) ;
#40891 = FACE_OUTER_BOUND ( 'NONE', #95171, .T. ) ;
#40892 =( BOUNDED_CURVE ( )  B_SPLINE_CURVE ( 3, ( #53824, #51592, #34779, #68965 ),
 .UNSPECIFIED., .F., .T. ) 
 B_SPLINE_CURVE_WITH_KNOTS ( ( 4, 4 ),
 ( 4.163468865690415299, 5.261334023187549391 ),
 .UNSPECIFIED. ) 
 CURVE ( )  GEOMETRIC_REPRESENTATION_ITEM ( )  RATIONAL_B_SPLINE_CURVE ( ( 1.000000000000000000, 0.9020546424876372260, 0.9020546424876372260, 1.000000000000000000 ) ) 
 REPRESENTATION_ITEM ( '' )  );
#40893 = CARTESIAN_POINT ( 'NONE',  ( 0.2059318620510010023, 1459.640043076150050, 182.9685224155400078 ) ) ;
#40895 = ORIENTED_EDGE ( 'NONE', *, *, #27051, .F. ) ;
#40894 = CARTESIAN_POINT ( 'NONE',  ( -10.79382269979189957, 1414.913060387349788, 196.1395788316550011 ) ) ;
#40896 = CARTESIAN_POINT ( 'NONE',  ( -20.22153155800000235, 1444.740067931809790, 161.9155394238979966 ) ) ;
#40897 = CARTESIAN_POINT ( 'NONE',  ( -29.06644740117960168, 1509.916355021930030, 211.6311731943499979 ) ) ;
#40898 = CARTESIAN_POINT ( 'NONE',  ( 13.80518339569999853, 1434.979590798060144, 149.4781242251980302 ) ) ;
#40899 = CARTESIAN_POINT ( 'NONE',  ( -41.49772933732800340, 1445.334750750280136, 134.0999999984909721 ) ) ;
#40900 = CARTESIAN_POINT ( 'NONE',  ( -109.5348954149999940, 1384.904938781000055, 297.1231113849590315 ) ) ;
#40901 = VERTEX_POINT ( 'NONE', #28924 ) ;
#40902 = B_SPLINE_SURFACE_WITH_KNOTS ( 'NONE', 5, 1, ( 
 ( #30966, #100379 ),
 ( #55650, #99810 ),
 ( #23104, #5784 ),
 ( #64603, #15250 ),
 ( #23664, #29863 ),
 ( #5219, #65141 ) ),
 .UNSPECIFIED., .F., .F., .F.,
 ( 6, 6 ),
 ( 2, 2 ),
 ( 0.000000000000000000, 15.53865474348330089 ),
 ( 0.000000000000000000, 14.00001426917759950 ),
 .UNSPECIFIED. ) ;
#40903 = CARTESIAN_POINT ( 'NONE',  ( -16.85976061912589330, 1525.821544997590081, 182.0492613858612856 ) ) ;
#40904 = CARTESIAN_POINT ( 'NONE',  ( 9.659057376369998948, 1477.882669201989984, 202.4105350377390096 ) ) ;
#40905 = CARTESIAN_POINT ( 'NONE',  ( -108.1829836398146796, 1383.261649930543399, 310.8763756577378672 ) ) ;
#40906 = DIRECTION ( 'NONE',  ( 0.02091224828123159837, -0.9990482215818557998, 0.03827961371219689574 ) ) ;
#40907 = CARTESIAN_POINT ( 'NONE',  ( -5.682011391568829950, 1434.576080618040123, 216.5206222332380150 ) ) ;
#40908 = CARTESIAN_POINT ( 'NONE',  ( -109.1320112420000044, 1384.953741877089897, 311.2644403302589353 ) ) ;
#40909 = AXIS2_PLACEMENT_3D ( 'NONE', #38461, #106225, #53645 ) ;
#40910 = CARTESIAN_POINT ( 'NONE',  ( -15.32670450039999999, 1414.929621208459821, 211.2240752700589894 ) ) ;
#40911 = CARTESIAN_POINT ( 'NONE',  ( -12.52644033109999988, 1379.461106441880020, 210.4487255907489782 ) ) ;
#40912 = CARTESIAN_POINT ( 'NONE',  ( 21.02608924029999926, 1456.853724928630072, 225.6706377209980303 ) ) ;
#40913 = B_SPLINE_SURFACE_WITH_KNOTS ( 'NONE', 5, 1, ( 
 ( #63643, #88815 ),
 ( #36757, #64185 ),
 ( #106704, #70950 ),
 ( #3186, #45736 ),
 ( #37315, #29994 ),
 ( #70391, #71510 ) ),
 .UNSPECIFIED., .F., .F., .F.,
 ( 6, 6 ),
 ( 2, 2 ),
 ( 0.000000000000000000, 3.407694589789999728 ),
 ( 0.000000000000000000, 14.00000000000000000 ),
 .UNSPECIFIED. ) ;
#40914 = CARTESIAN_POINT ( 'NONE',  ( -59.40129820653180559, 1385.058454097869799, 242.7081510328939942 ) ) ;
#40915 = CARTESIAN_POINT ( 'NONE',  ( -18.19590854888122067, 1522.382868172863937, 238.2026672068776918 ) ) ;
#40916 = CARTESIAN_POINT ( 'NONE',  ( 10.39668864703249973, 1424.335650574019837, 206.8537076104200025 ) ) ;
#40917 = ORIENTED_EDGE ( 'NONE', *, *, #71381, .T. ) ;
#40918 = CARTESIAN_POINT ( 'NONE',  ( -33.93392600300000339, 1451.271752324530098, 135.9465290377980011 ) ) ;
#40919 = CARTESIAN_POINT ( 'NONE',  ( -16.78004044744790235, 1410.586458347280086, 226.3834300362210001 ) ) ;
#40920 = EDGE_CURVE ( 'NONE', #71147, #12190, #28364, .T. ) ;
#40922 = VERTEX_POINT ( 'NONE', #3196 ) ;
#40921 = CARTESIAN_POINT ( 'NONE',  ( -1.313045906442075417, 1526.382868172863937, 239.3665138341975194 ) ) ;
#40923 = CARTESIAN_POINT ( 'NONE',  ( 3.438860216040000140, 1473.468534316989917, 218.9084199681889800 ) ) ;
#40924 = AXIS2_PLACEMENT_3D ( 'NONE', #20606, #45859, #79992 ) ;
#40925 = CARTESIAN_POINT ( 'NONE',  ( 10.10501075033869967, 1471.402064569889944, 212.2221579359460009 ) ) ;
#40926 = CARTESIAN_POINT ( 'NONE',  ( -20.78416915826518618, 1410.998464924520249, 218.9268079218183232 ) ) ;
#40927 = CARTESIAN_POINT ( 'NONE',  ( -109.4864630750000174, 1384.848068253500060, 311.2837400852590122 ) ) ;
#40928 = CARTESIAN_POINT ( 'NONE',  ( -0.2146684641345620037, 1419.294041481389968, 184.5302216556299868 ) ) ;
#40929 = B_SPLINE_CURVE_WITH_KNOTS ( 'NONE', 3,
 ( #25657, #2714, #94521, #87816, #45265, #36283, #70475, #77744, #11104, #51433, #17795, #103473, #18358, #52552 ),
 .UNSPECIFIED., .F., .F.,
 ( 4, 2, 2, 2, 2, 2, 4 ),
 ( 0.000000000000000000, 0.0005413989221883810064, 0.001082797844376762013, 0.002165595688753024425, 0.002706994610941156065, 0.003248393533129286404, 0.004331191377505529301 ),
 .UNSPECIFIED. ) ;
#40930 = ADVANCED_FACE ( 'NONE', ( #44072 ), #48188, .F. ) ;
#40931 = CARTESIAN_POINT ( 'NONE',  ( 22.84636239139999603, 1410.205970967429948, 213.3090871733579661 ) ) ;
#40932 = CARTESIAN_POINT ( 'NONE',  ( -22.52564151159999639, 1509.699673122230024, 190.3321270482979912 ) ) ;
#40933 = CARTESIAN_POINT ( 'NONE',  ( -17.05725733019999879, 1423.778776128129948, 228.3108127086979948 ) ) ;
#40934 = CARTESIAN_POINT ( 'NONE',  ( -4.993716309010864940, 1511.400001115550822, 200.6009875924737855 ) ) ;
#40935 = CARTESIAN_POINT ( 'NONE',  ( 7.257468615629999675, 1448.222523044890295, 203.1720000238289856 ) ) ;
#40936 = CARTESIAN_POINT ( 'NONE',  ( -100.1346419727999972, 1320.102705746890251, 304.2218459572590064 ) ) ;
#40937 = CARTESIAN_POINT ( 'NONE',  ( 13.22806383159999832, 1431.113060387329824, 223.7296695649979767 ) ) ;
#40938 = CARTESIAN_POINT ( 'NONE',  ( -30.95751052620429888, 1525.821544997590308, 216.7905424461076223 ) ) ;
#40939 = CARTESIAN_POINT ( 'NONE',  ( 4.997250153905000047, 1516.727068157269969, 205.8570671527170077 ) ) ;
#40940 = AXIS2_PLACEMENT_3D ( 'NONE', #82985, #40975, #6276 ) ;
#40941 = CARTESIAN_POINT ( 'NONE',  ( -5.424805956284839858, 1485.524231091950014, 183.2664633616439858 ) ) ;
#40942 = ORIENTED_EDGE ( 'NONE', *, *, #61029, .F. ) ;
#40943 = CARTESIAN_POINT ( 'NONE',  ( -2.664535259099999805E-15, 1424.786834349990158, 209.1218459616989946 ) ) ;
#40944 = CARTESIAN_POINT ( 'NONE',  ( -4.221749840679269283, 1441.602648943890017, 169.9194788150119848 ) ) ;
#40946 = EDGE_LOOP ( 'NONE', ( #52416, #46670, #66602, #78297 ) ) ;
#40945 = CARTESIAN_POINT ( 'NONE',  ( -68.53014284327269934, 1379.747351453789861, 280.1403612264239769 ) ) ;
#40947 = CARTESIAN_POINT ( 'NONE',  ( -16.67802482740000158, 1423.369746731130135, 229.1820141820979870 ) ) ;
#40948 = VERTEX_POINT ( 'NONE', #14304 ) ;
#40949 = CARTESIAN_POINT ( 'NONE',  ( -16.78936288871751614, 1513.473960729824284, 222.1909530149808631 ) ) ;
#40950 = CARTESIAN_POINT ( 'NONE',  ( 11.90463986800000029, 1500.041165469490124, 206.3230776397589921 ) ) ;
#40952 = CARTESIAN_POINT ( 'NONE',  ( 15.77332111128689895, 1410.712355435420022, 191.5214290250879685 ) ) ;
#40951 = CARTESIAN_POINT ( 'NONE',  ( -11.15802834450066960, 1425.158734329488198, 144.3721351036122940 ) ) ;
#40953 = CARTESIAN_POINT ( 'NONE',  ( 2.881548424445000034, 1516.909589401870107, 211.4054166033970148 ) ) ;
#40954 = CARTESIAN_POINT ( 'NONE',  ( 39.14754442216379715, 1437.687579504329960, 135.1140516034500081 ) ) ;
#40955 = CARTESIAN_POINT ( 'NONE',  ( -106.4534877654000127, 1378.913060387279984, 306.3385543931779580 ) ) ;
#40956 = CARTESIAN_POINT ( 'NONE',  ( -3.829620113550000315, 1515.551704408389924, 211.4519800877889963 ) ) ;
#40957 = CARTESIAN_POINT ( 'NONE',  ( 12.62398172905319882, 1500.937524318219857, 210.6201263454209993 ) ) ;
#40958 = CARTESIAN_POINT ( 'NONE',  ( 39.62133910696010020, 1449.056109088829999, 134.0999999980940061 ) ) ;
#40959 = CARTESIAN_POINT ( 'NONE',  ( -25.50058789191978903, 1507.958244999422959, 219.0382223049803372 ) ) ;
#40960 = EDGE_LOOP ( 'NONE', ( #76010, #17823, #39169 ) ) ;
#40961 = CARTESIAN_POINT ( 'NONE',  ( -20.36853080839999919, 1464.956632876090225, 210.9458194778790130 ) ) ;
#40962 = DIRECTION ( 'NONE',  ( 0.01561979272848090620, -2.869309375241887618E-18, 0.9998780035959984325 ) ) ;
#40963 = EDGE_LOOP ( 'NONE', ( #81293, #100187, #73795, #109232 ) ) ;
#40964 = ORIENTED_EDGE ( 'NONE', *, *, #29311, .F. ) ;
#40965 = CARTESIAN_POINT ( 'NONE',  ( 2.500000000000000000, 1411.429641636930000, 126.8043280305979863 ) ) ;
#40966 = CARTESIAN_POINT ( 'NONE',  ( -19.59884465730855396, 1526.382868172863937, 181.1441328703422187 ) ) ;
#40967 = CARTESIAN_POINT ( 'NONE',  ( 0.1012992125219999984, 1452.346416936929927, 183.2694984107980076 ) ) ;
#40968 = CARTESIAN_POINT ( 'NONE',  ( -3.226026720880000198, 1485.996674929329856, 182.1725539718979974 ) ) ;
#40969 = CARTESIAN_POINT ( 'NONE',  ( -2.500000000000000000, 1439.466623781370117, 162.9904194795870183 ) ) ;
#40970 = FACE_OUTER_BOUND ( 'NONE', #49615, .T. ) ;
#40971 = CIRCLE ( 'NONE', #103547, 1.638701816490922836 ) ;
#40972 = CARTESIAN_POINT ( 'NONE',  ( -12.62383844309999859, 1379.141235998960155, 208.5749163320770094 ) ) ;
#40973 = CARTESIAN_POINT ( 'NONE',  ( 12.65728676410210163, 1420.119835224449844, 200.3472210950669989 ) ) ;
#40974 = CARTESIAN_POINT ( 'NONE',  ( 2.215029529077919612, 1421.204142362009861, 183.2132787965950058 ) ) ;
#40975 = DIRECTION ( 'NONE',  ( -0.3363363969981477131, 0.6659120918162938496, -0.6659120918162938496 ) ) ;
#40976 = CARTESIAN_POINT ( 'NONE',  ( -10.81163464159999954, 1391.913060620420083, 213.5809022996290025 ) ) ;
#40977 = CARTESIAN_POINT ( 'NONE',  ( -84.10394180980790679, 1384.813803161769783, 287.8662587808539683 ) ) ;
#40978 = ORIENTED_EDGE ( 'NONE', *, *, #67475, .F. ) ;
#40979 = CARTESIAN_POINT ( 'NONE',  ( -0.7538707734179979081, 1516.719999691880048, 202.1833671473370089 ) ) ;
#40980 = CARTESIAN_POINT ( 'NONE',  ( -7.726684725664999753, 1517.208444099459939, 207.9957078235169945 ) ) ;
#40981 = EDGE_LOOP ( 'NONE', ( #30158, #76910, #35279 ) ) ;
#40982 = CARTESIAN_POINT ( 'NONE',  ( -12.42529224677512900, 1517.151704408390060, 215.5613278979431868 ) ) ;
#40983 = AXIS2_PLACEMENT_3D ( 'NONE', #84835, #102732, #17057 ) ;
#40984 = CARTESIAN_POINT ( 'NONE',  ( 18.93563805549999657, 1457.027062798830002, 226.9364425294979810 ) ) ;
#40985 = EDGE_LOOP ( 'NONE', ( #3270, #4506, #36386, #75922, #97911 ) ) ;
#40986 = CARTESIAN_POINT ( 'NONE',  ( -13.76900370180000088, 1415.553739807329976, 221.3900038008980005 ) ) ;
#40987 = CARTESIAN_POINT ( 'NONE',  ( 5.994546415740489742, 1429.671868418749909, 216.4766293005329771 ) ) ;
#40988 = CARTESIAN_POINT ( 'NONE',  ( -7.823403845102177456, 1435.182002661693332, 212.6572978892697563 ) ) ;
#40989 = CARTESIAN_POINT ( 'NONE',  ( -9.771304594386510445, 1462.553183801680007, 206.2411433844070245 ) ) ;
#40990 = CARTESIAN_POINT ( 'NONE',  ( 21.62164173326539895, 1519.551704408389924, 208.0273405521070060 ) ) ;
#40991 = CARTESIAN_POINT ( 'NONE',  ( 9.905021055853989509, 1468.629943020290057, 207.6432958796129924 ) ) ;
#40992 = CARTESIAN_POINT ( 'NONE',  ( -10.54299263360008432, 1469.936041725191217, 213.3752367157486560 ) ) ;
#40993 = CARTESIAN_POINT ( 'NONE',  ( -11.87539561500000040, 1433.006908915509939, 148.5636847365980202 ) ) ;
#40994 = CARTESIAN_POINT ( 'NONE',  ( -16.08458092929999950, 1496.377567048629999, 224.3648175664979760 ) ) ;
#40996 = CARTESIAN_POINT ( 'NONE',  ( 2.487935084889999704, 1508.551704408389924, 214.1089244042930204 ) ) ;
#40995 = CARTESIAN_POINT ( 'NONE',  ( 12.57364047979999810, 1461.601951568030017, 232.5174476254979652 ) ) ;
#40997 = CARTESIAN_POINT ( 'NONE',  ( -4.832904859673011977, 1422.320778277333375, 184.7689124830623086 ) ) ;
#40998 = CARTESIAN_POINT ( 'NONE',  ( 7.717505752974999744, 1516.857914730730045, 216.8393517232070167 ) ) ;
#40999 = VERTEX_POINT ( 'NONE', #31663 ) ;
#41000 = AXIS2_PLACEMENT_3D ( 'NONE', #102913, #1054, #60402 ) ;
#41001 = CARTESIAN_POINT ( 'NONE',  ( 19.26683521067225868, 1456.110280151028292, 225.0772932314519892 ) ) ;
#41002 = CARTESIAN_POINT ( 'NONE',  ( 19.05195134132430113, 1485.012485562190022, 228.6148904062209795 ) ) ;
#41003 = AXIS2_PLACEMENT_3D ( 'NONE', #87490, #17475, #103148 ) ;
#41004 = CARTESIAN_POINT ( 'NONE',  ( -0.4346943098025670138, 1517.051704408590012, 216.8444262844809884 ) ) ;
#41005 = CARTESIAN_POINT ( 'NONE',  ( -6.548821979184999975, 1516.688761843659904, 213.1592242262869945 ) ) ;
#41006 = CARTESIAN_POINT ( 'NONE',  ( 4.138326088227719524, 1515.492270357839971, 211.4517668477679990 ) ) ;
#41007 = CARTESIAN_POINT ( 'NONE',  ( -11.60004869885885981, 1425.580039266544873, 138.3016037470954984 ) ) ;
#41009 = ORIENTED_EDGE ( 'NONE', *, *, #92498, .T. ) ;
#41008 = CARTESIAN_POINT ( 'NONE',  ( 4.492644271869690620, 1508.880967335730247, 212.9248485414070160 ) ) ;
#41010 = CARTESIAN_POINT ( 'NONE',  ( -15.51611637578909253, 1415.679618464087071, 209.5978448638990415 ) ) ;
#41011 = CARTESIAN_POINT ( 'NONE',  ( -2.182617347539999919, 1508.212127139989889, 220.8438686939989850 ) ) ;
#41012 = CARTESIAN_POINT ( 'NONE',  ( -11.56293446569999972, 1431.298376297659843, 151.1185897447979869 ) ) ;
#41013 = DIRECTION ( 'NONE',  ( 0.001339522651315419892, 0.9999644786255611484, 0.008321488218843280452 ) ) ;
#41014 = CARTESIAN_POINT ( 'NONE',  ( -109.6203430457589860, 1383.204584676429931, 311.2218735730909884 ) ) ;
#41015 = CARTESIAN_POINT ( 'NONE',  ( 11.76196303810490029, 1425.587148917709783, 146.3422016857230119 ) ) ;
#41016 = CARTESIAN_POINT ( 'NONE',  ( 7.923742487380000199, 1501.702996767189916, 206.8471783426489878 ) ) ;
#41017 = CARTESIAN_POINT ( 'NONE',  ( 9.201169484990000313, 1472.509397971289900, 190.7635733242989886 ) ) ;
#41019 = DIRECTION ( 'NONE',  ( -1.755985294532469921E-16, 1.000000000000000000, -1.338183447452831989E-16 ) ) ;
#41018 = CARTESIAN_POINT ( 'NONE',  ( -19.12494372069999926, 1470.092089012029874, 227.6083304972979988 ) ) ;
#41020 = DIRECTION ( 'NONE',  ( 0.000000000000000000, 0.000000000000000000, -1.000000000000000000 ) ) ;
#41021 = CIRCLE ( 'NONE', #99998, 11.71219856409999949 ) ;
#41022 = ORIENTED_EDGE ( 'NONE', *, *, #34725, .T. ) ;
#41023 = CARTESIAN_POINT ( 'NONE',  ( 0.7355686427760019797, 1517.012231669750008, 205.8548062402470009 ) ) ;
#41024 = CARTESIAN_POINT ( 'NONE',  ( 7.089205951499999436, 1406.122960630329999, 267.8325111671979926 ) ) ;
#41025 = CARTESIAN_POINT ( 'NONE',  ( 0.04535681774329999860, 1409.423586797529879, 185.2161043470979678 ) ) ;
#41026 = CARTESIAN_POINT ( 'NONE',  ( -19.53786426058999481, 1512.187213306747481, 238.7197124308268030 ) ) ;
#41027 = CARTESIAN_POINT ( 'NONE',  ( 24.41839517916415403, 1437.873015353542996, 212.8347989158633027 ) ) ;
#41028 = B_SPLINE_CURVE_WITH_KNOTS ( 'NONE', 3,
 ( #15196, #21936, #21393, #13002, #47186, #42083, #50495, #76233, #9019, #93019, #43192, #85171, #17952, #25249, #85722, #9565, #59451, #51589, #49934, #7912, #93562, #67303, #60559, #34223, #67850 ),
 .UNSPECIFIED., .F., .F.,
 ( 4, 3, 3, 3, 3, 3, 3, 3, 4 ),
 ( -15.26428536230000077, -15.04480521863770015, -14.77980626134180042, -14.51062898585870009, -14.40705048899830132, -14.15432204787279957, -13.90085348180759972, -13.66131906363690085, -13.44470525013180051 ),
 .UNSPECIFIED. ) ;
#41029 = CARTESIAN_POINT ( 'NONE',  ( -8.158010031739319601, 1387.526404868172904, 218.5023346017954395 ) ) ;
#41030 = CARTESIAN_POINT ( 'NONE',  ( 1.546943247107299912, 1416.828039266790029, 190.2227890105679933 ) ) ;
#41031 = DIRECTION ( 'NONE',  ( 1.000000000000000000, 0.000000000000000000, 0.000000000000000000 ) ) ;
#41032 = CARTESIAN_POINT ( 'NONE',  ( -16.02484169309999729, 1417.968543311129906, 204.0964181816090104 ) ) ;
#41033 = CIRCLE ( 'NONE', #94664, 1.000000000000071498 ) ;
#41034 = CARTESIAN_POINT ( 'NONE',  ( -12.76211179859999945, 1446.342786738940049, 187.8166300136979885 ) ) ;
#41035 = CARTESIAN_POINT ( 'NONE',  ( 1.971747376402030127, 1450.333125966990110, 155.0636711809370070 ) ) ;
#41036 = CARTESIAN_POINT ( 'NONE',  ( -16.21393388683536330, 1419.735053903993730, 209.9280921983989003 ) ) ;
#41037 = CARTESIAN_POINT ( 'NONE',  ( -3.805400412610000060, 1495.647977866990004, 219.6495694401989738 ) ) ;
#41038 = B_SPLINE_CURVE_WITH_KNOTS ( 'NONE', 5,
 ( #62435, #4160, #96561, #105514, #38287, #19833, #72469, #98194, #54038, #106599, #29884, #1969 ),
 .UNSPECIFIED., .F., .F.,
 ( 6, 3, 3, 6 ),
 ( 0.000000000000000000, 0.1840082528089916347, 0.5520247584167143895, 1.000000000000000000 ),
 .UNSPECIFIED. ) ;
#41039 = CARTESIAN_POINT ( 'NONE',  ( -6.509745615790000883, 1426.468882645629947, 219.6133833021979740 ) ) ;
#41040 = B_SPLINE_SURFACE_WITH_KNOTS ( 'NONE', 4, 5, ( 
 ( #110563, #18147, #69139, #102687, #93736, #17014 ),
 ( #103243, #95975, #25982, #103824, #94299, #51777 ),
 ( #85915, #52342, #70265, #1942, #36080, #104374 ),
 ( #27670, #3601, #90315, #70820, #88693, #72449 ),
 ( #29865, #79195, #72989, #11432, #56176, #4140 ) ),
 .UNSPECIFIED., .F., .F., .F.,
 ( 5, 5 ),
 ( 6, 6 ),
 ( 83.28839604430000065, 84.04303036039999597 ),
 ( 0.000000000000000000, 2.000000000000000000 ),
 .UNSPECIFIED. ) ;
#41041 = CARTESIAN_POINT ( 'NONE',  ( 10.88304335850896010, 1425.085735208080905, 138.6335396438064436 ) ) ;
#41042 = CARTESIAN_POINT ( 'NONE',  ( -12.21146186157374558, 1377.806055270933484, 210.7083772430368072 ) ) ;
#41043 = CARTESIAN_POINT ( 'NONE',  ( -2.755319248979999802, 1475.501610869329852, 269.2919052328979888 ) ) ;
#41044 = CARTESIAN_POINT ( 'NONE',  ( -4.224262963665889714, 1446.243947084759839, 166.7663216723609878 ) ) ;
#41045 = CARTESIAN_POINT ( 'NONE',  ( -14.09480582055672926, 1514.058997558268629, 192.5091585815071937 ) ) ;
#41046 = CARTESIAN_POINT ( 'NONE',  ( 18.21301937251889669, 1417.703604459479948, 223.2038275229089948 ) ) ;
#41047 = CARTESIAN_POINT ( 'NONE',  ( -52.45833321412619910, 1384.728393318099961, 266.7659804183330152 ) ) ;
#41048 = CARTESIAN_POINT ( 'NONE',  ( -10.17701364196129887, 1462.839837219120000, 206.1633443696570112 ) ) ;
#41049 = CARTESIAN_POINT ( 'NONE',  ( -11.97827956719999776, 1441.604408666619975, 150.7817505876979851 ) ) ;
#41050 = B_SPLINE_SURFACE_WITH_KNOTS ( 'NONE', 5, 5, ( 
 ( #52474, #79875, #27253, #69277, #79322, #96674 ),
 ( #95012, #36759, #68727, #3189, #86602, #77658 ),
 ( #102832, #26689, #9353, #53025, #87732, #105068 ),
 ( #2633, #28357, #971, #62555, #11562, #35096 ),
 ( #45738, #87161, #26126, #19382, #2080, #94433 ),
 ( #95560, #18830, #103383, #45181, #60885, #44064 ),
 ( #10450, #78764, #104512, #36209, #70394, #27809 ),
 ( #61991, #65287, #89908, #38943, #63645, #47918 ),
 ( #73694, #37869, #107820, #82053, #3736, #12659 ),
 ( #29996, #4272, #31108, #29448, #13182, #14298 ),
 ( #56324, #91008, #63109, #38402, #13734, #5359 ),
 ( #21587, #4798, #55793, #97760, #107265, #21032 ),
 ( #64187, #98861, #99400, #71512, #37317, #47371 ),
 ( #81496, #97208, #46838, #73123, #106706, #12103 ),
 ( #39518, #89368, #55235, #80967, #90456, #72578 ),
 ( #30560, #64750, #22125, #22679, #56878, #98309 ),
 ( #48487, #54691, #20481, #82627, #105631, #88817 ),
 ( #28918, #46296, #80424, #72054, #106169, #57447 ),
 ( #32760, #14848, #23249, #59636, #99954, #66943 ),
 ( #49039, #75342, #74244, #84805, #100517, #108374 ),
 ( #68051, #59091, #49585, #66397, #25442, #83716 ) ),
 .UNSPECIFIED., .F., .F., .F.,
 ( 6, 3, 3, 3, 3, 3, 6 ),
 ( 6, 6 ),
 ( 2.123077381369999905, 2.437842270119999988, 2.821447585090000043, 3.205052900050000098, 4.739453051259999938, 7.802280429849999699, 10.88241929079999970 ),
 ( 0.000000000000000000, 2.000000000000000000 ),
 .UNSPECIFIED. ) ;
#41051 = CARTESIAN_POINT ( 'NONE',  ( -25.55722864341189648, 1470.062555774519979, 211.0468171208650006 ) ) ;
#41052 = DIRECTION ( 'NONE',  ( -0.000000000000000000, 1.000000000000000000, 0.000000000000000000 ) ) ;
#41053 = CARTESIAN_POINT ( 'NONE',  ( -46.16777962713913297, 1440.913025796686270, 266.9714940337735811 ) ) ;
#41054 = CARTESIAN_POINT ( 'NONE',  ( -22.22003955790000163, 1410.184095304630091, 203.2211024675479791 ) ) ;
#41055 = CARTESIAN_POINT ( 'NONE',  ( -10.43567586334632935, 1379.713673404171232, 202.4914496242319331 ) ) ;
#41056 = CARTESIAN_POINT ( 'NONE',  ( -15.08006399635999983, 1422.394886018492116, 228.4054473227839992 ) ) ;
#41057 = CARTESIAN_POINT ( 'NONE',  ( 11.35315220146310011, 1478.711703769590031, 206.1320505837120152 ) ) ;
#41058 = ORIENTED_EDGE ( 'NONE', *, *, #35253, .F. ) ;
#41059 = EDGE_CURVE ( 'NONE', #68445, #78057, #110697, .T. ) ;
#41060 = B_SPLINE_SURFACE_WITH_KNOTS ( 'NONE', 5, 5, ( 
 ( #18146, #69704, #77525, #69138, #62976, #18690 ),
 ( #826, #86462, #95427, #87590, #43919, #3051 ),
 ( #36621, #9755, #2500, #88143, #45602, #78066 ),
 ( #70264, #70819, #20353, #1369, #78626, #52887 ),
 ( #54558, #103242, #87015, #37177, #35511, #103823 ),
 ( #26552, #88692, #1941, #36079, #60746, #27123 ) ),
 .UNSPECIFIED., .F., .F., .F.,
 ( 6, 6 ),
 ( 6, 6 ),
 ( 2.161187085849999967, 3.155691482920000013 ),
 ( 0.000000000000000000, 2.242653719299999793 ),
 .UNSPECIFIED. ) ;
#41061 = CARTESIAN_POINT ( 'NONE',  ( -4.500000000000000000, 1448.210448412289907, 183.1418046154980175 ) ) ;
#41062 = CARTESIAN_POINT ( 'NONE',  ( 5.093836579314430679, 1436.649832418680035, 228.7462252422310200 ) ) ;
#41063 = CARTESIAN_POINT ( 'NONE',  ( -7.540337791715355564, 1510.559702728800175, 214.8951611895496399 ) ) ;
#41064 = CARTESIAN_POINT ( 'NONE',  ( -9.771939461242810765, 1448.872234804809978, 190.8346844886999918 ) ) ;
#41066 = CARTESIAN_POINT ( 'NONE',  ( -15.05391208946500115, 1514.225267046429963, 193.1292084085670240 ) ) ;
#41065 = CARTESIAN_POINT ( 'NONE',  ( 11.61671915839999869, 1425.877048038330031, 142.7663299324979960 ) ) ;
#41067 = CARTESIAN_POINT ( 'NONE',  ( 16.97880994394067500, 1525.055427061254477, 236.9933064582837687 ) ) ;
#41068 = AXIS2_PLACEMENT_3D ( 'NONE', #34050, #479, #92296 ) ;
#41069 = CARTESIAN_POINT ( 'NONE',  ( -119.4939992282800034, 1358.631207110790001, 300.8926790057490166 ) ) ;
#41070 = CARTESIAN_POINT ( 'NONE',  ( 27.13948228459569734, 1449.857009993160091, 136.5864004438930124 ) ) ;
#41071 = CARTESIAN_POINT ( 'NONE',  ( -0.06764669157372509012, 1408.848989335589977, 223.4935224539250100 ) ) ;
#41072 = CARTESIAN_POINT ( 'NONE',  ( 5.003220727074999985, 1516.983995446890049, 202.1750974131470286 ) ) ;
#41073 = DIRECTION ( 'NONE',  ( 1.192122195693504081E-14, -4.372198439846870180E-16, -1.000000000000000000 ) ) ;
#41074 = CARTESIAN_POINT ( 'NONE',  ( -7.214502255410000231, 1427.316505021429975, 144.1938086916980239 ) ) ;
#41075 = CARTESIAN_POINT ( 'NONE',  ( 16.52887561823499851, 1513.466724478469814, 194.9208948791670082 ) ) ;
#41076 = CARTESIAN_POINT ( 'NONE',  ( -16.16601204028820149, 1420.773371822770059, 203.3216470037820045 ) ) ;
#41077 = CARTESIAN_POINT ( 'NONE',  ( -27.44664266310000400, 1376.937662249230016, 217.0346396320790063 ) ) ;
#41078 = VECTOR ( 'NONE', #21152, 1000.000000000000000 ) ;
#41079 = CARTESIAN_POINT ( 'NONE',  ( 22.02982242722629991, 1509.705750766509937, 228.9645431730439782 ) ) ;
#41081 = ORIENTED_EDGE ( 'NONE', *, *, #37412, .F. ) ;
#41080 = CARTESIAN_POINT ( 'NONE',  ( -31.42949257678390040, 1379.646779223169915, 219.2469095604439815 ) ) ;
#41082 = ORIENTED_EDGE ( 'NONE', *, *, #90599, .T. ) ;
#41083 = CARTESIAN_POINT ( 'NONE',  ( 11.97707002367110007, 1433.612440445840093, 149.8647669520520083 ) ) ;
#41084 = CARTESIAN_POINT ( 'NONE',  ( -9.880256809820002317, 1396.317500971430036, 216.0574990009879741 ) ) ;
#41085 = CARTESIAN_POINT ( 'NONE',  ( -21.13431007490000013, 1409.651086757829944, 211.8287213018879811 ) ) ;
#41086 = ORIENTED_EDGE ( 'NONE', *, *, #47972, .T. ) ;
#41087 = CARTESIAN_POINT ( 'NONE',  ( -12.92812670435129796, 1444.919964772552021, 169.4323874481358700 ) ) ;
#41088 = CARTESIAN_POINT ( 'NONE',  ( 22.14096540611513575, 1509.702029783286889, 228.7416374943908579 ) ) ;
#41089 = CARTESIAN_POINT ( 'NONE',  ( 0.000000000000000000, 1511.187213306747708, 209.1218459616979999 ) ) ;
#41091 = CARTESIAN_POINT ( 'NONE',  ( 18.02093535799999913, 1424.326836137830014, 225.1991050518980160 ) ) ;
#41090 = CARTESIAN_POINT ( 'NONE',  ( 3.094100512289999827, 1445.021403822989896, 200.6774107941290026 ) ) ;
#41092 = CARTESIAN_POINT ( 'NONE',  ( 2.889876570069999762, 1449.237408619179860, 183.9651879290979934 ) ) ;
#41093 = CARTESIAN_POINT ( 'NONE',  ( -4.342662522768870659, 1464.389982461639875, 199.4525629763099914 ) ) ;
#41094 = CARTESIAN_POINT ( 'NONE',  ( -17.54273015099310129, 1417.931783278020021, 206.8684746656099946 ) ) ;
#41095 = CARTESIAN_POINT ( 'NONE',  ( 7.090230613856629560, 1396.160656768040099, 200.6535277794220065 ) ) ;
#41096 = CARTESIAN_POINT ( 'NONE',  ( 1.226570660889999997, 1415.553739809529816, 190.6686965949980106 ) ) ;
#41097 = CARTESIAN_POINT ( 'NONE',  ( 11.30181802809999958, 1432.344320995729731, 151.5221848940979896 ) ) ;
#41098 = CARTESIAN_POINT ( 'NONE',  ( 8.900197448897545272, 1509.223855520506504, 181.2015886599364762 ) ) ;
#41099 = ORIENTED_EDGE ( 'NONE', *, *, #65274, .T. ) ;
#41100 = CARTESIAN_POINT ( 'NONE',  ( 13.38600686010279972, 1434.923461442529970, 148.9942416261320091 ) ) ;
#41101 = B_SPLINE_CURVE_WITH_KNOTS ( 'NONE', 5,
 ( #100960, #65738, #92564, #76894, #7468, #102066, #25349, #15299, #6912, #32123, #41069, #8015, #84168, #75784, #57355, #67404, #91480, #33215 ),
 .UNSPECIFIED., .F., .F.,
 ( 6, 3, 3, 3, 3, 6 ),
 ( -75.86994138869999915, -60.45619974110000072, -46.86861349480000172, -18.08975840989999284, -6.500000000000000000, -0.4214913904880006612 ),
 .UNSPECIFIED. ) ;
#41102 = ORIENTED_EDGE ( 'NONE', *, *, #59611, .T. ) ;
#41103 = ORIENTED_EDGE ( 'NONE', *, *, #65451, .T. ) ;
#41104 = EDGE_CURVE ( 'NONE', #77481, #29796, #99979, .T. ) ;
#41105 = CARTESIAN_POINT ( 'NONE',  ( -19.93329733863729913, 1507.860201379970022, 229.2059767788809950 ) ) ;
#41106 = CARTESIAN_POINT ( 'NONE',  ( -5.374569443010000391, 1464.404629604329784, 236.8301565885979869 ) ) ;
#41107 = AXIS2_PLACEMENT_3D ( 'NONE', #34728, #81009, #21627 ) ;
#41108 = CARTESIAN_POINT ( 'NONE',  ( -109.0465141062722410, 1387.661433126290603, 310.8477273668624434 ) ) ;
#41109 = CARTESIAN_POINT ( 'NONE',  ( -1.124289693584999972, 1517.184063036290127, 215.6857614941170027 ) ) ;
#41110 = CARTESIAN_POINT ( 'NONE',  ( -7.951444182101831792, 1511.804172066088313, 212.3302999886905980 ) ) ;
#41111 = ORIENTED_EDGE ( 'NONE', *, *, #19397, .T. ) ;
#41112 = CARTESIAN_POINT ( 'NONE',  ( -5.599233173528683771, 1387.285800435509827, 209.1218459616989946 ) ) ;
#41113 = CARTESIAN_POINT ( 'NONE',  ( 2.578840932191499675E-14, 1375.413060387289988, 208.3364477938620212 ) ) ;
#41114 = ORIENTED_EDGE ( 'NONE', *, *, #24725, .T. ) ;
#41115 = CARTESIAN_POINT ( 'NONE',  ( -6.561686461364999445, 1517.069378699710114, 205.6695567495270041 ) ) ;
#41116 = VERTEX_POINT ( 'NONE', #55241 ) ;
#41117 = CARTESIAN_POINT ( 'NONE',  ( -5.011551406145000165, 1517.080322339569875, 208.3849417611969841 ) ) ;
#41118 = AXIS2_PLACEMENT_3D ( 'NONE', #78135, #1438, #9287 ) ;
#41119 = FACE_OUTER_BOUND ( 'NONE', #29830, .T. ) ;
#41120 = CARTESIAN_POINT ( 'NONE',  ( -2.923263438819999838, 1409.521015953330107, 186.8216762074980011 ) ) ;
#41121 = CARTESIAN_POINT ( 'NONE',  ( -0.3331912114570000361, 1408.924695680830155, 232.1910260989980088 ) ) ;
#41123 = ORIENTED_EDGE ( 'NONE', *, *, #86544, .F. ) ;
#41122 = CARTESIAN_POINT ( 'NONE',  ( -0.5835301444350500244, 1415.089118586289942, 226.3143562410230061 ) ) ;
#41124 = CARTESIAN_POINT ( 'NONE',  ( 19.10224170140000410, 1426.438701496329941, 223.3166183795979975 ) ) ;
#41125 = DIRECTION ( 'NONE',  ( 1.755985294532464991E-16, -1.000000000000000000, 1.338183447452830017E-16 ) ) ;
#41126 = CARTESIAN_POINT ( 'NONE',  ( -54.14955217329999471, 1384.412447748920158, 270.3592636482590024 ) ) ;
#41127 = CARTESIAN_POINT ( 'NONE',  ( -0.4080517659392200458, 1465.111786428190044, 238.1138255402620132 ) ) ;
#41128 = CARTESIAN_POINT ( 'NONE',  ( 7.559855552100000153, 1408.395244667930001, 270.2818740095979706 ) ) ;
#41129 = CARTESIAN_POINT ( 'NONE',  ( -7.711550716115000093, 1516.630499592039996, 213.1573366827869904 ) ) ;
#41130 = CARTESIAN_POINT ( 'NONE',  ( 22.71503220009999779, 1409.706269051729805, 209.0936436305159987 ) ) ;
#41131 = DIRECTION ( 'NONE',  ( -0.6736849260863839728, 0.000000000000000000, 0.7390186874254150995 ) ) ;
#41132 = CARTESIAN_POINT ( 'NONE',  ( 16.98839455092350192, 1428.323430003820022, 202.7579036764070111 ) ) ;
#41134 = ADVANCED_FACE ( 'NONE', ( #47377 ), #109918, .F. ) ;
#41133 = CARTESIAN_POINT ( 'NONE',  ( 7.012524221607120190, 1508.551704613440052, 215.1061910685279770 ) ) ;
#41135 = CARTESIAN_POINT ( 'NONE',  ( 5.788691325514999875, 1517.157901477309906, 210.2449475486469908 ) ) ;
#41136 = EDGE_CURVE ( 'NONE', #69131, #64021, #23089, .T. ) ;
#41137 = CARTESIAN_POINT ( 'NONE',  ( 9.686384332386170470, 1434.926238005200048, 207.6434806796090129 ) ) ;
#41138 = CARTESIAN_POINT ( 'NONE',  ( 0.2324887852820000100, 1420.496092096330131, 182.7590697851979940 ) ) ;
#41139 = FACE_OUTER_BOUND ( 'NONE', #61803, .T. ) ;
#41140 = ADVANCED_FACE ( 'NONE', ( #33866 ), #31183, .F. ) ;
#41142 = EDGE_LOOP ( 'NONE', ( #63336, #44314, #16029, #75373 ) ) ;
#41141 = CARTESIAN_POINT ( 'NONE',  ( -62.07030651009999644, 1385.055139444880069, 284.7661505247589844 ) ) ;
#41143 = CARTESIAN_POINT ( 'NONE',  ( -47.91919660017039462, 1385.134697410870103, 257.4398826552600212 ) ) ;
#41144 = CIRCLE ( 'NONE', #48278, 2.000000000000003553 ) ;
#41145 = B_SPLINE_SURFACE_WITH_KNOTS ( 'NONE', 5, 5, ( 
 ( #91522, #74734, #83661, #92609, #109979, #57936 ),
 ( #14246, #59040, #92068, #33255, #107767, #56823 ),
 ( #40561, #108319, #58481, #24299, #65781, #48435 ),
 ( #49536, #73637, #15340, #15884, #75289, #82577 ),
 ( #67446, #6957, #6416, #5306, #48987, #108870 ),
 ( #31603, #39465, #99344, #5868, #99899, #13676 ),
 ( #22620, #40010, #32161, #7509, #66894, #41671 ),
 ( #66348, #74190, #23196, #50085, #101002, #14801 ),
 ( #83120, #100465, #23748, #109435, #32712, #84213 ) ),
 .UNSPECIFIED., .F., .F., .F.,
 ( 6, 3, 6 ),
 ( 6, 6 ),
 ( 0.5394538425010000360, 1.941044340399999957, 4.123493948330000158 ),
 ( 0.000000000000000000, 2.000000000000000000 ),
 .UNSPECIFIED. ) ;
#41146 = CARTESIAN_POINT ( 'NONE',  ( 30.61443310237122617, 1523.382868172863937, 196.4193608261158772 ) ) ;
#41147 = EDGE_CURVE ( 'NONE', #35589, #41404, #10125, .T. ) ;
#41148 = CARTESIAN_POINT ( 'NONE',  ( -38.61942532600000533, 1444.188087375399846, 137.1592399812980148 ) ) ;
#41149 = ADVANCED_FACE ( 'NONE', ( #45478 ), #19115, .F. ) ;
#41150 = CARTESIAN_POINT ( 'NONE',  ( 0.4193190673965659920, 1494.284500131298500, 220.2488346745992942 ) ) ;
#41151 = CIRCLE ( 'NONE', #59077, 1.999999999999999556 ) ;
#41152 = DIRECTION ( 'NONE',  ( 0.000000000000000000, -1.000000000000000000, 0.000000000000000000 ) ) ;
#41153 = CARTESIAN_POINT ( 'NONE',  ( -23.84859116899999876, 1446.062256459500077, 214.1355555763180121 ) ) ;
#41154 = CARTESIAN_POINT ( 'NONE',  ( 0.8957613442250700331, 1452.912621291000050, 183.3566031976109798 ) ) ;
#41155 = ADVANCED_FACE ( 'NONE', ( #19685 ), #16920, .F. ) ;
#41157 = CARTESIAN_POINT ( 'NONE',  ( -8.022767810159999513, 1384.891328718069872, 218.7875262018289959 ) ) ;
#41156 = CARTESIAN_POINT ( 'NONE',  ( -3.260357166894999992, 1517.133889586189980, 216.8465783791270098 ) ) ;
#41158 = CARTESIAN_POINT ( 'NONE',  ( -9.288805682565799415, 1448.817640831179915, 209.5382110545150169 ) ) ;
#41159 = CARTESIAN_POINT ( 'NONE',  ( 31.81407709659918481, 1522.644714754857659, 221.9534378623320379 ) ) ;
#41160 = ORIENTED_EDGE ( 'NONE', *, *, #63318, .F. ) ;
#41161 = CARTESIAN_POINT ( 'NONE',  ( 1.708102589285000139, 1517.199196846569976, 202.5572672468869939 ) ) ;
#41162 = CARTESIAN_POINT ( 'NONE',  ( -16.48353621536499958, 1512.679339245399888, 220.7760042011669839 ) ) ;
#41163 = VECTOR ( 'NONE', #81535, 1000.000000000000114 ) ;
#41164 = CARTESIAN_POINT ( 'NONE',  ( -0.04665562252469999949, 1457.821573612329985, 229.0784639932980156 ) ) ;
#41165 = CARTESIAN_POINT ( 'NONE',  ( 22.77748398619999648, 1450.072706315450205, 219.0539608951079913 ) ) ;
#41166 = CARTESIAN_POINT ( 'NONE',  ( 10.81897510151069852, 1461.808313873119914, 210.9528785559000141 ) ) ;
#41167 = CARTESIAN_POINT ( 'NONE',  ( 11.60004869885203682, 0.000000000000000000, 134.0999999980979851 ) ) ;
#41168 = EDGE_CURVE ( 'NONE', #100091, #79464, #86278, .T. ) ;
#41169 = CARTESIAN_POINT ( 'NONE',  ( 26.26611707621578873, 1450.753935678440257, 136.6023704354048220 ) ) ;
#41170 = CARTESIAN_POINT ( 'NONE',  ( 3.775314256393730084, 1507.374707593759922, 220.2027404254530154 ) ) ;
#41171 = CARTESIAN_POINT ( 'NONE',  ( 29.68682906300000113, 1435.534167576209938, 135.1977161657979991 ) ) ;
#41172 = CARTESIAN_POINT ( 'NONE',  ( 38.15215272849530237, 1448.684869598680052, 136.3987171033640209 ) ) ;
#41173 = CARTESIAN_POINT ( 'NONE',  ( 20.00077711682029857, 1506.539416727767502, 218.4579560628022818 ) ) ;
#41174 = LINE ( 'NONE', #32765, #57449 ) ;
#41175 = CARTESIAN_POINT ( 'NONE',  ( -108.4333501240000004, 1387.441885140250179, 297.7992663317590427 ) ) ;
#41176 = CARTESIAN_POINT ( 'NONE',  ( -17.45221183250000152, 1413.296611998330036, 225.8619397856980129 ) ) ;
#41177 = CARTESIAN_POINT ( 'NONE',  ( 19.00259723422722047, 1526.382868172571079, 185.3307583833850458 ) ) ;
#41178 = ADVANCED_FACE ( 'NONE', ( #57175 ), #58969, .T. ) ;
#41179 = CARTESIAN_POINT ( 'NONE',  ( -29.80092322115732983, 1462.394957644986334, 269.4686990303187599 ) ) ;
#41180 = EDGE_LOOP ( 'NONE', ( #82433, #105863, #42237, #13980 ) ) ;
#41181 = CARTESIAN_POINT ( 'NONE',  ( -8.224133852202001549, 1439.811765298699811, 205.6917440491770037 ) ) ;
#41182 = CARTESIAN_POINT ( 'NONE',  ( 4.144681717681806710, 1507.117986406631189, 186.7896738910754380 ) ) ;
#41183 = EDGE_CURVE ( 'NONE', #51752, #106043, #70263, .T. ) ;
#41184 = CARTESIAN_POINT ( 'NONE',  ( -3.487585252374380218, 1508.551704408389924, 213.9544597463709863 ) ) ;
#41185 = DIRECTION ( 'NONE',  ( 0.9098001251504946874, -0.3556210061633369723, 0.2140033463558929649 ) ) ;
#41186 = CIRCLE ( 'NONE', #60873, 2.000000000000011102 ) ;
#41187 = CARTESIAN_POINT ( 'NONE',  ( -0.8265242355799999885, 1408.941923249630008, 187.0792671738979891 ) ) ;
#41188 = CARTESIAN_POINT ( 'NONE',  ( -12.95896253566151834, 1444.901424241698123, 186.2279615641708972 ) ) ;
#41189 = B_SPLINE_SURFACE_WITH_KNOTS ( 'NONE', 3, 5, ( 
 ( #93880, #59215, #92238, #77111, #34537, #16597 ),
 ( #101722, #7681, #110143, #41837, #83838, #42952 ),
 ( #68719, #419, #85472, #42385, #102824, #40737 ),
 ( #94427, #76540, #17703, #51907, #75993, #17146 ) ),
 .UNSPECIFIED., .F., .F., .F.,
 ( 4, 4 ),
 ( 6, 6 ),
 ( 5.479561955080000324, 5.505632800979999963 ),
 ( 0.000000000000000000, 1.000000000000000000 ),
 .UNSPECIFIED. ) ;
#41190 = CARTESIAN_POINT ( 'NONE',  ( -16.66936639845668822, 1523.456872492435195, 180.4828114240741570 ) ) ;
#41191 = CARTESIAN_POINT ( 'NONE',  ( 2.807700783748780182, 1495.041702816110046, 220.3586040259340280 ) ) ;
#41192 = EDGE_CURVE ( 'NONE', #25016, #57781, #16835, .T. ) ;
#41193 = CARTESIAN_POINT ( 'NONE',  ( -4.193705225835856254, 1415.995780155225248, 232.4011042397820859 ) ) ;
#41194 = CARTESIAN_POINT ( 'NONE',  ( 17.74176952027255183, 1410.893628039027362, 223.3341983228125400 ) ) ;
#41195 = CARTESIAN_POINT ( 'NONE',  ( 25.28186086219999851, 1435.386619864120121, 135.7772238486980143 ) ) ;
#41196 = CARTESIAN_POINT ( 'NONE',  ( -12.94642120436389554, 1442.917301946143425, 169.4295745761914702 ) ) ;
#41198 = ORIENTED_EDGE ( 'NONE', *, *, #41579, .F. ) ;
#41197 = CARTESIAN_POINT ( 'NONE',  ( 18.01510524478549868, 1424.528298123270133, 225.6033285300410114 ) ) ;
#41199 = CIRCLE ( 'NONE', #39443, 0.9999999999999952260 ) ;
#41200 = CARTESIAN_POINT ( 'NONE',  ( 0.2612772523340000097, 1416.851343897030119, 190.7759414237980025 ) ) ;
#41201 = CARTESIAN_POINT ( 'NONE',  ( 1.702416261868870073, 1493.957958506549858, 220.1113518634800243 ) ) ;
#41202 = EDGE_LOOP ( 'NONE', ( #38510, #38864, #54094, #99451 ) ) ;
#41203 = ORIENTED_EDGE ( 'NONE', *, *, #20828, .F. ) ;
#41204 = CARTESIAN_POINT ( 'NONE',  ( 18.10358820054819873, 1416.830086716310007, 209.0369172249700114 ) ) ;
#41205 = CARTESIAN_POINT ( 'NONE',  ( -19.98413504154972387, 1526.143142182167139, 233.2906832176993817 ) ) ;
#41207 = CARTESIAN_POINT ( 'NONE',  ( 1.651430464342579896, 1456.566497830990102, 219.6140531495319976 ) ) ;
#41206 = CARTESIAN_POINT ( 'NONE',  ( 2.501002156060000203, 1456.165277925289956, 219.0283583277490038 ) ) ;
#41208 = CARTESIAN_POINT ( 'NONE',  ( -3.311233732019999820, 1444.392778043689987, 217.8868263135390180 ) ) ;
#41209 = CARTESIAN_POINT ( 'NONE',  ( -11.46499703930000003, 1433.136224980220049, 151.2988949122980102 ) ) ;
#41210 = CARTESIAN_POINT ( 'NONE',  ( -12.29038035583180033, 1378.270906290520088, 210.0591904295070265 ) ) ;
#41211 = CARTESIAN_POINT ( 'NONE',  ( 9.525081731767038207, 1464.196465044419938, 211.5190840894209998 ) ) ;
#41212 = CARTESIAN_POINT ( 'NONE',  ( 7.301745199710000023, 1423.622635854230111, 213.2704416234889777 ) ) ;
#41213 = CARTESIAN_POINT ( 'NONE',  ( -24.65468602429999834, 1440.334300524250011, 210.6770184181980028 ) ) ;
#41214 = SPHERICAL_SURFACE ( 'NONE', #53364, 2.000000000000000000 ) ;
#41215 = CARTESIAN_POINT ( 'NONE',  ( 1.610950544670000095, 1451.193671323529998, 183.0676007769979776 ) ) ;
#41216 = CARTESIAN_POINT ( 'NONE',  ( 7.340269731169999368, 1361.836778001489847, 207.6218459616989946 ) ) ;
#41217 = CARTESIAN_POINT ( 'NONE',  ( -27.81626572861782520, 1509.996270472295009, 197.8821087052356518 ) ) ;
#41219 = VERTEX_POINT ( 'NONE', #25171 ) ;
#41218 = CARTESIAN_POINT ( 'NONE',  ( -2.747389875506000363E-09, 1415.237975642199899, 243.5845164730120018 ) ) ;
#41220 = ORIENTED_EDGE ( 'NONE', *, *, #4136, .F. ) ;
#41221 = CARTESIAN_POINT ( 'NONE',  ( -11.83934983080530046, 1430.503885545030016, 149.6717847768150023 ) ) ;
#41222 = EDGE_CURVE ( 'NONE', #101083, #96085, #6154, .T. ) ;
#41223 = CARTESIAN_POINT ( 'NONE',  ( -13.81174872492939976, 1503.065987535760087, 227.5153026160529919 ) ) ;
#41224 = CARTESIAN_POINT ( 'NONE',  ( -5.377271149169999376, 1473.660644874129957, 270.2871877486979884 ) ) ;
#41225 = CARTESIAN_POINT ( 'NONE',  ( -1.549353400650000046, 1416.067629296030191, 227.8551223243979962 ) ) ;
#41226 =( BOUNDED_CURVE ( )  B_SPLINE_CURVE ( 3, ( #61550, #10017, #53144, #87282 ),
 .UNSPECIFIED., .F., .F. ) 
 B_SPLINE_CURVE_WITH_KNOTS ( ( 4, 4 ),
 ( 2.356485375018650075, 3.926596517583369916 ),
 .UNSPECIFIED. ) 
 CURVE ( )  GEOMETRIC_REPRESENTATION_ITEM ( )  RATIONAL_B_SPLINE_CURVE ( ( 1.000000000000000000, 0.8048993259288232949, 0.8048993259288232949, 1.000000000000000000 ) ) 
 REPRESENTATION_ITEM ( '' )  );
#41227 = CARTESIAN_POINT ( 'NONE',  ( -109.7187440601658466, 1348.229899472568604, 310.4276940313056343 ) ) ;
#41228 = CARTESIAN_POINT ( 'NONE',  ( 39.85254359737009366, 1448.755683825020014, 135.8476807215540134 ) ) ;
#41229 = CARTESIAN_POINT ( 'NONE',  ( 15.29461995089999959, 1453.313060387329870, 195.2084026670979995 ) ) ;
#41230 = CARTESIAN_POINT ( 'NONE',  ( -9.094257307190000361, 1384.874748762100126, 199.9429999480290121 ) ) ;
#41231 = CARTESIAN_POINT ( 'NONE',  ( 17.85932443592169960, 1430.949825052579854, 205.3160887855020178 ) ) ;
#41232 = DIRECTION ( 'NONE',  ( 0.000000000000000000, 0.000000000000000000, -1.000000000000000000 ) ) ;
#41233 = CARTESIAN_POINT ( 'NONE',  ( 9.984115569218559472, 1365.258395869460173, 210.6218459616991936 ) ) ;
#41234 = CARTESIAN_POINT ( 'NONE',  ( -12.14973932564840098, 1406.923408263400006, 267.7908327071809822 ) ) ;
#41235 = VERTEX_POINT ( 'NONE', #89932 ) ;
#41236 = LINE ( 'NONE', #14910, #96707 ) ;
#41237 = VERTEX_POINT ( 'NONE', #99423 ) ;
#41238 = EDGE_LOOP ( 'NONE', ( #60448, #45842, #45688, #82971, #30050 ) ) ;
#41239 = CARTESIAN_POINT ( 'NONE',  ( -2.477373643995000485, 1516.891731298979948, 212.0030687278169808 ) ) ;
#41240 = EDGE_CURVE ( 'NONE', #58183, #32684, #91593, .T. ) ;
#41241 = CARTESIAN_POINT ( 'NONE',  ( 4.952140499603463475, 1422.530607013576628, 184.3907845083923007 ) ) ;
#41242 = CARTESIAN_POINT ( 'NONE',  ( -21.63849897585056681, 1517.051704408389924, 215.5584779397909188 ) ) ;
#41244 = DIRECTION ( 'NONE',  ( 0.000000000000000000, 0.000000000000000000, -1.000000000000000000 ) ) ;
#41243 = CARTESIAN_POINT ( 'NONE',  ( -4.997250192034999650, 1516.727068157269969, 212.3866247496169990 ) ) ;
#41245 = CARTESIAN_POINT ( 'NONE',  ( -19.45227738350000024, 1485.491809083029921, 189.8902479364980138 ) ) ;
#41246 = VECTOR ( 'NONE', #74669, 1000.000000000000000 ) ;
#41247 = CARTESIAN_POINT ( 'NONE',  ( -17.88319679657989880, 1498.319102843910059, 229.4271407816139856 ) ) ;
#41248 = VERTEX_POINT ( 'NONE', #108395 ) ;
#41249 = CARTESIAN_POINT ( 'NONE',  ( -105.6883447910000058, 1379.461008902830145, 304.2218452742590102 ) ) ;
#41250 = B_SPLINE_CURVE_WITH_KNOTS ( 'NONE', 3,
 ( #36058, #10856, #95404, #80811, #20881, #104352, #97067 ),
 .UNSPECIFIED., .F., .F.,
 ( 4, 3, 4 ),
 ( 5.821231011620000118, 13.81665860822499781, 14.11476443669999981 ),
 .UNSPECIFIED. ) ;
#41251 = CARTESIAN_POINT ( 'NONE',  ( -0.7538707734179979081, 1516.719999691880048, 202.1833671473370089 ) ) ;
#41252 = EDGE_CURVE ( 'NONE', #58610, #80101, #32924, .T. ) ;
#41253 = CARTESIAN_POINT ( 'NONE',  ( -0.7264217198650000373, 1457.949969450530034, 229.7272997097979896 ) ) ;
#41254 = CARTESIAN_POINT ( 'NONE',  ( -33.65891623492240115, 1384.565199592660065, 207.7968822506400102 ) ) ;
#41255 = CARTESIAN_POINT ( 'NONE',  ( -44.43459082169709973, 1440.913052735869996, 270.0922309517229678 ) ) ;
#41256 = AXIS2_PLACEMENT_3D ( 'NONE', #19152, #8014, #76331 ) ;
#41257 = LINE ( 'NONE', #16026, #86510 ) ;
#41259 = ORIENTED_EDGE ( 'NONE', *, *, #80164, .T. ) ;
#41258 = CARTESIAN_POINT ( 'NONE',  ( 30.17514222261037915, 1525.712835404586031, 196.9772729963927702 ) ) ;
#41260 = CARTESIAN_POINT ( 'NONE',  ( -11.86654302293240093, 1432.368244302329913, 149.9823801698750003 ) ) ;
#41261 = CARTESIAN_POINT ( 'NONE',  ( -28.27139721233027458, 1526.382868172864164, 219.5606225550389468 ) ) ;
#41262 = CARTESIAN_POINT ( 'NONE',  ( 1.125466269979470191, 1425.802411463860153, 191.1258191377030187 ) ) ;
#41263 = CARTESIAN_POINT ( 'NONE',  ( -24.91674476280000050, 1436.144616349540001, 137.7434857531980015 ) ) ;
#41264 = AXIS2_PLACEMENT_3D ( 'NONE', #100283, #34176, #41489 ) ;
#41265 = CARTESIAN_POINT ( 'NONE',  ( -24.36140358970000008, 1441.380331911939948, 211.7116804488580044 ) ) ;
#41266 = CARTESIAN_POINT ( 'NONE',  ( -2.476170635034999901, 1516.819260244609950, 210.8389306816469855 ) ) ;
#41267 = CARTESIAN_POINT ( 'NONE',  ( -68.77502866369999879, 1379.747951483830093, 280.1868250462589458 ) ) ;
#41268 = CARTESIAN_POINT ( 'NONE',  ( -2.455930012020000053, 1497.729421728190118, 200.9736040853090060 ) ) ;
#41269 = CARTESIAN_POINT ( 'NONE',  ( 4.943223444412789824, 1441.096092932190004, 216.6493757176620250 ) ) ;
#41270 = CARTESIAN_POINT ( 'NONE',  ( -13.13054719229040046, 1414.913526854310021, 220.1717702895670072 ) ) ;
#41271 = EDGE_CURVE ( 'NONE', #71251, #80762, #42526, .T. ) ;
#41272 = CARTESIAN_POINT ( 'NONE',  ( -0.01319654689839849966, 1516.941178807709775, 206.8296289214069930 ) ) ;
#41273 = ORIENTED_EDGE ( 'NONE', *, *, #2427, .T. ) ;
#41274 = CARTESIAN_POINT ( 'NONE',  ( -2.485061398530379773, 1451.956239371870197, 184.6525714882409943 ) ) ;
#41275 = FACE_OUTER_BOUND ( 'NONE', #23471, .T. ) ;
#41276 = CARTESIAN_POINT ( 'NONE',  ( -19.62068968046267514, 1457.036717113561963, 225.8553759409991244 ) ) ;
#41277 = ORIENTED_EDGE ( 'NONE', *, *, #11073, .T. ) ;
#41279 = AXIS2_PLACEMENT_3D ( 'NONE', #17717, #77664, #25026 ) ;
#41278 = CARTESIAN_POINT ( 'NONE',  ( -28.54400548274723093, 1526.382868172864164, 198.4417401822219631 ) ) ;
#41280 = EDGE_CURVE ( 'NONE', #5427, #43546, #825, .T. ) ;
#41281 = CARTESIAN_POINT ( 'NONE',  ( 33.93019615848955084, 1501.977400791986611, 220.5829544587961095 ) ) ;
#41282 = CARTESIAN_POINT ( 'NONE',  ( -4.117520247412672418, 1441.433507593749027, 184.2698927454183035 ) ) ;
#41283 = DIRECTION ( 'NONE',  ( 0.000000000000000000, 6.123233995736769734E-17, 1.000000000000000000 ) ) ;
#41284 = DIRECTION ( 'NONE',  ( 1.836970198721029688E-16, 1.000000000000000000, -2.953460612019999929E-19 ) ) ;
#41285 = CARTESIAN_POINT ( 'NONE',  ( 8.809986217320000534, 1488.981908579989977, 201.8653081004390231 ) ) ;
#41286 = DIRECTION ( 'NONE',  ( -1.065814103640000080E-14, -1.000000000000000000, -2.775557561560010037E-16 ) ) ;
#41287 = DIRECTION ( 'NONE',  ( 1.000000000000000000, 0.000000000000000000, 0.000000000000000000 ) ) ;
#41288 = EDGE_CURVE ( 'NONE', #90688, #107214, #50399, .T. ) ;
#41290 = CARTESIAN_POINT ( 'NONE',  ( 41.20351478744365181, 1440.849789031605269, 135.3869887111343076 ) ) ;
#41289 = CARTESIAN_POINT ( 'NONE',  ( 6.946748518954999341, 1516.983995446890049, 214.1250666973070054 ) ) ;
#41291 = CARTESIAN_POINT ( 'NONE',  ( 15.94345596297699963, 1409.469818137940138, 225.2684692625209948 ) ) ;
#41292 = CARTESIAN_POINT ( 'NONE',  ( -2.290256301855000398, 1517.170721208160103, 216.0730210990169837 ) ) ;
#41293 = ORIENTED_EDGE ( 'NONE', *, *, #106335, .F. ) ;
#41294 = CARTESIAN_POINT ( 'NONE',  ( -12.78776258890000150, 1416.851343897030119, 195.9645815389980044 ) ) ;
#41295 = CARTESIAN_POINT ( 'NONE',  ( 11.75869035672759999, 1522.051704408389924, 227.2994842695800060 ) ) ;
#41296 = CARTESIAN_POINT ( 'NONE',  ( 1.506876827590000190, 1419.080345689929800, 184.9340756889980071 ) ) ;
#41297 = EDGE_CURVE ( 'NONE', #19483, #9730, #97012, .T. ) ;
#41298 = CARTESIAN_POINT ( 'NONE',  ( -3.439961641710000517, 1475.703222190290035, 218.9903650269789921 ) ) ;
#41300 = B_SPLINE_CURVE_WITH_KNOTS ( 'NONE', 5,
 ( #17668, #102249, #101132, #102785, #110106, #24427 ),
 .UNSPECIFIED., .F., .F.,
 ( 6, 6 ),
 ( 0.000000000000000000, 1.000000000000000000 ),
 .UNSPECIFIED. ) ;
#41299 = CARTESIAN_POINT ( 'NONE',  ( 2.744860007233061339, 1525.790287071781222, 177.2996080414773132 ) ) ;
#41301 = CARTESIAN_POINT ( 'NONE',  ( -1.247057868944360104, 1423.218537098029856, 191.2427100806079920 ) ) ;
#41302 = CARTESIAN_POINT ( 'NONE',  ( -11.25721726106180043, 1471.236964352069890, 207.2321767610409893 ) ) ;
#41303 = CARTESIAN_POINT ( 'NONE',  ( -7.460430899790702064, 1508.409396344885863, 219.6019905338215494 ) ) ;
#41304 = CARTESIAN_POINT ( 'NONE',  ( 17.66103185136753595, 1423.256579349406593, 226.2635097096822960 ) ) ;
#41305 = CARTESIAN_POINT ( 'NONE',  ( 18.34194392892833392, 1425.469024528380032, 224.8862135115603564 ) ) ;
#41306 = CARTESIAN_POINT ( 'NONE',  ( -22.08622291482367572, 1523.382868172864164, 184.4183880513178053 ) ) ;
#41307 = CARTESIAN_POINT ( 'NONE',  ( 43.48089572550729542, 1440.913060357599988, 263.7552761525859637 ) ) ;
#41309 = CARTESIAN_POINT ( 'NONE',  ( 4.328706393743970260, 1515.093143318830244, 207.9156808863739911 ) ) ;
#41308 = CARTESIAN_POINT ( 'NONE',  ( -9.699590169216451230, 1472.031374714349795, 212.1565849597349995 ) ) ;
#41310 = FACE_OUTER_BOUND ( 'NONE', #83165, .T. ) ;
#41311 = ORIENTED_EDGE ( 'NONE', *, *, #69228, .T. ) ;
#41312 = VERTEX_POINT ( 'NONE', #77013 ) ;
#41313 = B_SPLINE_CURVE_WITH_KNOTS ( 'NONE', 3,
 ( #38037, #62733, #29625, #55403, #37486, #29088, #27978, #63273, #98481, #2263, #28534, #96854, #63809 ),
 .UNSPECIFIED., .F., .F.,
 ( 4, 3, 3, 3, 4 ),
 ( 0.9322656447709229965, 0.9706014474725359609, 1.008994579606269815, 1.040095003257240025, 1.047387711740000116 ),
 .UNSPECIFIED. ) ;
#41314 = B_SPLINE_CURVE_WITH_KNOTS ( 'NONE', 3,
 ( #96591, #45661, #79799, #35012 ),
 .UNSPECIFIED., .F., .F.,
 ( 4, 4 ),
 ( 0.000000000000000000, 0.0002220129587134776392 ),
 .UNSPECIFIED. ) ;
#41315 = EDGE_CURVE ( 'NONE', #60256, #1490, #108953, .T. ) ;
#41316 = CARTESIAN_POINT ( 'NONE',  ( -19.67975695282724402, 1485.238170136274221, 190.3376061193639828 ) ) ;
#41317 = CARTESIAN_POINT ( 'NONE',  ( -14.17032501240000109, 1507.703614819789891, 209.3618925486269973 ) ) ;
#41318 = CARTESIAN_POINT ( 'NONE',  ( 11.60172759230599837, 1502.019123038000089, 211.3760841748210169 ) ) ;
#41319 = CARTESIAN_POINT ( 'NONE',  ( 9.314155605375137981, 1440.512919951834874, 186.6528570261106665 ) ) ;
#41320 = ADVANCED_FACE ( 'NONE', ( #87051 ), #98201, .F. ) ;
#41321 = CIRCLE ( 'NONE', #32366, 1.848467280504758614 ) ;
#41322 = CARTESIAN_POINT ( 'NONE',  ( 9.555172118568348694, 1422.588896727079828, 212.6615495601689929 ) ) ;
#41323 = DIRECTION ( 'NONE',  ( -5.980589973904019347E-17, 1.000000000000000000, -1.736889445713099699E-16 ) ) ;
#41324 = CARTESIAN_POINT ( 'NONE',  ( -4.282704111109999268, 1515.349907855090123, 208.0217043178890037 ) ) ;
#41325 = CARTESIAN_POINT ( 'NONE',  ( -55.82031311308629995, 1383.802674022899964, 273.0220194663820052 ) ) ;
#41326 = CARTESIAN_POINT ( 'NONE',  ( -14.46927441969999961, 1471.316885393030134, 193.6194182199980105 ) ) ;
#41327 = CARTESIAN_POINT ( 'NONE',  ( -26.92366826496267151, 1508.479997278783912, 212.0212860892887647 ) ) ;
#41329 = CLOSED_SHELL ( 'NONE', ( #58471, #13051, #27636, #52015, #6304, #72642, #23330, #87945, #84548, #41374, #4256, #29795, #51079, #25376, #93883, #109561, #12226, #105359, #90306, #16720, #77524, #33985, #33055, #94786, #17231, #100761, #55232, #106788, #35386, #104975, #105817, #95434, #91061, #85065, #59094, #39757, #69895, #77487, #108905, #11497, #108548, #74689, #28520, #88389, #5649, #21264, #92139, #8673, #73359, #13160, #5169, #75094, #57043, #81558, #25307, #20716, #7754, #5591, #7800, #78844, #8305, #45464, #39791, #68920, #11689, #24984, #39294, #55567, #40552, #67859, #96019, #100334, #99395, #19328, #45138, #70642, #38355, #14093, #79015, #84913, #4041, #58254, #33224, #14455, #103460, #53013, #106376, #4266, #54621, #76316, #103493, #98169, #73540, #95876, #67492, #90218, #43972, #106567, #5625, #28916, #53455, #64211, #43360, #33797, #58353, #87202, #92449, #106823, #37421, #2920, #101828, #9814, #36467, #13278, #21885, #62537, #98196, #55732, #13907, #12406, #61162, #2365, #37744, #52427, #7779, #44894, #24680, #16253, #106873, #2207, #38000, #90059, #15233, #48867, #71999, #13329, #46069, #107912, #87350, #38647, #57299, #80971, #59605, #24956, #79737, #74683, #22807, #13679, #83729, #98435, #60405, #93078, #29608, #82381, #104124, #102046, #91947, #30924, #53205, #39267, #94151, #19853, #95389, #88387, #15112, #3267, #30901, #98743, #45134, #80840, #78692, #53601, #84853, #95124, #2876, #22663, #87341, #56981, #51489, #37873, #50798, #98288, #36983, #94598, #41900, #33743, #41862, #99303, #18650, #18935, #10607, #91067, #75069, #102052, #33081, #87470, #88412, #59065, #107155, #97693, #13207, #66228, #62516, #107140, #26398, #89910, #55634, #2104, #23922, #38656, #70779, #3931, #37732, #73945, #96553, #18628, #16465, #73813, #46785, #69965, #90437, #86903, #96797, #102947, #106977, #86418, #105464, #87951, #110330, #4383, #95376, #27185, #86082, #81615, #68749, #39133, #54987, #78295, #93307, #109135, #7953, #60531, #63784, #5514, #43947, #62560, #101458, #65836, #11117, #75212, #87957, #43264, #10934, #28412, #54078, #76355, #10400, #97551, #108983, #9447, #70635, #97977, #56155, #67927, #50904, #85654, #51631, #67377, #50178, #105636, #17481, #76444, #22526, #68710, #36483, #1019, #9155, #42228, #100079, #98519, #5785, #53710, #1386, #78359, #19578, #109636, #49769, #21424, #93238, #16246, #13062, #49056, #57696, #92488, #47388, #35708, #29787, #101299, #57676, #108529, #40469, #101399, #3114, #46921, #5709, #34179, #68625, #67317, #108687 ) ) ;
#41328 = CARTESIAN_POINT ( 'NONE',  ( -10.98084453577630093, 1433.016921785290151, 151.7694248368179899 ) ) ;
#41331 = ORIENTED_EDGE ( 'NONE', *, *, #97715, .T. ) ;
#41330 = CARTESIAN_POINT ( 'NONE',  ( 1.295798300469999997, 1456.648087910589993, 219.6777443815990125 ) ) ;
#41332 = CARTESIAN_POINT ( 'NONE',  ( 32.77044109517639470, 1525.581535527371898, 219.1629015078801785 ) ) ;
#41333 = CARTESIAN_POINT ( 'NONE',  ( -67.77685405889999970, 1381.735381056040069, 263.8753344557590026 ) ) ;
#41334 = CARTESIAN_POINT ( 'NONE',  ( 0.2196276506829989983, 1429.899695672290136, 217.4576539075590063 ) ) ;
#41335 = ORIENTED_EDGE ( 'NONE', *, *, #83922, .F. ) ;
#41336 = ORIENTED_EDGE ( 'NONE', *, *, #70277, .F. ) ;
#41337 = AXIS2_PLACEMENT_3D ( 'NONE', #77657, #20479, #18279 ) ;
#41338 = CARTESIAN_POINT ( 'NONE',  ( -21.30496379579999910, 1505.027833310889946, 212.2085733242190031 ) ) ;
#41339 = CARTESIAN_POINT ( 'NONE',  ( -3.829164872246469731, 1515.551704201149960, 206.7918886383120025 ) ) ;
#41341 = CARTESIAN_POINT ( 'NONE',  ( 1.443308927659999963, 1409.130619246129982, 231.7887507488979963 ) ) ;
#41340 = LINE ( 'NONE', #67109, #71096 ) ;
#41342 = CARTESIAN_POINT ( 'NONE',  ( -8.451623981890000081, 1463.123780996790174, 203.2630781829089983 ) ) ;
#41343 = CARTESIAN_POINT ( 'NONE',  ( -104.4199114259999845, 1380.436187834239945, 300.6363748219590093 ) ) ;
#41344 = CARTESIAN_POINT ( 'NONE',  ( -4.367937192439999450, 1447.898255911189835, 190.6350925615990093 ) ) ;
#41345 =( REPRESENTATION_RELATIONSHIP ('NONE','NONE', #14372, #72299 ) REPRESENTATION_RELATIONSHIP_WITH_TRANSFORMATION ( #67293 )SHAPE_REPRESENTATION_RELATIONSHIP( ) );
#41346 = AXIS2_PLACEMENT_3D ( 'NONE', #73014, #107150, #81381 ) ;
#41347 = CARTESIAN_POINT ( 'NONE',  ( 2.390047989679215501, 1526.069472839385980, 177.7067300826763301 ) ) ;
#41348 = CARTESIAN_POINT ( 'NONE',  ( -7.649966233313090669, 1508.551704408389924, 219.0282755267929815 ) ) ;
#41349 = CARTESIAN_POINT ( 'NONE',  ( -1.883109339810000060, 1456.914664128490131, 202.5483680118790062 ) ) ;
#41350 = B_SPLINE_CURVE_WITH_KNOTS ( 'NONE', 3,
 ( #52759, #70140, #9086, #43252, #79622, #87465, #88026, #104804, #34834, #44362, #69023, #28092, #26426, #35954, #62854, #96966, #80150, #56054, #30284, #56608, #5653, #82352, #64476, #29198, #39801, #54972, #81236, #65011, #20772, #47109, #97503, #106453, #89098, #63922, #12386, #4551, #39235 ),
 .UNSPECIFIED., .F., .F.,
 ( 4, 3, 3, 3, 3, 3, 3, 3, 3, 3, 3, 3, 4 ),
 ( -2.000000000000000000, -1.966354504360819933, -1.792372297947200099, -1.616329574349380183, -1.438982451719919897, -1.251976602293230156, -1.072120690327510006, -0.8919554514786369737, -0.7119274688212668956, -0.5279171072243049601, -0.3502797711574010542, -0.1742312679962050304, 0.000000000000000000 ),
 .UNSPECIFIED. ) ;
#41351 = CARTESIAN_POINT ( 'NONE',  ( 18.12087390759399952, 1425.009392209530006, 225.3858863835779971 ) ) ;
#41352 = CARTESIAN_POINT ( 'NONE',  ( 0.6499393709957180798, 1486.288793463719912, 197.2259022801050037 ) ) ;
#41353 = CARTESIAN_POINT ( 'NONE',  ( 7.374876521353709968, 1435.142022087859914, 204.6561785625810046 ) ) ;
#41354 = CARTESIAN_POINT ( 'NONE',  ( -2.708033116823189701, 1440.599352780370054, 162.2211373591810002 ) ) ;
#41355 = CARTESIAN_POINT ( 'NONE',  ( -2.167054049770140267, 1450.334844765639900, 183.7367558523040145 ) ) ;
#41356 = VERTEX_POINT ( 'NONE', #27700 ) ;
#41357 = CARTESIAN_POINT ( 'NONE',  ( -15.90990259576500065, 1512.830284628050094, 220.0820010595669771 ) ) ;
#41358 = CARTESIAN_POINT ( 'NONE',  ( 18.86441005807279936, 1457.254199909039926, 227.0288101415989956 ) ) ;
#41359 = CYLINDRICAL_SURFACE ( 'NONE', #76893, 26.99999999999999289 ) ;
#41360 = VECTOR ( 'NONE', #40771, 1000.000000000000000 ) ;
#41361 = B_SPLINE_CURVE_WITH_KNOTS ( 'NONE', 3,
 ( #43283, #85818, #71277, #63420 ),
 .UNSPECIFIED., .F., .F.,
 ( 4, 4 ),
 ( 0.000000000000000000, 0.0002220129587134771513 ),
 .UNSPECIFIED. ) ;
#41362 = CARTESIAN_POINT ( 'NONE',  ( -5.634996128403319327E-09, 1475.539493321410191, 266.4014118970719665 ) ) ;
#41363 = CARTESIAN_POINT ( 'NONE',  ( -19.92782875493840322, 1486.092669036620009, 191.0199231053420021 ) ) ;
#41364 = CARTESIAN_POINT ( 'NONE',  ( 1.847634168259999932, 1478.089546575790109, 198.8590796125990039 ) ) ;
#41365 = CARTESIAN_POINT ( 'NONE',  ( -105.9905438320000002, 1390.329878123639901, 307.5477013747590149 ) ) ;
#41367 =( BOUNDED_CURVE ( )  B_SPLINE_CURVE ( 3, ( #57296, #3586, #56720, #72972 ),
 .UNSPECIFIED., .F., .T. ) 
 B_SPLINE_CURVE_WITH_KNOTS ( ( 4, 4 ),
 ( 4.711836388641210682, 5.211837385119190813 ),
 .UNSPECIFIED. ) 
 CURVE ( )  GEOMETRIC_REPRESENTATION_ITEM ( )  RATIONAL_B_SPLINE_CURVE ( ( 1.000000000000000000, 0.9792748656294838483, 0.9792748656294838483, 1.000000000000000000 ) ) 
 REPRESENTATION_ITEM ( '' )  );
#41366 = AXIS2_PLACEMENT_3D ( 'NONE', #25723, #103549, #68330 ) ;
#41368 = CARTESIAN_POINT ( 'NONE',  ( -1.027602790635403940, 1484.904666167705045, 182.1256391034334001 ) ) ;
#41369 = CARTESIAN_POINT ( 'NONE',  ( -10.03857228576058702, 1362.268081971562196, 210.6218459617030021 ) ) ;
#41370 = DIRECTION ( 'NONE',  ( 0.000000000000000000, -1.000000000000000000, 0.000000000000000000 ) ) ;
#41371 = CARTESIAN_POINT ( 'NONE',  ( 0.7439185208581500230, 1429.698669720969974, 217.4034785395159872 ) ) ;
#41372 = CARTESIAN_POINT ( 'NONE',  ( -4.222176722049999498, 1443.314582379889771, 199.9747765569790090 ) ) ;
#41373 = CARTESIAN_POINT ( 'NONE',  ( 3.255809864005000165, 1516.837969789639828, 208.3644199470059846 ) ) ;
#41374 = ADVANCED_FACE ( 'NONE', ( #43956 ), #55108, .T. ) ;
#41375 = CARTESIAN_POINT ( 'NONE',  ( 6.972733162820000885, 1409.156553594830029, 222.0127823373979936 ) ) ;
#41376 = DIRECTION ( 'NONE',  ( -0.6736849260863839728, 0.000000000000000000, 0.7390186874254150995 ) ) ;
#41377 = CARTESIAN_POINT ( 'NONE',  ( 7.522034444203620218, 1425.444008626959885, 212.2045359387309702 ) ) ;
#41378 = CIRCLE ( 'NONE', #98587, 39.03564169359999170 ) ;
#41379 = CARTESIAN_POINT ( 'NONE',  ( -26.23819217370180112, 1451.260861365519986, 136.3865425181880084 ) ) ;
#41380 = EDGE_LOOP ( 'NONE', ( #84769, #22084 ) ) ;
#41381 = CARTESIAN_POINT ( 'NONE',  ( -1.492328960440000234E-08, 1421.349368237830049, 217.1428156467079873 ) ) ;
#41383 = CARTESIAN_POINT ( 'NONE',  ( -17.59268554400000184, 1410.455475221230017, 194.0661810319979850 ) ) ;
#41382 = CARTESIAN_POINT ( 'NONE',  ( -10.93477970757400008, 1492.771114947679962, 207.3280309501589898 ) ) ;
#41384 = CARTESIAN_POINT ( 'NONE',  ( -6.379043878270000079, 1461.120655808090078, 208.1971959041119931 ) ) ;
#41385 = CARTESIAN_POINT ( 'NONE',  ( -16.32163182381450284, 1508.551704408389924, 213.4489841974129831 ) ) ;
#41386 = CARTESIAN_POINT ( 'NONE',  ( -2.074953700500000053, 1486.986190320790229, 220.1252486097989731 ) ) ;
#41387 = EDGE_CURVE ( 'NONE', #3936, #103706, #54023, .T. ) ;
#41388 = CARTESIAN_POINT ( 'NONE',  ( 0.2174505330332355268, 1415.406392250408317, 233.4370360999116087 ) ) ;
#41389 = CARTESIAN_POINT ( 'NONE',  ( -11.60004869885203682, 1428.983126981193436, 134.0999999980979851 ) ) ;
#41390 = ORIENTED_EDGE ( 'NONE', *, *, #94644, .F. ) ;
#41391 = DIRECTION ( 'NONE',  ( 0.9900965937346507539, -0.1403878024439509931, 3.790652827686679061E-16 ) ) ;
#41392 = CARTESIAN_POINT ( 'NONE',  ( 13.07195414875639905, 1420.782728793139995, 229.6046982246629966 ) ) ;
#41393 = DIRECTION ( 'NONE',  ( -0.000000000000000000, -1.000000000000000000, -0.000000000000000000 ) ) ;
#41394 = ORIENTED_EDGE ( 'NONE', *, *, #39244, .T. ) ;
#41395 = ORIENTED_EDGE ( 'NONE', *, *, #109532, .F. ) ;
#41396 = CARTESIAN_POINT ( 'NONE',  ( -58.30576893479999967, 1384.922188666229886, 240.0674386386589845 ) ) ;
#41397 = CARTESIAN_POINT ( 'NONE',  ( -24.14721334009210096, 1411.115368492089829, 209.1440074703779999 ) ) ;
#41398 = EDGE_LOOP ( 'NONE', ( #59713, #48714, #31706, #100853 ) ) ;
#41399 = CARTESIAN_POINT ( 'NONE',  ( -99.47577618349998829, 1328.501055712589960, 311.8286840973790390 ) ) ;
#41400 = CARTESIAN_POINT ( 'NONE',  ( -44.91577693743988675, 1434.529242213127191, 266.2100843130238559 ) ) ;
#41401 = MECHANICAL_DESIGN_GEOMETRIC_PRESENTATION_REPRESENTATION (  '', ( #75387 ), #93181 ) ;
#41402 = CARTESIAN_POINT ( 'NONE',  ( -16.67592638840000063, 1498.345628701330043, 229.8334741389980138 ) ) ;
#41403 = CARTESIAN_POINT ( 'NONE',  ( 4.832611295398050011, 1508.551704408489968, 211.6097683635340161 ) ) ;
#41404 = VERTEX_POINT ( 'NONE', #31546 ) ;
#41405 = CARTESIAN_POINT ( 'NONE',  ( 44.41064987292289601, 1449.900485654209888, 266.4579286601659760 ) ) ;
#41406 = CARTESIAN_POINT ( 'NONE',  ( -10.97729220953150175, 1391.913060387059886, 205.9368150485350100 ) ) ;
#41407 = FACE_OUTER_BOUND ( 'NONE', #27481, .T. ) ;
#41408 = CARTESIAN_POINT ( 'NONE',  ( 3.253462060665000433, 1516.874084700499907, 205.6604858388269861 ) ) ;
#41409 = CIRCLE ( 'NONE', #272, 39.03564169359999170 ) ;
#41410 = VERTEX_POINT ( 'NONE', #22563 ) ;
#41411 = CARTESIAN_POINT ( 'NONE',  ( 18.74615377336336763, 1458.186127939198286, 227.2766744674128461 ) ) ;
#41412 = CARTESIAN_POINT ( 'NONE',  ( 0.4985499550132489466, 1445.062937618880142, 199.0667931780290019 ) ) ;
#41413 = SPHERICAL_SURFACE ( 'NONE', #110546, 2.000000000000000000 ) ;
#41414 = ORIENTED_EDGE ( 'NONE', *, *, #97715, .F. ) ;
#41415 = CARTESIAN_POINT ( 'NONE',  ( 2.664669577620000229, 1448.940583421350084, 183.3789499996979941 ) ) ;
#41416 = EDGE_CURVE ( 'NONE', #33283, #105726, #52992, .T. ) ;
#41417 = CARTESIAN_POINT ( 'NONE',  ( 26.61928075775020019, 1451.917450893630075, 135.4298136244730131 ) ) ;
#41418 = CARTESIAN_POINT ( 'NONE',  ( -4.449471081727619293, 1508.551704408389924, 213.1599751400310083 ) ) ;
#41419 = CARTESIAN_POINT ( 'NONE',  ( 3.363656671351779703, 1452.795598908070133, 152.3302338689809687 ) ) ;
#41420 = ADVANCED_FACE ( 'NONE', ( #30997 ), #41983, .F. ) ;
#41421 = CARTESIAN_POINT ( 'NONE',  ( 7.986285408849999712, 1421.471180981509860, 195.9504200288989750 ) ) ;
#41422 = CARTESIAN_POINT ( 'NONE',  ( 22.29596073799999800, 1409.691652492829917, 210.9314411838980163 ) ) ;
#41423 = CARTESIAN_POINT ( 'NONE',  ( 10.06162192388379850, 1480.175689251570020, 205.9450596422540229 ) ) ;
#41424 = CARTESIAN_POINT ( 'NONE',  ( 1.791777137004639808, 1408.975630623710003, 186.8710971495229956 ) ) ;
#41426 = FACE_OUTER_BOUND ( 'NONE', #70658, .T. ) ;
#41425 = CARTESIAN_POINT ( 'NONE',  ( 31.00914578552986711, 1524.547395018738371, 196.4333264031763520 ) ) ;
#41427 = CARTESIAN_POINT ( 'NONE',  ( 4.220605471363215067, 1441.596061467261961, 170.5366720304299974 ) ) ;
#41428 = EDGE_CURVE ( 'NONE', #8770, #49915, #376, .T. ) ;
#41429 = CARTESIAN_POINT ( 'NONE',  ( -12.60774700310000007, 1379.062501030589829, 211.6870459648190206 ) ) ;
#41430 = CARTESIAN_POINT ( 'NONE',  ( -7.641777896465000275, 1513.965983108850196, 203.2025656438369765 ) ) ;
#41431 = ORIENTED_EDGE ( 'NONE', *, *, #88115, .F. ) ;
#41432 = CARTESIAN_POINT ( 'NONE',  ( 12.25440271872080089, 1415.429375168339902, 221.8382653057779805 ) ) ;
#41433 = CARTESIAN_POINT ( 'NONE',  ( 11.58617225630350056, 1432.339219477939878, 151.0669298090909933 ) ) ;
#41434 = CARTESIAN_POINT ( 'NONE',  ( -14.35518320136639936, 1509.483853104240097, 182.9676327163749932 ) ) ;
#41435 = ADVANCED_FACE ( 'NONE', ( #24237 ), #93103, .T. ) ;
#41436 = CARTESIAN_POINT ( 'NONE',  ( -10.00419192350000053, 1389.336578153429855, 201.7954106102789922 ) ) ;
#41437 = CARTESIAN_POINT ( 'NONE',  ( 9.912752747455510161, 1426.220655830240048, 209.0668641679729944 ) ) ;
#41438 = CARTESIAN_POINT ( 'NONE',  ( 10.98117345485269958, 1424.286751519139898, 203.1416149009169771 ) ) ;
#41439 = CARTESIAN_POINT ( 'NONE',  ( -10.85475431940500002, 1462.808527540379828, 207.0334558119959638 ) ) ;
#41440 = CIRCLE ( 'NONE', #107695, 1.999999999999997335 ) ;
#41441 = CARTESIAN_POINT ( 'NONE',  ( -30.40113726820000295, 1448.202175313850148, 255.3819207742980097 ) ) ;
#41442 = CARTESIAN_POINT ( 'NONE',  ( -8.927662180601840802, 1384.337400639210045, 218.6377081841249890 ) ) ;
#41443 = FACE_OUTER_BOUND ( 'NONE', #73154, .T. ) ;
#41444 = CARTESIAN_POINT ( 'NONE',  ( 40.73184307449999864, 1440.913060387330006, 268.3665355201979992 ) ) ;
#41445 = CARTESIAN_POINT ( 'NONE',  ( -9.666742485873120572, 1460.834176539050077, 209.6559978844479986 ) ) ;
#41446 = CARTESIAN_POINT ( 'NONE',  ( -15.97231422325309858, 1420.661169593619888, 229.0305620570229905 ) ) ;
#41447 = CARTESIAN_POINT ( 'NONE',  ( 10.61252713196669895, 1425.442803612520038, 197.7433300990009855 ) ) ;
#41448 = CARTESIAN_POINT ( 'NONE',  ( 8.460065138274888596, 1464.559580154269952, 214.4881923900420020 ) ) ;
#41449 = CARTESIAN_POINT ( 'NONE',  ( 11.75869035456349998, 1517.051704408389924, 227.2994842691620079 ) ) ;
#41450 = DIRECTION ( 'NONE',  ( 0.03489949670250328678, 0.9993908270190956511, 0.000000000000000000 ) ) ;
#41451 = CARTESIAN_POINT ( 'NONE',  ( -16.28816891670000189, 1409.481855779529951, 224.8535106610980279 ) ) ;
#41452 = EDGE_CURVE ( 'NONE', #69558, #25738, #14142, .T. ) ;
#41453 = VECTOR ( 'NONE', #43387, 1000.000000000000000 ) ;
#41454 = CARTESIAN_POINT ( 'NONE',  ( -8.123331533938953797, 1425.256042585743444, 209.1379764726806911 ) ) ;
#41455 = CARTESIAN_POINT ( 'NONE',  ( -33.36586802512182715, 1512.187213306747481, 201.9069332299493169 ) ) ;
#41456 = CARTESIAN_POINT ( 'NONE',  ( -17.60613511254510044, 1410.891461967290070, 193.0293542103540005 ) ) ;
#41457 = CARTESIAN_POINT ( 'NONE',  ( 1.352725010051470031E-06, 1408.141559141799917, 195.7211362560979921 ) ) ;
#41458 = CARTESIAN_POINT ( 'NONE',  ( -2.682480990172567026, 1524.330813522192102, 176.3761848884415997 ) ) ;
#41459 = DIRECTION ( 'NONE',  ( 0.03206643377773112091, -0.01102865171324966288, 0.9994248909578780093 ) ) ;
#41460 = EDGE_CURVE ( 'NONE', #42124, #97968, #6778, .T. ) ;
#41461 = CARTESIAN_POINT ( 'NONE',  ( -1.546872636329999828, 1416.828040559629926, 228.0209234244979655 ) ) ;
#41463 = VECTOR ( 'NONE', #7742, 1000.000000000000000 ) ;
#41462 = CARTESIAN_POINT ( 'NONE',  ( -18.98876737475859855, 1419.092652900649909, 207.4035108679890129 ) ) ;
#41464 = CARTESIAN_POINT ( 'NONE',  ( 0.1725211256299399865, 1478.850466436460010, 182.1437687294350098 ) ) ;
#41466 = ORIENTED_EDGE ( 'NONE', *, *, #87035, .T. ) ;
#41465 = CYLINDRICAL_SURFACE ( 'NONE', #78358, 1.000000000000000888 ) ;
#41467 = B_SPLINE_CURVE_WITH_KNOTS ( 'NONE', 3,
 ( #30088, #98403, #21675, #109029, #84361, #30654, #83809, #100057, #23344, #64840, #82152, #24436, #41262, #7108, #74878, #49128, #48015, #58077, #98948, #92210, #22771, #32312, #40707, #56977, #83261 ),
 .UNSPECIFIED., .F., .F.,
 ( 4, 3, 3, 3, 3, 3, 3, 3, 4 ),
 ( 0.000000000000000000, 0.9101832234901460206, 1.814229467067710155, 2.708290536397560011, 3.291079314230000108, 3.823282037274009948, 4.734358896883110290, 5.649465372364789850, 6.557401248809999750 ),
 .UNSPECIFIED. ) ;
#41468 = CARTESIAN_POINT ( 'NONE',  ( -27.48389906189999721, 1443.913060387330006, 168.8435737885979790 ) ) ;
#41469 = CARTESIAN_POINT ( 'NONE',  ( -6.291725117431780312, 1441.035272557219969, 154.5485622712799909 ) ) ;
#41470 = CARTESIAN_POINT ( 'NONE',  ( 11.94102939159999899, 1433.615517387009959, 149.9804957290979814 ) ) ;
#41471 = CARTESIAN_POINT ( 'NONE',  ( -41.31139259188770296, 1441.358669517780072, 134.0999999980719792 ) ) ;
#41472 = FACE_BOUND ( 'NONE', #83855, .T. ) ;
#41473 = VERTEX_POINT ( 'NONE', #76317 ) ;
#41474 = CARTESIAN_POINT ( 'NONE',  ( -1.954670228789999964, 1485.152615003790061, 198.1756555629989975 ) ) ;
#41475 = CARTESIAN_POINT ( 'NONE',  ( 9.605737541349999020, 1478.647301563190013, 203.8155412612589998 ) ) ;
#41476 = CARTESIAN_POINT ( 'NONE',  ( -16.55223816414050120, 1420.586707762020069, 203.2624066023280136 ) ) ;
#41477 = CARTESIAN_POINT ( 'NONE',  ( 19.45418216399269795, 1498.414413235519987, 218.7471445023780063 ) ) ;
#41478 = CARTESIAN_POINT ( 'NONE',  ( 18.99535453092520143, 1472.738766242029897, 202.2605984988649936 ) ) ;
#41479 = CARTESIAN_POINT ( 'NONE',  ( 30.51231035492518728, 1526.382868172863937, 200.0858385050239008 ) ) ;
#41480 = DIRECTION ( 'NONE',  ( 0.6665120492724535550, 0.000000000000000000, 0.7454942576402816545 ) ) ;
#41481 = CARTESIAN_POINT ( 'NONE',  ( 2.987353644710000200, 1434.208463618870155, 184.4752811826979837 ) ) ;
#41482 = CARTESIAN_POINT ( 'NONE',  ( -58.24912898052569687, 1385.052983837999818, 240.2872141092589970 ) ) ;
#41483 = CARTESIAN_POINT ( 'NONE',  ( -11.38914589676969946, 1391.913060387289988, 211.4051490118059746 ) ) ;
#41484 = CARTESIAN_POINT ( 'NONE',  ( 12.38845540937129996, 1427.144650814109809, 206.9724466152189848 ) ) ;
#41485 = EDGE_LOOP ( 'NONE', ( #22059, #7698, #67923, #58334 ) ) ;
#41486 = CARTESIAN_POINT ( 'NONE',  ( -28.55763293120000057, 1451.763088273230096, 135.7446055613980036 ) ) ;
#41487 = B_SPLINE_CURVE_WITH_KNOTS ( 'NONE', 3,
 ( #108115, #66158, #29761, #98065, #65034, #21336, #64500, #57201, #89666, #90205, #13489, #90768, #14048, #12952, #46595, #14608, #91325, #80730, #72884, #107022, #47679, #48238, #81808, #108675, #5109, #39824, #39264, #73438, #107573, #82379, #5679, #48797, #82919, #20797, #54999, #89122, #12411, #54048, #4167, #106608, #29892, #20387, #54590, #38845, #36660, #97118, #89810, #22020, #72478 ),
 .UNSPECIFIED., .F., .F.,
 ( 4, 3, 3, 3, 3, 3, 3, 3, 3, 3, 3, 3, 3, 3, 3, 3, 4 ),
 ( -12.57626448940000152, -12.52235396050270033, -12.19521703350000053, -11.85293761877430008, -11.51065820404859963, -11.17664517332659990, -10.83712121993539945, -10.49485907924760042, -10.14901485447220075, -9.802596852533810079, -9.456470061949168837, -9.112590635329999245, -8.869360225144090393, -8.533531448524120933, -8.201658424667050085, -7.872532270376759733, -7.548593288820000247 ),
 .UNSPECIFIED. ) ;
#41488 = CARTESIAN_POINT ( 'NONE',  ( -15.73449429231209962, 1409.488492326539927, 225.5890253965289958 ) ) ;
#41490 = EDGE_LOOP ( 'NONE', ( #96648, #88006, #79948 ) ) ;
#41489 = DIRECTION ( 'NONE',  ( 0.000000000000000000, 0.000000000000000000, -1.000000000000000000 ) ) ;
#41491 = CARTESIAN_POINT ( 'NONE',  ( 3.195005116169999937, 1472.592485613090048, 218.8132852216689912 ) ) ;
#41492 = CARTESIAN_POINT ( 'NONE',  ( -19.18702366623263345, 1410.944745777546132, 222.6092016983794508 ) ) ;
#41493 = CARTESIAN_POINT ( 'NONE',  ( -109.9783053820000021, 1384.541737252609892, 311.4424107222589555 ) ) ;
#41494 = CARTESIAN_POINT ( 'NONE',  ( -5.202920349680000278, 1495.777356229890074, 199.0561181787990108 ) ) ;
#41495 = CARTESIAN_POINT ( 'NONE',  ( -5.205339500303640676, 1440.970228300089957, 155.0076768945519916 ) ) ;
#41496 = CARTESIAN_POINT ( 'NONE',  ( 0.8350686643532190256, 1526.382868172863937, 177.3106345060153046 ) ) ;
#41497 = CARTESIAN_POINT ( 'NONE',  ( 18.23339910126861696, 1435.524963833022184, 214.8813641882896661 ) ) ;
#41498 = CARTESIAN_POINT ( 'NONE',  ( -7.012921583605000286, 1508.551704408389924, 214.6352815282469919 ) ) ;
#41499 = CARTESIAN_POINT ( 'NONE',  ( 5.037981958419999629, 1447.001160774289929, 201.0441824198890117 ) ) ;
#41500 = CARTESIAN_POINT ( 'NONE',  ( -96.14154407968899818, 1340.114449826970940, 286.9633900369476578 ) ) ;
#41501 = CARTESIAN_POINT ( 'NONE',  ( 22.65255995593916793, 1509.725411181612344, 190.0317360007398406 ) ) ;
#41502 = CARTESIAN_POINT ( 'NONE',  ( -2.039871424690000268, 1455.397043516590202, 199.5224340987989819 ) ) ;
#41503 = AXIS2_PLACEMENT_3D ( 'NONE', #83781, #7076, #41232 ) ;
#41504 = CARTESIAN_POINT ( 'NONE',  ( -1.716392779905000054, 1516.788317650260069, 206.2580580763669786 ) ) ;
#41505 = CARTESIAN_POINT ( 'NONE',  ( 4.283011301580000207, 1446.850650613710059, 156.0811442086979923 ) ) ;
#41506 = ORIENTED_EDGE ( 'NONE', *, *, #94723, .T. ) ;
#41507 = CARTESIAN_POINT ( 'NONE',  ( 14.20204665139999989, 1416.837080243330092, 196.5054414751979834 ) ) ;
#41509 = ORIENTED_EDGE ( 'NONE', *, *, #47356, .T. ) ;
#41508 = CARTESIAN_POINT ( 'NONE',  ( -68.60958769707259819, 1379.747566127410209, 280.2272292274159895 ) ) ;
#41510 = CARTESIAN_POINT ( 'NONE',  ( -17.54273015099310129, 1417.931783278020021, 206.8684746656099946 ) ) ;
#41511 = ORIENTED_EDGE ( 'NONE', *, *, #59709, .F. ) ;
#41512 = CARTESIAN_POINT ( 'NONE',  ( -16.37694617458279822, 1512.916366990779579, 220.6826468655462463 ) ) ;
#41513 = CARTESIAN_POINT ( 'NONE',  ( -22.14280421120000142, 1430.347761830729951, 200.3259973920780226 ) ) ;
#41515 = CARTESIAN_POINT ( 'NONE',  ( 16.02348580795440114, 1409.472571313510116, 192.9354709474999936 ) ) ;
#41514 = CARTESIAN_POINT ( 'NONE',  ( -11.73643846425350112, 1426.280394569859936, 144.1643001077410133 ) ) ;
#41516 = CARTESIAN_POINT ( 'NONE',  ( 4.043990307595000111, 1516.983612918759945, 211.6010928179370012 ) ) ;
#41517 = CARTESIAN_POINT ( 'NONE',  ( 41.00233898590440162, 1442.023813499529979, 136.7354043627939859 ) ) ;
#41518 = B_SPLINE_CURVE_WITH_KNOTS ( 'NONE', 3,
 ( #37363, #47421, #4845, #82105, #62609, #96723 ),
 .UNSPECIFIED., .F., .F.,
 ( 4, 2, 4 ),
 ( -1.131363979620092418E-05, 0.001067788114096002898, 0.002146889867988206399 ),
 .UNSPECIFIED. ) ;
#41519 = AXIS2_PLACEMENT_3D ( 'NONE', #60319, #94437, #51350 ) ;
#41520 = B_SPLINE_CURVE_WITH_KNOTS ( 'NONE', 3,
 ( #87422, #19079, #53283, #62811, #20194, #27502, #1221, #79039, #103664, #79581, #86860, #26962, #2885, #10718, #2340, #37004, #80112, #86309, #44889, #71196, #104215, #28052, #43763, #88525, #95267, #96368, #36453 ),
 .UNSPECIFIED., .F., .F.,
 ( 4, 2, 2, 1, 1, 1, 2, 2, 2, 2, 1, 1, 2, 2, 2, 4 ),
 ( 0.000000000000000000, 0.1250000000031543101, 0.1875000000047308546, 0.2187500000055191129, 0.2343750000059132421, 0.2421875000061094463, 0.2460937500061190775, 0.2500000000061286531, 0.3750000000060828564, 0.4375000000060604854, 0.4687500000059777738, 0.4843750000059379168, 0.4921875000059188765, 0.5000000000058997252, 0.7500000000029501956, 1.000000000000000000 ),
 .UNSPECIFIED. ) ;
#41521 =( LENGTH_UNIT ( ) NAMED_UNIT ( * ) SI_UNIT ( .MILLI., .METRE. ) );
#41522 = CARTESIAN_POINT ( 'NONE',  ( -2.233190733192939703, 1509.062325976219881, 179.3893463272050042 ) ) ;
#41523 = CARTESIAN_POINT ( 'NONE',  ( 16.95828785292910368, 1460.444661627857840, 228.7722236097744712 ) ) ;
#41524 = PRODUCT_CONTEXT ( 'NONE', #32019, 'mechanical' ) ;
#41525 = CARTESIAN_POINT ( 'NONE',  ( 4.976599076821749179, 1508.551704408389924, 211.8383979467219831 ) ) ;
#41526 = CARTESIAN_POINT ( 'NONE',  ( -33.91369265678890343, 1437.010538859309918, 136.5611844326260211 ) ) ;
#41527 = ORIENTED_EDGE ( 'NONE', *, *, #73558, .T. ) ;
#41528 = CARTESIAN_POINT ( 'NONE',  ( -18.65942339678869999, 1468.219813745079819, 201.0822072839200132 ) ) ;
#41529 = LINE ( 'NONE', #76227, #35135 ) ;
#41530 = VERTEX_POINT ( 'NONE', #93639 ) ;
#41531 = ORIENTED_EDGE ( 'NONE', *, *, #78829, .T. ) ;
#41532 = CARTESIAN_POINT ( 'NONE',  ( 1.065212260669379907, 1370.038499060255617, 211.2582246529558745 ) ) ;
#41533 = CARTESIAN_POINT ( 'NONE',  ( 10.54167417284469899, 1452.797503886009963, 210.1255431293710103 ) ) ;
#41534 = DIRECTION ( 'NONE',  ( -1.000000000000000000, 0.000000000000000000, 0.000000000000000000 ) ) ;
#41535 = CARTESIAN_POINT ( 'NONE',  ( -13.59448361969050012, 1507.983769305739997, 209.3963040809830147 ) ) ;
#41537 = CARTESIAN_POINT ( 'NONE',  ( 4.328507300020000059, 1515.100746401290053, 210.1973568915390160 ) ) ;
#41536 = AXIS2_PLACEMENT_3D ( 'NONE', #64175, #39504, #73678 ) ;
#41538 = CARTESIAN_POINT ( 'NONE',  ( 11.75889809420000098, 1441.171049811090143, 188.0932782936979777 ) ) ;
#41539 = CARTESIAN_POINT ( 'NONE',  ( 36.37832876739999932, 1435.767865857460265, 134.0999984849980251 ) ) ;
#41540 = CARTESIAN_POINT ( 'NONE',  ( -20.06562366400000030, 1485.934169092390221, 214.0282076738189971 ) ) ;
#41541 = FACE_OUTER_BOUND ( 'NONE', #53521, .T. ) ;
#41542 =( BOUNDED_CURVE ( )  B_SPLINE_CURVE ( 3, ( #12687, #46867, #72606, #106735 ),
 .UNSPECIFIED., .F., .F. ) 
 B_SPLINE_CURVE_WITH_KNOTS ( ( 4, 4 ),
 ( 3.141592653589793116, 4.712388980384689674 ),
 .UNSPECIFIED. ) 
 CURVE ( )  GEOMETRIC_REPRESENTATION_ITEM ( )  RATIONAL_B_SPLINE_CURVE ( ( 1.000000000000000000, 0.8047378541243649375, 0.8047378541243649375, 1.000000000000000000 ) ) 
 REPRESENTATION_ITEM ( '' )  );
#41543 = CARTESIAN_POINT ( 'NONE',  ( -3.263114576272079827E-31, 1414.677402202029953, 209.1218459616989946 ) ) ;
#41544 = CARTESIAN_POINT ( 'NONE',  ( -71.11512261416528702, 1384.744247007000013, 268.1821084325539459 ) ) ;
#41545 = EDGE_LOOP ( 'NONE', ( #45107, #110517, #80029, #38079 ) ) ;
#41546 = CARTESIAN_POINT ( 'NONE',  ( -2.485846037024999955, 1516.545806094630279, 201.8003900583769905 ) ) ;
#41547 = CARTESIAN_POINT ( 'NONE',  ( -5.013429394184999666, 1517.123342927159911, 207.9998951881570122 ) ) ;
#41548 = ORIENTED_EDGE ( 'NONE', *, *, #15873, .T. ) ;
#41549 = CARTESIAN_POINT ( 'NONE',  ( 11.75361422675159950, 1426.796514659970171, 145.3264244949029944 ) ) ;
#41550 = CARTESIAN_POINT ( 'NONE',  ( 3.858606800919823332, 1511.506734315490121, 217.2722139618800838 ) ) ;
#41551 = EDGE_LOOP ( 'NONE', ( #79559, #94833, #10523, #46031 ) ) ;
#41552 = CARTESIAN_POINT ( 'NONE',  ( -13.97021087459999933, 1416.254459046630018, 221.7771524697980112 ) ) ;
#41553 = ADVANCED_FACE ( 'NONE', ( #51123 ), #110829, .T. ) ;
#41554 = CARTESIAN_POINT ( 'NONE',  ( -12.29654148988069373, 1442.773887286368335, 164.4841150006940325 ) ) ;
#41555 = CARTESIAN_POINT ( 'NONE',  ( 21.44520247467869822, 1525.343727714918259, 233.4338397409588595 ) ) ;
#41556 = B_SPLINE_CURVE_WITH_KNOTS ( 'NONE', 5,
 ( #56030, #64447, #81210, #91816, #56581, #81754 ),
 .UNSPECIFIED., .F., .F.,
 ( 6, 6 ),
 ( 0.000000000000000000, 1.000000000000000000 ),
 .UNSPECIFIED. ) ;
#41557 = DIRECTION ( 'NONE',  ( -0.6736849260863840838, 0.000000000000000000, 0.7390186874254150995 ) ) ;
#41558 = CARTESIAN_POINT ( 'NONE',  ( -12.97083089140000034, 1419.897565124330185, 222.0283718032980005 ) ) ;
#41559 = CARTESIAN_POINT ( 'NONE',  ( 11.09419342938610065, 1470.256789811390036, 206.9270417508720072 ) ) ;
#41560 = CARTESIAN_POINT ( 'NONE',  ( -9.644458973949999958, 1472.935586159989953, 205.1723540604189964 ) ) ;
#41561 = CARTESIAN_POINT ( 'NONE',  ( -10.07044770968007086, 1410.639375716134509, 188.4534418757513663 ) ) ;
#41562 = CARTESIAN_POINT ( 'NONE',  ( -62.06866934319999274, 1379.739831236870032, 266.3550163871590257 ) ) ;
#41563 = CARTESIAN_POINT ( 'NONE',  ( 25.17408349516659882, 1470.080148438860078, 206.2206069998139810 ) ) ;
#41565 = CARTESIAN_POINT ( 'NONE',  ( -1.748115639427892942, 1451.913200175966722, 184.1800637472881021 ) ) ;
#41564 = CARTESIAN_POINT ( 'NONE',  ( 14.06063856439999959, 1462.621720260530083, 230.5467405163980175 ) ) ;
#41566 = DIRECTION ( 'NONE',  ( 0.7067700363771036720, 0.03085824620770448445, -0.7067700363771035610 ) ) ;
#41567 = CARTESIAN_POINT ( 'NONE',  ( -2.290886304614999869, 1517.184383877180153, 216.4605998004670084 ) ) ;
#41568 = EDGE_LOOP ( 'NONE', ( #86416, #39011, #17388 ) ) ;
#41569 = CARTESIAN_POINT ( 'NONE',  ( 18.05238084035439883, 1424.492099674600013, 224.2916874381059813 ) ) ;
#41570 = EDGE_CURVE ( 'NONE', #38120, #63746, #44388, .T. ) ;
#41571 = CARTESIAN_POINT ( 'NONE',  ( 1.353280373286737559, 1516.590829936330465, 216.8323578617266207 ) ) ;
#41572 = CARTESIAN_POINT ( 'NONE',  ( 7.334957356574999920, 1517.030858226499959, 213.7381182667970165 ) ) ;
#41573 = CARTESIAN_POINT ( 'NONE',  ( -2.923257245691396555, 1484.976779218816773, 183.1526432644509725 ) ) ;
#41574 = CARTESIAN_POINT ( 'NONE',  ( -11.60004869885203682, 1426.385955719393905, 138.5855947434999962 ) ) ;
#41576 = EDGE_LOOP ( 'NONE', ( #4872, #110779, #20724, #90614 ) ) ;
#41575 = CARTESIAN_POINT ( 'NONE',  ( -3.984081752359151185, 1515.551704408386286, 211.4519800883278720 ) ) ;
#41577 = CARTESIAN_POINT ( 'NONE',  ( 0.5988589531109999031, 1507.637957906029897, 186.4745305517980114 ) ) ;
#41578 = CARTESIAN_POINT ( 'NONE',  ( -0.3843944283460010158, 1508.551705141689808, 220.3095046180989698 ) ) ;
#41579 = EDGE_CURVE ( 'NONE', #87392, #79695, #103587, .T. ) ;
#41580 = CARTESIAN_POINT ( 'NONE',  ( -11.18028693329999967, 1425.314180641229996, 146.2031382805980115 ) ) ;
#41581 = CARTESIAN_POINT ( 'NONE',  ( -3.915802145044672944, 1515.051704408389696, 204.7920544193108014 ) ) ;
#41582 = CARTESIAN_POINT ( 'NONE',  ( 2.670692781143860106, 1446.036047624690127, 199.3704865114669929 ) ) ;
#41583 = CYLINDRICAL_SURFACE ( 'NONE', #57539, 2.000000000000003553 ) ;
#41584 = CARTESIAN_POINT ( 'NONE',  ( 8.024292235439999033, 1501.827778037190001, 207.2343894779990023 ) ) ;
#41585 = CARTESIAN_POINT ( 'NONE',  ( 6.420990609280000427, 1480.020290046689979, 205.1468653125089929 ) ) ;
#41587 = CARTESIAN_POINT ( 'NONE',  ( -16.38166793929999798, 1503.850271706589865, 209.2715074860340110 ) ) ;
#41586 = CARTESIAN_POINT ( 'NONE',  ( -21.25027440960000291, 1495.370426451130015, 226.3512016020980013 ) ) ;
#41588 = LINE ( 'NONE', #6860, #37087 ) ;
#41589 = ORIENTED_EDGE ( 'NONE', *, *, #109763, .T. ) ;
#41590 = CARTESIAN_POINT ( 'NONE',  ( -0.01327408612949850138, 1516.939877939420057, 205.6663500982469941 ) ) ;
#41591 = CARTESIAN_POINT ( 'NONE',  ( 4.991045909560000382, 1405.947371129429939, 267.5267951891979692 ) ) ;
#41592 = CARTESIAN_POINT ( 'NONE',  ( -32.23393008313268382, 1523.382868172863937, 216.8400319010857515 ) ) ;
#41593 = CARTESIAN_POINT ( 'NONE',  ( 19.25987197789999783, 1430.303363230129889, 194.0063009370979898 ) ) ;
#41594 = DIRECTION ( 'NONE',  ( 1.224646799147350002E-16, -1.836970198721029688E-16, -1.000000000000000000 ) ) ;
#41595 = CARTESIAN_POINT ( 'NONE',  ( 3.261561639834900106, 1454.263685100609791, 217.9259794001679893 ) ) ;
#41596 = CARTESIAN_POINT ( 'NONE',  ( -1.514430937639999808, 1450.835264095519960, 183.4743802333980227 ) ) ;
#41597 = ADVANCED_FACE ( 'NONE', ( #27567 ), #61212, .T. ) ;
#41598 = CARTESIAN_POINT ( 'NONE',  ( 15.44143521737569991, 1490.297619048229990, 194.0665802802050166 ) ) ;
#41599 = CARTESIAN_POINT ( 'NONE',  ( -14.75778373319999837, 1417.788090000929969, 203.2704188695489904 ) ) ;
#41600 = CARTESIAN_POINT ( 'NONE',  ( -12.89353471100000093, 1445.498271942709835, 187.5282893900980241 ) ) ;
#41601 = CARTESIAN_POINT ( 'NONE',  ( 18.89959486413309975, 1416.839692127159879, 210.6687135792209915 ) ) ;
#41602 = CARTESIAN_POINT ( 'NONE',  ( 0.04641543544835614876, 1521.951704408389787, 187.8934844801420923 ) ) ;
#41603 = CARTESIAN_POINT ( 'NONE',  ( 7.595213675750000171, 1408.121098801730113, 270.1248737335980081 ) ) ;
#41604 = CARTESIAN_POINT ( 'NONE',  ( 1.449210345413849854, 1506.595259686350118, 181.1359157415290042 ) ) ;
#41605 = CARTESIAN_POINT ( 'NONE',  ( -9.145222436720001014, 1428.303966710330087, 214.3676144197979738 ) ) ;
#41606 = CARTESIAN_POINT ( 'NONE',  ( 10.48718144549209974, 1482.007409792639919, 210.6586160354689810 ) ) ;
#41607 = CARTESIAN_POINT ( 'NONE',  ( -12.16253670259992070, 1419.838831626010915, 197.2883662463995336 ) ) ;
#41608 = CARTESIAN_POINT ( 'NONE',  ( -9.935412840599997963, 1475.334996326929968, 267.8131885700980206 ) ) ;
#41609 = CARTESIAN_POINT ( 'NONE',  ( 11.36018337630000019, 1414.996442546230128, 222.2791104318980047 ) ) ;
#41610 = CARTESIAN_POINT ( 'NONE',  ( -22.52564151159999639, 1509.699673122230024, 190.3321270482979912 ) ) ;
#41611 = CARTESIAN_POINT ( 'NONE',  ( -19.34729233231120205, 1486.470064436709890, 189.5887045964369975 ) ) ;
#41612 = CARTESIAN_POINT ( 'NONE',  ( -52.23114955023309847, 1384.729457832849903, 266.3052987280540265 ) ) ;
#41613 = CARTESIAN_POINT ( 'NONE',  ( -106.8192835944930010, 1391.913060387289988, 302.1276685733210456 ) ) ;
#41614 = CARTESIAN_POINT ( 'NONE',  ( -6.510459374210000760, 1435.947057077009958, 154.7340827710979738 ) ) ;
#41615 = DIRECTION ( 'NONE',  ( 1.755985294532469921E-16, -1.000000000000000000, 1.338183447452831989E-16 ) ) ;
#41616 = CARTESIAN_POINT ( 'NONE',  ( 4.290508147089998836, 1515.379315998089851, 209.1218459616989946 ) ) ;
#41617 = FACE_OUTER_BOUND ( 'NONE', #77147, .T. ) ;
#41618 = CARTESIAN_POINT ( 'NONE',  ( -19.54165211589999629, 1410.091287196029953, 197.8089316916980067 ) ) ;
#41619 = CARTESIAN_POINT ( 'NONE',  ( -11.87852638355199808, 1378.094445099329278, 205.8387931305373684 ) ) ;
#41620 = DIRECTION ( 'NONE',  ( 3.469446951953611033E-14, 0.000000000000000000, 1.000000000000000000 ) ) ;
#41621 = CARTESIAN_POINT ( 'NONE',  ( 10.23616613091340000, 1480.714510420149963, 206.5818171423960052 ) ) ;
#41622 = CARTESIAN_POINT ( 'NONE',  ( -1.300519565079999921E-15, 1440.444625599219989, 150.6821045058979962 ) ) ;
#41623 = CARTESIAN_POINT ( 'NONE',  ( 11.87053796280000029, 1436.297149115689990, 225.5644864776990062 ) ) ;
#41624 = CARTESIAN_POINT ( 'NONE',  ( 16.86500412378484981, 1525.697946996602695, 181.8505176293797660 ) ) ;
#41625 = CARTESIAN_POINT ( 'NONE',  ( 11.69994065948550066, 1435.514598502499894, 225.6365353821880149 ) ) ;
#41627 = CARTESIAN_POINT ( 'NONE',  ( -12.05861758146710017, 1378.268530118770059, 211.6765750960350090 ) ) ;
#41626 = CARTESIAN_POINT ( 'NONE',  ( 11.42701431400000089, 1425.487255414029960, 143.4621352013980129 ) ) ;
#41628 = CARTESIAN_POINT ( 'NONE',  ( 11.73351217698500015, 1426.698186165599964, 143.9179939085790068 ) ) ;
#41629 = SPHERICAL_SURFACE ( 'NONE', #23581, 2.000000000550000046 ) ;
#41630 = CARTESIAN_POINT ( 'NONE',  ( 0.000000000000000000, 1391.913060387289988, 209.1218459616989946 ) ) ;
#41631 = CARTESIAN_POINT ( 'NONE',  ( 10.29623711278930109, 1451.524458584259946, 207.0169742271000075 ) ) ;
#41632 = CARTESIAN_POINT ( 'NONE',  ( -17.15874760866699944, 1507.620489300740019, 224.4056177524859947 ) ) ;
#41633 = CARTESIAN_POINT ( 'NONE',  ( 2.482067860225000366, 1517.099836525840146, 203.3337487049469985 ) ) ;
#41634 = CARTESIAN_POINT ( 'NONE',  ( -18.89253556303020076, 1486.193265656730091, 200.5306675107350145 ) ) ;
#41635 = CARTESIAN_POINT ( 'NONE',  ( -9.559188306630000298, 1428.004395111430085, 145.6094494780980142 ) ) ;
#41636 = CARTESIAN_POINT ( 'NONE',  ( 16.61115974343499957, 1513.007288725360013, 197.1622553098669925 ) ) ;
#41637 = FACE_BOUND ( 'NONE', #72045, .T. ) ;
#41638 = CARTESIAN_POINT ( 'NONE',  ( -49.24962907673570811, 1526.382868172863937, 407.9033880519289710 ) ) ;
#41639 = FACE_OUTER_BOUND ( 'NONE', #88917, .T. ) ;
#41641 = VERTEX_POINT ( 'NONE', #61750 ) ;
#41640 = CARTESIAN_POINT ( 'NONE',  ( -43.26295850523789710, 1379.661000266170049, 233.4033348232310061 ) ) ;
#41642 = ORIENTED_EDGE ( 'NONE', *, *, #32901, .F. ) ;
#41643 = CARTESIAN_POINT ( 'NONE',  ( 12.02044816154730178, 1433.916076607059949, 150.4036537052579945 ) ) ;
#41644 = CARTESIAN_POINT ( 'NONE',  ( -7.930219352209999073, 1398.148604353429846, 219.9854233436979882 ) ) ;
#41645 = ORIENTED_EDGE ( 'NONE', *, *, #96661, .T. ) ;
#41646 = CARTESIAN_POINT ( 'NONE',  ( -8.796782887879999180, 1468.013265501289879, 190.7844261045989640 ) ) ;
#41647 = CARTESIAN_POINT ( 'NONE',  ( -25.61067805310000267, 1508.555235019130123, 199.5030921420180050 ) ) ;
#41648 = CARTESIAN_POINT ( 'NONE',  ( -4.678155166858989134, 1508.611350403214146, 211.6097810837688087 ) ) ;
#41650 = CARTESIAN_POINT ( 'NONE',  ( -14.32200080931659869, 1509.463657562170056, 183.0292320648689781 ) ) ;
#41649 = CARTESIAN_POINT ( 'NONE',  ( -0.5456026930049990842, 1443.714663396890046, 200.0731752116790005 ) ) ;
#41651 = CARTESIAN_POINT ( 'NONE',  ( 10.70473176346070154, 1498.104840791710103, 233.7592016339740155 ) ) ;
#41652 = B_SPLINE_CURVE_WITH_KNOTS ( 'NONE', 3,
 ( #103161, #77983, #9126, #200 ),
 .UNSPECIFIED., .F., .F.,
 ( 4, 4 ),
 ( 0.000000000000000000, 1.000000000000000000 ),
 .UNSPECIFIED. ) ;
#41653 = CARTESIAN_POINT ( 'NONE',  ( 15.28119998530000068, 1449.230982227970117, 190.0712285711979916 ) ) ;
#41654 = CARTESIAN_POINT ( 'NONE',  ( 3.048828143997139861, 1509.019527812190063, 237.9289388395170306 ) ) ;
#41655 = CARTESIAN_POINT ( 'NONE',  ( 0.5086982348340010063, 1417.713718843059951, 204.0301964970090012 ) ) ;
#41656 =( LENGTH_UNIT ( ) NAMED_UNIT ( * ) SI_UNIT ( .MILLI., .METRE. ) );
#41657 = CARTESIAN_POINT ( 'NONE',  ( 1.435225544770050154, 1395.963179567740099, 198.2036689045829974 ) ) ;
#41658 = CARTESIAN_POINT ( 'NONE',  ( 0.9667867126429999791, 1415.996778984329922, 190.4114842333980278 ) ) ;
#41659 = CARTESIAN_POINT ( 'NONE',  ( 11.56574130529999955, 1431.513070563570182, 151.1467947063979977 ) ) ;
#41660 = CARTESIAN_POINT ( 'NONE',  ( 7.951263610455001185, 1511.644799026709961, 203.1079519610169939 ) ) ;
#41661 = VERTEX_POINT ( 'NONE', #53343 ) ;
#41662 = CARTESIAN_POINT ( 'NONE',  ( 13.04027018280589978, 1434.994425313320107, 149.9717208830880111 ) ) ;
#41663 = ORIENTED_EDGE ( 'NONE', *, *, #49160, .T. ) ;
#41664 = ORIENTED_EDGE ( 'NONE', *, *, #24005, .T. ) ;
#41665 = CARTESIAN_POINT ( 'NONE',  ( 13.13752534233263347, 1444.768944423229641, 169.4002553938786946 ) ) ;
#41666 = CARTESIAN_POINT ( 'NONE',  ( -11.13364320589999856, 1462.223842109729958, 233.3656537020980011 ) ) ;
#41667 = CARTESIAN_POINT ( 'NONE',  ( -4.219439073160000220, 1446.230224797059918, 170.2811368938980081 ) ) ;
#41668 = CARTESIAN_POINT ( 'NONE',  ( 3.454748808194999743, 1516.609912606490070, 216.4448802441970088 ) ) ;
#41669 = CARTESIAN_POINT ( 'NONE',  ( -19.83859993069999916, 1467.194195006989958, 209.1218459616989946 ) ) ;
#41670 = ORIENTED_EDGE ( 'NONE', *, *, #20821, .F. ) ;
#41671 = CARTESIAN_POINT ( 'NONE',  ( -13.08802352330000041, 1503.233211745590097, 208.6735908916250253 ) ) ;
#41672 = CARTESIAN_POINT ( 'NONE',  ( -1.797631911580000130, 1415.838340813430023, 185.8046423929979767 ) ) ;
#41673 = CARTESIAN_POINT ( 'NONE',  ( -3.771520285720000309, 1380.389610323579973, 209.1218458698340044 ) ) ;
#41674 = EDGE_LOOP ( 'NONE', ( #40391, #36381, #63799, #68893 ) ) ;
#41675 = CARTESIAN_POINT ( 'NONE',  ( 6.547881374914999775, 1516.647534046129977, 205.6658385469270058 ) ) ;
#41676 = EDGE_LOOP ( 'NONE', ( #33366, #82674, #59448, #93292 ) ) ;
#41677 = CARTESIAN_POINT ( 'NONE',  ( -104.1969030333949888, 1379.825940447170069, 304.0107167257339711 ) ) ;
#41678 = DIRECTION ( 'NONE',  ( -0.02616798426500965835, 0.9993150019883683122, 0.02616798426500950916 ) ) ;
#41679 = CARTESIAN_POINT ( 'NONE',  ( -12.26976426819999944, 1410.715041853229877, 189.3560318399979963 ) ) ;
#41680 = CARTESIAN_POINT ( 'NONE',  ( 7.194888332885001070, 1513.142795523620180, 216.4219129324669950 ) ) ;
#41682 = VERTEX_POINT ( 'NONE', #35416 ) ;
#41681 = CARTESIAN_POINT ( 'NONE',  ( 0.3551244063982409993, 1416.218047878440075, 227.0926723912329805 ) ) ;
#41683 = CARTESIAN_POINT ( 'NONE',  ( 23.64707162479999880, 1434.553497323629927, 214.9047861787279885 ) ) ;
#41684 = DIRECTION ( 'NONE',  ( 0.9510565162951566398, 0.000000000000000000, 0.3090169943749382919 ) ) ;
#41685 = CARTESIAN_POINT ( 'NONE',  ( 3.156166260290000025, 1466.544008048530031, 236.1241471695980181 ) ) ;
#41686 = CARTESIAN_POINT ( 'NONE',  ( 1.779428963082609894, 1456.357349037730046, 198.6855221610310309 ) ) ;
#41687 = CARTESIAN_POINT ( 'NONE',  ( 15.04635084860490046, 1411.118372808829918, 270.3649387868580334 ) ) ;
#41688 = CARTESIAN_POINT ( 'NONE',  ( 7.722536764694999611, 1517.050041317280147, 213.7387458049869906 ) ) ;
#41689 = CARTESIAN_POINT ( 'NONE',  ( 23.98506269609999819, 1411.113951130829946, 208.3864704457530195 ) ) ;
#41690 = CARTESIAN_POINT ( 'NONE',  ( 6.253177251166829542, 1511.742575854359984, 217.9101135377649996 ) ) ;
#41691 = CARTESIAN_POINT ( 'NONE',  ( 6.766101877248090091, 1508.878901734200099, 216.3823889200130282 ) ) ;
#41692 = CARTESIAN_POINT ( 'NONE',  ( -2.476450702264999748, 1516.843453247299749, 211.4215022863270121 ) ) ;
#41693 = DIRECTION ( 'NONE',  ( 1.224646799147353454E-16, 0.000000000000000000, -1.000000000000000000 ) ) ;
#41694 = CARTESIAN_POINT ( 'NONE',  ( -16.50400130224731754, 1525.907212628473644, 236.2546788475584094 ) ) ;
#41695 = CARTESIAN_POINT ( 'NONE',  ( 2.685928792098830620, 1419.763152350967857, 137.0999999980978430 ) ) ;
#41697 = EDGE_LOOP ( 'NONE', ( #29287, #110791, #76773, #791 ) ) ;
#41696 = CARTESIAN_POINT ( 'NONE',  ( -59.23393169420000248, 1385.069165163979960, 279.9259648821590645 ) ) ;
#41698 = CARTESIAN_POINT ( 'NONE',  ( -43.88791476831470106, 1385.159211288639881, 249.3278255667920007 ) ) ;
#41699 = CARTESIAN_POINT ( 'NONE',  ( 36.92076361760000225, 1453.101244315629856, 259.2255047987979992 ) ) ;
#41700 = CARTESIAN_POINT ( 'NONE',  ( 20.27427188109263057, 1519.551704408389924, 209.5053779269578342 ) ) ;
#41701 = CARTESIAN_POINT ( 'NONE',  ( 0.9020232525101885557, 1494.156807207756856, 220.2151267746179713 ) ) ;
#41702 = CARTESIAN_POINT ( 'NONE',  ( -5.483186321339999836, 1439.280902240999922, 154.7474923763980144 ) ) ;
#41703 = CARTESIAN_POINT ( 'NONE',  ( 11.26795897200000063, 1422.300791247489997, 207.0941861644789981 ) ) ;
#41704 = CARTESIAN_POINT ( 'NONE',  ( 12.38551412853500011, 1511.900571936589813, 224.8158055378670213 ) ) ;
#41706 = CARTESIAN_POINT ( 'NONE',  ( -8.023003986910000052, 1384.895936019509918, 218.7875326659089978 ) ) ;
#41705 = CARTESIAN_POINT ( 'NONE',  ( -0.7403206051589980019, 1517.139320148880188, 216.8467205834170102 ) ) ;
#41707 = CARTESIAN_POINT ( 'NONE',  ( -9.901291130804080964, 1447.905280604810059, 209.8165545639580216 ) ) ;
#41709 = B_SPLINE_CURVE_WITH_KNOTS ( 'NONE', 5,
 ( #55345, #56439, #73234, #81611, #29032, #30107 ),
 .UNSPECIFIED., .F., .F.,
 ( 6, 6 ),
 ( 0.000000000000000000, 11.48858425020000240 ),
 .UNSPECIFIED. ) ;
#41708 = CARTESIAN_POINT ( 'NONE',  ( 31.55762699681134009, 1523.390106123591067, 221.9258384720627646 ) ) ;
#41710 = ORIENTED_EDGE ( 'NONE', *, *, #10108, .T. ) ;
#41711 = CARTESIAN_POINT ( 'NONE',  ( -4.036748876935000396, 1516.667393516340098, 202.1854475764570225 ) ) ;
#41712 = CARTESIAN_POINT ( 'NONE',  ( -27.03405935060176901, 1451.816840469728959, 135.7882905775978770 ) ) ;
#41713 = CARTESIAN_POINT ( 'NONE',  ( 12.55018658110000196, 1419.800154493929995, 223.5686081623980215 ) ) ;
#41714 = CARTESIAN_POINT ( 'NONE',  ( 38.61927353243170558, 1444.188088105049928, 137.1592452208769828 ) ) ;
#41715 = CARTESIAN_POINT ( 'NONE',  ( -5.851191224163104110, 1425.133440372593213, 186.4975237928585443 ) ) ;
#41716 = CARTESIAN_POINT ( 'NONE',  ( 4.156019621739999614, 1466.560893159090028, 218.5576475902890081 ) ) ;
#41717 = CARTESIAN_POINT ( 'NONE',  ( -24.15153490410000359, 1438.063247892820073, 212.1983423404379892 ) ) ;
#41718 = B_SPLINE_CURVE_WITH_KNOTS ( 'NONE', 5,
 ( #18566, #52216, #53893, #96412, #95852, #87467 ),
 .UNSPECIFIED., .F., .F.,
 ( 6, 6 ),
 ( -1.452596962060000108, -1.327391353722617851E-06 ),
 .UNSPECIFIED. ) ;
#41719 = CARTESIAN_POINT ( 'NONE',  ( 27.34169570636690239, 1435.928060154659988, 136.5046493440970039 ) ) ;
#41720 = CARTESIAN_POINT ( 'NONE',  ( 40.12924064502020371, 1445.213485489899995, 136.9285573339909945 ) ) ;
#41721 = CARTESIAN_POINT ( 'NONE',  ( 16.68563273243293210, 1506.380977035248861, 223.4251768443501760 ) ) ;
#41722 = PLANE ( 'NONE',  #109310 ) ;
#41723 = CARTESIAN_POINT ( 'NONE',  ( -109.5401826309999933, 1386.334633747299904, 297.2194470817590286 ) ) ;
#41724 = CARTESIAN_POINT ( 'NONE',  ( 10.95491197589999999, 1509.295614343230227, 182.0238867766980206 ) ) ;
#41725 = CARTESIAN_POINT ( 'NONE',  ( -21.35005939118667584, 1525.163457223744217, 183.8372695436867446 ) ) ;
#41726 = CARTESIAN_POINT ( 'NONE',  ( -38.63865849408829689, 1452.914171151027176, 269.5870376815316831 ) ) ;
#41727 = EDGE_LOOP ( 'NONE', ( #48183, #99906, #88110, #13476 ) ) ;
#41728 = DIRECTION ( 'NONE',  ( 0.8236474686107853049, 0.5669078173018522460, 0.01484500364079610613 ) ) ;
#41729 = CARTESIAN_POINT ( 'NONE',  ( 5.008389395533990651, 1455.723473645530021, 218.4926572036009986 ) ) ;
#41730 = B_SPLINE_CURVE_WITH_KNOTS ( 'NONE', 5,
 ( #56570, #13987, #48174, #73923, #57135, #108052 ),
 .UNSPECIFIED., .F., .F.,
 ( 6, 6 ),
 ( 176.6690472260000035, 181.4923368590000052 ),
 .UNSPECIFIED. ) ;
#41731 = CARTESIAN_POINT ( 'NONE',  ( 545.1437632904659267, 11220.04953453919370, 2113.080198834563362 ) ) ;
#41732 = CYLINDRICAL_SURFACE ( 'NONE', #45612, 2.000000000000003109 ) ;
#41733 = DIRECTION ( 'NONE',  ( -0.9455185755993178454, 0.000000000000000000, 0.3255681544571537578 ) ) ;
#41734 = CARTESIAN_POINT ( 'NONE',  ( -0.1681681984989999989, 1405.973120458222411, 137.0999999980979851 ) ) ;
#41735 = CARTESIAN_POINT ( 'NONE',  ( -8.803830034714509978, 1437.965405572629834, 209.7008996341119769 ) ) ;
#41736 = CARTESIAN_POINT ( 'NONE',  ( -4.329415281104970425, 1515.068899390480283, 212.0799436200479704 ) ) ;
#41737 = CARTESIAN_POINT ( 'NONE',  ( -10.99560576475330542, 1418.486348324287064, 229.4293017187473538 ) ) ;
#41738 = CARTESIAN_POINT ( 'NONE',  ( -20.54020145117927498, 1450.964032953651895, 144.9884247554932415 ) ) ;
#41739 = CARTESIAN_POINT ( 'NONE',  ( 2.330134126090000368, 1515.551704408389924, 212.9514660752490158 ) ) ;
#41740 = CARTESIAN_POINT ( 'NONE',  ( 25.00561208829999771, 1436.149542637609784, 137.5831833732979987 ) ) ;
#41741 = FACE_OUTER_BOUND ( 'NONE', #52307, .T. ) ;
#41742 = ORIENTED_EDGE ( 'NONE', *, *, #62736, .T. ) ;
#41743 = CARTESIAN_POINT ( 'NONE',  ( -0.3142797416910570463, 1415.426207913209964, 191.6391945173240003 ) ) ;
#41744 = CARTESIAN_POINT ( 'NONE',  ( 5.312679136500000787, 1493.059131431590231, 218.8466398904690209 ) ) ;
#41745 = ORIENTED_EDGE ( 'NONE', *, *, #21296, .F. ) ;
#41746 = ORIENTED_EDGE ( 'NONE', *, *, #79772, .T. ) ;
#41747 = CARTESIAN_POINT ( 'NONE',  ( 7.135682362486938324, 1445.817047258000457, 183.2676370014899589 ) ) ;
#41748 = CARTESIAN_POINT ( 'NONE',  ( 12.87691439960000039, 1507.477875213329980, 233.2689574170979938 ) ) ;
#41750 = CARTESIAN_POINT ( 'NONE',  ( -22.53808385540000003, 1454.461372222829823, 231.7546718361979856 ) ) ;
#41749 = CARTESIAN_POINT ( 'NONE',  ( 4.441317194709999860, 1455.879597309289920, 218.7824459606689800 ) ) ;
#41751 = CARTESIAN_POINT ( 'NONE',  ( -8.166278650529999794, 1445.984953112289986, 214.8591734898389802 ) ) ;
#41752 = CARTESIAN_POINT ( 'NONE',  ( 4.396219768207910050, 1425.786877246529912, 185.4645489200509871 ) ) ;
#41753 = CARTESIAN_POINT ( 'NONE',  ( -12.29890937187139954, 1378.335772002519889, 209.9648712015939793 ) ) ;
#41754 = CARTESIAN_POINT ( 'NONE',  ( -2.558108261982198428, 1420.763624677371809, 185.5735512640813170 ) ) ;
#41755 = CARTESIAN_POINT ( 'NONE',  ( 7.705241972949999685, 1423.949153165739972, 212.4347587744790076 ) ) ;
#41756 = CARTESIAN_POINT ( 'NONE',  ( -14.63475337105202101, 1429.908932556607169, 222.0813138987385287 ) ) ;
#41757 = FACE_BOUND ( 'NONE', #22494, .T. ) ;
#41758 = CARTESIAN_POINT ( 'NONE',  ( 2.059290213318034191, 1495.373074823845400, 220.5469163244703168 ) ) ;
#41759 = CARTESIAN_POINT ( 'NONE',  ( 7.314476403582760078, 1363.998884265407241, 208.3718459617061285 ) ) ;
#41760 = CARTESIAN_POINT ( 'NONE',  ( -24.55563515408854158, 1509.884957629476048, 191.8160791308368402 ) ) ;
#41762 = ORIENTED_EDGE ( 'NONE', *, *, #13293, .T. ) ;
#41761 = CARTESIAN_POINT ( 'NONE',  ( -14.38014760757802968, 1517.151704408390060, 209.8840156948171511 ) ) ;
#41763 = ORIENTED_EDGE ( 'NONE', *, *, #73976, .T. ) ;
#41764 = CARTESIAN_POINT ( 'NONE',  ( -33.23571934791681315, 1511.187213306747708, 198.7594255952499793 ) ) ;
#41765 = EDGE_CURVE ( 'NONE', #105162, #11259, #51742, .T. ) ;
#41766 = ADVANCED_FACE ( 'NONE', ( #62881 ), #89285, .F. ) ;
#41767 = DIRECTION ( 'NONE',  ( -1.000000000000000000, 0.000000000000000000, 0.000000000000000000 ) ) ;
#41768 = CARTESIAN_POINT ( 'NONE',  ( -5.165175409120000616, 1471.356177552630015, 269.6177996896980176 ) ) ;
#41769 = CARTESIAN_POINT ( 'NONE',  ( 12.08137332695765842, 1433.867263877792993, 147.5406663739968565 ) ) ;
#41770 = CARTESIAN_POINT ( 'NONE',  ( -113.4000000000000057, 1331.448250124730066, 321.4071368064089711 ) ) ;
#41772 = EDGE_CURVE ( 'NONE', #777, #8596, #110266, .T. ) ;
#41771 = CARTESIAN_POINT ( 'NONE',  ( 14.60782360329999996, 1431.113060387329824, 195.8937821300980033 ) ) ;
#41773 = CARTESIAN_POINT ( 'NONE',  ( -7.978157731919999662, 1384.423773816979974, 199.5156531754190041 ) ) ;
#41774 = EDGE_CURVE ( 'NONE', #77110, #5392, #76975, .T. ) ;
#41775 = FILL_AREA_STYLE_COLOUR ( '', #34194 ) ;
#41776 = CARTESIAN_POINT ( 'NONE',  ( -17.83228018670000026, 1408.913060387329779, 204.9623371014980080 ) ) ;
#41777 = CARTESIAN_POINT ( 'NONE',  ( 10.60049277610792373, 1367.947287196954221, 208.3718459617010978 ) ) ;
#41778 = CARTESIAN_POINT ( 'NONE',  ( -8.706652659834380970, 1448.779525635259915, 211.9411403000989935 ) ) ;
#41779 = CARTESIAN_POINT ( 'NONE',  ( -20.53126236479100086, 1409.661581851170013, 266.7933185538669818 ) ) ;
#41780 = CARTESIAN_POINT ( 'NONE',  ( -13.68913941687680058, 1435.559263906229944, 150.0920709695850235 ) ) ;
#41781 = EDGE_LOOP ( 'NONE', ( #66220, #98644, #44873, #53943 ) ) ;
#41782 = CARTESIAN_POINT ( 'NONE',  ( 2.472529913803023227, 1523.678648413191695, 242.8674788698241400 ) ) ;
#41783 = VERTEX_POINT ( 'NONE', #43277 ) ;
#41784 = ORIENTED_EDGE ( 'NONE', *, *, #53746, .T. ) ;
#41785 = CARTESIAN_POINT ( 'NONE',  ( -21.97938480444670262, 1506.433683733529961, 209.5040264213440082 ) ) ;
#41786 = CARTESIAN_POINT ( 'NONE',  ( 22.03465957474552184, 1522.862737210649811, 182.8300405912328870 ) ) ;
#41787 = CARTESIAN_POINT ( 'NONE',  ( 5.011367946795000528, 1516.974592746400049, 212.5716232859570027 ) ) ;
#41788 = CARTESIAN_POINT ( 'NONE',  ( -17.09529087520000346, 1470.470234692029862, 189.0510684403979837 ) ) ;
#41789 = CARTESIAN_POINT ( 'NONE',  ( -17.09199761692149977, 1498.340372574690036, 229.5617320311440039 ) ) ;
#41790 = EDGE_LOOP ( 'NONE', ( #24806, #104305, #84491, #47162 ) ) ;
#41791 = LINE ( 'NONE', #18229, #1037 ) ;
#41792 = EDGE_CURVE ( 'NONE', #4103, #108385, #1705, .T. ) ;
#41793 = CARTESIAN_POINT ( 'NONE',  ( -6.944231786295000042, 1516.882690742909972, 202.5683215544970039 ) ) ;
#41794 = CARTESIAN_POINT ( 'NONE',  ( -7.565982892814109739, 1517.051704408389924, 208.6835997737739774 ) ) ;
#41795 = EDGE_CURVE ( 'NONE', #7367, #40565, #35407, .T. ) ;
#41796 = CARTESIAN_POINT ( 'NONE',  ( -44.07146870577229691, 1384.596160883839957, 217.2312231507009983 ) ) ;
#41797 = CARTESIAN_POINT ( 'NONE',  ( -1.398741533879999999, 1408.961905518030107, 194.4353072542980101 ) ) ;
#41798 = B_SPLINE_CURVE_WITH_KNOTS ( 'NONE', 3,
 ( #26388, #19076, #45976, #17979, #86857, #52174, #45434, #2882, #10149, #86305, #37001, #61149, #71193, #95264, #105315, #9589 ),
 .UNSPECIFIED., .F., .F.,
 ( 4, 3, 3, 3, 3, 4 ),
 ( -48.30090647720000163, -47.55390437728789976, -46.79923191349099909, -45.99756063279310325, -45.16082034306089810, -44.26078367470000074 ),
 .UNSPECIFIED. ) ;
#41799 = CARTESIAN_POINT ( 'NONE',  ( -107.1491673510000027, 1387.396471041590075, 310.3410155632590204 ) ) ;
#41801 = VERTEX_POINT ( 'NONE', #77423 ) ;
#41800 = CARTESIAN_POINT ( 'NONE',  ( 15.31956813402619666, 1506.436298853404651, 193.3531772691010815 ) ) ;
#41803 = ADVANCED_FACE ( 'NONE', ( #52238 ), #86366, .T. ) ;
#41802 = DIRECTION ( 'NONE',  ( 0.8775825618903713154, 0.000000000000000000, 0.4794255386042060030 ) ) ;
#41804 = CARTESIAN_POINT ( 'NONE',  ( 26.43941340970000198, 1488.684867473429904, 213.7762971690580116 ) ) ;
#41805 = AXIS2_PLACEMENT_3D ( 'NONE', #73487, #23604, #24139 ) ;
#41806 = CARTESIAN_POINT ( 'NONE',  ( -46.04389586920228794, 1379.678237767303244, 238.4312470573368898 ) ) ;
#41807 = CARTESIAN_POINT ( 'NONE',  ( 19.91508182626240142, 1477.278815843640132, 225.3081590611470233 ) ) ;
#41808 = CARTESIAN_POINT ( 'NONE',  ( -11.49747572423030029, 1414.913060387329779, 197.9009878255399997 ) ) ;
#41809 = CARTESIAN_POINT ( 'NONE',  ( -24.64589136669999903, 1442.596336934359897, 210.7637021778280086 ) ) ;
#41810 = CARTESIAN_POINT ( 'NONE',  ( 6.563595869685000750, 1517.154223579619838, 211.4114704024570131 ) ) ;
#41811 = CARTESIAN_POINT ( 'NONE',  ( -68.30985499899999525, 1379.746831550510251, 279.0972868482590457 ) ) ;
#41812 = VECTOR ( 'NONE', #84288, 1000.000000000000227 ) ;
#41813 = CARTESIAN_POINT ( 'NONE',  ( 5.500900010980000587, 1439.900099495240056, 154.7565255832979858 ) ) ;
#41814 = FACE_OUTER_BOUND ( 'NONE', #62257, .T. ) ;
#41815 = CARTESIAN_POINT ( 'NONE',  ( 3.831162495979924643, 1440.893596831928335, 156.3803834073238477 ) ) ;
#41816 = CARTESIAN_POINT ( 'NONE',  ( 2.868112131164999745, 1516.855632454399938, 208.3641823986619954 ) ) ;
#41817 = ORIENTED_EDGE ( 'NONE', *, *, #76661, .T. ) ;
#41818 = CARTESIAN_POINT ( 'NONE',  ( -38.81202645930000017, 1436.797832437210218, 134.0999985825980332 ) ) ;
#41819 = CARTESIAN_POINT ( 'NONE',  ( -10.84042494649999888, 1471.406554747690052, 207.3881111542589792 ) ) ;
#41820 = CARTESIAN_POINT ( 'NONE',  ( -19.86778455305866942, 1456.672304896796277, 225.4249518172526052 ) ) ;
#41821 = ORIENTED_EDGE ( 'NONE', *, *, #90435, .T. ) ;
#41822 = DIRECTION ( 'NONE',  ( 0.000000000000000000, -1.836970198721029688E-16, -1.000000000000000000 ) ) ;
#41823 = DIRECTION ( 'NONE',  ( -0.000000000000000000, -1.000000000000000000, -0.000000000000000000 ) ) ;
#41824 = B_SPLINE_SURFACE_WITH_KNOTS ( 'NONE', 5, 5, ( 
 ( #69549, #103669, #61157, #46540, #81206, #12903, #88531, #53289, #11815 ),
 ( #96932, #87993, #87427, #54936, #89065, #11280, #45985, #36458, #63892 ),
 ( #72290, #3436, #3987, #38112, #21278, #20741, #29165, #72832, #20200 ),
 ( #38657, #95817, #62819, #106423, #54398, #47082, #79586, #12350, #104773 ),
 ( #2891, #80675, #29707, #98007, #44895, #80117, #62248, #70657, #105884 ),
 ( #63354, #106966, #55486, #89612, #37567, #4523, #10723, #30250, #71768 ),
 ( #19085, #97471, #79044, #2346, #28058, #96373, #19652, #53856, #45444 ),
 ( #37009, #71202, #105323, #28616, #5057, #74494, #108622, #31910, #41430 ),
 ( #32477, #65541, #66649, #56027, #83966, #99649, #22940, #31357, #39202 ) ),
 .UNSPECIFIED., .F., .F., .F.,
 ( 6, 3, 6 ),
 ( 6, 3, 6 ),
 ( 3.580107477790000381, 6.558749095509999627, 9.700153431640000434 ),
 ( 0.000000000000000000, 0.5000000000000000000, 1.000000000000000000 ),
 .UNSPECIFIED. ) ;
#41825 = FACE_OUTER_BOUND ( 'NONE', #58214, .T. ) ;
#41826 = CARTESIAN_POINT ( 'NONE',  ( -12.25020723839999981, 1415.706272599410113, 207.6119962243290331 ) ) ;
#41827 = AXIS2_PLACEMENT_3D ( 'NONE', #7101, #48571, #22216 ) ;
#41828 = CARTESIAN_POINT ( 'NONE',  ( 2.451271202390000070, 1433.447543843880112, 150.3250444719979839 ) ) ;
#41829 = CARTESIAN_POINT ( 'NONE',  ( 8.654318022629999163, 1488.600155993789940, 202.1361091811689903 ) ) ;
#41830 = FACE_OUTER_BOUND ( 'NONE', #26947, .T. ) ;
#41831 = CARTESIAN_POINT ( 'NONE',  ( 4.223051414464590536, 1441.592138948940146, 167.3011229986659885 ) ) ;
#41833 = DIRECTION ( 'NONE',  ( 0.000000000000000000, -1.000000000000000000, -2.312964634635740689E-15 ) ) ;
#41832 = CARTESIAN_POINT ( 'NONE',  ( 4.039897278065000208, 1516.787536375099990, 214.1203611275269907 ) ) ;
#41834 = CARTESIAN_POINT ( 'NONE',  ( 20.84366507899999732, 1509.634592532730039, 188.2028936218980277 ) ) ;
#41835 = CARTESIAN_POINT ( 'NONE',  ( -1.124894088365000044, 1517.194816588360027, 216.0733631026070043 ) ) ;
#41836 = VERTEX_POINT ( 'NONE', #15555 ) ;
#41837 = CARTESIAN_POINT ( 'NONE',  ( -12.73024483699999898, 1416.833018152729892, 195.1128574262980067 ) ) ;
#41838 = B_SPLINE_SURFACE_WITH_KNOTS ( 'NONE', 5, 1, ( 
 ( #104603, #30648 ),
 ( #14926, #92749 ),
 ( #15476, #107352 ),
 ( #73774, #56414 ),
 ( #109020, #64834 ),
 ( #73208, #23336 ),
 ( #98941, #31740 ),
 ( #48007, #58071 ),
 ( #100048, #83803 ) ),
 .UNSPECIFIED., .F., .F., .F.,
 ( 6, 3, 6 ),
 ( 2, 2 ),
 ( 0.000000000000000000, 8.685334524039999948, 17.34448624229999680 ),
 ( 0.000000000000000000, 14.00000434508570102 ),
 .UNSPECIFIED. ) ;
#41839 = CARTESIAN_POINT ( 'NONE',  ( -16.95087640679999907, 1420.353012175349932, 203.7180132809789939 ) ) ;
#41840 = CARTESIAN_POINT ( 'NONE',  ( -16.32163182381450284, 1508.551704408389924, 213.4489841974129831 ) ) ;
#41841 = PRODUCT_DEFINITION ( 'UNKNOWN', '', #94155, #54690 ) ;
#41842 = B_SPLINE_CURVE_WITH_KNOTS ( 'NONE', 5,
 ( #65302, #72592, #40077, #6477, #90473, #99413, #98323, #56341, #46854 ),
 .UNSPECIFIED., .F., .F.,
 ( 6, 3, 6 ),
 ( -3.000000000000000000, -1.500000000000000000, 0.000000000000000000 ),
 .UNSPECIFIED. ) ;
#41843 = CARTESIAN_POINT ( 'NONE',  ( 0.5456170147259989944, 1474.667248827789990, 219.7869908219989838 ) ) ;
#41844 = CARTESIAN_POINT ( 'NONE',  ( 2.599451791485461349, 1525.231887713385959, 176.7177626659179452 ) ) ;
#41845 = CARTESIAN_POINT ( 'NONE',  ( -0.8583877449824180994, 1423.306587861139860, 191.2160083861890030 ) ) ;
#41846 = CARTESIAN_POINT ( 'NONE',  ( 1.807048120887469578, 1416.685803381123378, 232.7081437053816728 ) ) ;
#41847 = CARTESIAN_POINT ( 'NONE',  ( 17.70041754922767296, 1423.341415640119749, 226.2080326948689901 ) ) ;
#41848 = CARTESIAN_POINT ( 'NONE',  ( 18.45217032144871894, 1425.619926260229931, 224.9274540208776330 ) ) ;
#41849 = CARTESIAN_POINT ( 'NONE',  ( 12.03449227190490056, 1491.353386486839781, 206.6667661091970274 ) ) ;
#41850 = CARTESIAN_POINT ( 'NONE',  ( 43.27085592825979887, 1440.913060356199821, 263.5081753078439988 ) ) ;
#41852 = CARTESIAN_POINT ( 'NONE',  ( 0.000000000000000000, 1519.913060387329779, 233.4018459616980010 ) ) ;
#41851 = CARTESIAN_POINT ( 'NONE',  ( -7.233408913757819469, 1421.233011291230014, 193.8023897524950030 ) ) ;
#41853 = CARTESIAN_POINT ( 'NONE',  ( -11.81780673814840021, 1522.051704408389924, 222.7166774759110126 ) ) ;
#41854 = ORIENTED_EDGE ( 'NONE', *, *, #18763, .T. ) ;
#41855 = VERTEX_POINT ( 'NONE', #21881 ) ;
#41856 = B_SPLINE_CURVE_WITH_KNOTS ( 'NONE', 3,
 ( #68067, #93762, #102179, #33875, #33315, #102714, #67510, #51802, #24900, #9244, #35535, #27148, #93232, #17040, #51237, #85370, #52369, #85942, #34437, #84819, #69163 ),
 .UNSPECIFIED., .F., .F.,
 ( 4, 2, 1, 1, 1, 2, 2, 2, 2, 2, 2, 4 ),
 ( 0.000000000000000000, 1.207358997277241904E-05, 2.414717994554483807E-05, 4.829435989153836644E-05, 9.658871978357142722E-05, 0.0001931774395680907182, 0.0003863548791367152433, 0.0007727097582739642393, 0.001159064637411213235, 0.001352242076979837679, 0.001448830796764309387, 0.001545419516548780878 ),
 .UNSPECIFIED. ) ;
#41857 = DIRECTION ( 'NONE',  ( 0.000000000000000000, 0.000000000000000000, 1.000000000000000000 ) ) ;
#41858 = EDGE_CURVE ( 'NONE', #70574, #98399, #64886, .T. ) ;
#41859 = CARTESIAN_POINT ( 'NONE',  ( 17.22354464511785821, 1410.184082523955794, 192.5759529289406942 ) ) ;
#41860 = CARTESIAN_POINT ( 'NONE',  ( -24.34268787264259970, 1442.549328851149994, 212.2035684885649687 ) ) ;
#41861 = CARTESIAN_POINT ( 'NONE',  ( 2.273290303349758457, 1410.370752790504412, 185.5123687935691237 ) ) ;
#41862 = ADVANCED_FACE ( 'NONE', ( #107026 ), #73274, .F. ) ;
#41863 = CARTESIAN_POINT ( 'NONE',  ( 16.19492410460000187, 1409.478599598930032, 217.9908631324380224 ) ) ;
#41864 = CARTESIAN_POINT ( 'NONE',  ( 18.49631469930000094, 1416.851343894929869, 209.5335333753989744 ) ) ;
#41865 = CARTESIAN_POINT ( 'NONE',  ( -113.3764034147090882, 1381.413060387289988, 303.2221243954415968 ) ) ;
#41866 = CARTESIAN_POINT ( 'NONE',  ( -4.326992699839999901, 1515.158586648489973, 208.7650084369950036 ) ) ;
#41867 = CARTESIAN_POINT ( 'NONE',  ( -66.54748892587809905, 1383.788754390270014, 290.5652759867210193 ) ) ;
#41868 = CARTESIAN_POINT ( 'NONE',  ( 22.80545758519999922, 1450.887189432959758, 142.4385674641980017 ) ) ;
#41870 = CARTESIAN_POINT ( 'NONE',  ( -8.779116450932770377, 1385.568036331880194, 220.6413991625189794 ) ) ;
#41869 =( BOUNDED_CURVE ( )  B_SPLINE_CURVE ( 3, ( #32571, #91376, #82967, #6261 ),
 .UNSPECIFIED., .F., .F. ) 
 B_SPLINE_CURVE_WITH_KNOTS ( ( 4, 4 ),
 ( 4.704954595420359986, 5.211301734500129790 ),
 .UNSPECIFIED. ) 
 CURVE ( )  GEOMETRIC_REPRESENTATION_ITEM ( )  RATIONAL_B_SPLINE_CURVE ( ( 1.000000000000000000, 0.9787482600944612532, 0.9787482600944612532, 1.000000000000000000 ) ) 
 REPRESENTATION_ITEM ( '' )  );
#41871 = CARTESIAN_POINT ( 'NONE',  ( 11.84335401826939993, 1492.196273574100132, 210.1769102818510078 ) ) ;
#41873 = ORIENTED_EDGE ( 'NONE', *, *, #82403, .T. ) ;
#41872 = CARTESIAN_POINT ( 'NONE',  ( -1.221315768609999797, 1455.568494079489938, 218.5163151374690074 ) ) ;
#41874 = CARTESIAN_POINT ( 'NONE',  ( -15.13342374508840038, 1507.606285602760181, 191.8462590464540085 ) ) ;
#41875 = EDGE_CURVE ( 'NONE', #64568, #71455, #83918, .T. ) ;
#41876 = CARTESIAN_POINT ( 'NONE',  ( -49.19940419029999390, 1380.956237859229986, 255.4336207247589527 ) ) ;
#41877 = CARTESIAN_POINT ( 'NONE',  ( 4.932890325442090607, 1508.551704408389924, 206.1093674645129852 ) ) ;
#41878 = VERTEX_POINT ( 'NONE', #80180 ) ;
#41879 = ORIENTED_EDGE ( 'NONE', *, *, #95879, .T. ) ;
#41880 = FACE_OUTER_BOUND ( 'NONE', #60172, .T. ) ;
#41881 = CARTESIAN_POINT ( 'NONE',  ( -21.51339057090000040, 1505.551704408389924, 209.1218459616989946 ) ) ;
#41882 = CARTESIAN_POINT ( 'NONE',  ( 36.34707484411779888, 1437.575034581910131, 136.5422136037309713 ) ) ;
#41884 = CARTESIAN_POINT ( 'NONE',  ( 0.000000000000000000, 1518.913060387330006, 209.1218459616979999 ) ) ;
#41883 = CARTESIAN_POINT ( 'NONE',  ( 18.19590854888164699, 1501.977400791986611, 238.2026672068774644 ) ) ;
#41885 = CIRCLE ( 'NONE', #36539, 10.00000000000000000 ) ;
#41886 = CARTESIAN_POINT ( 'NONE',  ( 11.77194447489770113, 1479.596685624299880, 209.5331444464590049 ) ) ;
#41887 = CARTESIAN_POINT ( 'NONE',  ( -107.1082468550000044, 1381.675179291449922, 298.5714521776590118 ) ) ;
#41888 = CARTESIAN_POINT ( 'NONE',  ( -2.559284476340000225, 1448.316302177390071, 190.2468044718989972 ) ) ;
#41889 = CARTESIAN_POINT ( 'NONE',  ( -0.4299350982835939416, 1451.092099702937730, 182.2245401379511520 ) ) ;
#41890 = CARTESIAN_POINT ( 'NONE',  ( 18.95790016943493939, 1509.575089211102750, 186.6267876694127779 ) ) ;
#41891 = CARTESIAN_POINT ( 'NONE',  ( 18.28985832975333281, 1517.151704408390060, 219.7143006364888436 ) ) ;
#41892 = EDGE_CURVE ( 'NONE', #55821, #57154, #90207, .T. ) ;
#41893 = CARTESIAN_POINT ( 'NONE',  ( 3.022804847239999759, 1409.018619058630065, 186.7640392999980179 ) ) ;
#41894 = CARTESIAN_POINT ( 'NONE',  ( 1.282357359580419853, 1486.462675952139989, 197.2709641886989971 ) ) ;
#41895 = CARTESIAN_POINT ( 'NONE',  ( 2.796706406386159749, 1431.643787548970067, 200.3851250015239884 ) ) ;
#41896 = CARTESIAN_POINT ( 'NONE',  ( -4.222336330638260193, 1441.606005989779987, 166.9080596108109944 ) ) ;
#41897 = VECTOR ( 'NONE', #12430, 999.9999999999998863 ) ;
#41898 = CARTESIAN_POINT ( 'NONE',  ( -25.16854656449999794, 1451.224506337529874, 137.5711276817980320 ) ) ;
#41899 = ORIENTED_EDGE ( 'NONE', *, *, #44574, .F. ) ;
#41900 = ADVANCED_FACE ( 'NONE', ( #38168 ), #93213, .F. ) ;
#41901 = B_SPLINE_SURFACE_WITH_KNOTS ( 'NONE', 5, 5, ( 
 ( #561, #58255, #17301, #77262, #67759, #109210 ),
 ( #102432, #92375, #15647, #66666, #51496, #6725 ),
 ( #58797, #23523, #25163, #25716, #16208, #76145 ),
 ( #93477, #8929, #50412, #91833, #84537, #49853 ),
 ( #83986, #40881, #16748, #85079, #7285, #7826 ),
 ( #32494, #34687, #41448, #57717, #42539, #4 ),
 ( #59367, #101872, #75613, #41996, #109744, #33025 ),
 ( #101311, #34138, #67214, #110290, #33567, #59917 ),
 ( #8370, #85628, #18971, #11167, #87877, #52061 ),
 ( #10040, #36897, #60465, #96821, #78355, #18414 ),
 ( #61572, #61033, #1113, #27391, #45874, #95705 ),
 ( #53166, #62133, #43652, #105215, #69428, #70537 ) ),
 .UNSPECIFIED., .F., .F., .F.,
 ( 6, 3, 3, 6 ),
 ( 6, 6 ),
 ( -7.850178216250999828E-05, 7.062844993700000629, 14.12568998740000126, 17.37861058108219936 ),
 ( 0.000000000000000000, 2.000078501782160068 ),
 .UNSPECIFIED. ) ;
#41902 = CARTESIAN_POINT ( 'NONE',  ( -18.31738235171379969, 1464.474234536650101, 217.5285399418669954 ) ) ;
#41903 = DIRECTION ( 'NONE',  ( 1.755985294532464991E-16, -1.000000000000000000, 1.338183447452830017E-16 ) ) ;
#41904 = CARTESIAN_POINT ( 'NONE',  ( 19.46939419728449749, 1455.727202090050014, 226.4972727368899825 ) ) ;
#41905 = DIRECTION ( 'NONE',  ( 1.755985294532464991E-16, -1.000000000000000000, 1.338183447452830017E-16 ) ) ;
#41906 = EDGE_CURVE ( 'NONE', #29269, #76248, #100932, .T. ) ;
#41907 = CARTESIAN_POINT ( 'NONE',  ( -6.848531018220000099, 1473.608249816489888, 207.2687511549490011 ) ) ;
#41908 = B_SPLINE_CURVE_WITH_KNOTS ( 'NONE', 5,
 ( #21028, #4265, #81492, #11558, #22120, #47365, #29993, #45735, #38398 ),
 .UNSPECIFIED., .F., .F.,
 ( 6, 3, 6 ),
 ( 0.000000000000000000, 0.5000000000000000000, 1.000000000000000000 ),
 .UNSPECIFIED. ) ;
#41909 = CARTESIAN_POINT ( 'NONE',  ( -1.032992184830370031E-08, 1474.676908767299892, 264.7279807803609515 ) ) ;
#41910 = CARTESIAN_POINT ( 'NONE',  ( -3.829620113550000315, 1515.551704408389924, 211.2083941403789993 ) ) ;
#41911 = CARTESIAN_POINT ( 'NONE',  ( -0.7133824534919999127, 1416.822690122329959, 227.9183239597979878 ) ) ;
#41912 = DIRECTION ( 'NONE',  ( 0.000000000000000000, 0.000000000000000000, 1.000000000000000000 ) ) ;
#41913 = CARTESIAN_POINT ( 'NONE',  ( -3.151260259420000320, 1476.308151181189942, 199.2625566838590032 ) ) ;
#41914 = CARTESIAN_POINT ( 'NONE',  ( -105.5049133189999964, 1391.244241388860246, 305.3574306296589498 ) ) ;
#41915 = CARTESIAN_POINT ( 'NONE',  ( -8.322537005615968653, 1511.435455886209866, 214.5074547685709945 ) ) ;
#41916 = CARTESIAN_POINT ( 'NONE',  ( -9.651661623395108691, 1361.059646503146041, 208.3718459617010978 ) ) ;
#41917 = CARTESIAN_POINT ( 'NONE',  ( -45.59497939955269885, 1438.873046339160055, 266.1906450788720235 ) ) ;
#41918 = CARTESIAN_POINT ( 'NONE',  ( 1.316738241441249846, 1429.477911528270170, 217.3230272967620067 ) ) ;
#41919 = CARTESIAN_POINT ( 'NONE',  ( -8.016638155169999891, 1425.903768209389909, 207.5828447795889815 ) ) ;
#41920 = ADVANCED_FACE ( 'NONE', ( #109648 ), #73441, .T. ) ;
#41921 = CARTESIAN_POINT ( 'NONE',  ( 3.449647440015000122, 1516.829948096479939, 208.3645479958780129 ) ) ;
#41922 = CARTESIAN_POINT ( 'NONE',  ( -9.923943078109999760, 1386.701148096399947, 200.5013422001489687 ) ) ;
#41923 = B_SPLINE_CURVE_WITH_KNOTS ( 'NONE', 3,
 ( #48621, #100104, #99532, #24478, #74923, #101182, #67078, #32354, #6045, #82753, #13314, #14424, #107395, #49169, #90037, #73256, #22816, #40196 ),
 .UNSPECIFIED., .F., .F.,
 ( 4, 2, 2, 2, 2, 2, 2, 2, 4 ),
 ( 0.000000000000000000, 0.07958679019459939663, 0.1577458466451709951, 0.2359250078159189912, 0.2750922612652370036, 0.2946660706215870063, 0.3044518104690189797, 0.3144120845289309907, 0.3151965516711889848 ),
 .UNSPECIFIED. ) ;
#41924 = CARTESIAN_POINT ( 'NONE',  ( -27.69925886641940238, 1441.434395751479997, 137.3015763626259798 ) ) ;
#41925 = CARTESIAN_POINT ( 'NONE',  ( 7.535336306764500058, 1425.758512211720017, 212.2082866544780018 ) ) ;
#41926 = EDGE_CURVE ( 'NONE', #58564, #71251, #15462, .T. ) ;
#41927 = CARTESIAN_POINT ( 'NONE',  ( -26.16688589682070187, 1451.542564073259882, 136.1869649791260315 ) ) ;
#41928 = ORIENTED_EDGE ( 'NONE', *, *, #60333, .T. ) ;
#41929 = CARTESIAN_POINT ( 'NONE',  ( 25.15583052850000101, 1439.261431119660074, 217.2951522780279845 ) ) ;
#41931 = CARTESIAN_POINT ( 'NONE',  ( 15.51935361379999989, 1506.809279316930088, 193.4756025686980081 ) ) ;
#41930 = CARTESIAN_POINT ( 'NONE',  ( -3.415238448984999842, 1511.801704408389924, 213.5367417060670050 ) ) ;
#41932 = CARTESIAN_POINT ( 'NONE',  ( -9.491012693391989759E-16, 1374.413060387289988, 209.1218459616989946 ) ) ;
#41933 = CARTESIAN_POINT ( 'NONE',  ( -3.018087336003992593, 1475.315668037541400, 198.8202750044643778 ) ) ;
#41934 = CARTESIAN_POINT ( 'NONE',  ( -12.93678125246493771, 1396.364822743412560, 207.0732903518876924 ) ) ;
#41935 = CARTESIAN_POINT ( 'NONE',  ( -13.58235846979999906, 1416.828040475229955, 221.9087530951979659 ) ) ;
#41936 = CARTESIAN_POINT ( 'NONE',  ( 18.03426301339999682, 1429.185447070490000, 206.6153916553589909 ) ) ;
#41937 = ORIENTED_EDGE ( 'NONE', *, *, #102190, .F. ) ;
#41938 = CARTESIAN_POINT ( 'NONE',  ( -4.767656242956440416, 1410.583764236560228, 269.3374945991810137 ) ) ;
#41939 = CARTESIAN_POINT ( 'NONE',  ( 16.63147820130039989, 1421.790408391879964, 227.0569735401810192 ) ) ;
#41940 = FACE_OUTER_BOUND ( 'NONE', #43328, .T. ) ;
#41941 = ORIENTED_EDGE ( 'NONE', *, *, #67477, .F. ) ;
#41942 = ORIENTED_EDGE ( 'NONE', *, *, #47515, .F. ) ;
#41943 = EDGE_CURVE ( 'NONE', #5163, #68079, #58337, .T. ) ;
#41944 = CARTESIAN_POINT ( 'NONE',  ( -24.02381549939999772, 1410.732491813230126, 209.5701859032720051 ) ) ;
#41945 = ORIENTED_EDGE ( 'NONE', *, *, #71588, .T. ) ;
#41946 = DIRECTION ( 'NONE',  ( -1.000000000000000000, 0.000000000000000000, 0.000000000000000000 ) ) ;
#41947 = CARTESIAN_POINT ( 'NONE',  ( -11.16223122930000144, 1428.970455832429934, 101.8807690336980016 ) ) ;
#41948 = B_SPLINE_SURFACE_WITH_KNOTS ( 'NONE', 5, 5, ( 
 ( #47078, #73928, #99097, #39198, #54932, #56024 ),
 ( #107513, #73375, #30803, #64440, #22375, #108058 ),
 ( #90705, #98556, #72287, #90149, #63888, #29704 ),
 ( #31354, #99644, #22935, #82861, #12346, #13431 ),
 ( #38653, #105881, #6152, #29162, #63350, #97468 ),
 ( #47621, #46537, #98003, #106961, #80671, #21274 ) ),
 .UNSPECIFIED., .F., .F., .F.,
 ( 6, 6 ),
 ( 6, 6 ),
 ( -1.743397922130910115E-05, 7.850533482159220533 ),
 ( -1.743397922130910115E-05, 1.000000000000000000 ),
 .UNSPECIFIED. ) ;
#41949 = EDGE_CURVE ( 'NONE', #63792, #46121, #64289, .T. ) ;
#41950 = CARTESIAN_POINT ( 'NONE',  ( -1.581402563589999977, 1498.352608146529974, 236.7257605069980002 ) ) ;
#41951 = CARTESIAN_POINT ( 'NONE',  ( -17.57163213930000012, 1410.882994532030125, 225.4813515594979947 ) ) ;
#41952 = CARTESIAN_POINT ( 'NONE',  ( 45.59504749288019809, 1442.766519910440138, 268.9761053574069933 ) ) ;
#41953 = CARTESIAN_POINT ( 'NONE',  ( -0.5656601614563600000, 1424.194575819369902, 228.0927458373740251 ) ) ;
#41954 = CARTESIAN_POINT ( 'NONE',  ( -16.13553931567702193, 1420.899259742274353, 227.0324294037215225 ) ) ;
#41955 = CARTESIAN_POINT ( 'NONE',  ( 3.254401403604999743, 1516.919782530640077, 205.0791161293069820 ) ) ;
#41956 = VERTEX_POINT ( 'NONE', #52513 ) ;
#41957 = CARTESIAN_POINT ( 'NONE',  ( -11.14671771210699980, 1434.019356486030119, 151.6529807626459956 ) ) ;
#41958 = CARTESIAN_POINT ( 'NONE',  ( 0.1765913036374869849, 1444.932331911239999, 199.0604220796319908 ) ) ;
#41959 = DIRECTION ( 'NONE',  ( 0.000000000000000000, 0.000000000000000000, 1.000000000000000000 ) ) ;
#41960 = ORIENTED_EDGE ( 'NONE', *, *, #82403, .F. ) ;
#41961 = CARTESIAN_POINT ( 'NONE',  ( 3.932342930579999507, 1448.638726228580026, 184.2846140409980364 ) ) ;
#41962 = CARTESIAN_POINT ( 'NONE',  ( 1.964958540781392982, 1433.107491112560638, 200.8576305902842023 ) ) ;
#41963 = DIRECTION ( 'NONE',  ( -1.000000000000000000, 0.000000000000000000, 0.000000000000000000 ) ) ;
#41964 = CARTESIAN_POINT ( 'NONE',  ( -13.36456641330000039, 1385.300820372649923, 218.9430041755990146 ) ) ;
#41965 = CARTESIAN_POINT ( 'NONE',  ( 7.803888876470000291, 1421.636253146019953, 195.8400330162989746 ) ) ;
#41967 = B_SPLINE_SURFACE_WITH_KNOTS ( 'NONE', 5, 5, ( 
 ( #24604, #59368, #93478, #68325, #66668, #75614 ),
 ( #5, #109747, #58798, #7286, #34139, #24062 ),
 ( #6178, #58256, #84538, #15648, #59918, #74513 ),
 ( #92376, #94038, #100246, #15114, #49304, #83429 ),
 ( #16209, #6726, #49854, #50413, #96260, #102979 ),
 ( #62135, #86195, #51497, #77805, #105216, #9487 ),
 ( #86751, #36346, #104102, #10041, #19535, #2230 ),
 ( #18415, #35805, #70538, #1664, #1114, #61035 ),
 ( #62703, #53743, #104655, #35243, #10603, #27952 ),
 ( #69429, #87878, #87310, #11169, #45329, #34688 ),
 ( #69985, #26277, #44774, #103544, #79468, #60467 ),
 ( #96822, #85630, #68878, #2778, #28504, #36898 ) ),
 .UNSPECIFIED., .F., .F., .F.,
 ( 6, 3, 3, 6 ),
 ( 6, 6 ),
 ( 6.182282359980000308, 12.54225916440000077, 24.91223976350000058, 34.19375089779999399 ),
 ( 0.1502731719950000100, 0.6000000000009999557 ),
 .UNSPECIFIED. ) ;
#41966 = CARTESIAN_POINT ( 'NONE',  ( 0.08322839651420729790, 1431.805008108389984, 218.6146693997570196 ) ) ;
#41968 = CARTESIAN_POINT ( 'NONE',  ( -4.522294835890000364, 1496.991527996390232, 198.8128890079989901 ) ) ;
#41969 = CIRCLE ( 'NONE', #104553, 1.999999997221749704 ) ;
#41970 = CARTESIAN_POINT ( 'NONE',  ( 1.748432842252070074, 1408.974117007579935, 186.8594775301320112 ) ) ;
#41972 = CARTESIAN_POINT ( 'NONE',  ( -111.7220106148852778, 1305.733110638860126, 301.1503069906427186 ) ) ;
#41971 = CARTESIAN_POINT ( 'NONE',  ( 1.009298393719999964, 1415.944724089230021, 233.1672510863979824 ) ) ;
#41973 = DIRECTION ( 'NONE',  ( -0.4438071788273494356, -0.8961223063964589564, 0.000000000000000000 ) ) ;
#41974 = CARTESIAN_POINT ( 'NONE',  ( -13.54127076360000004, 1379.893677090969959, 213.5390424406290037 ) ) ;
#41975 = VECTOR ( 'NONE', #77387, 1000.000000000000000 ) ;
#41976 = CARTESIAN_POINT ( 'NONE',  ( 13.87806392702616698, 1421.462115117653866, 230.8073813634572105 ) ) ;
#41977 = ORIENTED_EDGE ( 'NONE', *, *, #16871, .F. ) ;
#41978 = CARTESIAN_POINT ( 'NONE',  ( -32.38845792001078649, 1523.456924617338927, 202.1182848006243944 ) ) ;
#41979 = AXIS2_PLACEMENT_3D ( 'NONE', #9783, #17601, #51236 ) ;
#41980 = CARTESIAN_POINT ( 'NONE',  ( 11.83148343547229864, 1432.336211092349913, 150.3814746356140120 ) ) ;
#41981 = CARTESIAN_POINT ( 'NONE',  ( -10.61669498371649922, 1508.551704408389924, 207.6874897006059939 ) ) ;
#41982 = EDGE_CURVE ( 'NONE', #27781, #72991, #20824, .T. ) ;
#41983 = B_SPLINE_SURFACE_WITH_KNOTS ( 'NONE', 5, 5, ( 
 ( #97659, #56212, #81384, #38841, #90342, #29888 ),
 ( #55137, #82519, #107713, #99844, #57341, #14189 ),
 ( #4164, #64082, #5250, #14746, #3630, #12552 ),
 ( #80864, #39406, #99287, #72473, #56768, #106603 ),
 ( #98202, #21472, #5817, #89804, #16921, #42163 ),
 ( #75769, #102588, #8546, #74679, #33198, #92547 ),
 ( #48933, #15815, #16374, #84152, #100944, #85247 ),
 ( #59527, #7452, #109919, #50020, #67388, #25331 ),
 ( #24773, #50572, #25888, #75229, #76874, #58970 ) ),
 .UNSPECIFIED., .F., .F., .F.,
 ( 6, 3, 6 ),
 ( 6, 6 ),
 ( 1.461586381270000068, 8.269156193220000617, 13.54897587289999983 ),
 ( 0.000000000000000000, 1.000000000000000000 ),
 .UNSPECIFIED. ) ;
#41984 = CARTESIAN_POINT ( 'NONE',  ( -10.51196183719999944, 1389.287104299670091, 202.3467939211689952 ) ) ;
#41985 = CARTESIAN_POINT ( 'NONE',  ( 9.216942500360310930, 1427.824353572689915, 211.8045479288090007 ) ) ;
#41986 = CARTESIAN_POINT ( 'NONE',  ( 11.11191080231209938, 1422.810623797719927, 203.3290056078989778 ) ) ;
#41987 = CARTESIAN_POINT ( 'NONE',  ( -10.90301725406700051, 1462.753400739099789, 207.3092048343249871 ) ) ;
#41988 = CARTESIAN_POINT ( 'NONE',  ( -38.34143788450000301, 1445.301772818269910, 265.6112251771979800 ) ) ;
#41989 = CARTESIAN_POINT ( 'NONE',  ( -21.53951952428644745, 1509.203566254688440, 191.7343637106751828 ) ) ;
#41990 = CARTESIAN_POINT ( 'NONE',  ( 11.92439245019999916, 1433.423794087070064, 149.9160333479979954 ) ) ;
#41991 = CARTESIAN_POINT ( 'NONE',  ( 14.35418281399999962, 1450.996202460929908, 214.3676144200779845 ) ) ;
#41992 = B_SPLINE_SURFACE_WITH_KNOTS ( 'NONE', 5, 5, ( 
 ( #34000, #16075, #9904, #102297, #84940, #103391 ),
 ( #44073, #68193, #59775, #50278, #85488, #16613 ),
 ( #84407, #76554, #109614, #25582, #7694, #41851 ),
 ( #42401, #93896, #17161, #94441, #69286, #77667 ),
 ( #18289, #42969, #101741, #17720, #77128, #67627 ),
 ( #110710, #51354, #76006, #434, #50810, #32887 ),
 ( #110160, #25029, #34553, #68736, #52482, #59231 ),
 ( #102840, #86610, #26134, #60323, #51922, #67081 ),
 ( #86065, #101184, #980, #35104, #26697, #97767 ) ),
 .UNSPECIFIED., .F., .F., .F.,
 ( 6, 3, 6 ),
 ( 6, 6 ),
 ( 15.02943005950050015, 30.78174686530000059, 37.58808827629950144 ),
 ( -1.629659945966520018E-05, 2.000000000000000000 ),
 .UNSPECIFIED. ) ;
#41993 = CARTESIAN_POINT ( 'NONE',  ( -9.670053538248419400, 1461.149818306590078, 208.5229399444750129 ) ) ;
#41994 = CARTESIAN_POINT ( 'NONE',  ( -29.37542415142715768, 1526.382868172864164, 200.9849896654584143 ) ) ;
#41995 = CARTESIAN_POINT ( 'NONE',  ( 2.760778564396810353, 1409.009468899150079, 230.1977509304229841 ) ) ;
#41996 = CARTESIAN_POINT ( 'NONE',  ( 8.997196703874418944, 1463.834352910819916, 214.0592121972250084 ) ) ;
#41997 = ADVANCED_FACE ( 'NONE', ( #95055 ), #76047, .F. ) ;
#41998 = CARTESIAN_POINT ( 'NONE',  ( 8.800000000000002487, 1413.913060387329779, 209.1218459616989946 ) ) ;
#41999 = DIRECTION ( 'NONE',  ( -5.612627869608440548E-17, -0.03489949670197409898, 0.9993908270191140808 ) ) ;
#42000 = CARTESIAN_POINT ( 'NONE',  ( -17.38481315180000308, 1410.884446742730233, 225.7833460420979748 ) ) ;
#42001 = CARTESIAN_POINT ( 'NONE',  ( 23.00452548930000063, 1430.350017905930144, 215.8863230596679728 ) ) ;
#42002 = CARTESIAN_POINT ( 'NONE',  ( 4.703965987320000013E-16, 1428.579607037230062, 149.5143047311979672 ) ) ;
#42003 = CARTESIAN_POINT ( 'NONE',  ( -13.77020040508769938, 1383.859715768199976, 219.0313993434459690 ) ) ;
#42004 = CARTESIAN_POINT ( 'NONE',  ( -0.4992773797353766141, 1524.841055067849993, 174.1119671515087930 ) ) ;
#42005 = CARTESIAN_POINT ( 'NONE',  ( -21.26810763296740348, 1485.919194788800041, 201.7808564414550290 ) ) ;
#42006 = CARTESIAN_POINT ( 'NONE',  ( 7.723480079395000253, 1517.086065052259983, 213.1573821953169841 ) ) ;
#42007 = CARTESIAN_POINT ( 'NONE',  ( -21.07255583944779787, 1418.159754048780087, 208.6257934781920085 ) ) ;
#42008 = CARTESIAN_POINT ( 'NONE',  ( 0.1703894054731670271, 1480.100913143119897, 182.0900560439260119 ) ) ;
#42010 = ORIENTED_EDGE ( 'NONE', *, *, #95410, .F. ) ;
#42009 = CARTESIAN_POINT ( 'NONE',  ( -10.80134480061109947, 1441.261220175989820, 153.0805715986579969 ) ) ;
#42011 = CARTESIAN_POINT ( 'NONE',  ( -13.31869796660000027, 1444.740067931809790, 169.3753098992980028 ) ) ;
#42012 = EDGE_CURVE ( 'NONE', #68807, #48271, #35140, .T. ) ;
#42013 = FACE_OUTER_BOUND ( 'NONE', #72012, .T. ) ;
#42014 = DIRECTION ( 'NONE',  ( -0.8775825618903754233, 0.000000000000000000, -0.4794255386041978984 ) ) ;
#42015 = CARTESIAN_POINT ( 'NONE',  ( -40.44958274777649621, 1439.458628679120011, 134.0999999981179940 ) ) ;
#42016 = CARTESIAN_POINT ( 'NONE',  ( -109.7178863559999940, 1384.903230390709950, 297.0861955617589842 ) ) ;
#42017 = ORIENTED_EDGE ( 'NONE', *, *, #41428, .T. ) ;
#42018 = CARTESIAN_POINT ( 'NONE',  ( -5.931183514203220319, 1391.913060387289988, 203.1296912725950108 ) ) ;
#42019 = AXIS2_PLACEMENT_3D ( 'NONE', #93433, #67714, #41946 ) ;
#42020 = CARTESIAN_POINT ( 'NONE',  ( 10.10955624819999876, 1478.902419763290027, 204.8960363941690161 ) ) ;
#42021 = CARTESIAN_POINT ( 'NONE',  ( -15.03806458159999870, 1414.913060387229962, 216.3136682808679723 ) ) ;
#42022 = DIRECTION ( 'NONE',  ( -0.8775825618903722036, 0.000000000000000000, -0.4794255386042038936 ) ) ;
#42023 = EDGE_CURVE ( 'NONE', #47384, #84894, #87695, .T. ) ;
#42024 = CARTESIAN_POINT ( 'NONE',  ( -8.694328787849268991, 1436.795955225099988, 213.8530210085260137 ) ) ;
#42025 = CARTESIAN_POINT ( 'NONE',  ( -12.78776258889159934, 1416.851343895820037, 195.9645815067300134 ) ) ;
#42026 = CARTESIAN_POINT ( 'NONE',  ( 0.000000000000000000, 1511.187213306747708, 209.1218459616979999 ) ) ;
#42027 = DIRECTION ( 'NONE',  ( -0.3892484888175452573, 0.9211327884476036010, 0.000000000000000000 ) ) ;
#42028 = CARTESIAN_POINT ( 'NONE',  ( -83.30886681774781266, 1385.170142578559989, 287.0534937087779781 ) ) ;
#42029 = CARTESIAN_POINT ( 'NONE',  ( -11.66044326631700123, 1391.913060387289988, 209.8209183207389970 ) ) ;
#42030 = CARTESIAN_POINT ( 'NONE',  ( 11.54915390828909949, 1427.568721002570101, 209.3630650540049771 ) ) ;
#42031 = VERTEX_POINT ( 'NONE', #7729 ) ;
#42032 = CARTESIAN_POINT ( 'NONE',  ( -28.55009876189999574, 1451.915930383729801, 135.3068286921980246 ) ) ;
#42033 = CARTESIAN_POINT ( 'NONE',  ( -15.79838181210750214, 1409.567131171960000, 225.8770295224450138 ) ) ;
#42035 = VERTEX_POINT ( 'NONE', #101772 ) ;
#42034 = FACE_OUTER_BOUND ( 'NONE', #20938, .T. ) ;
#42036 = CARTESIAN_POINT ( 'NONE',  ( 1.396945621630000023, 1473.097535868490013, 219.2356281688989839 ) ) ;
#42037 = CARTESIAN_POINT ( 'NONE',  ( -21.64610633839767573, 1411.027676083505639, 216.2671881281004005 ) ) ;
#42038 = CARTESIAN_POINT ( 'NONE',  ( -8.059861619861480975, 1364.726888446574776, 208.3718459617061285 ) ) ;
#42039 = CARTESIAN_POINT ( 'NONE',  ( -10.84952760220000023, 1492.388833904489957, 203.1614253636989815 ) ) ;
#42040 = EDGE_CURVE ( 'NONE', #15017, #37845, #75594, .T. ) ;
#42041 = CARTESIAN_POINT ( 'NONE',  ( 38.90111251957022631, 1452.461926335832231, 269.5912703700630573 ) ) ;
#42042 = CARTESIAN_POINT ( 'NONE',  ( 17.94471134571137583, 1434.902817273550909, 215.4479691263156553 ) ) ;
#42043 = LINE ( 'NONE', #43699, #17473 ) ;
#42044 = CARTESIAN_POINT ( 'NONE',  ( 8.814478973669999107, 1449.891423584090035, 204.2733476837790079 ) ) ;
#42045 = CARTESIAN_POINT ( 'NONE',  ( -21.13674105400000158, 1506.830501455790227, 213.5414170319390053 ) ) ;
#42046 = ADVANCED_FACE ( 'NONE', ( #25063 ), #72297, .T. ) ;
#42047 = CARTESIAN_POINT ( 'NONE',  ( 10.78330898009999927, 1453.313060387329870, 226.3563104863980016 ) ) ;
#42048 = CARTESIAN_POINT ( 'NONE',  ( -2.642610841670000266, 1455.978071948890147, 200.0212207443690033 ) ) ;
#42049 = ADVANCED_FACE ( 'NONE', ( #46882 ), #96407, .T. ) ;
#42050 = CARTESIAN_POINT ( 'NONE',  ( 1.702405985064999960, 1516.999105586269934, 205.8518611507970206 ) ) ;
#42051 = LINE ( 'NONE', #110348, #8977 ) ;
#42052 = VERTEX_POINT ( 'NONE', #106209 ) ;
#42053 = CARTESIAN_POINT ( 'NONE',  ( -109.1344552622740025, 1384.804943809120005, 311.2633325561420179 ) ) ;
#42054 = CARTESIAN_POINT ( 'NONE',  ( 14.45760372910000058, 1416.831925117829996, 196.8518845416979843 ) ) ;
#42056 = ORIENTED_EDGE ( 'NONE', *, *, #70015, .T. ) ;
#42055 = CARTESIAN_POINT ( 'NONE',  ( -68.71293640201129449, 1379.747782475320037, 280.3108351316460016 ) ) ;
#42057 = ADVANCED_FACE ( 'NONE', ( #19991 ), #21283, .F. ) ;
#42058 = CARTESIAN_POINT ( 'NONE',  ( -17.47050761057940349, 1417.655283096519952, 206.4347063045530035 ) ) ;
#42059 = ORIENTED_EDGE ( 'NONE', *, *, #72193, .F. ) ;
#42060 = CARTESIAN_POINT ( 'NONE',  ( -16.48452152037296159, 1514.266850646888997, 223.5216240896907038 ) ) ;
#42061 = CARTESIAN_POINT ( 'NONE',  ( -25.36027075149999988, 1449.801358176479880, 206.9464496238279878 ) ) ;
#42064 = CARTESIAN_POINT ( 'NONE',  ( 16.29451049919999761, 1409.859978110029942, 192.0605078528979845 ) ) ;
#42063 = AXIS2_PLACEMENT_3D ( 'NONE', #70545, #71667, #72197 ) ;
#42062 = CARTESIAN_POINT ( 'NONE',  ( -11.13172969966639947, 1426.040969812840103, 108.4495695014479963 ) ) ;
#42065 = CARTESIAN_POINT ( 'NONE',  ( 5.788436334164999586, 1517.116049120239950, 211.4102033778369787 ) ) ;
#42066 = CARTESIAN_POINT ( 'NONE',  ( 18.29376482344865451, 1509.671222653318864, 185.3449578346911437 ) ) ;
#42067 = CARTESIAN_POINT ( 'NONE',  ( 1.562525333773240543, 1450.589639673192551, 181.7027468294939183 ) ) ;
#42068 = B_SPLINE_SURFACE_WITH_KNOTS ( 'NONE', 5, 5, ( 
 ( #85287, #25928, #51720, #60126, #769, #34898 ),
 ( #69644, #59020, #69086, #103187, #1315, #67429 ),
 ( #8587, #18631, #103767, #26490, #93147, #25374 ),
 ( #16415, #94811, #18087, #102092, #95368, #59566 ),
 ( #52828, #50608, #16959, #51160, #80220, #37661 ),
 ( #44425, #36558, #89165, #11373, #19175, #11912 ),
 ( #21378, #36020, #37109, #71310, #28157, #97570 ),
 ( #3538, #53951, #80772, #12456, #20842, #45544 ),
 ( #71867, #1883, #10249, #88085, #88633, #79684 ) ),
 .UNSPECIFIED., .F., .F., .F.,
 ( 6, 3, 6 ),
 ( 6, 6 ),
 ( 2.894173653929999812, 6.772837685190000734, 11.90357780880000149 ),
 ( 0.000000000000000000, 2.000000000000000000 ),
 .UNSPECIFIED. ) ;
#42069 = SURFACE_STYLE_USAGE ( .BOTH. , #101947 ) ;
#42070 = CARTESIAN_POINT ( 'NONE',  ( -12.74586014692540026, 1379.133382998009893, 208.7590490476249840 ) ) ;
#42071 = CARTESIAN_POINT ( 'NONE',  ( 17.11588712847992610, 1460.309517847519601, 228.6647148658520337 ) ) ;
#42072 = APPLICATION_PROTOCOL_DEFINITION ( 'draft international standard', 'automotive_design', 1998, #32019 ) ;
#42073 = CARTESIAN_POINT ( 'NONE',  ( 3.425924819994940140, 1508.551704408389924, 213.9259735013179977 ) ) ;
#42074 = DIRECTION ( 'NONE',  ( -6.123233995736769734E-17, -1.000000000000000000, -1.124819836996389922E-32 ) ) ;
#42075 = ORIENTED_EDGE ( 'NONE', *, *, #15380, .F. ) ;
#42076 = DIRECTION ( 'NONE',  ( 0.000000000000000000, 0.000000000000000000, 1.000000000000000000 ) ) ;
#42077 = EDGE_CURVE ( 'NONE', #75704, #49504, #42778, .T. ) ;
#42078 = CARTESIAN_POINT ( 'NONE',  ( -116.9103302475592301, 1305.913060387289988, 302.3041438028434413 ) ) ;
#42079 = ORIENTED_EDGE ( 'NONE', *, *, #15951, .T. ) ;
#42080 = ORIENTED_EDGE ( 'NONE', *, *, #92483, .F. ) ;
#42081 = CARTESIAN_POINT ( 'NONE',  ( -29.67498122965860929, 1509.980309120330958, 210.3356156768038261 ) ) ;
#42082 = CARTESIAN_POINT ( 'NONE',  ( 10.17590696771870107, 1453.471716470849969, 212.1423554297430201 ) ) ;
#42083 = CARTESIAN_POINT ( 'NONE',  ( -14.12838654810969885, 1379.942489218340143, 211.2222688814750029 ) ) ;
#42084 = CARTESIAN_POINT ( 'NONE',  ( -12.00127168876410444, 1417.517758714561751, 199.4623453708297518 ) ) ;
#42085 = EDGE_CURVE ( 'NONE', #24144, #96069, #49623, .T. ) ;
#42086 = CARTESIAN_POINT ( 'NONE',  ( 4.138993620949999119, 1515.551749212189861, 209.4962163748910200 ) ) ;
#42087 = CARTESIAN_POINT ( 'NONE',  ( -6.445381995435790046, 1454.081129442119845, 202.3077001288629901 ) ) ;
#42088 = CARTESIAN_POINT ( 'NONE',  ( 33.91369117179520032, 1451.728768195329849, 134.4205496120819987 ) ) ;
#42089 = CARTESIAN_POINT ( 'NONE',  ( 2.935376380067538982, 1516.592453103030493, 216.0331898163414621 ) ) ;
#42090 = CIRCLE ( 'NONE', #49289, 1.560060070890045836 ) ;
#42091 = CARTESIAN_POINT ( 'NONE',  ( 26.48466844540000054, 1437.480003640949917, 136.8777945664980109 ) ) ;
#42092 = CARTESIAN_POINT ( 'NONE',  ( -12.16877406210000068, 1391.738014982129926, 211.0029804830490150 ) ) ;
#42093 = CARTESIAN_POINT ( 'NONE',  ( -101.1025779375780047, 1384.877682633120003, 296.4583214505040587 ) ) ;
#42094 = ORIENTED_EDGE ( 'NONE', *, *, #19568, .F. ) ;
#42095 = CARTESIAN_POINT ( 'NONE',  ( 2.484577657225000014, 1517.170512887980067, 201.7834339727070017 ) ) ;
#42096 = CARTESIAN_POINT ( 'NONE',  ( 7.332063939445000678, 1516.939491476980038, 209.1111146381379911 ) ) ;
#42097 = VERTEX_POINT ( 'NONE', #65331 ) ;
#42098 = CARTESIAN_POINT ( 'NONE',  ( 11.78445004594039958, 1427.574272142750033, 147.3232557260809870 ) ) ;
#42099 = CARTESIAN_POINT ( 'NONE',  ( 20.08410857819999862, 1507.858969061830066, 229.0550880116979897 ) ) ;
#42100 = ORIENTED_EDGE ( 'NONE', *, *, #23843, .T. ) ;
#42101 = CARTESIAN_POINT ( 'NONE',  ( -13.79555462530000121, 1416.822690122329959, 221.9085254461979844 ) ) ;
#42102 = CARTESIAN_POINT ( 'NONE',  ( -16.90776107416510143, 1442.831169986189479, 162.4346387413914385 ) ) ;
#42103 = CARTESIAN_POINT ( 'NONE',  ( -8.341276443498419013, 1436.001163936675994, 211.2993112092940180 ) ) ;
#42104 = CIRCLE ( 'NONE', #54674, 10.31100486199999722 ) ;
#42105 = CARTESIAN_POINT ( 'NONE',  ( -3.505398281758470791, 1488.737999217582001, 219.4357265464652755 ) ) ;
#42106 = CARTESIAN_POINT ( 'NONE',  ( 21.47248244664589834, 1409.703582322209968, 206.3643650589729930 ) ) ;
#42107 = CARTESIAN_POINT ( 'NONE',  ( -8.085907062746878537, 1446.678893608761427, 154.0132172026529531 ) ) ;
#42108 = CARTESIAN_POINT ( 'NONE',  ( -10.52442967350000025, 1471.882653751090174, 205.8053291943989791 ) ) ;
#42109 = CARTESIAN_POINT ( 'NONE',  ( -7.854300036778085747, 1410.563322333322276, 187.7028744996234764 ) ) ;
#42110 = CARTESIAN_POINT ( 'NONE',  ( -63.99844030340000245, 1379.735010176050082, 270.2820024461590265 ) ) ;
#42111 = CARTESIAN_POINT ( 'NONE',  ( -15.58140587179999947, 1473.850404518229880, 223.6693376217980074 ) ) ;
#42113 = CARTESIAN_POINT ( 'NONE',  ( 2.487935122070182192, 1508.611350403214601, 213.8000011285579092 ) ) ;
#42112 = LINE ( 'NONE', #86861, #12810 ) ;
#42114 = CARTESIAN_POINT ( 'NONE',  ( -68.45261304034977456, 1379.747725225361137, 280.0177415625872186 ) ) ;
#42115 = B_SPLINE_SURFACE_WITH_KNOTS ( 'NONE', 5, 5, ( 
 ( #8207, #15498, #8761, #77101, #42373, #43497, #50253, #42942, #77641, #409, #50781, #51896, #92227, #84382, #34526, #60297, #94414, #953, #67600, #101159, #33405, #92775, #17692, #66513 ),
 ( #83826, #58095, #7126, #7668, #101709, #75455, #25001, #27785, #70935, #61418, #78746, #69821, #28340, #36741, #79304, #61974, #62535, #96088, #19364, #53567, #35628, #52456, #10992, #94994 ),
 ( #87712, #44045, #19925, #2616, #2061, #105051, #36193, #70377, #18262, #104494, #79858, #69258, #78184, #1495, #96656, #53008, #45164, #103939, #86586, #54125, #88252, #11545, #45720, #27237 ),
 ( #3168, #9877, #87142, #10432, #37300, #71493, #95541, #26669, #35078, #103366, #18813, #44603, #60868, #110504, #7490, #9692, #50064, #8035, #8585, #34349, #16957, #43860, #25371, #59017 ),
 ( #59563, #94809, #86404, #60123, #41651, #17516, #78007, #16412, #33784, #25926, #68526, #224, #767, #76356, #51158, #50606, #69084, #43317, #9153, #76916, #103185, #102625, #94241, #51715 ),
 ( #85854, #75807, #101525, #92587, #77465, #1313, #34896, #85285, #42754, #26488, #58459, #35453, #84738, #60683, #18084, #52279, #67981, #67426, #24813, #69641, #93144, #24278, #42205, #15858 ) ),
 .UNSPECIFIED., .F., .F., .F.,
 ( 6, 6 ),
 ( 6, 3, 3, 3, 3, 3, 3, 6 ),
 ( 50.65640425731359642, 99.21450639910000291 ),
 ( 27.66900091189999955, 34.04388441780000107, 36.53848016469999749, 37.78577803820000014, 38.40942697490000057, 39.03307591160000101, 39.72592191760000446, 40.41939032376900087 ),
 .UNSPECIFIED. ) ;
#42116 = CARTESIAN_POINT ( 'NONE',  ( -2.499950827471990156, 1420.113971994240046, 91.17141353883751265 ) ) ;
#42117 = ORIENTED_EDGE ( 'NONE', *, *, #108440, .T. ) ;
#42118 = CARTESIAN_POINT ( 'NONE',  ( -3.801724533410361317, 1509.034510030706087, 204.6344869826262709 ) ) ;
#42119 = CARTESIAN_POINT ( 'NONE',  ( -21.53712143570538373, 1523.621879633028811, 234.3036048850999578 ) ) ;
#42120 = CARTESIAN_POINT ( 'NONE',  ( -3.449777353855000062, 1516.974592746400049, 214.1332139170270068 ) ) ;
#42121 = CARTESIAN_POINT ( 'NONE',  ( -2.975995255039647791, 1485.562730373825843, 182.7647656639549893 ) ) ;
#42122 = DIRECTION ( 'NONE',  ( -0.8090169943749551118, 0.000000000000000000, -0.5877852522924625900 ) ) ;
#42124 = VERTEX_POINT ( 'NONE', #64229 ) ;
#42123 = CARTESIAN_POINT ( 'NONE',  ( -11.38664936716510034, 1500.852607708580081, 211.0998368167220178 ) ) ;
#42125 = CARTESIAN_POINT ( 'NONE',  ( 1.121218210719999941, 1416.837080253930026, 190.1583376728979999 ) ) ;
#42126 = CARTESIAN_POINT ( 'NONE',  ( -0.9795538395430010148, 1508.551704408389924, 220.0924926876990071 ) ) ;
#42127 = CARTESIAN_POINT ( 'NONE',  ( -11.70642185290000015, 1427.901906309730066, 149.0556982179979855 ) ) ;
#42128 = CARTESIAN_POINT ( 'NONE',  ( -10.89398335968819609, 1427.232626390989253, 149.7228750583091426 ) ) ;
#42129 = CARTESIAN_POINT ( 'NONE',  ( -5.672962389570000319, 1441.121347655589943, 185.4629166390980117 ) ) ;
#42130 = CARTESIAN_POINT ( 'NONE',  ( 16.74268639634610167, 1509.497727879889908, 233.3777497809320209 ) ) ;
#42131 = LINE ( 'NONE', #57846, #57376 ) ;
#42132 = CARTESIAN_POINT ( 'NONE',  ( 0.2751658889820000065, 1506.798305107329952, 186.8348836488979998 ) ) ;
#42134 = CARTESIAN_POINT ( 'NONE',  ( -10.18972684899999948, 1478.941447477790007, 211.7723057433990164 ) ) ;
#42133 = CARTESIAN_POINT ( 'NONE',  ( -21.53048477309999953, 1495.369685639130012, 225.8950395148980022 ) ) ;
#42135 = CARTESIAN_POINT ( 'NONE',  ( -16.12914238563999803, 1459.079501637530029, 229.9877974799539970 ) ) ;
#42136 = ORIENTED_EDGE ( 'NONE', *, *, #37776, .F. ) ;
#42137 = CARTESIAN_POINT ( 'NONE',  ( 1.702754371344999962, 1517.014196759610059, 205.6580786742169948 ) ) ;
#42138 = CARTESIAN_POINT ( 'NONE',  ( 31.50789225850000008, 1415.566663160229837, 266.5723572024979831 ) ) ;
#42139 = CARTESIAN_POINT ( 'NONE',  ( 23.61230825720000226, 1435.322028862560046, 137.2857987807979896 ) ) ;
#42140 = CARTESIAN_POINT ( 'NONE',  ( 18.72836455420000235, 1430.305649525229910, 193.0986251508980160 ) ) ;
#42141 = CARTESIAN_POINT ( 'NONE',  ( -0.03116252646638100615, 1508.849096702560018, 238.3754306579919842 ) ) ;
#42142 = VECTOR ( 'NONE', #3531, 1000.000000000000227 ) ;
#42143 = CARTESIAN_POINT ( 'NONE',  ( -9.817630982705171760, 1389.998136714420298, 216.6420858646567353 ) ) ;
#42144 = CARTESIAN_POINT ( 'NONE',  ( -1.418593301179999822, 1450.896267606680112, 183.3515803373980191 ) ) ;
#42145 = CARTESIAN_POINT ( 'NONE',  ( 6.415419946120000105, 1464.066614333030202, 235.9991510476980068 ) ) ;
#42146 = CARTESIAN_POINT ( 'NONE',  ( -15.77622222279999953, 1417.628996888570100, 204.9296672929689862 ) ) ;
#42147 = CARTESIAN_POINT ( 'NONE',  ( -13.52632321789999992, 1443.506831778320247, 187.5835459910979921 ) ) ;
#42148 = LINE ( 'NONE', #103131, #69415 ) ;
#42149 = B_SPLINE_SURFACE_WITH_KNOTS ( 'NONE', 5, 5, ( 
 ( #12871, #37532, #73343, #12317, #105288, #45408, #38081, #38622, #90120, #47051, #46507, #20704 ),
 ( #63857, #47591, #54900, #62780, #72258, #96894, #106388, #39168, #89579, #11247, #20165, #21240 ),
 ( #79548, #81175, #4491, #106927, #29673, #30215, #72800, #64406, #88492, #81715, #107477, #30775 ),
 ( #66620, #33511, #75009, #108591, #50364, #109159, #24004, #15057, #32972, #108028, #99617, #31325 ),
 ( #32443, #40832, #65508, #23474, #56548, #82288, #91237, #58200, #22902, #83377, #6678, #41397 ),
 ( #75562, #76099, #48150, #57667, #109697, #101259, #31878, #7778, #92328, #57110, #14516, #48706 ),
 ( #82830, #6122, #49256, #83936, #84490, #90676, #15599, #40278, #41944, #13961, #100722, #5586 ),
 ( #74463, #66066, #39736, #67161, #100190, #91779, #49804, #24557, #7237, #58745, #92884, #110237 ),
 ( #16161, #67712, #22347, #73902, #17253, #60979, #76641, #59319, #35750, #77213, #25669, #103487 ),
 ( #110793, #26791, #516, #42485, #85575, #17807, #34086, #26226, #85031, #9992, #86148, #95104 ),
 ( #18370, #87257, #94533, #10549, #69377, #93431, #53120, #44162, #34641, #51445, #52008, #68825 ),
 ( #104049, #102926, #8323, #9441, #50900, #8872, #44722, #52565, #2180, #68279, #1065, #60416 ) ),
 .UNSPECIFIED., .F., .F., .F.,
 ( 6, 3, 3, 6 ),
 ( 6, 3, 3, 6 ),
 ( 6.280178283895380353, 6.736940245399999583, 7.650418229669999626, 8.353136552314619934 ),
 ( -2.296936462289909714E-05, 0.3577959157660000056, 1.028223679459999929, 1.454028915480000128 ),
 .UNSPECIFIED. ) ;
#42150 = CARTESIAN_POINT ( 'NONE',  ( -13.40958089250450058, 1414.996442620860080, 220.3303868550709694 ) ) ;
#42151 = CARTESIAN_POINT ( 'NONE',  ( -5.512326787969999309, 1497.963565169690128, 220.3136703888989985 ) ) ;
#42152 = CARTESIAN_POINT ( 'NONE',  ( -3.681141709870000334, 1470.728927551090010, 189.4465201588989771 ) ) ;
#42153 = CARTESIAN_POINT ( 'NONE',  ( -18.17365796220000007, 1441.208305948289762, 213.5442559039389891 ) ) ;
#42154 = CARTESIAN_POINT ( 'NONE',  ( -11.96878399152000050, 1507.593741218769992, 208.5523078654620122 ) ) ;
#42155 = FACE_OUTER_BOUND ( 'NONE', #6120, .T. ) ;
#42156 = CARTESIAN_POINT ( 'NONE',  ( -7.003472331669999384, 1474.927564370629852, 269.4815203934979877 ) ) ;
#42157 = CARTESIAN_POINT ( 'NONE',  ( -18.26023438560000045, 1443.256148476890075, 213.5656046648789754 ) ) ;
#42158 = CARTESIAN_POINT ( 'NONE',  ( -13.86349730046637774, 1513.912023431221542, 192.4354951056943435 ) ) ;
#42159 = CARTESIAN_POINT ( 'NONE',  ( -24.14549998876145764, 1444.489244581972571, 211.6571596010163034 ) ) ;
#42160 = CARTESIAN_POINT ( 'NONE',  ( -59.61913777331309916, 1384.697267862580020, 280.3101250345580411 ) ) ;
#42161 = CARTESIAN_POINT ( 'NONE',  ( -14.88313348660000024, 1507.431571772529878, 226.1823695288979934 ) ) ;
#42162 = CARTESIAN_POINT ( 'NONE',  ( -3.329166574300000292, 1441.604926038239910, 155.7074624611979914 ) ) ;
#42163 = CARTESIAN_POINT ( 'NONE',  ( -106.5791719940000064, 1378.913060387289988, 301.6884094550590021 ) ) ;
#42164 = CARTESIAN_POINT ( 'NONE',  ( 5.478408486960455903, 1471.900903316932499, 217.7034505013053547 ) ) ;
#42165 = CARTESIAN_POINT ( 'NONE',  ( -14.94140562103229897, 1495.722860151610121, 224.6009365516689797 ) ) ;
#42166 = AXIS2_PLACEMENT_3D ( 'NONE', #29071, #45885, #80022 ) ;
#42167 = CARTESIAN_POINT ( 'NONE',  ( -21.71184628989999865, 1409.671254766829861, 205.3856355629080213 ) ) ;
#42168 = CARTESIAN_POINT ( 'NONE',  ( -9.125244859669765063, 1381.433788410652596, 200.7127777233266954 ) ) ;
#42169 = ADVANCED_FACE ( 'NONE', ( #14335 ), #57483, .T. ) ;
#42170 = CARTESIAN_POINT ( 'NONE',  ( 4.955221929980000439, 1484.956700206389996, 218.7828209749189909 ) ) ;
#42171 = CARTESIAN_POINT ( 'NONE',  ( 2.853106639830000072E-11, 1406.768167790330153, 269.6447283206980501 ) ) ;
#42172 = EDGE_CURVE ( 'NONE', #100706, #2433, #67462, .T. ) ;
#42173 = CARTESIAN_POINT ( 'NONE',  ( 1.669693912109999845, 1443.913060387330006, 150.7596247526980164 ) ) ;
#42174 = CARTESIAN_POINT ( 'NONE',  ( 20.38104524799999950, 1433.225738552389885, 214.6696956538789891 ) ) ;
#42175 = CARTESIAN_POINT ( 'NONE',  ( -6.648384463103849562, 1508.610125760109895, 216.2179245631680260 ) ) ;
#42176 = AXIS2_PLACEMENT_3D ( 'NONE', #57140, #14546, #48179 ) ;
#42177 = LINE ( 'NONE', #18599, #35710 ) ;
#42179 = CARTESIAN_POINT ( 'NONE',  ( -12.83815065481509876, 1379.340893115409926, 211.5974809773499885 ) ) ;
#42178 = CARTESIAN_POINT ( 'NONE',  ( 2.500000000000000000, 1419.524771318244348, 137.0999999980979851 ) ) ;
#42180 = CARTESIAN_POINT ( 'NONE',  ( 11.70815223902249969, 1426.714662349520040, 142.1026649480299966 ) ) ;
#42181 = CARTESIAN_POINT ( 'NONE',  ( 9.819515741042740942, 1435.473629839329988, 209.0286173952219997 ) ) ;
#42182 = CARTESIAN_POINT ( 'NONE',  ( -14.51552834752570043, 1420.580226155020000, 213.2889873630980162 ) ) ;
#42183 = CARTESIAN_POINT ( 'NONE',  ( 3.375977085881459949, 1446.395221913229989, 199.5681764770490076 ) ) ;
#42184 = CARTESIAN_POINT ( 'NONE',  ( -0.02192817098988990299, 1407.539782047199878, 222.1835171467989767 ) ) ;
#42185 = CARTESIAN_POINT ( 'NONE',  ( -6.944231786295000042, 1516.882690742909972, 202.5683215544970039 ) ) ;
#42186 = FACE_OUTER_BOUND ( 'NONE', #29934, .T. ) ;
#42187 = DIRECTION ( 'NONE',  ( 1.000000000000000000, 0.000000000000000000, 0.000000000000000000 ) ) ;
#42188 = DIRECTION ( 'NONE',  ( -1.000000000000000000, 0.000000000000000000, 0.000000000000000000 ) ) ;
#42189 = DIRECTION ( 'NONE',  ( -0.7071067811865492381, 0.000000000000000000, 0.7071067811865457964 ) ) ;
#42190 = CARTESIAN_POINT ( 'NONE',  ( -6.500000019064997581, 1515.051704408389924, 209.1218459511669892 ) ) ;
#42191 = CARTESIAN_POINT ( 'NONE',  ( 20.49662116624929808, 1508.357926176179944, 228.4036846774660034 ) ) ;
#42193 = ORIENTED_EDGE ( 'NONE', *, *, #14490, .T. ) ;
#42192 = CARTESIAN_POINT ( 'NONE',  ( -54.40028651508519886, 1379.725038095049968, 254.0986852477319928 ) ) ;
#42194 = EDGE_CURVE ( 'NONE', #54705, #86845, #81109, .T. ) ;
#42195 = VERTEX_POINT ( 'NONE', #92159 ) ;
#42196 = CARTESIAN_POINT ( 'NONE',  ( 11.94807789040000046, 1434.016817471380136, 150.6813232005980012 ) ) ;
#42197 = CARTESIAN_POINT ( 'NONE',  ( 0.02816728215279999670, 1396.454734798429854, 221.5795905766979956 ) ) ;
#42198 = ORIENTED_EDGE ( 'NONE', *, *, #63062, .T. ) ;
#42199 = CARTESIAN_POINT ( 'NONE',  ( -106.8784014550000023, 1378.913059888100179, 307.4679267909590408 ) ) ;
#42200 = CARTESIAN_POINT ( 'NONE',  ( -3.487592468028334114, 1508.783371651612924, 213.6678281800169259 ) ) ;
#42201 = CARTESIAN_POINT ( 'NONE',  ( 3.582837879391640001, 1515.224507406410112, 205.0446031332039922 ) ) ;
#42202 =( BOUNDED_SURFACE ( )  B_SPLINE_SURFACE ( 3, 2, ( 
 ( #65844, #13190, #74793 ),
 ( #5366, #108936, #32226 ),
 ( #66405, #93223, #77544 ),
 ( #24892, #17595, #66952 ),
 ( #43394, #41177, #75351 ),
 ( #32768, #60198, #848 ) ),
 .UNSPECIFIED., .F., .F., .F. ) 
 B_SPLINE_SURFACE_WITH_KNOTS ( ( 4, 2, 4 ),
 ( 3, 3 ),
 ( 2.211772431870429045E-17, 0.001312027981647160809, 0.002624055963294299500 ),
 ( 0.000000000000000000, 1.000000000000000000 ),
 .UNSPECIFIED. ) 
 GEOMETRIC_REPRESENTATION_ITEM ( )  RATIONAL_B_SPLINE_SURFACE ( (
 ( 1.000000000000000000, 0.9376006582766006625, 1.000000000000000000),
 ( 1.000000000000000000, 0.9569320108033070316, 1.000000000000000000),
 ( 1.000000000000000000, 0.9725743441605053663, 1.000000000000000000),
 ( 1.000000000000000000, 0.9942095667149576377, 1.000000000000000000),
 ( 1.000000000000000000, 1.000043666449661917, 1.000000000000000000),
 ( 1.000000000000000000, 1.000000000000000000, 1.000000000000000000) ) ) 
 REPRESENTATION_ITEM ( '' )  SURFACE ( )  );
#42204 = CARTESIAN_POINT ( 'NONE',  ( -14.10445144186040167, 1509.241981962429918, 183.4385781783369964 ) ) ;
#42203 = DIRECTION ( 'NONE',  ( -0.6736849260863841948, 0.000000000000000000, 0.7390186874254148774 ) ) ;
#42205 = CARTESIAN_POINT ( 'NONE',  ( 19.83834310884089902, 1507.818237620550008, 229.2329726552200100 ) ) ;
#42206 = CARTESIAN_POINT ( 'NONE',  ( 6.468572857769999906, 1468.699776068629944, 184.1927265961979856 ) ) ;
#42207 = CARTESIAN_POINT ( 'NONE',  ( -4.912413666740000018, 1414.913060387329779, 193.3950669238979856 ) ) ;
#42208 = DIRECTION ( 'NONE',  ( 6.706399138190049698E-17, -1.000000000000000000, 0.000000000000000000 ) ) ;
#42209 = CARTESIAN_POINT ( 'NONE',  ( 1.694385804820909946, 1395.972229643439960, 198.2391840958000273 ) ) ;
#42210 = CARTESIAN_POINT ( 'NONE',  ( 1.499137190340000148, 1414.988017874730076, 191.7262494343979995 ) ) ;
#42211 = CARTESIAN_POINT ( 'NONE',  ( 11.29663592990000076, 1431.956444431130194, 151.5122984544979943 ) ) ;
#42212 = CARTESIAN_POINT ( 'NONE',  ( 5.763076004854999823, 1514.407352313670117, 201.4560207676169910 ) ) ;
#42213 = ORIENTED_EDGE ( 'NONE', *, *, #108576, .T. ) ;
#42214 = CARTESIAN_POINT ( 'NONE',  ( 13.48799209720280068, 1435.249280822409901, 149.8908522090940210 ) ) ;
#42215 = ORIENTED_EDGE ( 'NONE', *, *, #109746, .F. ) ;
#42216 = ORIENTED_EDGE ( 'NONE', *, *, #19715, .F. ) ;
#42217 = CARTESIAN_POINT ( 'NONE',  ( 13.15321365204082937, 1444.754408317047137, 169.3979468993565547 ) ) ;
#42218 = CARTESIAN_POINT ( 'NONE',  ( -4.160884814660000153, 1464.635754290229897, 236.0840284009980223 ) ) ;
#42219 = CARTESIAN_POINT ( 'NONE',  ( 27.70127829715709922, 1509.880410340700564, 198.6376133113687388 ) ) ;
#42220 = CARTESIAN_POINT ( 'NONE',  ( -0.7396922758749979732, 1517.135701590510052, 216.4591432822169850 ) ) ;
#42221 = CARTESIAN_POINT ( 'NONE',  ( -6.915889783819999970, 1473.238612257490104, 208.0311295836789895 ) ) ;
#42222 = ADVANCED_FACE ( 'NONE', ( #83211 ), #81538, .F. ) ;
#42223 = CARTESIAN_POINT ( 'NONE',  ( 11.84666127166159910, 1421.909629712770084, 209.1686410009280053 ) ) ;
#42224 = CARTESIAN_POINT ( 'NONE',  ( -19.53786426059057746, 1512.187213306747481, 181.5239794925695946 ) ) ;
#42225 = CARTESIAN_POINT ( 'NONE',  ( -29.19545364349999872, 1375.228231664269970, 214.3784411298690031 ) ) ;
#42226 = VECTOR ( 'NONE', #80383, 1000.000000000000000 ) ;
#42227 = B_SPLINE_CURVE_WITH_KNOTS ( 'NONE', 3,
 ( #91930, #76788, #105, #15202, #32027, #32587, #49393, #83521, #100863, #60006, #6815, #40974, #94127, #109301, #108736, #79018, #70080, #10695, #71173, #53826, #69522, #68967, #104193, #70624, #87965, #2319, #85727, #35333, #44867, #53261, #11254 ),
 .UNSPECIFIED., .F., .F.,
 ( 4, 3, 3, 3, 3, 3, 3, 3, 3, 3, 4 ),
 ( -9.981901822019999315, -7.493366175190000256, -7.462945440909900086, -7.082627746929741619, -6.854993841720989245, -6.664003371819999799, -6.519631016808869362, -5.825253142550000263, -5.772861621891269834, -4.972392862104999978, -4.119532581659999693 ),
 .UNSPECIFIED. ) ;
#42228 = ADVANCED_FACE ( 'NONE', ( #4839 ), #10645, .T. ) ;
#42229 = VERTEX_POINT ( 'NONE', #98353 ) ;
#42230 = CARTESIAN_POINT ( 'NONE',  ( -7.337153806245000354, 1517.119374999550018, 205.8621166342670108 ) ) ;
#42231 = ORIENTED_EDGE ( 'NONE', *, *, #88087, .T. ) ;
#42232 = CARTESIAN_POINT ( 'NONE',  ( -105.5846808233909968, 1377.935441088430025, 304.0467934059079766 ) ) ;
#42233 = CARTESIAN_POINT ( 'NONE',  ( -19.65556552330000173, 1509.582207740129888, 230.9700502577980217 ) ) ;
#42234 = CARTESIAN_POINT ( 'NONE',  ( -5.821460640849999812, 1409.620882950629948, 187.3298282121979810 ) ) ;
#42235 = CARTESIAN_POINT ( 'NONE',  ( 6.809551132454999767, 1512.240414293160029, 216.3848881498070114 ) ) ;
#42237 = ORIENTED_EDGE ( 'NONE', *, *, #64081, .F. ) ;
#42236 = CARTESIAN_POINT ( 'NONE',  ( -2.472546487080370170, 1422.360492482099744, 192.6709265187130029 ) ) ;
#42238 = CARTESIAN_POINT ( 'NONE',  ( 24.42325426270000222, 1438.217997540760052, 213.0745112425780121 ) ) ;
#42239 = DIRECTION ( 'NONE',  ( 0.03450791125932765879, 0.9994044208155703490, 8.783400807868103433E-05 ) ) ;
#42240 = CARTESIAN_POINT ( 'NONE',  ( 13.80599381087229993, 1434.979619881599774, 146.4346930152470065 ) ) ;
#42241 = CARTESIAN_POINT ( 'NONE',  ( -31.23437356469425907, 1512.187213306747481, 222.8968241038848248 ) ) ;
#42242 = LINE ( 'NONE', #104353, #21663 ) ;
#42243 = CARTESIAN_POINT ( 'NONE',  ( 4.040527303974999818, 1516.815231249920089, 213.7327841816070020 ) ) ;
#42244 = CARTESIAN_POINT ( 'NONE',  ( -3.812371247207599900, 1428.459941768050157, 200.5740418269730014 ) ) ;
#42245 = CIRCLE ( 'NONE', #2950, 2.000000000000003553 ) ;
#42246 = DIRECTION ( 'NONE',  ( -1.000000000000000000, 0.000000000000000000, 0.000000000000000000 ) ) ;
#42247 = CARTESIAN_POINT ( 'NONE',  ( 6.140129320397309520, 1508.880864719049896, 216.6292689899020161 ) ) ;
#42248 = CARTESIAN_POINT ( 'NONE',  ( -6.546302780145000000, 1516.577434278289957, 211.6089493897669911 ) ) ;
#42249 = CARTESIAN_POINT ( 'NONE',  ( 31.70762145559999468, 1417.952368988429953, 271.1218459616979999 ) ) ;
#42250 = CARTESIAN_POINT ( 'NONE',  ( 14.52033014849999759, 1409.926738468830081, 191.6835547760979921 ) ) ;
#42251 = PLANE ( 'NONE',  #11762 ) ;
#42253 = ORIENTED_EDGE ( 'NONE', *, *, #87706, .T. ) ;
#42252 = CARTESIAN_POINT ( 'NONE',  ( -75.41155982419999759, 1386.723053008149918, 276.7375609186589713 ) ) ;
#42254 = CARTESIAN_POINT ( 'NONE',  ( -62.29399749175660617, 1385.055196683239956, 284.7151661488870218 ) ) ;
#42255 = CARTESIAN_POINT ( 'NONE',  ( 27.90885394509999884, 1457.406260637129890, 250.2249407756980020 ) ) ;
#42256 = CARTESIAN_POINT ( 'NONE',  ( -4.409129114201552291, 1370.458449300261009, 208.8325715886037983 ) ) ;
#42257 = CARTESIAN_POINT ( 'NONE',  ( -8.076961596850001257, 1418.814380367629838, 233.3636024205979993 ) ) ;
#42258 = CARTESIAN_POINT ( 'NONE',  ( 10.46737760179999910, 1424.278704277569886, 206.5802270637989864 ) ) ;
#42259 = CARTESIAN_POINT ( 'NONE',  ( -0.7183524226490148878, 1444.865767701265895, 218.0773563375222182 ) ) ;
#42261 = CARTESIAN_POINT ( 'NONE',  ( -8.581307216309999930, 1384.896522437119984, 218.6696871011889982 ) ) ;
#42260 = CARTESIAN_POINT ( 'NONE',  ( -3.152270375085599596, 1474.954422185709745, 198.1306180807430053 ) ) ;
#42262 = CARTESIAN_POINT ( 'NONE',  ( -9.161971811502120033, 1449.701013728480120, 209.8667376539109739 ) ) ;
#42263 = CARTESIAN_POINT ( 'NONE',  ( -108.9612952299529951, 1383.599948435660053, 311.0484762934830201 ) ) ;
#42264 = ORIENTED_EDGE ( 'NONE', *, *, #94494, .T. ) ;
#42265 = CARTESIAN_POINT ( 'NONE',  ( -2.486474780875000512, 1516.560253536979872, 202.1879665292270261 ) ) ;
#42266 = CARTESIAN_POINT ( 'NONE',  ( 0.1071766512309999947, 1406.264975254330011, 269.2947192205979832 ) ) ;
#42267 = CARTESIAN_POINT ( 'NONE',  ( -0.04693436202600000107, 1467.618576924229956, 229.5068687307980042 ) ) ;
#42268 = CARTESIAN_POINT ( 'NONE',  ( 24.60632226619999940, 1440.982747020230136, 212.6699546725280072 ) ) ;
#42269 = CARTESIAN_POINT ( 'NONE',  ( 37.90967934912709580, 1445.000095422539971, 137.0440870150370074 ) ) ;
#42270 = CARTESIAN_POINT ( 'NONE',  ( -121.0090375485666527, 1390.939237335599955, 306.1199062271713274 ) ) ;
#42271 = CARTESIAN_POINT ( 'NONE',  ( 4.363541942640000393, 1466.192484605890058, 218.8344587469289877 ) ) ;
#42272 = CARTESIAN_POINT ( 'NONE',  ( 15.32734268939944933, 1420.809437254912609, 227.7941278867960762 ) ) ;
#42273 = CARTESIAN_POINT ( 'NONE',  ( 32.65728749220649973, 1435.637725527470138, 135.5426019811650065 ) ) ;
#42274 = CARTESIAN_POINT ( 'NONE',  ( 39.40243926798699903, 1447.114675383599888, 136.6257780722449979 ) ) ;
#42275 = CARTESIAN_POINT ( 'NONE',  ( -18.51436573157397092, 1511.187213306747708, 181.1015051776554969 ) ) ;
#42276 = CARTESIAN_POINT ( 'NONE',  ( -109.3312173139999999, 1385.266030154929922, 297.1495261968589716 ) ) ;
#42277 = CARTESIAN_POINT ( 'NONE',  ( -9.803834995107230554, 1522.051704408389924, 196.6215198571080123 ) ) ;
#42278 = CARTESIAN_POINT ( 'NONE',  ( -20.72500163405283047, 1525.697946996666815, 184.6549699785309144 ) ) ;
#42279 = CARTESIAN_POINT ( 'NONE',  ( -9.901400372228881253, 1447.905338697959905, 209.8163239975949637 ) ) ;
#42280 = VERTEX_POINT ( 'NONE', #58024 ) ;
#42281 = CARTESIAN_POINT ( 'NONE',  ( -8.937053649178221093, 1440.468819487419978, 205.6155253440409751 ) ) ;
#42283 = VERTEX_POINT ( 'NONE', #90498 ) ;
#42282 = CARTESIAN_POINT ( 'NONE',  ( -44.12252941662215022, 1432.101884911245406, 269.0173719654496836 ) ) ;
#42284 = CARTESIAN_POINT ( 'NONE',  ( -4.832613825698169663, 1508.551704408610021, 212.6094309338790254 ) ) ;
#42285 = CARTESIAN_POINT ( 'NONE',  ( 15.73707872690769882, 1469.695642903600174, 189.2816229824940137 ) ) ;
#42286 = FACE_OUTER_BOUND ( 'NONE', #55227, .T. ) ;
#42287 = CARTESIAN_POINT ( 'NONE',  ( 12.13166762299999846, 1501.269883488590040, 211.0250359440489660 ) ) ;
#42288 = CARTESIAN_POINT ( 'NONE',  ( 19.60089115691128470, 1455.490215338870485, 226.0492849636472954 ) ) ;
#42289 = CARTESIAN_POINT ( 'NONE',  ( 8.185066571180000139, 1426.771507121280138, 211.5403165378289714 ) ) ;
#42290 = LINE ( 'NONE', #93767, #41812 ) ;
#42291 = CARTESIAN_POINT ( 'NONE',  ( -13.93937700741352792, 1420.276149642025757, 227.5832580472266216 ) ) ;
#42292 = CARTESIAN_POINT ( 'NONE',  ( -33.93019615848961479, 1524.726013923371283, 197.6607374646001460 ) ) ;
#42293 = CARTESIAN_POINT ( 'NONE',  ( -7.542243412319999507, 1483.743633471490057, 200.8664480738789848 ) ) ;
#42294 = CARTESIAN_POINT ( 'NONE',  ( 25.32380175889999663, 1435.401097828169895, 135.8572049329980018 ) ) ;
#42295 = CARTESIAN_POINT ( 'NONE',  ( -10.70803624744210047, 1396.286993253289893, 206.3112538434370151 ) ) ;
#42296 = ORIENTED_EDGE ( 'NONE', *, *, #41774, .T. ) ;
#42297 = CARTESIAN_POINT ( 'NONE',  ( 0.8770414022313379743, 1414.913057846380070, 192.4603704288240067 ) ) ;
#42298 = CARTESIAN_POINT ( 'NONE',  ( 21.03615327617330166, 1508.023275217195760, 226.0759873548938117 ) ) ;
#42299 = ORIENTED_EDGE ( 'NONE', *, *, #3636, .F. ) ;
#42300 = ORIENTED_EDGE ( 'NONE', *, *, #42552, .F. ) ;
#42301 = CARTESIAN_POINT ( 'NONE',  ( 1.026847438530000156, 1494.050500594489904, 217.3813169704690154 ) ) ;
#42302 = CARTESIAN_POINT ( 'NONE',  ( -14.79126394052620164, 1416.133454573002609, 204.7564966609269845 ) ) ;
#42304 = CARTESIAN_POINT ( 'NONE',  ( -17.23416124950000139, 1457.524421634029977, 225.2691253537979890 ) ) ;
#42303 = DIRECTION ( 'NONE',  ( -0.9899229090099358475, 3.338231922391333496E-06, 0.1416073239848933130 ) ) ;
#42305 = CARTESIAN_POINT ( 'NONE',  ( -5.467724459860000330, 1444.780760362290039, 217.3521413719989823 ) ) ;
#42306 = CARTESIAN_POINT ( 'NONE',  ( 4.330481386014059630, 1425.574591470910036, 185.4354870873890206 ) ) ;
#42307 = CARTESIAN_POINT ( 'NONE',  ( -12.30339481767540022, 1378.359469321360166, 209.9065742530260081 ) ) ;
#42308 = FACE_OUTER_BOUND ( 'NONE', #30494, .T. ) ;
#42309 = CARTESIAN_POINT ( 'NONE',  ( 7.578931200799999601, 1423.300307201199985, 213.4057882997690001 ) ) ;
#42310 = CARTESIAN_POINT ( 'NONE',  ( -24.23130728210000129, 1437.896947393770006, 211.0914040829580074 ) ) ;
#42311 = FACE_OUTER_BOUND ( 'NONE', #24686, .T. ) ;
#42312 = FACE_OUTER_BOUND ( 'NONE', #89524, .T. ) ;
#42313 = CARTESIAN_POINT ( 'NONE',  ( 9.663424421700000266, 1363.752474719049815, 207.6218459616989946 ) ) ;
#42314 = CARTESIAN_POINT ( 'NONE',  ( -23.34220398524906770, 1509.843709858650982, 228.0495150535502091 ) ) ;
#42315 = MECHANICAL_DESIGN_GEOMETRIC_PRESENTATION_REPRESENTATION (  '', ( #44087 ), #51268 ) ;
#42317 = ORIENTED_EDGE ( 'NONE', *, *, #50162, .T. ) ;
#42316 = CARTESIAN_POINT ( 'NONE',  ( -2.713960167710639967E-10, 1417.262443616730025, 235.9145977375980010 ) ) ;
#42318 = ORIENTED_EDGE ( 'NONE', *, *, #46910, .T. ) ;
#42319 = ADVANCED_FACE ( 'NONE', ( #108412 ), #17709, .T. ) ;
#42320 = CARTESIAN_POINT ( 'NONE',  ( -11.78715034128589956, 1427.678896089820000, 147.4800145233820103 ) ) ;
#42321 = CARTESIAN_POINT ( 'NONE',  ( 7.530701491966509842, 1510.600498152046157, 203.2644113281531304 ) ) ;
#42322 = CARTESIAN_POINT ( 'NONE',  ( 12.42529224677513078, 1517.051704408389924, 202.6823640254548309 ) ) ;
#42323 = CARTESIAN_POINT ( 'NONE',  ( 1.081335638410579891, 1415.752565153090018, 209.4296050402819844 ) ) ;
#42324 = CARTESIAN_POINT ( 'NONE',  ( -126.6653580271999999, 1320.102705746890251, 304.2218459572590064 ) ) ;
#42325 = CARTESIAN_POINT ( 'NONE',  ( 1.775988990176029736, 1526.208281990539717, 240.5699127611650567 ) ) ;
#42326 = CARTESIAN_POINT ( 'NONE',  ( -15.69795926999090163, 1519.551704408389924, 195.4758181584410011 ) ) ;
#42327 = EDGE_CURVE ( 'NONE', #101819, #95045, #4314, .T. ) ;
#42328 = DIRECTION ( 'NONE',  ( 1.000000000000000000, 0.000000000000000000, 0.000000000000000000 ) ) ;
#42329 = CARTESIAN_POINT ( 'NONE',  ( -22.93376428353440488, 1507.619498552430059, 207.7003816026530103 ) ) ;
#42330 = CARTESIAN_POINT ( 'NONE',  ( 10.90489178456198793, 1367.786170745731170, 209.6218459617033432 ) ) ;
#42331 = CARTESIAN_POINT ( 'NONE',  ( -9.909475446137518517, 1446.884018808590099, 211.9943844666950099 ) ) ;
#42332 = CARTESIAN_POINT ( 'NONE',  ( -20.49050045394660202, 1409.815506645270034, 269.1358135908449754 ) ) ;
#42333 = CARTESIAN_POINT ( 'NONE',  ( -11.07188855570740138, 1414.941240495252941, 195.8493003954075391 ) ) ;
#42334 = VERTEX_POINT ( 'NONE', #99439 ) ;
#42335 = CARTESIAN_POINT ( 'NONE',  ( 2.485536261606702269, 1523.919934424249959, 242.8055311927600144 ) ) ;
#42336 = CARTESIAN_POINT ( 'NONE',  ( 13.81179073420000059, 1445.166753938590091, 189.1769591503979768 ) ) ;
#42337 = ORIENTED_EDGE ( 'NONE', *, *, #69646, .F. ) ;
#42338 = VERTEX_POINT ( 'NONE', #73163 ) ;
#42339 = CARTESIAN_POINT ( 'NONE',  ( 4.571912029077168427, 1422.069887020605847, 184.0289291679942494 ) ) ;
#42340 = CARTESIAN_POINT ( 'NONE',  ( 7.487277797411009850, 1424.824108058459842, 194.2252290839009845 ) ) ;
#42341 = CARTESIAN_POINT ( 'NONE',  ( 3.265407117845000151, 1516.754149861460064, 213.7315192116670062 ) ) ;
#42342 = CARTESIAN_POINT ( 'NONE',  ( 5.106974046795000000, 1511.397837225850026, 217.6801467072069727 ) ) ;
#42343 = CYLINDRICAL_SURFACE ( 'NONE', #7269, 1.000000000000001110 ) ;
#42344 = ORIENTED_EDGE ( 'NONE', *, *, #95973, .F. ) ;
#42345 = CARTESIAN_POINT ( 'NONE',  ( -10.83195828220730839, 1414.913060387329779, 196.7927967275896890 ) ) ;
#42346 = CARTESIAN_POINT ( 'NONE',  ( -6.945490086935000029, 1516.932669162149978, 203.3434733684869968 ) ) ;
#42347 = CARTESIAN_POINT ( 'NONE',  ( -28.68932943090000265, 1509.915949688529963, 202.5637259519879763 ) ) ;
#42348 = CARTESIAN_POINT ( 'NONE',  ( -0.9111207389620000763, 1467.881514926830050, 230.2715671425980020 ) ) ;
#42349 = CARTESIAN_POINT ( 'NONE',  ( -43.08576106324490240, 1384.592750897279984, 216.1018319972359905 ) ) ;
#42350 = CARTESIAN_POINT ( 'NONE',  ( -14.49786657906220100, 1379.669926966970024, 208.2185517401169932 ) ) ;
#42351 = CARTESIAN_POINT ( 'NONE',  ( -13.70772824027479864, 1507.648153509909889, 184.2587339175119894 ) ) ;
#42353 = ORIENTED_EDGE ( 'NONE', *, *, #70651, .F. ) ;
#42352 = CARTESIAN_POINT ( 'NONE',  ( 8.464772015878761380, 1517.051704408389924, 233.7053289272598420 ) ) ;
#42354 = CARTESIAN_POINT ( 'NONE',  ( 6.126746143464999683, 1514.923664147150021, 200.9956116846470309 ) ) ;
#42355 = CARTESIAN_POINT ( 'NONE',  ( 26.35247771890000124, 1469.246089662630084, 210.6409091504179969 ) ) ;
#42356 = CARTESIAN_POINT ( 'NONE',  ( -58.94826691570873578, 1379.722811456130103, 263.7298695812581855 ) ) ;
#42357 = CARTESIAN_POINT ( 'NONE',  ( -11.16953914610450127, 1480.956324501380095, 211.2841307982869807 ) ) ;
#42358 = CARTESIAN_POINT ( 'NONE',  ( -13.03231315604520191, 1436.015888718699898, 150.7292108121390299 ) ) ;
#42359 = CARTESIAN_POINT ( 'NONE',  ( 3.462948796544999652, 1516.956048353049937, 211.4063724288770061 ) ) ;
#42360 = CARTESIAN_POINT ( 'NONE',  ( -68.56117685350000102, 1379.747432481730129, 279.6402102005590109 ) ) ;
#42361 = AXIS2_PLACEMENT_3D ( 'NONE', #65567, #15656, #31938 ) ;
#42362 = CARTESIAN_POINT ( 'NONE',  ( -14.61893924920000032, 1413.173045456330101, 226.8392015079979842 ) ) ;
#42363 = CARTESIAN_POINT ( 'NONE',  ( 9.586487508724173878, 1493.457082605286359, 189.9081600023157819 ) ) ;
#42364 = CARTESIAN_POINT ( 'NONE',  ( -5.011551406145000165, 1517.080322339569875, 208.3849417611969841 ) ) ;
#42365 = EDGE_LOOP ( 'NONE', ( #105690, #53679, #82467, #91534 ) ) ;
#42366 = DIRECTION ( 'NONE',  ( 0.001614263105669359660, 0.06164622090537569266, -0.9980967576356069015 ) ) ;
#42367 = CARTESIAN_POINT ( 'NONE',  ( -1.387083595259999802, 1410.307627408429880, 232.9611065579980220 ) ) ;
#42368 = CARTESIAN_POINT ( 'NONE',  ( -19.74923653411236657, 1456.849059588098953, 225.6335635741733370 ) ) ;
#42369 = ORIENTED_EDGE ( 'NONE', *, *, #86662, .F. ) ;
#42370 = FACE_OUTER_BOUND ( 'NONE', #48289, .T. ) ;
#42371 = CARTESIAN_POINT ( 'NONE',  ( -3.824657326589999684, 1429.713551423189983, 201.7356720059990209 ) ) ;
#42372 = CARTESIAN_POINT ( 'NONE',  ( 12.80510718569220074, 1435.062306801080240, 150.3516382532390026 ) ) ;
#42373 = CARTESIAN_POINT ( 'NONE',  ( 9.922165068644240193, 1459.297038473970133, 232.1972491097930060 ) ) ;
#42374 = CARTESIAN_POINT ( 'NONE',  ( -14.61243671689999957, 1417.122520118429975, 205.5241932702090253 ) ) ;
#42375 = CARTESIAN_POINT ( 'NONE',  ( 2.493947715939999643, 1442.756953654919926, 150.6345094620980092 ) ) ;
#42376 = CARTESIAN_POINT ( 'NONE',  ( 5.495445188540000636, 1487.154938902290041, 199.6385650399689951 ) ) ;
#42377 = CARTESIAN_POINT ( 'NONE',  ( 2.285841285774699520E-15, 1391.426148861440197, 209.1218459572589836 ) ) ;
#42378 = CARTESIAN_POINT ( 'NONE',  ( 10.49215161174419997, 1461.076717979740124, 208.4970850488610097 ) ) ;
#42380 = FACE_OUTER_BOUND ( 'NONE', #213, .T. ) ;
#42379 = CARTESIAN_POINT ( 'NONE',  ( -3.255340964424999761, 1516.962555622980062, 213.7459452615670159 ) ) ;
#42381 = CARTESIAN_POINT ( 'NONE',  ( 20.10853051189999974, 1509.039643803929948, 188.6705484871980048 ) ) ;
#42382 = CARTESIAN_POINT ( 'NONE',  ( -4.035536263215000474, 1517.086065052259983, 216.8453260496270047 ) ) ;
#42383 = AXIS2_PLACEMENT_3D ( 'NONE', #82034, #5339, #100498 ) ;
#42384 = ORIENTED_EDGE ( 'NONE', *, *, #17225, .F. ) ;
#42385 = CARTESIAN_POINT ( 'NONE',  ( -12.72996574539999948, 1416.826388498530150, 195.1129838194979982 ) ) ;
#42386 = CARTESIAN_POINT ( 'NONE',  ( -16.79355118000000147, 1420.470915882059899, 203.2250788364389678 ) ) ;
#42387 = ORIENTED_EDGE ( 'NONE', *, *, #90708, .F. ) ;
#42388 = CARTESIAN_POINT ( 'NONE',  ( -18.28629418055740175, 1508.551704408389924, 210.6167475138960015 ) ) ;
#42389 = EDGE_CURVE ( 'NONE', #28257, #69866, #40836, .T. ) ;
#42390 = CARTESIAN_POINT ( 'NONE',  ( -105.3229575393603028, 1390.872468168539399, 304.1992835431211120 ) ) ;
#42391 = CARTESIAN_POINT ( 'NONE',  ( 11081.89558200929423, 2833.596074015641989, 8724.858692895628337 ) ) ;
#42392 = CARTESIAN_POINT ( 'NONE',  ( -11.39446592756109844, 1470.674086296440009, 209.5209556861319982 ) ) ;
#42393 = CARTESIAN_POINT ( 'NONE',  ( -4.249061451088596009, 1508.172007302874363, 220.6133281201646810 ) ) ;
#42394 = CARTESIAN_POINT ( 'NONE',  ( 18.89905511659999959, 1416.828040475729949, 210.6687957193779823 ) ) ;
#42395 = EDGE_CURVE ( 'NONE', #47896, #37975, #31882, .T. ) ;
#42396 = DIRECTION ( 'NONE',  ( -3.828568698926946970E-16, 0.000000000000000000, 1.000000000000000000 ) ) ;
#42397 = CARTESIAN_POINT ( 'NONE',  ( -7.013461631340700997, 1458.033762489906394, 215.6076664431717802 ) ) ;
#42398 = CARTESIAN_POINT ( 'NONE',  ( -9289.452348480423097, -2339.359351152911131, 1609.629554519071007 ) ) ;
#42400 = EDGE_CURVE ( 'NONE', #18368, #288, #72993, .T. ) ;
#42399 = CARTESIAN_POINT ( 'NONE',  ( 43.89935492036580200, 1440.913060360979898, 264.2399530293329803 ) ) ;
#42402 = CARTESIAN_POINT ( 'NONE',  ( 4.327091944037150029, 1515.154796665620097, 208.8633048373430086 ) ) ;
#42401 = CARTESIAN_POINT ( 'NONE',  ( -8.367456039295358750, 1418.839936894859875, 195.8971482936690052 ) ) ;
#42403 = CARTESIAN_POINT ( 'NONE',  ( 0.5620975284970839425, 1416.851343896850040, 190.4751211475700075 ) ) ;
#42404 = ORIENTED_EDGE ( 'NONE', *, *, #77466, .T. ) ;
#42405 = VERTEX_POINT ( 'NONE', #31694 ) ;
#42406 = CARTESIAN_POINT ( 'NONE',  ( 1.547340046859259965, 1416.576002133120028, 190.2496894819780096 ) ) ;
#42407 = CARTESIAN_POINT ( 'NONE',  ( 16.78578239015438811, 1409.668514543772062, 192.8593785157384275 ) ) ;
#42408 = CIRCLE ( 'NONE', #105013, 1.999999999999973577 ) ;
#42409 = CARTESIAN_POINT ( 'NONE',  ( -24.41180956639999877, 1441.164382444379953, 212.0429753022879993 ) ) ;
#42410 = CARTESIAN_POINT ( 'NONE',  ( 9.651066088509999474, 1425.440658930580184, 195.4941615409990163 ) ) ;
#42411 = CARTESIAN_POINT ( 'NONE',  ( -3.024617817738020076, 1425.990483723350280, 185.4946073275085894 ) ) ;
#42412 = CARTESIAN_POINT ( 'NONE',  ( 10.29338229012589956, 1422.407096038270083, 211.7839187185859942 ) ) ;
#42413 = CARTESIAN_POINT ( 'NONE',  ( -4.646147325060000277, 1378.399971913189802, 203.6922293430689876 ) ) ;
#42414 = CARTESIAN_POINT ( 'NONE',  ( 18.38166433807079869, 1428.164289305379953, 201.4944191049719961 ) ) ;
#42415 = CARTESIAN_POINT ( 'NONE',  ( -61.13138140197489889, 1383.795200718170008, 282.5130783835299439 ) ) ;
#42416 = CARTESIAN_POINT ( 'NONE',  ( 7.330937150280000481, 1451.832881924430239, 153.4313473593979893 ) ) ;
#42417 = DIRECTION ( 'NONE',  ( 0.9417419115949053898, -0.3363363969979660806, 5.735553207809421716E-15 ) ) ;
#42418 = CARTESIAN_POINT ( 'NONE',  ( 10.92074801238010018, 1490.510034778949830, 210.1931246329349960 ) ) ;
#42420 = ORIENTED_EDGE ( 'NONE', *, *, #31071, .F. ) ;
#42419 = CARTESIAN_POINT ( 'NONE',  ( 23.57479768189999803, 1509.037294151330116, 194.3365427184980092 ) ) ;
#42421 = CARTESIAN_POINT ( 'NONE',  ( 31.95643112691247367, 1526.329757971584741, 216.6807372298920313 ) ) ;
#42422 = CARTESIAN_POINT ( 'NONE',  ( -55.58170576269999685, 1379.125231693479918, 252.4809319844590334 ) ) ;
#42423 = CARTESIAN_POINT ( 'NONE',  ( -20.01979917808080245, 1409.612167179720018, 217.0233986995509952 ) ) ;
#42424 = EDGE_LOOP ( 'NONE', ( #98364, #51169, #65370, #44592 ) ) ;
#42425 = EDGE_LOOP ( 'NONE', ( #96463, #63593, #106626, #45679, #4264 ) ) ;
#42426 = CARTESIAN_POINT ( 'NONE',  ( 19.76863720275370184, 1508.335761315370064, 229.3107344876569869 ) ) ;
#42427 = FACE_OUTER_BOUND ( 'NONE', #36570, .T. ) ;
#42428 = CARTESIAN_POINT ( 'NONE',  ( 39.89315444343499450, 1441.403880509019928, 136.8692038438520058 ) ) ;
#42430 = CYLINDRICAL_SURFACE ( 'NONE', #98487, 23.69926344187880929 ) ;
#42429 = CARTESIAN_POINT ( 'NONE',  ( 0.1681681984989999989, 1432.413060387330006, 146.1721969590979882 ) ) ;
#42431 = CARTESIAN_POINT ( 'NONE',  ( -9.467901848279998589, 1462.744805377290049, 205.1999451337790106 ) ) ;
#42432 = AXIS2_PLACEMENT_3D ( 'NONE', #95706, #18972, #53168 ) ;
#42433 = CARTESIAN_POINT ( 'NONE',  ( -109.4887233469999899, 1383.428478228959875, 297.2448718180590390 ) ) ;
#42434 = CARTESIAN_POINT ( 'NONE',  ( -22.08622291482314282, 1523.382868172864164, 233.8253038720786776 ) ) ;
#42435 = CARTESIAN_POINT ( 'NONE',  ( -12.81082785388507794, 1435.922453314257382, 150.8250786316239953 ) ) ;
#42436 = CARTESIAN_POINT ( 'NONE',  ( 8.013264357029996177, 1375.413060387289988, 209.1218459572589836 ) ) ;
#42437 = CARTESIAN_POINT ( 'NONE',  ( 4.817021387869999671, 1409.081274480830189, 187.8331875977980019 ) ) ;
#42438 = CARTESIAN_POINT ( 'NONE',  ( 4.660105491930000454, 1423.711922466630085, 183.8926758387979703 ) ) ;
#42439 = CARTESIAN_POINT ( 'NONE',  ( 2.625463805309249832, 1431.952376572269941, 200.6791034752619964 ) ) ;
#42440 = CARTESIAN_POINT ( 'NONE',  ( -2.500000000250119925, 1440.023260367290050, 162.2535809969560034 ) ) ;
#42441 = AXIS2_PLACEMENT_3D ( 'NONE', #55535, #21329, #32385 ) ;
#42442 = CARTESIAN_POINT ( 'NONE',  ( -22.21719680079999648, 1451.325171265629933, 143.2349378059979870 ) ) ;
#42443 = CARTESIAN_POINT ( 'NONE',  ( 0.7566313362349998961, 1467.043555274730124, 235.5078946572979817 ) ) ;
#42444 = VERTEX_POINT ( 'NONE', #74825 ) ;
#42445 = CARTESIAN_POINT ( 'NONE',  ( 5.021805632604219305, 1470.186357947040051, 187.8118227978269772 ) ) ;
#42446 = CARTESIAN_POINT ( 'NONE',  ( -11.03352341481849841, 1462.446812322350070, 208.7213867630900097 ) ) ;
#42447 = CARTESIAN_POINT ( 'NONE',  ( 22.12758967943027244, 1506.606278686416999, 209.2169694191676967 ) ) ;
#42448 = CARTESIAN_POINT ( 'NONE',  ( 16.77073029129999782, 1488.221064575230002, 188.9956101863979825 ) ) ;
#42449 = CARTESIAN_POINT ( 'NONE',  ( -1.782192625468050338E-12, 1470.276122712049983, 254.7521491344949993 ) ) ;
#42450 = CARTESIAN_POINT ( 'NONE',  ( 15.85112983123188357, 1436.286788543214243, 149.0859302454996111 ) ) ;
#42452 = EDGE_CURVE ( 'NONE', #4789, #12462, #55831, .T. ) ;
#42451 = CARTESIAN_POINT ( 'NONE',  ( -0.6414547015529999952, 1416.067629290630066, 227.6224876852980117 ) ) ;
#42453 = CARTESIAN_POINT ( 'NONE',  ( -5.007571308570000213, 1417.958038874930025, 233.5392730366980061 ) ) ;
#42454 = CARTESIAN_POINT ( 'NONE',  ( 0.3867091632760010222, 1476.097381945789948, 198.0337097418990027 ) ) ;
#42455 = CARTESIAN_POINT ( 'NONE',  ( -105.2227265700000061, 1389.546011113689929, 307.5960479858590020 ) ) ;
#42456 = CARTESIAN_POINT ( 'NONE',  ( -0.1563126519980407303, 1486.071014054024317, 181.8244914540917421 ) ) ;
#42457 = CARTESIAN_POINT ( 'NONE',  ( 4.644984669262973043, 1358.972932498876844, 208.3718459617010978 ) ) ;
#42458 = CARTESIAN_POINT ( 'NONE',  ( -45.94107864437709310, 1438.459200226280245, 266.6805786380390373 ) ) ;
#42459 = CARTESIAN_POINT ( 'NONE',  ( 3.433134143449350084, 1428.624608639609960, 216.6434505333259892 ) ) ;
#42460 = CARTESIAN_POINT ( 'NONE',  ( -2.858448621680000024, 1443.821599769190016, 199.4616741486989895 ) ) ;
#42461 = EDGE_LOOP ( 'NONE', ( #49535, #67416, #3848, #41099, #5584, #106827, #22348, #113, #8574, #41277, #15849, #73971, #44431, #93153, #61971, #32343, #86394, #40917, #64951, #34024, #89028, #62335, #47949, #59318, #62116, #3399, #110239, #59389, #19064, #102619, #106923, #98669, #89128, #81879, #93226, #96480, #85235, #74875, #104064, #70199, #58351, #71523, #11903, #28165, #72588, #55047, #65867, #69849, #65233, #41645, #38335, #79800, #39050, #55896, #44449, #79415, #70386, #20407, #56065, #81838, #89041, #78647, #96892, #80211, #75288, #99867, #11046, #80159, #68404, #74723, #58198, #63759, #69442, #51011, #23590, #104676, #59313, #40054, #98726, #33368, #105834, #7790, #105140, #49015, #35337, #15547, #57758, #2812, #110805, #48688, #2472, #77842 ) ) ;
#42462 = CARTESIAN_POINT ( 'NONE',  ( 2.292217010694999946, 1516.941178807709775, 209.1086494233340147 ) ) ;
#42463 = CARTESIAN_POINT ( 'NONE',  ( -2.478828574380000038, 1434.283354135890022, 157.5745121407980207 ) ) ;
#42464 = VECTOR ( 'NONE', #47788, 1000.000000000000114 ) ;
#42465 = CARTESIAN_POINT ( 'NONE',  ( -6.657935129248458317, 1470.951763472646689, 216.7381263951724293 ) ) ;
#42466 = CARTESIAN_POINT ( 'NONE',  ( 7.485501385385199491, 1426.034470239760140, 212.3577792365530286 ) ) ;
#42467 = CARTESIAN_POINT ( 'NONE',  ( -26.75494362287030015, 1450.708015636789924, 136.4629296848829938 ) ) ;
#42468 = EDGE_LOOP ( 'NONE', ( #69237, #16443, #93073, #74060, #37121, #104197 ) ) ;
#42469 = CARTESIAN_POINT ( 'NONE',  ( 7.882974896040000345, 1421.108448708030210, 221.4185163294980327 ) ) ;
#42471 = CARTESIAN_POINT ( 'NONE',  ( 14.83720918809999922, 1488.813684183029864, 193.9548961439979848 ) ) ;
#42470 = LINE ( 'NONE', #41930, #4946 ) ;
#42472 = CARTESIAN_POINT ( 'NONE',  ( -2.510232470973990271, 1419.517688769939923, 186.1000036307290202 ) ) ;
#42473 = B_SPLINE_CURVE_WITH_KNOTS ( 'NONE', 5,
 ( #562, #71092, #8930, #27392, #52614, #43653, #43103, #77263, #26847, #95156, #94584, #17864 ),
 .UNSPECIFIED., .F., .F.,
 ( 6, 3, 3, 6 ),
 ( 0.000000000000000000, 0.3740180191949237787, 0.7913393397332487700, 1.000000000000000000 ),
 .UNSPECIFIED. ) ;
#42474 = CARTESIAN_POINT ( 'NONE',  ( -3.829620113550000315, 1515.551704408389924, 207.2788837304390199 ) ) ;
#42475 = CARTESIAN_POINT ( 'NONE',  ( 17.68711869539999881, 1428.828027849089949, 204.9896315466789929 ) ) ;
#42476 = CARTESIAN_POINT ( 'NONE',  ( 3.639548396805570185, 1468.126230336239814, 218.4317111027060037 ) ) ;
#42477 = CARTESIAN_POINT ( 'NONE',  ( 20.79738390328720499, 1511.187213306747708, 181.2030061003470394 ) ) ;
#42478 = ORIENTED_EDGE ( 'NONE', *, *, #7513, .T. ) ;
#42479 = CARTESIAN_POINT ( 'NONE',  ( -2.992362202849540243, 1410.309682308740094, 269.6157897731519597 ) ) ;
#42480 = CARTESIAN_POINT ( 'NONE',  ( 6.324577195401869467, 1417.249146248230090, 231.3662450834670210 ) ) ;
#42481 = CARTESIAN_POINT ( 'NONE',  ( 2.487935123020000194, 1509.038615934189920, 204.6345961887290059 ) ) ;
#42482 = ORIENTED_EDGE ( 'NONE', *, *, #48536, .F. ) ;
#42483 = VERTEX_POINT ( 'NONE', #99997 ) ;
#42484 = B_SPLINE_CURVE_WITH_KNOTS ( 'NONE', 5,
 ( #49386, #40415, #16290, #58336, #57257, #66208 ),
 .UNSPECIFIED., .F., .F.,
 ( 6, 6 ),
 ( 0.000000000000000000, 1.000000000000000000 ),
 .UNSPECIFIED. ) ;
#42485 = CARTESIAN_POINT ( 'NONE',  ( -22.87778797449940171, 1409.742461299279967, 209.5888460124660071 ) ) ;
#42486 = EDGE_CURVE ( 'NONE', #26498, #107758, #38082, .T. ) ;
#42487 = CARTESIAN_POINT ( 'NONE',  ( -11.41709567969999917, 1481.865892882389971, 208.5947888571609781 ) ) ;
#42488 = CARTESIAN_POINT ( 'NONE',  ( 16.42371624802357744, 1409.486589196651948, 222.7146196853670972 ) ) ;
#42489 = VECTOR ( 'NONE', #23380, 1000.000000000000000 ) ;
#42490 = CARTESIAN_POINT ( 'NONE',  ( -45.62084243191078770, 1439.252524108265561, 266.1900039064981343 ) ) ;
#42491 = CARTESIAN_POINT ( 'NONE',  ( -20.37302944780879699, 1486.732096115899822, 192.8446084916569987 ) ) ;
#42492 = CARTESIAN_POINT ( 'NONE',  ( 3.865553273121640210, 1508.610338516509955, 213.5325911278659987 ) ) ;
#42493 = CARTESIAN_POINT ( 'NONE',  ( 39.23058051887299769, 1459.489499153630049, 266.8982678320860487 ) ) ;
#42494 = CARTESIAN_POINT ( 'NONE',  ( -29.79881796581611297, 1526.748660780343471, 221.5803863269308636 ) ) ;
#42495 = CARTESIAN_POINT ( 'NONE',  ( -17.25240610853359513, 1422.435072564651591, 226.6616450818354735 ) ) ;
#42496 = CARTESIAN_POINT ( 'NONE',  ( -3.267603553834999897, 1516.858171774179937, 205.8687047948669999 ) ) ;
#42497 = VERTEX_POINT ( 'NONE', #83757 ) ;
#42498 = CARTESIAN_POINT ( 'NONE',  ( 18.67276003095157932, 1458.371783447332291, 227.3962319617383230 ) ) ;
#42499 = CARTESIAN_POINT ( 'NONE',  ( 15.25249359122459936, 1513.170547668170002, 195.0348937637239999 ) ) ;
#42500 = FACE_OUTER_BOUND ( 'NONE', #81606, .T. ) ;
#42501 = ORIENTED_EDGE ( 'NONE', *, *, #57877, .F. ) ;
#42502 = CARTESIAN_POINT ( 'NONE',  ( 3.439931081349999697, 1448.290196152649969, 184.1542931849980107 ) ) ;
#42503 = CARTESIAN_POINT ( 'NONE',  ( 2.685817909462222985, 1433.387035614327488, 201.0472282066888283 ) ) ;
#42504 = CARTESIAN_POINT ( 'NONE',  ( -2.885329902869700369, 1508.551704408389924, 214.0785756058540130 ) ) ;
#42505 = CARTESIAN_POINT ( 'NONE',  ( -8.835575458280001016, 1388.613171834459990, 217.0371058496990031 ) ) ;
#42506 = CARTESIAN_POINT ( 'NONE',  ( 7.943378312860001067, 1421.399538177179920, 195.9193817166990073 ) ) ;
#42507 = CARTESIAN_POINT ( 'NONE',  ( -3.008413779357860030, 1433.155062154890174, 218.1878497074879988 ) ) ;
#42508 = CARTESIAN_POINT ( 'NONE',  ( -3.856935219870000431, 1496.767660296590066, 198.5573707464990036 ) ) ;
#42509 = CARTESIAN_POINT ( 'NONE',  ( 0.7136616831755410173, 1408.937982002440094, 186.5967116053269876 ) ) ;
#42511 = CARTESIAN_POINT ( 'NONE',  ( 4.019837106079773292, 1515.589591810383126, 209.7430514019713428 ) ) ;
#42510 = CARTESIAN_POINT ( 'NONE',  ( 1.363624045170000132, 1415.765549035329968, 232.8698710209980050 ) ) ;
#42512 = CIRCLE ( 'NONE', #35403, 2.000000000000000444 ) ;
#42513 = DIRECTION ( 'NONE',  ( -0.1070030146457423004, 0.000000000000000000, -0.9942586961433744763 ) ) ;
#42514 = CARTESIAN_POINT ( 'NONE',  ( -12.00629556859999880, 1378.345379175390008, 212.2149338467490054 ) ) ;
#42515 = CARTESIAN_POINT ( 'NONE',  ( 2.599446155150029636, 1525.231909165033585, 241.5259142133259047 ) ) ;
#42516 = VERTEX_POINT ( 'NONE', #93256 ) ;
#42517 = CARTESIAN_POINT ( 'NONE',  ( 12.78749341904959991, 1416.842625005220043, 222.1385636096939891 ) ) ;
#42518 = B_SPLINE_SURFACE_WITH_KNOTS ( 'NONE', 5, 5, ( 
 ( #106573, #3595, #37719, #28770, #62971, #88687 ),
 ( #46695, #80825, #21435, #44476, #4668, #57842 ),
 ( #100900, #109342, #66799, #56169, #81908, #57305 ),
 ( #48896, #99804, #108772, #91431, #99249, #83023 ),
 ( #55646, #32066, #89767, #100374, #40462, #5213 ),
 ( #98717, #30409, #64598, #47774, #39367, #74637 ),
 ( #66256, #6315, #38806, #21977, #47226, #108218 ),
 ( #72981, #5778, #32624, #90307, #75191, #31506 ),
 ( #49436, #91969, #30961, #41012, #14707, #13587 ),
 ( #23659, #15244, #73541, #83558, #82478, #6851 ),
 ( #13038, #90865, #81352, #107676, #107119, #65686 ),
 ( #65136, #39920, #22527, #56728, #14153, #48339 ),
 ( #74089, #23099, #33703, #69562, #85769, #35373 ),
 ( #688, #103109, #93064, #24735, #52195, #8502 ),
 ( #60046, #94724, #75735, #102551, #18002, #76277 ),
 ( #102006, #9068, #110425, #43237, #26410, #77385 ),
 ( #58383, #67898, #24197, #33159, #94164, #50536 ),
 ( #1236, #84115, #86324, #51632, #34818, #16881 ),
 ( #85211, #25290, #42127, #59492, #69005, #9608 ),
 ( #60602, #93602, #92509, #77929, #15776, #58932 ),
 ( #25844, #16337, #49978, #42674, #51085, #76831 ),
 ( #17434, #67348, #7414, #43779, #41580, #109879 ),
 ( #84661, #145, #101445, #7960, #34266, #68448 ),
 ( #11829, #37022, #80130, #20213, #52742, #70123 ) ),
 .UNSPECIFIED., .F., .F., .F.,
 ( 6, 3, 3, 3, 3, 3, 3, 6 ),
 ( 6, 6 ),
 ( 3.408434289659999727, 3.762248994509999722, 4.579389332449999905, 5.750344375240000083, 7.455049017759999508, 9.159753660279999821, 12.56916294530000044, 19.70543437909999795 ),
 ( 0.000000000000000000, 2.208859368739999773 ),
 .UNSPECIFIED. ) ;
#42519 = CARTESIAN_POINT ( 'NONE',  ( 11.85318847787639918, 1432.336023879089907, 150.2214167536129992 ) ) ;
#42520 = CARTESIAN_POINT ( 'NONE',  ( -10.83363501528680040, 1483.150651703840140, 204.1787077859559929 ) ) ;
#42521 = MECHANICAL_DESIGN_GEOMETRIC_PRESENTATION_REPRESENTATION (  '', ( #47889 ), #6787 ) ;
#42522 = EDGE_CURVE ( 'NONE', #71158, #82014, #103517, .T. ) ;
#42523 = CARTESIAN_POINT ( 'NONE',  ( -12.55964041559999878, 1391.412561036180023, 208.3681481067449965 ) ) ;
#42524 = EDGE_CURVE ( 'NONE', #83875, #96052, #34115, .T. ) ;
#42525 = CARTESIAN_POINT ( 'NONE',  ( 10.27889274641360018, 1427.972273100049961, 211.4948331838920126 ) ) ;
#42526 =( BOUNDED_CURVE ( )  B_SPLINE_CURVE ( 3, ( #81520, #73146, #41194, #8672 ),
 .UNSPECIFIED., .F., .T. ) 
 B_SPLINE_CURVE_WITH_KNOTS ( ( 4, 4 ),
 ( 2.628864438368395007, 3.267182934356360313 ),
 .UNSPECIFIED. ) 
 CURVE ( )  GEOMETRIC_REPRESENTATION_ITEM ( )  RATIONAL_B_SPLINE_CURVE ( ( 1.000000000000000000, 0.9663330366853500886, 0.9663330366853500886, 1.000000000000000000 ) ) 
 REPRESENTATION_ITEM ( '' )  );
#42527 = CARTESIAN_POINT ( 'NONE',  ( -34.26800564901520119, 1450.417484578289987, 136.2368926780540050 ) ) ;
#42528 = ADVANCED_FACE ( 'NONE', ( #75193 ), #81212, .T. ) ;
#42529 = CARTESIAN_POINT ( 'NONE',  ( -11.01785496395880060, 1462.531659345610024, 208.3487688801509989 ) ) ;
#42530 = CARTESIAN_POINT ( 'NONE',  ( -1.073363620209200085E-15, 1380.371560387289946, 209.1218459616989946 ) ) ;
#42531 = CARTESIAN_POINT ( 'NONE',  ( -9.128312996346709340, 1383.866482198609901, 218.5287380008880120 ) ) ;
#42532 = EDGE_CURVE ( 'NONE', #51877, #98379, #92132, .T. ) ;
#42533 = CARTESIAN_POINT ( 'NONE',  ( 11.65871887359999981, 1433.573214819259874, 151.0439516045979929 ) ) ;
#42534 = CARTESIAN_POINT ( 'NONE',  ( 25.65427092719999891, 1447.057116126670053, 243.9198229650980068 ) ) ;
#42536 = EDGE_CURVE ( 'NONE', #74589, #20620, #24656, .T. ) ;
#42535 = CARTESIAN_POINT ( 'NONE',  ( 12.16511160558169991, 1414.971513442450032, 197.5444944024079916 ) ) ;
#42537 = CARTESIAN_POINT ( 'NONE',  ( -30.37359097063415803, 1526.143142182216934, 201.3152257445480871 ) ) ;
#42538 = CARTESIAN_POINT ( 'NONE',  ( 11.39828671546239924, 1425.690482886019936, 199.4434797265739974 ) ) ;
#42539 = CARTESIAN_POINT ( 'NONE',  ( 8.858323751961959758, 1463.855706633549971, 215.0058157969349679 ) ) ;
#42540 = EDGE_CURVE ( 'NONE', #98568, #52837, #107622, .T. ) ;
#42541 = CARTESIAN_POINT ( 'NONE',  ( 22.12673984907599944, 1409.685743169220132, 208.3470065775269973 ) ) ;
#42542 = CARTESIAN_POINT ( 'NONE',  ( 33.13357216314884823, 1523.313115944345100, 217.3564597502656568 ) ) ;
#42543 = CARTESIAN_POINT ( 'NONE',  ( 2.641403850869999737, 1466.630502951829840, 234.1756239694980195 ) ) ;
#42544 = VECTOR ( 'NONE', #45231, 1000.000000000000000 ) ;
#42545 = CARTESIAN_POINT ( 'NONE',  ( 23.83044711719999853, 1430.353408614430009, 213.6317407082179898 ) ) ;
#42546 = CARTESIAN_POINT ( 'NONE',  ( 0.5707576997041963196, 1477.813279947535420, 198.7217904697586448 ) ) ;
#42547 = CARTESIAN_POINT ( 'NONE',  ( -8.878767216129999085, 1509.223113770430018, 236.7286233840980003 ) ) ;
#42548 = CARTESIAN_POINT ( 'NONE',  ( -1.471738374290000095, 1515.341568496189893, 204.8474131707589834 ) ) ;
#42549 = CARTESIAN_POINT ( 'NONE',  ( 16.37061378800000000, 1453.313060387329870, 220.2891823736979973 ) ) ;
#42550 = CARTESIAN_POINT ( 'NONE',  ( -22.19117980480319829, 1483.602007368270051, 216.8115291794120196 ) ) ;
#42551 = CARTESIAN_POINT ( 'NONE',  ( 0.01322035751810150123, 1516.939819969850078, 213.1588969678170145 ) ) ;
#42552 = EDGE_CURVE ( 'NONE', #37540, #64955, #92627, .T. ) ;
#42553 = CARTESIAN_POINT ( 'NONE',  ( -20.54173704900959763, 1418.376418166659960, 208.6868407705159996 ) ) ;
#42554 = CARTESIAN_POINT ( 'NONE',  ( 0.1826399099826500061, 1472.956896255519951, 182.3968825522989903 ) ) ;
#42556 = VERTEX_POINT ( 'NONE', #102174 ) ;
#42555 = DIRECTION ( 'NONE',  ( 5.980589973904019347E-17, -1.000000000000000000, 1.736889445713099699E-16 ) ) ;
#42557 = CARTESIAN_POINT ( 'NONE',  ( -18.57285056714472304, 1444.740067931808881, 161.9794701184628991 ) ) ;
#42558 = CARTESIAN_POINT ( 'NONE',  ( -5.839375756963000264, 1441.004146652379859, 154.6877192777659786 ) ) ;
#42559 = CARTESIAN_POINT ( 'NONE',  ( -2.596261494520225366, 1525.907212628473644, 177.4701144822246874 ) ) ;
#42560 = CARTESIAN_POINT ( 'NONE',  ( -41.42406817617050052, 1441.754257788219775, 134.0999999980809889 ) ) ;
#42561 = CARTESIAN_POINT ( 'NONE',  ( -109.1645122539999875, 1384.901545528990027, 297.1326340414590277 ) ) ;
#42562 = ORIENTED_EDGE ( 'NONE', *, *, #33330, .T. ) ;
#42564 = EDGE_CURVE ( 'NONE', #86539, #30027, #90876, .T. ) ;
#42563 = CARTESIAN_POINT ( 'NONE',  ( -10.55952073400000124, 1471.180150010990019, 209.5617685337520015 ) ) ;
#42565 = CARTESIAN_POINT ( 'NONE',  ( 9.959589143500000574, 1478.327753353190019, 203.6760996314889951 ) ) ;
#42566 = CARTESIAN_POINT ( 'NONE',  ( -15.86930209750000031, 1414.913060387329779, 211.6478204561080076 ) ) ;
#42567 = CARTESIAN_POINT ( 'NONE',  ( 2.979994341136180225, 1507.572973720820073, 217.5187881045870029 ) ) ;
#42568 = EDGE_CURVE ( 'NONE', #37624, #37252, #16744, .T. ) ;
#42569 = CARTESIAN_POINT ( 'NONE',  ( -9.158906349748429321, 1437.718415169640139, 211.6837391772429839 ) ) ;
#42570 = VECTOR ( 'NONE', #49084, 1000.000000000000000 ) ;
#42571 = CARTESIAN_POINT ( 'NONE',  ( -109.0688921503400763, 1382.192801452487629, 310.8631491596341903 ) ) ;
#42572 = CARTESIAN_POINT ( 'NONE',  ( 22.95908931529999819, 1507.624001450029937, 210.4418640519579924 ) ) ;
#42573 = CARTESIAN_POINT ( 'NONE',  ( 0.000000000000000000, 1523.382868172864164, 209.1218459616979999 ) ) ;
#42574 = CARTESIAN_POINT ( 'NONE',  ( -11.07525038950000074, 1391.808614258399984, 204.6545583908090009 ) ) ;
#42575 = CARTESIAN_POINT ( 'NONE',  ( -68.65572861644470493, 1385.105512080379867, 263.0716478229380186 ) ) ;
#42576 = CARTESIAN_POINT ( 'NONE',  ( -10.24890398481989884, 1391.913060387289988, 214.0452963765859806 ) ) ;
#42577 = CARTESIAN_POINT ( 'NONE',  ( 11.09274063877570171, 1422.410694574019999, 207.6743043836530092 ) ) ;
#42578 = VERTEX_POINT ( 'NONE', #40075 ) ;
#42579 = EDGE_CURVE ( 'NONE', #49402, #48060, #110038, .T. ) ;
#42580 = CARTESIAN_POINT ( 'NONE',  ( -30.95328360879999963, 1451.678783263429978, 135.6739097202980133 ) ) ;
#42581 = CARTESIAN_POINT ( 'NONE',  ( 12.53676446056794624, 1442.773887286370382, 169.5333422587208645 ) ) ;
#42583 = EDGE_LOOP ( 'NONE', ( #62191, #26721, #1042, #10531 ) ) ;
#42582 = CARTESIAN_POINT ( 'NONE',  ( 10.11781796957937551, 1428.435797280887527, 137.0999999980966777 ) ) ;
#42584 = CARTESIAN_POINT ( 'NONE',  ( 1.859895485220000033, 1474.627878747789964, 219.9708147289989881 ) ) ;
#42585 = CARTESIAN_POINT ( 'NONE',  ( 1.842962231260000028, 1515.551704408389924, 205.2922258481490303 ) ) ;
#42586 = CARTESIAN_POINT ( 'NONE',  ( -7.107332553001914910, 1363.850055010189408, 208.3718459617061285 ) ) ;
#42587 = CARTESIAN_POINT ( 'NONE',  ( -9.320710346250001166, 1493.328639440889901, 201.5612320172390071 ) ) ;
#42588 = CARTESIAN_POINT ( 'NONE',  ( 41.02245392713034988, 1447.677742136113920, 269.6289972548281071 ) ) ;
#42589 = CARTESIAN_POINT ( 'NONE',  ( 14.35695837613839032, 1409.414416421430587, 192.9647261027294007 ) ) ;
#42590 = CARTESIAN_POINT ( 'NONE',  ( 5.343479918049999888, 1396.099658817830004, 218.7752541424879951 ) ) ;
#42591 = CARTESIAN_POINT ( 'NONE',  ( -1776.370103581280091, 5181.793945261120825, 9288.252068156898531 ) ) ;
#42592 = CARTESIAN_POINT ( 'NONE',  ( 5.845238504180000128, 1446.767628288889910, 202.1062060431090117 ) ) ;
#42593 = CARTESIAN_POINT ( 'NONE',  ( -9.317611367242571774, 1367.919873931656866, 207.6218459616987673 ) ) ;
#42594 = VECTOR ( 'NONE', #74926, 1000.000000000000114 ) ;
#42595 = CARTESIAN_POINT ( 'NONE',  ( -29.67167576299870646, 1526.344110814219675, 216.9865736510277827 ) ) ;
#42596 = CARTESIAN_POINT ( 'NONE',  ( -7.725372170364999569, 1517.158319634930194, 206.2490093095770192 ) ) ;
#42597 = CIRCLE ( 'NONE', #13966, 1.000000000000000888 ) ;
#42598 = CARTESIAN_POINT ( 'NONE',  ( 2.499999987519999856, 1448.405371708940038, 154.5226066912979945 ) ) ;
#42599 = CARTESIAN_POINT ( 'NONE',  ( -2.500000000000000000, 1436.625622233000058, 157.6304333937980005 ) ) ;
#42600 = CARTESIAN_POINT ( 'NONE',  ( -0.9164389294989989665, 1497.287211993289930, 197.7316609878989766 ) ) ;
#42603 = ORIENTED_EDGE ( 'NONE', *, *, #92897, .T. ) ;
#42602 = CARTESIAN_POINT ( 'NONE',  ( 1.265340693600000233, 1494.980160179489758, 220.3616726747989958 ) ) ;
#42601 = CONICAL_SURFACE ( 'NONE', #87293, 21.50000000000000355, 0.3430239404209998177 ) ;
#42604 = EDGE_CURVE ( 'NONE', #60628, #22154, #12218, .T. ) ;
#42605 = CARTESIAN_POINT ( 'NONE',  ( 31.92108011125344191, 1511.187213306747708, 197.2845127572061301 ) ) ;
#42606 = ORIENTED_EDGE ( 'NONE', *, *, #11363, .F. ) ;
#42607 = VECTOR ( 'NONE', #19656, 1000.000000000000000 ) ;
#42608 = DIRECTION ( 'NONE',  ( 0.000000000000000000, -0.02617694830808806397, -0.9996573249755517088 ) ) ;
#42609 = CARTESIAN_POINT ( 'NONE',  ( -23.00452549200000263, 1430.350017918430012, 202.3573688689379821 ) ) ;
#42611 = CARTESIAN_POINT ( 'NONE',  ( 16.62869176917200065, 1409.868729623830177, 192.2451677454709795 ) ) ;
#42610 = CARTESIAN_POINT ( 'NONE',  ( -10.81738549768889968, 1425.668387765759917, 102.3030755685860100 ) ) ;
#42612 = CARTESIAN_POINT ( 'NONE',  ( 2.494020282435000180, 1516.876240617270014, 211.4047611534970201 ) ) ;
#42613 = CARTESIAN_POINT ( 'NONE',  ( 29.04764039190411395, 1510.038300840001739, 201.6228361755694323 ) ) ;
#42614 = TOROIDAL_SURFACE ( 'NONE', #46244, 2.000000000000000000, 1.000000000000000000 ) ;
#42615 = CARTESIAN_POINT ( 'NONE',  ( 1.539252401269999959, 1434.992946304420002, 189.4158960071980005 ) ) ;
#42616 = CARTESIAN_POINT ( 'NONE',  ( -12.65810595541850070, 1379.039847990219869, 208.8385753629780197 ) ) ;
#42617 = CARTESIAN_POINT ( 'NONE',  ( 12.70147564075329960, 1500.571916961849865, 209.2764580048830112 ) ) ;
#42618 = PRODUCT_CONTEXT ( 'NONE', #5534, 'mechanical' ) ;
#42619 = CARTESIAN_POINT ( 'NONE',  ( -5.146359508130000648, 1391.913486340589998, 214.6520581086589914 ) ) ;
#42620 = CARTESIAN_POINT ( 'NONE',  ( -15.97230738210199696, 1420.722887419069821, 227.0315163971459924 ) ) ;
#42621 = VERTEX_POINT ( 'NONE', #110585 ) ;
#42622 = CARTESIAN_POINT ( 'NONE',  ( 10.02107572612820086, 1396.322385283019912, 216.0185856081670011 ) ) ;
#42623 = CARTESIAN_POINT ( 'NONE',  ( 9.387379239281479215, 1461.645186388049979, 206.6211749101620114 ) ) ;
#42624 = CARTESIAN_POINT ( 'NONE',  ( -16.38659414299999639, 1458.929922077130186, 229.9995173766979804 ) ) ;
#42625 = EDGE_LOOP ( 'NONE', ( #61141, #100371, #47158, #45235, #83306, #87785 ) ) ;
#42626 = ORIENTED_EDGE ( 'NONE', *, *, #61044, .T. ) ;
#42627 = CARTESIAN_POINT ( 'NONE',  ( -3.076366055149999834, 1424.853903601579987, 191.3970713258989917 ) ) ;
#42628 = CARTESIAN_POINT ( 'NONE',  ( 8.770757543469729952E-15, 1422.771842310740112, 151.0941926623779921 ) ) ;
#42629 = EDGE_CURVE ( 'NONE', #12135, #35462, #74255, .T. ) ;
#42630 = DIRECTION ( 'NONE',  ( 0.9900962604114871279, -0.1403901532130690244, 1.186453863995930381E-14 ) ) ;
#42631 = CIRCLE ( 'NONE', #33657, 10.31100486199999722 ) ;
#42632 = CARTESIAN_POINT ( 'NONE',  ( -15.30723763684610006, 1508.551704406429963, 210.0839430030410142 ) ) ;
#42633 = CARTESIAN_POINT ( 'NONE',  ( 4.175275161990000150, 1515.456650324490056, 210.6054913326990174 ) ) ;
#42634 = CARTESIAN_POINT ( 'NONE',  ( 12.20923102414920436, 1507.046626258653760, 228.0865972342955956 ) ) ;
#42635 = CARTESIAN_POINT ( 'NONE',  ( 12.40160258794860049, 1420.584110727309962, 200.5244627772079866 ) ) ;
#42636 = CARTESIAN_POINT ( 'NONE',  ( 0.4151546846821903003, 1512.187213306747481, 244.9330574173806951 ) ) ;
#42637 = CARTESIAN_POINT ( 'NONE',  ( 9.176106830921559876, 1450.535193219119947, 208.1385774281999943 ) ) ;
#42638 = CARTESIAN_POINT ( 'NONE',  ( 33.98103710425687041, 1443.501467202839649, 154.9319925572100942 ) ) ;
#42639 = CARTESIAN_POINT ( 'NONE',  ( -99.29130229444270128, 1384.871901381209909, 296.1281569486179706 ) ) ;
#42640 = VERTEX_POINT ( 'NONE', #33871 ) ;
#42641 = CARTESIAN_POINT ( 'NONE',  ( 7.714371502985000184, 1516.738222552470233, 203.3422428319769892 ) ) ;
#42642 = CARTESIAN_POINT ( 'NONE',  ( -1.122033430074999893, 1516.972341476009888, 209.8777854684929878 ) ) ;
#42643 = VERTEX_POINT ( 'NONE', #17036 ) ;
#42644 = CARTESIAN_POINT ( 'NONE',  ( 11.76080740273470049, 1426.908826233330046, 145.8170930824429945 ) ) ;
#42645 = ADVANCED_FACE ( 'NONE', ( #100527 ), #47261, .F. ) ;
#42646 = CARTESIAN_POINT ( 'NONE',  ( 20.33516419129999875, 1507.859939371830023, 228.7622698018979861 ) ) ;
#42647 = VERTEX_POINT ( 'NONE', #69159 ) ;
#42648 = CARTESIAN_POINT ( 'NONE',  ( -14.00875078090000159, 1416.819756528429934, 221.8514975898980026 ) ) ;
#42649 = CARTESIAN_POINT ( 'NONE',  ( -17.11778670694504711, 1443.086052842848176, 162.7557629363845990 ) ) ;
#42650 = CARTESIAN_POINT ( 'NONE',  ( 22.07680858347410435, 1523.847233649538339, 233.7985801730517323 ) ) ;
#42651 = CARTESIAN_POINT ( 'NONE',  ( -10.15064982388159898, 1462.077207233110130, 208.4365470241570222 ) ) ;
#42652 = CARTESIAN_POINT ( 'NONE',  ( -4.983945999730000409, 1425.062923145830155, 186.2539488382980153 ) ) ;
#42653 = EDGE_CURVE ( 'NONE', #100587, #47989, #87479, .T. ) ;
#42654 = CARTESIAN_POINT ( 'NONE',  ( -5.465287381910192366, 1446.862131887090982, 154.6411839201834937 ) ) ;
#42655 = CARTESIAN_POINT ( 'NONE',  ( -9.950505953960002259, 1472.615817291290114, 206.1541412670590034 ) ) ;
#42656 = CARTESIAN_POINT ( 'NONE',  ( 6.128601823160000350, 1493.316819573389921, 218.4060617982489987 ) ) ;
#42657 = CARTESIAN_POINT ( 'NONE',  ( -51.90601367590000592, 1379.692123994150279, 243.6554138731589774 ) ) ;
#42658 = CARTESIAN_POINT ( 'NONE',  ( -16.83556428340000011, 1507.627023023630045, 224.6625388484980022 ) ) ;
#42660 = CARTESIAN_POINT ( 'NONE',  ( 3.844278957675350217, 1466.491520180780071, 198.7404678004429854 ) ) ;
#42659 = CARTESIAN_POINT ( 'NONE',  ( -6.252266492314999979, 1511.741868877540128, 200.3335294429169835 ) ) ;
#42661 = CARTESIAN_POINT ( 'NONE',  ( -4.688107345455859054, 1423.663410245182149, 184.4846934393623599 ) ) ;
#42662 = CARTESIAN_POINT ( 'NONE',  ( 0.1562295902064984587, 1410.302064435142938, 185.0131410921949850 ) ) ;
#42663 = ORIENTED_EDGE ( 'NONE', *, *, #81097, .T. ) ;
#42664 = CARTESIAN_POINT ( 'NONE',  ( 18.03753337733320095, 1424.489286807229973, 224.3984010197989960 ) ) ;
#42665 = CARTESIAN_POINT ( 'NONE',  ( -21.28823305372391772, 1525.253996226948175, 234.3566951577463158 ) ) ;
#42666 = EDGE_CURVE ( 'NONE', #12743, #103816, #74207, .T. ) ;
#42667 = CARTESIAN_POINT ( 'NONE',  ( -2.928324112734959517, 1485.053537356824791, 183.1171725139605542 ) ) ;
#42668 = CARTESIAN_POINT ( 'NONE',  ( -9.176206605676330024E-06, 1406.768156800490033, 269.6447221830679837 ) ) ;
#42670 = VERTEX_POINT ( 'NONE', #2521 ) ;
#42669 = CARTESIAN_POINT ( 'NONE',  ( -1.842963219480119985, 1515.064792700640055, 204.7923971808919816 ) ) ;
#42671 = CARTESIAN_POINT ( 'NONE',  ( 0.5862352712159999424, 1471.323284329630042, 188.0726871234980138 ) ) ;
#42672 = DIRECTION ( 'NONE',  ( -0.6736849260863841948, 0.000000000000000000, 0.7390186874254148774 ) ) ;
#42673 = EDGE_CURVE ( 'NONE', #69390, #73043, #28775, .T. ) ;
#42674 = CARTESIAN_POINT ( 'NONE',  ( -11.47389391070000109, 1425.951597195029990, 147.0448823332980055 ) ) ;
#42675 = CARTESIAN_POINT ( 'NONE',  ( 19.79299573329999617, 1474.475016451189958, 213.0583662838989767 ) ) ;
#42676 = CARTESIAN_POINT ( 'NONE',  ( 29.31378126858938060, 1450.601291961854031, 136.3806914572924143 ) ) ;
#42677 = DIRECTION ( 'NONE',  ( -0.9455185755993178454, 0.000000000000000000, 0.3255681544571539243 ) ) ;
#42678 = DIRECTION ( 'NONE',  ( 5.980589973904019347E-17, -1.000000000000000000, 1.736889445713099699E-16 ) ) ;
#42679 = DIRECTION ( 'NONE',  ( -1.000000000000000000, 0.000000000000000000, 0.000000000000000000 ) ) ;
#42680 = EDGE_CURVE ( 'NONE', #18354, #5861, #78334, .T. ) ;
#42682 = CARTESIAN_POINT ( 'NONE',  ( -11.74755037768770016, 1482.417789575780262, 207.1586782760400069 ) ) ;
#42681 = CARTESIAN_POINT ( 'NONE',  ( -20.75531091540000261, 1495.371774238330090, 227.1192881343980048 ) ) ;
#42683 = CARTESIAN_POINT ( 'NONE',  ( 6.826200034800000260, 1424.874072630889941, 213.4902541782590220 ) ) ;
#42684 = B_SPLINE_CURVE_WITH_KNOTS ( 'NONE', 5,
 ( #1006, #36243, #70431, #27845, #62026, #9385 ),
 .UNSPECIFIED., .F., .F.,
 ( 6, 6 ),
 ( 0.000000000000000000, 1.000000000000000000 ),
 .UNSPECIFIED. ) ;
#42685 = ORIENTED_EDGE ( 'NONE', *, *, #31314, .T. ) ;
#42687 = MECHANICAL_DESIGN_GEOMETRIC_PRESENTATION_REPRESENTATION (  '', ( #74907 ), #53492 ) ;
#42686 = CARTESIAN_POINT ( 'NONE',  ( -1.716392779905000054, 1516.788317650260069, 206.2580580763669786 ) ) ;
#42688 = CARTESIAN_POINT ( 'NONE',  ( 30.23511527080000150, 1414.232503506630110, 267.4627318704980325 ) ) ;
#42689 = CARTESIAN_POINT ( 'NONE',  ( 24.92728913490000053, 1436.178271453029993, 137.8894200858980241 ) ) ;
#42690 = AXIS2_PLACEMENT_3D ( 'NONE', #66052, #15586, #40818 ) ;
#42691 = CARTESIAN_POINT ( 'NONE',  ( 20.31340460420000227, 1449.728792434289971, 194.1812982889979935 ) ) ;
#42692 = ADVANCED_FACE ( 'NONE', ( #36644 ), #30256, .F. ) ;
#42693 = ADVANCED_FACE ( 'NONE', ( #109369 ), #32647, .F. ) ;
#42694 = AXIS2_PLACEMENT_3D ( 'NONE', #78758, #36204, #69833 ) ;
#42695 = CARTESIAN_POINT ( 'NONE',  ( 20.22029059781747407, 1426.889228552814757, 220.9842331285456964 ) ) ;
#42696 = CARTESIAN_POINT ( 'NONE',  ( -9.484515027067567772, 1389.595169172901706, 217.0780171008755701 ) ) ;
#42697 = CARTESIAN_POINT ( 'NONE',  ( -0.5042624802195529998, 1509.595895645290057, 205.5688950569590077 ) ) ;
#42698 = CARTESIAN_POINT ( 'NONE',  ( 15.95383384960000228, 1506.798305107329952, 193.5571554442980187 ) ) ;
#42699 = CARTESIAN_POINT ( 'NONE',  ( -15.34446697350000122, 1417.328256708470008, 204.9827898744490255 ) ) ;
#42700 = CARTESIAN_POINT ( 'NONE',  ( -13.51374722289999930, 1445.514830763570217, 188.1418749665980101 ) ) ;
#42701 = CARTESIAN_POINT ( 'NONE',  ( -3.362747762569299859, 1485.356940126880090, 197.7060954189079780 ) ) ;
#42702 = CARTESIAN_POINT ( 'NONE',  ( -16.04213126322901672, 1419.787388156080397, 210.3004129104147637 ) ) ;
#42703 = CARTESIAN_POINT ( 'NONE',  ( 10.97762738470000166, 1408.611869070129842, 270.1116084948980074 ) ) ;
#42704 = EDGE_LOOP ( 'NONE', ( #45839, #29010, #28907, #18380 ) ) ;
#42705 = CARTESIAN_POINT ( 'NONE',  ( 1.453362474727719844, 1502.444710984339963, 181.3169649662810059 ) ) ;
#42706 = CARTESIAN_POINT ( 'NONE',  ( -14.48215298470269907, 1409.418788313440018, 205.4675657464059952 ) ) ;
#42707 = ADVANCED_FACE ( 'NONE', ( #66824 ), #109905, .T. ) ;
#42708 = CARTESIAN_POINT ( 'NONE',  ( -11.54256419585919957, 1508.172464970640021, 207.9362749538369997 ) ) ;
#42709 = CARTESIAN_POINT ( 'NONE',  ( 21.83550407203919974, 1523.678648413191695, 234.9693198511250785 ) ) ;
#42710 = CARTESIAN_POINT ( 'NONE',  ( -9.929189165030001263, 1475.283055377529990, 268.4433786484979692 ) ) ;
#42712 = CIRCLE ( 'NONE', #105291, 26.50000000000001421 ) ;
#42711 = CARTESIAN_POINT ( 'NONE',  ( 30.12521068615187048, 1524.538969332612623, 195.8585657628962906 ) ) ;
#42713 = CARTESIAN_POINT ( 'NONE',  ( -11.19935784055662786, 1391.089543242234640, 214.3845051435474716 ) ) ;
#42714 = ADVANCED_FACE ( 'NONE', ( #24761 ), #13263, .T. ) ;
#42715 = CARTESIAN_POINT ( 'NONE',  ( -24.38621446027962847, 1444.659099962498203, 211.1570028031310073 ) ) ;
#42716 = CARTESIAN_POINT ( 'NONE',  ( -79.56500322749430154, 1384.639486651150037, 303.5682780263990139 ) ) ;
#42717 = CARTESIAN_POINT ( 'NONE',  ( -24.20882859423510070, 1435.739118765830199, 210.8967395777180229 ) ) ;
#42718 = CARTESIAN_POINT ( 'NONE',  ( -11.94206337009999963, 1438.199233188169956, 150.9847479746979957 ) ) ;
#42719 = DIRECTION ( 'NONE',  ( 0.000000000000000000, -1.000000000000000000, 0.000000000000000000 ) ) ;
#42720 = CARTESIAN_POINT ( 'NONE',  ( 9.549000552458089430, 1470.075890067440014, 212.3436661921319910 ) ) ;
#42721 = CARTESIAN_POINT ( 'NONE',  ( -2.360319324342201153, 1507.471933479789868, 221.3436898553985941 ) ) ;
#42722 = CARTESIAN_POINT ( 'NONE',  ( -23.19328137029999937, 1410.218139083129927, 206.0158621637780243 ) ) ;
#42723 = DIRECTION ( 'NONE',  ( 0.6709778558543766369, 0.000000000000000000, 0.7414773880254632576 ) ) ;
#42724 = CARTESIAN_POINT ( 'NONE',  ( 3.323702338719999982, 1484.956220939089917, 220.0842284974989695 ) ) ;
#42725 = CARTESIAN_POINT ( 'NONE',  ( -29.99620953741480278, 1526.382868172863937, 219.7462484079463252 ) ) ;
#42726 = CARTESIAN_POINT ( 'NONE',  ( 2.446787376320000096, 1432.353341358199941, 150.2884730787980061 ) ) ;
#42727 = CARTESIAN_POINT ( 'NONE',  ( -19.86559622680790227, 1442.607244639209966, 212.9307904419119950 ) ) ;
#42728 = CARTESIAN_POINT ( 'NONE',  ( 16.58908872130572121, 1524.412455883367329, 180.6440485805556193 ) ) ;
#42729 = CARTESIAN_POINT ( 'NONE',  ( -3.549608351769999892, 1507.276797637930031, 180.9704965309979912 ) ) ;
#42731 = CARTESIAN_POINT ( 'NONE',  ( -9.459903729319998789, 1382.054661141809902, 200.9046470295689915 ) ) ;
#42730 = CARTESIAN_POINT ( 'NONE',  ( 14.11150867580459511, 1517.034034075909631, 192.1634499395738942 ) ) ;
#42732 = CARTESIAN_POINT ( 'NONE',  ( 11.69897705284829925, 1426.720814411340143, 141.4468014655840022 ) ) ;
#42733 = CARTESIAN_POINT ( 'NONE',  ( -0.9985785836218079581, 1368.656171449427575, 210.4211784751752248 ) ) ;
#42734 = CARTESIAN_POINT ( 'NONE',  ( -7.500000019064999357, 1516.934643012909874, 209.1218459511669892 ) ) ;
#42735 = CARTESIAN_POINT ( 'NONE',  ( 9.027641301329820678, 1449.985334637959795, 203.9681922101850091 ) ) ;
#42736 = CARTESIAN_POINT ( 'NONE',  ( -16.71438865490179992, 1507.439213204299904, 224.6678772092570000 ) ) ;
#42737 = CARTESIAN_POINT ( 'NONE',  ( 7.326795523374999952, 1516.760434454289907, 203.3416138547669902 ) ) ;
#42738 = CARTESIAN_POINT ( 'NONE',  ( -4.376213210466648462, 1398.043588354321628, 221.3632903160299463 ) ) ;
#42739 = CARTESIAN_POINT ( 'NONE',  ( 0.000000000000000000, 1405.413060387330006, 209.1218459616979999 ) ) ;
#42740 = PLANE ( 'NONE',  #33995 ) ;
#42741 = CARTESIAN_POINT ( 'NONE',  ( -17.60568779080000112, 1410.876629449830034, 194.3219271762980043 ) ) ;
#42742 = AXIS2_PLACEMENT_3D ( 'NONE', #22333, #31863, #83363 ) ;
#42744 = ORIENTED_EDGE ( 'NONE', *, *, #55075, .T. ) ;
#42743 = CARTESIAN_POINT ( 'NONE',  ( -54.44063311709999908, 1379.743533640540136, 254.0790799858589821 ) ) ;
#42745 = ORIENTED_EDGE ( 'NONE', *, *, #35885, .F. ) ;
#42746 = CARTESIAN_POINT ( 'NONE',  ( 11.94927061825729986, 1433.750257499170175, 150.4505018609179956 ) ) ;
#42747 = CARTESIAN_POINT ( 'NONE',  ( 21.78049460968683348, 1524.843416604514687, 184.6507917665084335 ) ) ;
#42748 = VERTEX_POINT ( 'NONE', #33732 ) ;
#42749 = CARTESIAN_POINT ( 'NONE',  ( -107.2899035190000063, 1379.886884136000162, 309.1794862632590366 ) ) ;
#42750 = CARTESIAN_POINT ( 'NONE',  ( -10.22594067180810029, 1448.813191590999850, 207.3202860899079951 ) ) ;
#42751 = DIRECTION ( 'NONE',  ( -0.1041548977914050628, 0.000000000000000000, 0.9945610877497982338 ) ) ;
#42753 = CARTESIAN_POINT ( 'NONE',  ( -0.1613635983459999756, 1507.107001919430104, 180.9028748717980193 ) ) ;
#42752 = DIRECTION ( 'NONE',  ( 0.9455185755993178454, 0.000000000000000000, -0.3255681544571537578 ) ) ;
#42754 = CARTESIAN_POINT ( 'NONE',  ( 15.90103281899999921, 1507.811112176129882, 231.7872566220979991 ) ) ;
#42755 = B_SPLINE_CURVE_WITH_KNOTS ( 'NONE', 3,
 ( #63831, #39708, #97943, #55420, #65483, #6099, #40254, #23446, #88998, #39137 ),
 .UNSPECIFIED., .F., .F.,
 ( 4, 3, 3, 4 ),
 ( -157.4421957120000002, -134.5125376663179964, -78.90079083566818952, -29.52656374254129901 ),
 .UNSPECIFIED. ) ;
#42756 = TOROIDAL_SURFACE ( 'NONE', #64271, 2.000000000000000000, 1.000000000000000000 ) ;
#42757 = CARTESIAN_POINT ( 'NONE',  ( 4.322182879569999692, 1488.170148571130085, 182.6105505137979890 ) ) ;
#42758 = CARTESIAN_POINT ( 'NONE',  ( -0.3621993314249999929, 1416.825784011830137, 191.0664210096979900 ) ) ;
#42759 = CARTESIAN_POINT ( 'NONE',  ( -24.61293950550089704, 1444.770188684140066, 210.8869336946189890 ) ) ;
#42760 = B_SPLINE_SURFACE_WITH_KNOTS ( 'NONE', 5, 5, ( 
 ( #40692, #72656, #39021, #22207, #63720, #97831 ),
 ( #47997, #106784, #12737, #21109, #55311, #67569 ),
 ( #25521, #8727, #84344, #23867, #76497, #58062 ),
 ( #102243, #75419, #83796, #49663, #84879, #50218 ),
 ( #109557, #24423, #41789, #7090, #93825, #41247 ),
 ( #32828, #59712, #75948, #109009, #110099, #67020 ) ),
 .UNSPECIFIED., .F., .F., .F.,
 ( 6, 6 ),
 ( 6, 6 ),
 ( 19.14974397187629762, 84.90069406665540441 ),
 ( -1.908382372295470058E-05, 2.000000000000000000 ),
 .UNSPECIFIED. ) ;
#42761 = CARTESIAN_POINT ( 'NONE',  ( 11.76014171143800091, 1479.338753478690023, 208.6264959333659874 ) ) ;
#42762 = CARTESIAN_POINT ( 'NONE',  ( 1.600048698852036821, 1401.254281879943164, 134.0999999980979851 ) ) ;
#42763 = CARTESIAN_POINT ( 'NONE',  ( 11.85851232169999925, 1431.806521938459809, 149.9579072722980015 ) ) ;
#42764 = CARTESIAN_POINT ( 'NONE',  ( 8.308248917014999790, 1512.693483295309989, 202.0206284635169993 ) ) ;
#42765 = ORIENTED_EDGE ( 'NONE', *, *, #45962, .F. ) ;
#42766 = CARTESIAN_POINT ( 'NONE',  ( 14.11666836576459971, 1435.826325603770101, 149.9982859278159992 ) ) ;
#42767 = ORIENTED_EDGE ( 'NONE', *, *, #51511, .F. ) ;
#42768 = ORIENTED_EDGE ( 'NONE', *, *, #76478, .T. ) ;
#42769 = CARTESIAN_POINT ( 'NONE',  ( 13.17549261770877678, 1444.733027075352084, 169.3947134178655460 ) ) ;
#42770 = CARTESIAN_POINT ( 'NONE',  ( -4.035063157659999789, 1465.902341356430043, 234.8124638711979912 ) ) ;
#42771 = CARTESIAN_POINT ( 'NONE',  ( -32.02808312589930040, 1512.187213306747481, 198.2787714533499752 ) ) ;
#42772 = FACE_OUTER_BOUND ( 'NONE', #83203, .T. ) ;
#42773 = CARTESIAN_POINT ( 'NONE',  ( -19.27355791249999939, 1467.813399981289876, 204.3088842694490097 ) ) ;
#42774 = VECTOR ( 'NONE', #25150, 1000.000000000000000 ) ;
#42775 = CARTESIAN_POINT ( 'NONE',  ( -18.89211047122036646, 1444.064104411348126, 212.4334844116814338 ) ) ;
#42776 = CARTESIAN_POINT ( 'NONE',  ( -47.10178971561379768, 1379.678077506135423, 234.1671279625103637 ) ) ;
#42777 = CYLINDRICAL_SURFACE ( 'NONE', #40327, 0.4999999999999449329 ) ;
#42778 = CIRCLE ( 'NONE', #44620, 1.999999999999999556 ) ;
#42779 = ORIENTED_EDGE ( 'NONE', *, *, #70417, .T. ) ;
#42780 = CARTESIAN_POINT ( 'NONE',  ( 1.118353215965000036, 1516.977201124959947, 206.6281488911770055 ) ) ;
#42781 = ORIENTED_EDGE ( 'NONE', *, *, #72916, .F. ) ;
#42782 = CARTESIAN_POINT ( 'NONE',  ( -105.0405218166850005, 1379.391193415470070, 304.9871214168560414 ) ) ;
#42783 = EDGE_CURVE ( 'NONE', #76345, #90388, #67925, .T. ) ;
#42784 = CARTESIAN_POINT ( 'NONE',  ( -19.08918019649999920, 1507.695924774130162, 229.6553491538980154 ) ) ;
#42785 = ORIENTED_EDGE ( 'NONE', *, *, #62736, .F. ) ;
#42786 = CARTESIAN_POINT ( 'NONE',  ( -12.62875319149999953, 1409.354066166529719, 191.1165109835980047 ) ) ;
#42787 = CARTESIAN_POINT ( 'NONE',  ( 7.304088249714999925, 1513.265135866640094, 216.6543191384870113 ) ) ;
#42789 = ORIENTED_EDGE ( 'NONE', *, *, #67209, .F. ) ;
#42788 = CARTESIAN_POINT ( 'NONE',  ( 0.7166837575268250049, 1423.109731908320100, 192.5084507060149974 ) ) ;
#42790 = CARTESIAN_POINT ( 'NONE',  ( 18.27965585589999975, 1424.887530935629911, 223.6444487664979874 ) ) ;
#42791 = CARTESIAN_POINT ( 'NONE',  ( -15.44253390423740058, 1508.551704408389924, 210.3695883813369960 ) ) ;
#42792 = CARTESIAN_POINT ( 'NONE',  ( 8.337034337958536767, 1374.913060387289988, 213.6763885784389174 ) ) ;
#42793 = CARTESIAN_POINT ( 'NONE',  ( -34.68852446352951802, 1501.977400791986611, 199.9946320047955339 ) ) ;
#42794 = CARTESIAN_POINT ( 'NONE',  ( 3.968827103902559550, 1519.551704408389924, 188.7040005461919918 ) ) ;
#42795 = B_SPLINE_SURFACE_WITH_KNOTS ( 'NONE', 5, 5, ( 
 ( #44925, #29196, #26996, #28090, #80148, #105357 ),
 ( #62277, #105917, #61186, #96408, #95303, #46020 ),
 ( #104252, #18563, #63386, #45477, #3469, #19684 ),
 ( #62852, #78505, #20229, #52758, #79620, #86892 ),
 ( #2924, #10186, #28648, #27542, #61725, #95847 ),
 ( #19114, #53317, #59240, #83312, #92813, #31253 ) ),
 .UNSPECIFIED., .F., .F., .F.,
 ( 6, 6 ),
 ( 6, 6 ),
 ( -0.0003633979984830099813, 1.546630684984659831 ),
 ( 0.000000000000000000, 2.000363398052620312 ),
 .UNSPECIFIED. ) ;
#42796 = CARTESIAN_POINT ( 'NONE',  ( -7.713117841115000317, 1516.690345681169902, 214.1262880092169780 ) ) ;
#42797 = B_SPLINE_CURVE_WITH_KNOTS ( 'NONE', 5,
 ( #73364, #107502, #21815, #5043, #48170, #39188 ),
 .UNSPECIFIED., .F., .F.,
 ( 6, 6 ),
 ( 0.000000000000000000, 1.000000000000000000 ),
 .UNSPECIFIED. ) ;
#42798 = CARTESIAN_POINT ( 'NONE',  ( -2.831928916266819751, 1429.014365125550057, 200.1906073963359916 ) ) ;
#42799 = CARTESIAN_POINT ( 'NONE',  ( -22.45507226509999654, 1509.697208789830029, 190.1127326308979946 ) ) ;
#42800 = CARTESIAN_POINT ( 'NONE',  ( 5.513207777283239963, 1508.731180391410135, 216.5668095921479903 ) ) ;
#42801 = CARTESIAN_POINT ( 'NONE',  ( -1.700706814495000163, 1516.923170579120097, 211.4225755968969906 ) ) ;
#42802 = CARTESIAN_POINT ( 'NONE',  ( -11.71534935561269819, 1482.452763970830119, 207.0198387685339867 ) ) ;
#42803 = CARTESIAN_POINT ( 'NONE',  ( 30.36939524941482205, 1525.506916460681623, 221.4200585932857166 ) ) ;
#42805 = ORIENTED_EDGE ( 'NONE', *, *, #67827, .F. ) ;
#42804 = CARTESIAN_POINT ( 'NONE',  ( -43.09011427770000324, 1385.164419251190111, 247.5010251099589880 ) ) ;
#42806 = CARTESIAN_POINT ( 'NONE',  ( -67.78301067296590077, 1385.032250548179945, 292.4443811870189620 ) ) ;
#42807 = CARTESIAN_POINT ( 'NONE',  ( 29.81190406250000180, 1458.385319745129891, 254.8364781926979958 ) ) ;
#42808 = EDGE_CURVE ( 'NONE', #32688, #28487, #78142, .T. ) ;
#42809 = DIRECTION ( 'NONE',  ( 0.2020450509758154878, -0.9583089383565609465, -0.2020439953131532573 ) ) ;
#42810 = CARTESIAN_POINT ( 'NONE',  ( -3.703568358935259930, 1497.311626042180023, 220.9591690318370070 ) ) ;
#42811 = CARTESIAN_POINT ( 'NONE',  ( -2.573904878592180090, 1507.948512224160140, 237.1221455541720218 ) ) ;
#42812 = EDGE_CURVE ( 'NONE', #53037, #86983, #85497, .T. ) ;
#42813 = CARTESIAN_POINT ( 'NONE',  ( -5.721601866879999498, 1461.879722082089756, 205.5653134029390117 ) ) ;
#42814 = ADVANCED_FACE ( 'NONE', ( #38155 ), #25887, .F. ) ;
#42816 = CARTESIAN_POINT ( 'NONE',  ( 17.87007737865920021, 1410.277280938980084, 222.8748137377850185 ) ) ;
#42815 = LINE ( 'NONE', #76976, #92964 ) ;
#42817 = CARTESIAN_POINT ( 'NONE',  ( -9.905565548761760652, 1448.662754155020139, 208.1208174031709746 ) ) ;
#42818 = CARTESIAN_POINT ( 'NONE',  ( -108.1388787236599995, 1383.031276538240036, 310.7739520621719862 ) ) ;
#42819 = ORIENTED_EDGE ( 'NONE', *, *, #110287, .T. ) ;
#42820 = CARTESIAN_POINT ( 'NONE',  ( 4.613762356885000138, 1516.939574742129935, 203.3372076122869885 ) ) ;
#42821 = CARTESIAN_POINT ( 'NONE',  ( 0.2158683024189999855, 1405.842952038429985, 267.2349487601980513 ) ) ;
#42822 = CARTESIAN_POINT ( 'NONE',  ( 27.78452736639999898, 1508.000976259829940, 207.7754990609180084 ) ) ;
#42823 = TOROIDAL_SURFACE ( 'NONE', #60754, 10.71315034250000053, 1.000000000000000000 ) ;
#42824 = EDGE_CURVE ( 'NONE', #96418, #11469, #54183, .T. ) ;
#42825 = CARTESIAN_POINT ( 'NONE',  ( 12.91403689499999885, 1422.765650913930131, 223.3157943658980287 ) ) ;
#42826 = CYLINDRICAL_SURFACE ( 'NONE', #94969, 1.999999999999999556 ) ;
#42827 = CARTESIAN_POINT ( 'NONE',  ( -19.83859993069999916, 1467.194195006989958, 209.1218459616989946 ) ) ;
#42828 = CARTESIAN_POINT ( 'NONE',  ( 2.093054630779237257, 1468.720840884834388, 218.9195178419581396 ) ) ;
#42829 = CARTESIAN_POINT ( 'NONE',  ( 27.33348089620090349, 1436.347956869720065, 136.7123816897339736 ) ) ;
#42830 = CARTESIAN_POINT ( 'NONE',  ( 35.60247521962389783, 1450.154959175330077, 136.2349793190689979 ) ) ;
#42831 = DIRECTION ( 'NONE',  ( -0.4090087482554316534, 0.000000000000000000, -0.9125304618753967700 ) ) ;
#42832 = CARTESIAN_POINT ( 'NONE',  ( -2.127754871950000126, 1429.399568160389890, 199.9814804629589844 ) ) ;
#42833 = CARTESIAN_POINT ( 'NONE',  ( 11.97166819159999918, 1507.754052776729850, 184.6972969620979939 ) ) ;
#42834 = CARTESIAN_POINT ( 'NONE',  ( 11.26319909285720122, 1480.121028330829859, 210.5495473590729887 ) ) ;
#42835 = DIRECTION ( 'NONE',  ( -0.6709778558543678662, 0.000000000000000000, 0.7414773880254711402 ) ) ;
#42836 = CARTESIAN_POINT ( 'NONE',  ( 20.71343476517534299, 1501.977400791986611, 238.3377464195763764 ) ) ;
#42837 = ORIENTED_EDGE ( 'NONE', *, *, #37091, .F. ) ;
#42838 = TOROIDAL_SURFACE ( 'NONE', #28529, 9.522913805089999073, 1.000000000000000000 ) ;
#42839 = CARTESIAN_POINT ( 'NONE',  ( -29.75208676439999778, 1419.160608152730219, 268.3665355201979992 ) ) ;
#42840 = CARTESIAN_POINT ( 'NONE',  ( 12.06139631399999956, 1433.903263441289710, 146.7588256667980033 ) ) ;
#42841 = DIRECTION ( 'NONE',  ( -0.6736849260863840838, 0.000000000000000000, 0.7390186874254150995 ) ) ;
#42842 = CARTESIAN_POINT ( 'NONE',  ( 13.93255354277440006, 1413.006837750429895, 191.0564263268389880 ) ) ;
#42843 = CARTESIAN_POINT ( 'NONE',  ( -0.3602478992429999916, 1417.265131029429995, 235.9082177996980079 ) ) ;
#42845 = CARTESIAN_POINT ( 'NONE',  ( 30.31404213106226919, 1524.330813522192102, 196.4516891724779271 ) ) ;
#42844 = DIRECTION ( 'NONE',  ( 0.9510565162951566398, 0.000000000000000000, 0.3090169943749382919 ) ) ;
#42846 = CARTESIAN_POINT ( 'NONE',  ( -12.75438347776878523, 1444.998130645058609, 185.9525006451713409 ) ) ;
#42848 = EDGE_CURVE ( 'NONE', #101083, #49944, #81920, .T. ) ;
#42847 = EDGE_CURVE ( 'NONE', #103478, #96085, #23395, .T. ) ;
#42849 = CARTESIAN_POINT ( 'NONE',  ( 10.41177329615350011, 1460.024665156439823, 205.9063136364349873 ) ) ;
#42850 = CARTESIAN_POINT ( 'NONE',  ( 3.931910744533549718, 1448.296755838050103, 184.2998928686550073 ) ) ;
#42851 = CIRCLE ( 'NONE', #69805, 0.9999999999999981126 ) ;
#42852 = FACE_BOUND ( 'NONE', #34906, .T. ) ;
#42853 = CARTESIAN_POINT ( 'NONE',  ( -29.99620953741502660, 1526.382868172863937, 198.4974435154502999 ) ) ;
#42854 = CARTESIAN_POINT ( 'NONE',  ( -17.98384814369800111, 1416.218865267220053, 209.3252038692039889 ) ) ;
#42855 = CARTESIAN_POINT ( 'NONE',  ( 25.19713807460000154, 1435.377389496489741, 135.6160520644979783 ) ) ;
#42856 =( BOUNDED_CURVE ( )  B_SPLINE_CURVE ( 3, ( #93529, #109799, #50461, #59417 ),
 .UNSPECIFIED., .F., .F. ) 
 B_SPLINE_CURVE_WITH_KNOTS ( ( 4, 4 ),
 ( 5.097274837781307077, 5.883015582180852299 ),
 .UNSPECIFIED. ) 
 CURVE ( )  GEOMETRIC_REPRESENTATION_ITEM ( )  RATIONAL_B_SPLINE_CURVE ( ( 1.000000000000000000, 0.9492093126141469828, 0.9492093126141469828, 1.000000000000000000 ) ) 
 REPRESENTATION_ITEM ( '' )  );
#42858 = EDGE_CURVE ( 'NONE', #91618, #106043, #63515, .T. ) ;
#42857 = CARTESIAN_POINT ( 'NONE',  ( -13.43242319806410734, 1443.480650712422175, 169.3649796478555913 ) ) ;
#42859 = ORIENTED_EDGE ( 'NONE', *, *, #23624, .T. ) ;
#42860 = CARTESIAN_POINT ( 'NONE',  ( 0.04548916784448110012, 1416.835419214280137, 190.9576572557899965 ) ) ;
#42861 = CARTESIAN_POINT ( 'NONE',  ( 21.60872085536062315, 1509.279327547744060, 226.5667642667719690 ) ) ;
#42862 = ORIENTED_EDGE ( 'NONE', *, *, #23926, .F. ) ;
#42863 = ORIENTED_EDGE ( 'NONE', *, *, #95913, .T. ) ;
#42864 = CARTESIAN_POINT ( 'NONE',  ( -3.829620113920000346, 1515.551704408389924, 206.7917118429090237 ) ) ;
#42865 = CARTESIAN_POINT ( 'NONE',  ( 0.000000000000000000, 1508.913060387330006, 224.7618459619980058 ) ) ;
#42867 = CARTESIAN_POINT ( 'NONE',  ( -2.807895857490450009, 1457.864021610489999, 219.4185499695559827 ) ) ;
#42866 = CARTESIAN_POINT ( 'NONE',  ( 10.96395988120000098, 1426.065921947929837, 96.53120952369779673 ) ) ;
#42868 = CARTESIAN_POINT ( 'NONE',  ( 21.85421336060000286, 1409.676226334529929, 212.4289253482880042 ) ) ;
#42869 = CARTESIAN_POINT ( 'NONE',  ( -0.06958495686334870145, 1507.116651890610001, 237.3500246953010162 ) ) ;
#42870 = CARTESIAN_POINT ( 'NONE',  ( -12.30740102227800215, 1378.372698618640015, 209.8468845047000002 ) ) ;
#42871 = CIRCLE ( 'NONE', #84014, 40.01690241379998980 ) ;
#42872 = CARTESIAN_POINT ( 'NONE',  ( -2.534203887357130203, 1421.318133204249989, 184.2270941939309807 ) ) ;
#42873 = CARTESIAN_POINT ( 'NONE',  ( 7.868158389100000427, 1422.937290482379922, 214.1570520181289794 ) ) ;
#42874 = CARTESIAN_POINT ( 'NONE',  ( 3.217370068670000194, 1424.184623524309927, 188.9579833761989960 ) ) ;
#42875 = CARTESIAN_POINT ( 'NONE',  ( -23.96695290484002427, 1411.114064708981914, 209.9397034195345100 ) ) ;
#42876 = CARTESIAN_POINT ( 'NONE',  ( 3.225138584909999828, 1449.296389503839919, 183.9159307004979951 ) ) ;
#42877 = CARTESIAN_POINT ( 'NONE',  ( 7.930617565348595299, 1365.289423324231848, 208.3718459617061285 ) ) ;
#42879 = VERTEX_POINT ( 'NONE', #9510 ) ;
#42878 = CARTESIAN_POINT ( 'NONE',  ( 32.02808312589916540, 1501.977400791986611, 198.2787714533495489 ) ) ;
#42880 = ORIENTED_EDGE ( 'NONE', *, *, #72805, .T. ) ;
#42881 = CARTESIAN_POINT ( 'NONE',  ( -11.81668901717160125, 1429.106002162380037, 148.9487562432439915 ) ) ;
#42882 = CARTESIAN_POINT ( 'NONE',  ( 7.469839230337810498, 1510.808998942815151, 202.9715998142987985 ) ) ;
#42883 = CARTESIAN_POINT ( 'NONE',  ( -0.4703851458920000339, 1471.586156922030113, 269.6149382613980379 ) ) ;
#42884 = CARTESIAN_POINT ( 'NONE',  ( 13.80599381087229993, 1434.979619881599774, 146.4346930152470065 ) ) ;
#42885 = CARTESIAN_POINT ( 'NONE',  ( -98.25428003917552644, 1340.114449826969576, 312.4959904823201100 ) ) ;
#42886 = VECTOR ( 'NONE', #42417, 1000.000000000000114 ) ;
#42887 = CARTESIAN_POINT ( 'NONE',  ( 1.389373685237508260, 1526.382868173645647, 239.5386865367409825 ) ) ;
#42888 = CARTESIAN_POINT ( 'NONE',  ( 1.658713306182930225, 1476.135684546660059, 197.7577052247330016 ) ) ;
#42889 = CARTESIAN_POINT ( 'NONE',  ( 22.38213208939999888, 1410.189388605130034, 206.5142564081580190 ) ) ;
#42890 = DIRECTION ( 'NONE',  ( 0.000000000000000000, 0.000000000000000000, 1.000000000000000000 ) ) ;
#42891 = CARTESIAN_POINT ( 'NONE',  ( -21.79083509029999988, 1497.713060387329961, 204.1580431575879686 ) ) ;
#42892 = CARTESIAN_POINT ( 'NONE',  ( 10.69176820126198280, 1368.033143093960234, 209.6218459617033432 ) ) ;
#42893 = CARTESIAN_POINT ( 'NONE',  ( 13.39711660771139989, 1407.758611748120074, 204.6035603181729812 ) ) ;
#42894 = CARTESIAN_POINT ( 'NONE',  ( -20.64341172155089765, 1409.395087195580118, 268.3019762121069789 ) ) ;
#42895 = CARTESIAN_POINT ( 'NONE',  ( -14.27116635546209977, 1435.344418236619958, 149.4515510706479802 ) ) ;
#42896 = ORIENTED_EDGE ( 'NONE', *, *, #30977, .T. ) ;
#42897 = FACE_OUTER_BOUND ( 'NONE', #49526, .T. ) ;
#42898 = CARTESIAN_POINT ( 'NONE',  ( 14.26589412800000112, 1443.159997941379970, 189.6457918547979773 ) ) ;
#42899 = B_SPLINE_SURFACE_WITH_KNOTS ( 'NONE', 5, 5, ( 
 ( #47119, #107558, #30293, #40349, #106462, #54982 ),
 ( #72332, #31397, #108661, #108101, #89652, #107005 ),
 ( #29746, #82905, #55525, #12938, #21865, #56064 ),
 ( #90191, #13475, #57186, #5662, #99138, #39810 ),
 ( #73970, #47665, #12395, #89107, #65577, #56618 ),
 ( #81792, #99689, #5095, #21321, #73422, #91310 ) ),
 .UNSPECIFIED., .F., .F., .F.,
 ( 6, 6 ),
 ( 6, 6 ),
 ( 9.044683945550000104, 20.53336383379999930 ),
 ( 0.000000000000000000, 2.000000000000000000 ),
 .UNSPECIFIED. ) ;
#42900 = EDGE_LOOP ( 'NONE', ( #95102, #81112 ) ) ;
#42901 = EDGE_LOOP ( 'NONE', ( #85514, #90817, #96340, #11793, #54458, #77297, #86160, #40224, #26679, #514, #26571 ) ) ;
#42902 = LINE ( 'NONE', #58603, #96640 ) ;
#42903 = CARTESIAN_POINT ( 'NONE',  ( -21.80961449745526437, 1523.919934424249959, 183.3321337352031435 ) ) ;
#42904 = CARTESIAN_POINT ( 'NONE',  ( -6.549762485114999144, 1516.729202374750002, 213.7405950387170037 ) ) ;
#42905 = CARTESIAN_POINT ( 'NONE',  ( -17.36067012530000042, 1485.486309981630029, 188.4584240454980204 ) ) ;
#42906 = CARTESIAN_POINT ( 'NONE',  ( -9.842849654513400992, 1471.074449186950005, 212.0442494326119913 ) ) ;
#42907 = B_SPLINE_SURFACE_WITH_KNOTS ( 'NONE', 5, 5, ( 
 ( #88989, #98490, #73306, #87918, #12833, #12277 ),
 ( #79509, #100688, #100150, #22309, #74425, #58713 ),
 ( #64919, #66584, #99032, #56512, #109660, #23971 ),
 ( #108552, #49218, #31842, #109122, #15020, #92846 ),
 ( #90639, #66027, #6641, #32936, #13920, #22865 ),
 ( #84455, #41358, #23435, #48107, #58166, #7741 ),
 ( #16124, #57629, #107992, #49766, #91198, #101225 ),
 ( #83897, #40796, #40242, #91744, #30737, #82247 ),
 ( #5546, #57071, #75526, #107441, #41904, #14478 ) ),
 .UNSPECIFIED., .F., .F., .F.,
 ( 6, 3, 6 ),
 ( 6, 6 ),
 ( 1.978931347950330100, 6.366800399639999775, 10.01893279935279857 ),
 ( -0.02042752934279919858, 2.000000000000000000 ),
 .UNSPECIFIED. ) ;
#42908 = ORIENTED_EDGE ( 'NONE', *, *, #89272, .F. ) ;
#42909 = CARTESIAN_POINT ( 'NONE',  ( -109.5441724509999943, 1376.937034645699896, 301.4143085365590196 ) ) ;
#42910 = CARTESIAN_POINT ( 'NONE',  ( -5.360253346836620025, 1422.908173213679902, 148.1968392030750294 ) ) ;
#42911 = CARTESIAN_POINT ( 'NONE',  ( 3.451033388965000004, 1517.025653221279981, 203.3353183697670090 ) ) ;
#42912 = CIRCLE ( 'NONE', #37549, 1.000000000000000888 ) ;
#42913 = B_SPLINE_CURVE_WITH_KNOTS ( 'NONE', 3,
 ( #66093, #101286, #66644, #84514, #58229, #100745, #16185, #83961, #110819, #25140, #94013, #49279, #58774, #110262, #109721, #34663, #50927, #539, #24031, #76669, #68301, #7261, #75590, #24581, #8345, #40858, #32998, #100220, #23500, #101847, #57692, #75034, #59344, #67185, #92353, #91807, #15086, #34111, #15625, #92912, #93453, #83408, #109185, #16724, #49831, #6703, #32470, #41424, #50386, #7803, #41970, #43078, #102410, #76122, #33538, #67738, #85055, #25692, #42509, #59889, #17277, #51468, #85600, #8901 ),
 .UNSPECIFIED., .F., .F.,
 ( 4, 3, 3, 3, 3, 3, 3, 3, 3, 3, 3, 3, 3, 3, 3, 3, 3, 3, 3, 3, 3, 4 ),
 ( -26.25736392449690015, -24.17957599523969847, -21.70254519240599933, -19.22146160226090217, -16.73813815629290147, -15.82759752639899986, -13.34013828998019946, -11.64113835685350118, -9.942138423719999452, -9.890507822196667576, -9.830620131415628293, -9.764989817940161743, -9.692984518980310327, -9.605203300184257387, -9.521724663411312406, -9.450162862300381050, -9.387712128909072362, -9.328012329869999064, -8.803020716547550251, -8.080332690346452296, -7.533520025769998796, -7.218912042999999557 ),
 .UNSPECIFIED. ) ;
#42914 = CARTESIAN_POINT ( 'NONE',  ( -28.13477487810000000, 1508.112005706330137, 208.1343964124890249 ) ) ;
#42915 = B_SPLINE_SURFACE_WITH_KNOTS ( 'NONE', 4, 5, ( 
 ( #106398, #37541, #71176, #38089, #62789, #71743 ),
 ( #79560, #81182, #105860, #105297, #38632, #4498 ),
 ( #46514, #29683, #106938, #96904, #21804, #55460 ),
 ( #28588, #45417, #72264, #56004, #3962, #3411 ),
 ( #54372, #73352, #97447, #80648, #2860, #90128 ) ),
 .UNSPECIFIED., .F., .F., .F.,
 ( 5, 5 ),
 ( 6, 6 ),
 ( 21.65831097310000075, 21.66873975040000033 ),
 ( 0.000000000000000000, 2.175433359549999945 ),
 .UNSPECIFIED. ) ;
#42916 = CARTESIAN_POINT ( 'NONE',  ( -0.5884397385249999779, 1477.829042423129977, 230.4572567998980048 ) ) ;
#42917 = CARTESIAN_POINT ( 'NONE',  ( -48.07998102645539973, 1384.611432322939891, 222.4239625009780070 ) ) ;
#42918 = CARTESIAN_POINT ( 'NONE',  ( -4.214983652439999950, 1408.999356326429961, 195.2850467926979832 ) ) ;
#42919 = CARTESIAN_POINT ( 'NONE',  ( -11.90005276459999983, 1409.328619386830042, 226.7881247709979959 ) ) ;
#42921 = ORIENTED_EDGE ( 'NONE', *, *, #43617, .F. ) ;
#42920 = CARTESIAN_POINT ( 'NONE',  ( 15.83141032767047385, 1506.691119431293828, 193.5604645770621062 ) ) ;
#42922 = CARTESIAN_POINT ( 'NONE',  ( -23.83721392209670142, 1411.098975797860021, 210.1927897357339816 ) ) ;
#42923 = CARTESIAN_POINT ( 'NONE',  ( 26.41621169419999759, 1469.246811861230071, 210.3255135326479888 ) ) ;
#42924 = CARTESIAN_POINT ( 'NONE',  ( -46.82776862987225996, 1379.681009986248000, 239.8345724582786431 ) ) ;
#42925 = CARTESIAN_POINT ( 'NONE',  ( 19.02723184334069728, 1456.923419417749983, 225.4092703561889834 ) ) ;
#42926 = CARTESIAN_POINT ( 'NONE',  ( -24.38719517939999903, 1435.532251698759865, 137.4549481994980056 ) ) ;
#42928 = CARTESIAN_POINT ( 'NONE',  ( 4.624736859184999993, 1516.994127245590107, 211.9896495963369887 ) ) ;
#42927 = CIRCLE ( 'NONE', #33956, 1.999999999999997780 ) ;
#42929 = CARTESIAN_POINT ( 'NONE',  ( -68.68762034649999748, 1379.747740914639962, 279.9560673389590306 ) ) ;
#42930 = CARTESIAN_POINT ( 'NONE',  ( 8.691106598842869957, 1437.158280762230106, 210.3924950745289948 ) ) ;
#42931 = CARTESIAN_POINT ( 'NONE',  ( 17.08121475022219471, 1494.817603994912133, 195.5684645336626204 ) ) ;
#42932 = CARTESIAN_POINT ( 'NONE',  ( 5.781585778145000631, 1516.939646076049939, 209.1093989964429909 ) ) ;
#42933 = ORIENTED_EDGE ( 'NONE', *, *, #6036, .F. ) ;
#42934 = CARTESIAN_POINT ( 'NONE',  ( 0.000000000000000000, 0.000000000000000000, 137.0999999980979851 ) ) ;
#42935 = CARTESIAN_POINT ( 'NONE',  ( -3.094201202990000343, 1410.302849984529985, 232.4943490077980073 ) ) ;
#42936 = CARTESIAN_POINT ( 'NONE',  ( -67.04318418450000649, 1385.033547286170005, 292.1847026260589928 ) ) ;
#42937 = ORIENTED_EDGE ( 'NONE', *, *, #55066, .F. ) ;
#42938 = CARTESIAN_POINT ( 'NONE',  ( -105.0581303879369983, 1379.236400313860031, 304.0328620142400382 ) ) ;
#42939 = CARTESIAN_POINT ( 'NONE',  ( -3.727996856979999940, 1429.778334239190144, 201.6824411274789952 ) ) ;
#42940 = CARTESIAN_POINT ( 'NONE',  ( 12.11768918586579957, 1435.396653826159991, 151.1061025449240276 ) ) ;
#42941 = ADVANCED_FACE ( 'NONE', ( #585 ), #76873, .T. ) ;
#42942 = CARTESIAN_POINT ( 'NONE',  ( 13.59057177484809920, 1459.300748119509990, 230.6113061433740086 ) ) ;
#42943 = CARTESIAN_POINT ( 'NONE',  ( -23.56173385978110346, 1508.473166743119918, 223.3827176401680106 ) ) ;
#42944 = DIRECTION ( 'NONE',  ( 0.9455185755993178454, 0.000000000000000000, -0.3255681544571537578 ) ) ;
#42945 = CYLINDRICAL_SURFACE ( 'NONE', #109227, 1.000000000000001110 ) ;
#42946 = CARTESIAN_POINT ( 'NONE',  ( 10.10905480207389928, 1461.386512538610077, 208.4426341898000032 ) ) ;
#42948 = CARTESIAN_POINT ( 'NONE',  ( -3.268819354880000194, 1420.886035747430014, 185.9708108249980114 ) ) ;
#42947 = CARTESIAN_POINT ( 'NONE',  ( 3.265407117845000151, 1516.754149861460064, 213.7315192116670062 ) ) ;
#42949 = CARTESIAN_POINT ( 'NONE',  ( 19.86733751369999723, 1508.094164472129933, 189.0003703628979963 ) ) ;
#42950 = CARTESIAN_POINT ( 'NONE',  ( -6.554778571775000451, 1516.929962200689943, 216.8412383526069789 ) ) ;
#42951 = VERTEX_POINT ( 'NONE', #10629 ) ;
#42952 = CARTESIAN_POINT ( 'NONE',  ( -12.78752278169999812, 1416.843576337130116, 195.5392800409980225 ) ) ;
#42953 = CARTESIAN_POINT ( 'NONE',  ( -16.91136577339999647, 1420.382390858989993, 203.5950266307289951 ) ) ;
#42954 = ORIENTED_EDGE ( 'NONE', *, *, #88424, .F. ) ;
#42955 = FACE_OUTER_BOUND ( 'NONE', #108939, .T. ) ;
#42956 = ADVANCED_FACE ( 'NONE', ( #3354 ), #85812, .T. ) ;
#42957 = CARTESIAN_POINT ( 'NONE',  ( -109.1309839890330124, 1384.924126711810004, 311.2646841801559958 ) ) ;
#42958 = CARTESIAN_POINT ( 'NONE',  ( 2.444956619880277682, 1524.972613296788722, 175.9713629724293469 ) ) ;
#42959 = CARTESIAN_POINT ( 'NONE',  ( -1.634820292203019942, 1423.130284601479843, 191.2821113036930001 ) ) ;
#42960 = DIRECTION ( 'NONE',  ( -6.123233995736769734E-17, -1.000000000000000000, -1.124819836996399911E-32 ) ) ;
#42961 = CARTESIAN_POINT ( 'NONE',  ( -3.620610479546780169, 1508.125677570226799, 220.7440378608293656 ) ) ;
#42962 = CIRCLE ( 'NONE', #21433, 1.999999999999997780 ) ;
#42963 = CARTESIAN_POINT ( 'NONE',  ( 18.94857910520000033, 1416.535385209630022, 210.2462401506180072 ) ) ;
#42964 = CARTESIAN_POINT ( 'NONE',  ( 19.77969251879999746, 1507.818093401829856, 229.2755605921979907 ) ) ;
#42965 = CARTESIAN_POINT ( 'NONE',  ( -3.206876023519999563, 1419.434649146130141, 184.2270935464979971 ) ) ;
#42966 = EDGE_CURVE ( 'NONE', #43145, #2720, #88436, .T. ) ;
#42967 = CARTESIAN_POINT ( 'NONE',  ( 14.45783227242900004, 1416.839692127189892, 196.8516148535319985 ) ) ;
#42968 = CARTESIAN_POINT ( 'NONE',  ( 40.67904025323289829, 1440.913060359499923, 260.2254464820850330 ) ) ;
#42970 = CARTESIAN_POINT ( 'NONE',  ( -2.898761972770000028, 1491.529727365290000, 188.3233188772989877 ) ) ;
#42969 = CARTESIAN_POINT ( 'NONE',  ( -11.00755960056369887, 1418.479267630810000, 198.0234245325859774 ) ) ;
#42971 = CARTESIAN_POINT ( 'NONE',  ( 10.94841652689837197, 1430.808938732566503, 151.6571754023756569 ) ) ;
#42972 = ORIENTED_EDGE ( 'NONE', *, *, #70910, .F. ) ;
#42973 = CARTESIAN_POINT ( 'NONE',  ( 1.547206249379240006, 1416.640375553360172, 190.2404263963619826 ) ) ;
#42974 = CARTESIAN_POINT ( 'NONE',  ( 23.10158937639999976, 1411.031839729830153, 207.3184562272780056 ) ) ;
#42975 = DIRECTION ( 'NONE',  ( 1.000000000000000000, 0.000000000000000000, 0.000000000000000000 ) ) ;
#42976 = CARTESIAN_POINT ( 'NONE',  ( -28.77213282419999985, 1509.917805404529872, 211.3774502118079965 ) ) ;
#42977 = CARTESIAN_POINT ( 'NONE',  ( 8.876786928998038562, 1425.079649666100067, 195.6689664040229957 ) ) ;
#42978 = CARTESIAN_POINT ( 'NONE',  ( -3.945206105667222740, 1426.016427470225381, 186.0654355582702806 ) ) ;
#42979 = DIRECTION ( 'NONE',  ( -1.000000000000000000, 0.000000000000000000, 0.000000000000000000 ) ) ;
#42980 = DIRECTION ( 'NONE',  ( -0.9942586961433749204, 0.000000000000000000, 0.1070030146457375819 ) ) ;
#42981 = CARTESIAN_POINT ( 'NONE',  ( -9.104784486305129931, 1421.478983581930152, 192.1853070824809890 ) ) ;
#42982 = CARTESIAN_POINT ( 'NONE',  ( -73.85600498739088948, 1383.781764016229999, 298.7751872343750392 ) ) ;
#42983 = PLANE ( 'NONE',  #57114 ) ;
#42984 = CARTESIAN_POINT ( 'NONE',  ( -27.33695648125489441, 1509.220068158296499, 212.0715281516864081 ) ) ;
#42986 = EDGE_CURVE ( 'NONE', #58330, #77302, #80033, .T. ) ;
#42985 = CARTESIAN_POINT ( 'NONE',  ( -22.57319772750419773, 1409.701314710050156, 209.4509374963450057 ) ) ;
#42988 = ORIENTED_EDGE ( 'NONE', *, *, #5135, .F. ) ;
#42987 = CARTESIAN_POINT ( 'NONE',  ( 10.57168423260889867, 1452.490699057229904, 209.2976520326539855 ) ) ;
#42989 = CARTESIAN_POINT ( 'NONE',  ( -17.45699404409595346, 1460.525946869913014, 228.2422679384081619 ) ) ;
#42990 = CIRCLE ( 'NONE', #44842, 2.500000000000002220 ) ;
#42991 = CARTESIAN_POINT ( 'NONE',  ( -64.53155199309999546, 1384.701788983860297, 254.0354793386590018 ) ) ;
#42992 = CARTESIAN_POINT ( 'NONE',  ( -18.13442287810000053, 1409.546328388530128, 221.5845444630980126 ) ) ;
#42993 = EDGE_LOOP ( 'NONE', ( #97822, #36987, #5588, #104733 ) ) ;
#42994 = VERTEX_POINT ( 'NONE', #37479 ) ;
#42995 = CARTESIAN_POINT ( 'NONE',  ( 20.31327811046839926, 1509.661823207899943, 230.8228138406879850 ) ) ;
#42996 = FACE_OUTER_BOUND ( 'NONE', #37905, .T. ) ;
#42997 = CARTESIAN_POINT ( 'NONE',  ( 39.45646300420639818, 1440.433025902419786, 136.7700313797910212 ) ) ;
#42999 = CARTESIAN_POINT ( 'NONE',  ( 31.32995031131189378, 1523.678648413191695, 196.3423562208913324 ) ) ;
#42998 = CARTESIAN_POINT ( 'NONE',  ( 21.39582113410000019, 1488.805759879729976, 209.2914421362780217 ) ) ;
#43000 = AXIS2_PLACEMENT_3D ( 'NONE', #81271, #94637, #8417 ) ;
#43001 = MECHANICAL_DESIGN_GEOMETRIC_PRESENTATION_REPRESENTATION (  '', ( #48608 ), #100463 ) ;
#43002 = CARTESIAN_POINT ( 'NONE',  ( -3.467940602053699806, 1495.562067921990092, 197.2905559617530002 ) ) ;
#43003 = CARTESIAN_POINT ( 'NONE',  ( -108.9897655200000059, 1383.709197802749941, 297.2975670400589934 ) ) ;
#43004 = CARTESIAN_POINT ( 'NONE',  ( -12.36580673073694925, 1435.688790776224323, 151.0188895871725094 ) ) ;
#43005 = CARTESIAN_POINT ( 'NONE',  ( -21.10757296110000070, 1485.953501962929977, 191.9491461224980071 ) ) ;
#43006 = CARTESIAN_POINT ( 'NONE',  ( 3.145295632899999916, 1409.190415107630088, 186.3419696091980029 ) ) ;
#43007 = CARTESIAN_POINT ( 'NONE',  ( 1.120510598883349918, 1486.417731889569950, 197.2577259554180102 ) ) ;
#43008 = CARTESIAN_POINT ( 'NONE',  ( 11.34653490123289998, 1471.345105477939796, 210.4582031003209863 ) ) ;
#43009 = CARTESIAN_POINT ( 'NONE',  ( 11.04138766019999984, 1437.532134242359916, 152.0929085511980077 ) ) ;
#43010 = CARTESIAN_POINT ( 'NONE',  ( -8.316672828268760753, 1425.055149638239982, 204.9623390585310005 ) ) ;
#43011 = AXIS2_PLACEMENT_3D ( 'NONE', #28664, #45493, #71253 ) ;
#43012 = CARTESIAN_POINT ( 'NONE',  ( 32.86802468386292730, 1523.382868172864164, 217.2040256693915410 ) ) ;
#43013 = CARTESIAN_POINT ( 'NONE',  ( 1.280930038209999955, 1465.268052754130167, 235.9623018578980123 ) ) ;
#43014 = ORIENTED_EDGE ( 'NONE', *, *, #85913, .F. ) ;
#43015 = CARTESIAN_POINT ( 'NONE',  ( 22.29462128660000175, 1476.945831074090165, 209.5903111146230060 ) ) ;
#43016 = CARTESIAN_POINT ( 'NONE',  ( -40.40963026859999729, 1454.388582061129910, 270.2497097010980269 ) ) ;
#43017 = CARTESIAN_POINT ( 'NONE',  ( 0.000000000000000000, 1524.551704408390151, 209.1218459616989946 ) ) ;
#43018 = LINE ( 'NONE', #51407, #91574 ) ;
#43019 = CARTESIAN_POINT ( 'NONE',  ( 15.13342375178309851, 1507.606285622089899, 226.3974328904010065 ) ) ;
#43020 = CARTESIAN_POINT ( 'NONE',  ( -4.628375330620350073E-09, 1471.965220085929786, 258.9142969561589780 ) ) ;
#43021 = CARTESIAN_POINT ( 'NONE',  ( -3.071538966616303767, 1375.413060387289988, 207.4438565765842952 ) ) ;
#43022 = CARTESIAN_POINT ( 'NONE',  ( -2.112511269397119751, 1421.339275277370007, 193.6972829403189849 ) ) ;
#43023 = CARTESIAN_POINT ( 'NONE',  ( -10.01338583650000125, 1417.954340053530132, 229.9952712016979888 ) ) ;
#43024 = CARTESIAN_POINT ( 'NONE',  ( -0.7908576644959989244, 1476.560707045389790, 198.6323293514989814 ) ) ;
#43025 = CARTESIAN_POINT ( 'NONE',  ( -105.9466775579999904, 1388.732462752959918, 308.9851393517590168 ) ) ;
#43026 = CARTESIAN_POINT ( 'NONE',  ( -8.723513748773688903, 1511.461300288249959, 214.7083397760629850 ) ) ;
#43027 = CARTESIAN_POINT ( 'NONE',  ( 0.06125050287350902040, 1359.189416546558277, 210.6218459617030021 ) ) ;
#43028 = CARTESIAN_POINT ( 'NONE',  ( -45.86255884625870038, 1437.690697618850209, 266.6831300263739877 ) ) ;
#43029 = CARTESIAN_POINT ( 'NONE',  ( 1.077236975575300182, 1429.570469006359872, 217.3610909002520089 ) ) ;
#43030 = CARTESIAN_POINT ( 'NONE',  ( 32.38845791999500534, 1512.187213306747481, 216.1254071228445639 ) ) ;
#43031 = ORIENTED_EDGE ( 'NONE', *, *, #106120, .T. ) ;
#43032 = CARTESIAN_POINT ( 'NONE',  ( -0.7468175536419978666, 1517.006509894990131, 209.1289748073840258 ) ) ;
#43033 = AXIS2_PLACEMENT_3D ( 'NONE', #35842, #44809, #78963 ) ;
#43034 = CARTESIAN_POINT ( 'NONE',  ( -9.082734998440001206, 1385.203252519110038, 199.9450228470490174 ) ) ;
#43035 = B_SPLINE_SURFACE_WITH_KNOTS ( 'NONE', 5, 1, ( 
 ( #103864, #33890 ),
 ( #18190, #85387 ),
 ( #329, #7592 ),
 ( #9801, #68086 ),
 ( #8135, #102198 ),
 ( #9261, #1409 ),
 ( #94340, #110058 ),
 ( #86506, #60790 ),
 ( #42301, #35550 ) ),
 .UNSPECIFIED., .F., .F., .F.,
 ( 6, 3, 6 ),
 ( 2, 2 ),
 ( 0.000000000000000000, 4.014896071639999953, 8.012535616930000160 ),
 ( 0.000000000000000000, 14.00000000000000000 ),
 .UNSPECIFIED. ) ;
#43036 = CARTESIAN_POINT ( 'NONE',  ( -7.417501983117125164, 1471.160291404393547, 216.0174856262001128 ) ) ;
#43037 = CARTESIAN_POINT ( 'NONE',  ( 7.539259600540419548, 1425.677988097199886, 212.1893721227209824 ) ) ;
#43038 = CARTESIAN_POINT ( 'NONE',  ( -25.44898708460110015, 1451.960713826190158, 135.8021707696539977 ) ) ;
#43039 = VERTEX_POINT ( 'NONE', #21187 ) ;
#43040 = CARTESIAN_POINT ( 'NONE',  ( 28.07850873120000301, 1440.913060381239802, 231.9053043630979971 ) ) ;
#43042 = CARTESIAN_POINT ( 'NONE',  ( -14.86025866229079995, 1514.013728165539987, 223.9912627551279911 ) ) ;
#43041 = CARTESIAN_POINT ( 'NONE',  ( -2.691689582131152836, 1524.775785348137561, 176.4304728337446306 ) ) ;
#43043 = FACE_OUTER_BOUND ( 'NONE', #10126, .T. ) ;
#43044 = AXIS2_PLACEMENT_3D ( 'NONE', #99254, #107680, #81355 ) ;
#43045 = CARTESIAN_POINT ( 'NONE',  ( -23.04921901674742202, 1449.613099141845169, 219.4632572153743411 ) ) ;
#43046 = CARTESIAN_POINT ( 'NONE',  ( 7.911464481230000345, 1423.187191425399988, 213.2893462354790017 ) ) ;
#43047 = CARTESIAN_POINT ( 'NONE',  ( 4.220605471363215067, 1441.596061467261961, 170.5366720304299974 ) ) ;
#43048 = CARTESIAN_POINT ( 'NONE',  ( -15.72751745975079984, 1522.051704408389924, 211.3620530696679793 ) ) ;
#43049 = ORIENTED_EDGE ( 'NONE', *, *, #51374, .F. ) ;
#43050 = CARTESIAN_POINT ( 'NONE',  ( -1.867263997642370166, 1407.952308472890081, 270.2921350646259953 ) ) ;
#43051 = CARTESIAN_POINT ( 'NONE',  ( 8.033834871089998941, 1417.062815916630143, 230.8059444928980213 ) ) ;
#43052 = CARTESIAN_POINT ( 'NONE',  ( -0.4986843622567649348, 1508.982343520079894, 238.8510830230749775 ) ) ;
#43054 = ORIENTED_EDGE ( 'NONE', *, *, #25350, .T. ) ;
#43053 = CARTESIAN_POINT ( 'NONE',  ( -3.005276066433927973, 1369.205039411293910, 210.6218459616987957 ) ) ;
#43055 = VERTEX_POINT ( 'NONE', #89528 ) ;
#43056 = CARTESIAN_POINT ( 'NONE',  ( 18.86688640473602874, 1512.187213306747481, 237.4611898188519774 ) ) ;
#43057 = CARTESIAN_POINT ( 'NONE',  ( -0.6901598988031059090, 1408.937161423990119, 186.3200950031190075 ) ) ;
#43058 = CARTESIAN_POINT ( 'NONE',  ( -2.368833328420000051, 1427.018531676430030, 133.6118001900980232 ) ) ;
#43059 = CARTESIAN_POINT ( 'NONE',  ( -20.77546492954260060, 1499.605258637040151, 192.4370125005800105 ) ) ;
#43060 = CARTESIAN_POINT ( 'NONE',  ( -20.65311841410000326, 1420.828459663129934, 220.4668751674979887 ) ) ;
#43061 = CARTESIAN_POINT ( 'NONE',  ( 39.11478698586859082, 1459.396654483650082, 266.6203158930860013 ) ) ;
#43062 = CARTESIAN_POINT ( 'NONE',  ( -11.49929945651590124, 1391.913060387289988, 207.6743836541510007 ) ) ;
#43063 = DIRECTION ( 'NONE',  ( -0.9995237709234254808, 0.03085824620771311644, -1.986952269380852068E-13 ) ) ;
#43064 = CARTESIAN_POINT ( 'NONE',  ( 4.609064303374999838, 1516.723920667490120, 206.2441009858569885 ) ) ;
#43065 = EDGE_LOOP ( 'NONE', ( #7423, #65864 ) ) ;
#43066 = CARTESIAN_POINT ( 'NONE',  ( 18.30869780503379118, 1459.158508961783355, 227.8104749284805450 ) ) ;
#43067 = CARTESIAN_POINT ( 'NONE',  ( -0.5237593457439969624, 1444.658999873350012, 199.0797042155420229 ) ) ;
#43068 = AXIS2_PLACEMENT_3D ( 'NONE', #89554, #12286, #46480 ) ;
#43069 = ORIENTED_EDGE ( 'NONE', *, *, #21376, .F. ) ;
#43070 = CARTESIAN_POINT ( 'NONE',  ( -0.9613100514576319311, 1458.000292018469736, 229.8256281850430014 ) ) ;
#43071 = CARTESIAN_POINT ( 'NONE',  ( 25.65001819901760172, 1452.017406081909940, 135.2459253483869759 ) ) ;
#43072 = B_SPLINE_SURFACE_WITH_KNOTS ( 'NONE', 5, 4, ( 
 ( #110376, #33655, #93561, #5731, #74042 ),
 ( #26362, #34775, #60557, #104186, #77342 ),
 ( #69513, #2312, #9563, #44296, #103063 ),
 ( #60000, #644, #78439, #94119, #42628 ),
 ( #94678, #9018, #86832, #96339, #17391 ),
 ( #17949, #25802, #68960, #1194, #51588 ) ),
 .UNSPECIFIED., .F., .F., .F.,
 ( 6, 6 ),
 ( 5, 5 ),
 ( -1.876035874425760076E-05, 11.48858425020000062 ),
 ( 25.78146411700000229, 39.23969207129999859 ),
 .UNSPECIFIED. ) ;
#43073 = CARTESIAN_POINT ( 'NONE',  ( -3.274413360710510368, 1508.551704408389924, 213.9819696425469715 ) ) ;
#43074 = CARTESIAN_POINT ( 'NONE',  ( -7.129176379223929955E-16, 1388.284644706179961, 200.7336192388889913 ) ) ;
#43075 = CARTESIAN_POINT ( 'NONE',  ( 8.028494635650000433, 1421.573180670790180, 196.0255996755989827 ) ) ;
#43076 = CARTESIAN_POINT ( 'NONE',  ( 18.68627176030000214, 1410.927968804830016, 194.6744492970979934 ) ) ;
#43077 = CARTESIAN_POINT ( 'NONE',  ( -3.370191024799999990, 1496.076861593789772, 198.0269959760989877 ) ) ;
#43078 = CARTESIAN_POINT ( 'NONE',  ( 1.734150443606229830, 1408.973618255220117, 186.8556639801219887 ) ) ;
#43080 = CARTESIAN_POINT ( 'NONE',  ( -21.56194541866146608, 1429.229356591500391, 219.1470650008878067 ) ) ;
#43079 = CARTESIAN_POINT ( 'NONE',  ( 2.395751473290000266, 1417.680330609130124, 234.5234243683980253 ) ) ;
#43081 = CARTESIAN_POINT ( 'NONE',  ( 2.760778564396810353, 1409.009468899150079, 230.1977509304229841 ) ) ;
#43082 = CARTESIAN_POINT ( 'NONE',  ( -0.004856263471414200630, 1508.953874411239894, 179.4326758686540018 ) ) ;
#43083 = CARTESIAN_POINT ( 'NONE',  ( -10.76474969630000089, 1381.207448912699874, 216.6668544953589901 ) ) ;
#43084 = CARTESIAN_POINT ( 'NONE',  ( 3.067412410608044926, 1369.643261120324723, 207.6621350963564225 ) ) ;
#43085 = ORIENTED_EDGE ( 'NONE', *, *, #89086, .F. ) ;
#43086 = CARTESIAN_POINT ( 'NONE',  ( -32.23107245337178739, 1523.542365884048195, 201.4053004075473439 ) ) ;
#43087 = CARTESIAN_POINT ( 'NONE',  ( 11.84451615446399941, 1432.336085895850147, 150.3016814953629989 ) ) ;
#43088 = CARTESIAN_POINT ( 'NONE',  ( -13.58041510073769942, 1508.551704408389924, 210.3416170870220014 ) ) ;
#43089 = CARTESIAN_POINT ( 'NONE',  ( -11.20926149449999976, 1388.118472602389829, 201.8648932818790058 ) ) ;
#43090 = CARTESIAN_POINT ( 'NONE',  ( 9.544470063946011607, 1422.591896480089872, 212.6773163756829774 ) ) ;
#43091 = CARTESIAN_POINT ( 'NONE',  ( -35.80287825771539900, 1450.088642008699935, 136.2393403088510127 ) ) ;
#43092 = CLOSED_SHELL ( 'NONE', ( #80232, #61878, #71595, #83659, #43713, #56991, #64610, #43213, #54197, #22031, #78967, #19387, #43979, #23700, #13357, #79872, #32868, #82246, #90576, #60165, #89807, #105744, #18887, #109678, #4170, #77849, #22890, #56473, #33845, #58221, #84950, #11068, #58658, #32297, #66541, #5410, #109221, #33942, #99412, #19930, #94747, #78455, #58938, #9648, #42707, #2956, #110728, #64671, #47773, #45248, #52186, #76954, #86702, #7639, #89163, #90737, #14477, #1558, #68732, #28252, #29008, #50024, #6869, #78342, #29506, #54437, #14599, #27361, #31161, #85011, #36658, #41803, #11826, #88618, #61021, #68704, #62835, #86822, #8488, #37892, #16898, #103100, #50786, #17634, #34311, #102782, #93701, #109002, #57755, #85705, #48652, #14522, #104112, #68882, #44708, #88325, #14459, #49534, #102680, #85165, #109361, #69508, #58654, #45414, #83141, #37103 ) ) ;
#43093 = CARTESIAN_POINT ( 'NONE',  ( 0.9870989395629991003, 1430.542139991489876, 217.5404054456389815 ) ) ;
#43094 = DIRECTION ( 'NONE',  ( 0.8775825618903763115, 0.000000000000000000, -0.4794255386041963996 ) ) ;
#43095 = CARTESIAN_POINT ( 'NONE',  ( -21.07223475955725434, 1508.254227182171917, 192.1325232464991757 ) ) ;
#43096 = CARTESIAN_POINT ( 'NONE',  ( 11.88608296559999999, 1433.201875827699951, 150.0808573810979851 ) ) ;
#43097 = CARTESIAN_POINT ( 'NONE',  ( 1.998401444330000344E-15, 1456.909266848530024, 224.8635561844979804 ) ) ;
#43098 = CARTESIAN_POINT ( 'NONE',  ( -9.681529208496559846, 1461.089882836170091, 208.7501511576820121 ) ) ;
#43099 = CIRCLE ( 'NONE', #86010, 0.9999999999999971134 ) ;
#43100 = CARTESIAN_POINT ( 'NONE',  ( -17.17366476699999822, 1421.220024669489931, 201.7389906317289956 ) ) ;
#43101 = CARTESIAN_POINT ( 'NONE',  ( 11.20832017736389830, 1422.284948798140022, 203.3916373928120152 ) ) ;
#43102 = DIRECTION ( 'NONE',  ( 0.000000000000000000, 0.000000000000000000, 1.000000000000000000 ) ) ;
#43103 = CARTESIAN_POINT ( 'NONE',  ( 22.68092815790000216, 1409.705069317929883, 208.9674978898780182 ) ) ;
#43104 = TOROIDAL_SURFACE ( 'NONE', #282, 30.13701971169416538, 3.000000000000000000 ) ;
#43105 = DIRECTION ( 'NONE',  ( 0.000000000000000000, 0.000000000000000000, -1.000000000000000000 ) ) ;
#43106 = CARTESIAN_POINT ( 'NONE',  ( -29.58054436722819958, 1509.946035758800008, 208.7921511973499662 ) ) ;
#43107 = B_SPLINE_CURVE_WITH_KNOTS ( 'NONE', 3,
 ( #107928, #90018, #106279, #54792, #88924, #81071, #21138, #72162, #4915, #31221, #30672, #47488, #90570, #3853, #106816, #3299 ),
 .UNSPECIFIED., .F., .F.,
 ( 4, 3, 3, 3, 3, 4 ),
 ( -5.332638707570000136, -5.312294071160000186, -5.120178322282729511, -4.857691371485320708, -4.648885627528850151, -4.382742598909070253 ),
 .UNSPECIFIED. ) ;
#43108 = CARTESIAN_POINT ( 'NONE',  ( -8.114887008623513864, 1425.452370286069936, 208.6318797277072861 ) ) ;
#43109 = CARTESIAN_POINT ( 'NONE',  ( 0.000000000000000000, 1508.913060387330006, 209.1218459616979999 ) ) ;
#43110 = CARTESIAN_POINT ( 'NONE',  ( -8.767938172670000085, 1509.161953616930077, 236.4477657171979956 ) ) ;
#43111 = CARTESIAN_POINT ( 'NONE',  ( 3.115880651068799967, 1508.551704408389924, 219.3718644903320012 ) ) ;
#43112 = CARTESIAN_POINT ( 'NONE',  ( 17.20730882039999798, 1475.513060387329915, 220.8541519961979986 ) ) ;
#43113 = CARTESIAN_POINT ( 'NONE',  ( 19.38664731554619891, 1498.811923964060043, 221.8202412713110050 ) ) ;
#43114 = CARTESIAN_POINT ( 'NONE',  ( -5.773668852974999766, 1516.734985836460055, 213.1604834329569940 ) ) ;
#43115 = CARTESIAN_POINT ( 'NONE',  ( -17.56945858326109899, 1419.688318994619976, 207.5872967556749984 ) ) ;
#43116 = CARTESIAN_POINT ( 'NONE',  ( 0.1614806029945209942, 1485.376953580510190, 181.8633822554020014 ) ) ;
#43118 = ORIENTED_EDGE ( 'NONE', *, *, #89147, .F. ) ;
#43117 = CARTESIAN_POINT ( 'NONE',  ( 3.060041444019999890, 1442.201653547689830, 217.5704310926890059 ) ) ;
#43119 = LINE ( 'NONE', #27404, #23515 ) ;
#43120 = CIRCLE ( 'NONE', #26979, 2.000000000000003553 ) ;
#43121 = CARTESIAN_POINT ( 'NONE',  ( -17.22592475669603473, 1443.913060387329097, 162.9227486557985003 ) ) ;
#43122 = CARTESIAN_POINT ( 'NONE',  ( 11.94106625650000097, 1433.615480207630071, 149.7888360282980216 ) ) ;
#43123 = CARTESIAN_POINT ( 'NONE',  ( -35.94635777402429966, 1451.396212934329924, 134.0999999986040052 ) ) ;
#43124 = CARTESIAN_POINT ( 'NONE',  ( -109.5352543199999928, 1384.892772668599946, 297.1231677395590509 ) ) ;
#43125 = VERTEX_POINT ( 'NONE', #3902 ) ;
#43126 = DIRECTION ( 'NONE',  ( 0.000000000000000000, 1.000000000000000000, 0.000000000000000000 ) ) ;
#43127 = CARTESIAN_POINT ( 'NONE',  ( -14.46044090995190068, 1380.092572431659846, 208.8609369278819941 ) ) ;
#43128 = CARTESIAN_POINT ( 'NONE',  ( -14.38361700439999957, 1416.219761280730154, 221.3510334114980083 ) ) ;
#43129 = CARTESIAN_POINT ( 'NONE',  ( 4.726708812725099129, 1506.677470858050128, 216.7649860373589945 ) ) ;
#43130 = EDGE_CURVE ( 'NONE', #60994, #69449, #56734, .T. ) ;
#43131 = CARTESIAN_POINT ( 'NONE',  ( -8.342137585866080229, 1436.639472651299911, 213.6062562556910223 ) ) ;
#43132 = CARTESIAN_POINT ( 'NONE',  ( -109.6086345746109885, 1383.178240054900016, 311.2147542219479988 ) ) ;
#43133 = CARTESIAN_POINT ( 'NONE',  ( -17.01518731959999897, 1422.007497235210167, 208.9682088309940013 ) ) ;
#43134 = CARTESIAN_POINT ( 'NONE',  ( 10.95098532600490060, 1471.837423856070018, 212.3987399694809994 ) ) ;
#43135 = CARTESIAN_POINT ( 'NONE',  ( -11.67738853530000043, 1391.388800472150251, 205.1463387926490043 ) ) ;
#43136 = CARTESIAN_POINT ( 'NONE',  ( -73.46128287683579572, 1385.129171348790123, 272.7076196986540140 ) ) ;
#43137 = CARTESIAN_POINT ( 'NONE',  ( -20.71343476517093052, 1522.906561336852974, 238.3377464195795596 ) ) ;
#43138 = CARTESIAN_POINT ( 'NONE',  ( 10.86984765289039956, 1425.686504684909778, 206.4627855528160012 ) ) ;
#43139 = ORIENTED_EDGE ( 'NONE', *, *, #62202, .T. ) ;
#43140 = VECTOR ( 'NONE', #78323, 1000.000000000000000 ) ;
#43141 = CARTESIAN_POINT ( 'NONE',  ( -15.73521006790659982, 1409.471155031050102, 225.4906514931829804 ) ) ;
#43143 = ORIENTED_EDGE ( 'NONE', *, *, #53438, .F. ) ;
#43142 = CARTESIAN_POINT ( 'NONE',  ( 3.063543637962659716, 1437.235349907490217, 227.3972379739110181 ) ) ;
#43144 = DIRECTION ( 'NONE',  ( -0.9997613315435491810, 0.000000000000000000, 0.02184673774890954004 ) ) ;
#43145 = VERTEX_POINT ( 'NONE', #105802 ) ;
#43146 = CARTESIAN_POINT ( 'NONE',  ( 22.37845227239999701, 1507.839484417730091, 224.3727521372980220 ) ) ;
#43147 = CARTESIAN_POINT ( 'NONE',  ( -8.798121132677117373, 1364.254821810437306, 207.6218459616988241 ) ) ;
#43148 = CARTESIAN_POINT ( 'NONE',  ( -11.03587947549999981, 1492.068057612589882, 205.8034202075890278 ) ) ;
#43149 = CARTESIAN_POINT ( 'NONE',  ( 35.14304713054083606, 1457.618104024274999, 269.5334826510517701 ) ) ;
#43150 = DIRECTION ( 'NONE',  ( 0.000000000000000000, -1.000000000000000000, 6.123233995736769734E-17 ) ) ;
#43151 = CARTESIAN_POINT ( 'NONE',  ( 16.20831509755612032, 1432.093373871191261, 218.3923509098792124 ) ) ;
#43152 = B_SPLINE_CURVE_WITH_KNOTS ( 'NONE', 3,
 ( #24837, #68546, #93162, #50624, #76374, #59583, #788, #86977, #35472, #10266, #110523, #34917, #68001, #76935, #27087, #69663, #16432, #69103, #84758, #103204, #42223, #94261, #26509, #17537, #94829, #60706, #78586, #44442, #33807, #51739, #18105 ),
 .UNSPECIFIED., .F., .F.,
 ( 4, 3, 3, 3, 3, 3, 3, 3, 3, 3, 4 ),
 ( -8.078160033293929843, -8.078122911508929249, -8.000183041957479091, -7.821082747455149864, -7.564042583401359821, -7.049962255293790392, -6.267197145476660403, -5.680236814612510621, -5.048466761624530008, -4.152322103108110340, -3.282032658275399584 ),
 .UNSPECIFIED. ) ;
#43153 = CARTESIAN_POINT ( 'NONE',  ( 1.448737595259999900, 1416.464314113729870, 232.8152744311979916 ) ) ;
#43154 = CARTESIAN_POINT ( 'NONE',  ( 8.704769445429999308, 1449.383511506689956, 205.9663214812090359 ) ) ;
#43155 = CARTESIAN_POINT ( 'NONE',  ( -21.33188487129976352, 1507.840678936435324, 227.2305665397985308 ) ) ;
#43156 = CARTESIAN_POINT ( 'NONE',  ( -8.340540947510188374, 1369.726010807078183, 209.6218459617033432 ) ) ;
#43157 = CARTESIAN_POINT ( 'NONE',  ( -0.1310594861909990250, 1456.247027522389999, 199.2609668081589973 ) ) ;
#43158 = CARTESIAN_POINT ( 'NONE',  ( -7.724732447025000504, 1517.133889586189980, 205.8614888033369823 ) ) ;
#43159 = CARTESIAN_POINT ( 'NONE',  ( 3.657345069180000241, 1446.327858677260110, 165.9157416560979925 ) ) ;
#43160 = COLOUR_RGB ( '', 0.31764706, 0.68627451, 0.89019608) ;
#43161 = DIRECTION ( 'NONE',  ( 9.158755289808628626E-47, -1.000000000000000000, 1.836970198721029688E-16 ) ) ;
#43162 = CARTESIAN_POINT ( 'NONE',  ( -3.040146223219999833, 1497.073695284489986, 198.2723897717989985 ) ) ;
#43164 = ORIENTED_EDGE ( 'NONE', *, *, #55584, .F. ) ;
#43163 = CARTESIAN_POINT ( 'NONE',  ( 0.1770319947259980098, 1496.149864682889984, 221.4922559367990118 ) ) ;
#43165 = CARTESIAN_POINT ( 'NONE',  ( -17.84338787571961049, 1501.977400791986611, 180.3600277896300383 ) ) ;
#43166 = EDGE_LOOP ( 'NONE', ( #30234, #108332, #83033, #64551, #83246 ) ) ;
#43167 = CARTESIAN_POINT ( 'NONE',  ( -16.78391011319079951, 1513.564960623335764, 222.3707652303824318 ) ) ;
#43168 = EDGE_CURVE ( 'NONE', #81409, #5765, #51049, .T. ) ;
#43169 = CARTESIAN_POINT ( 'NONE',  ( -24.62246550749999940, 1430.359249636930144, 207.4018885027879833 ) ) ;
#43171 = CARTESIAN_POINT ( 'NONE',  ( 16.11138931009760000, 1409.475610048200224, 192.9913841948230129 ) ) ;
#43170 = CARTESIAN_POINT ( 'NONE',  ( -11.08641866761180061, 1425.203475087560037, 139.7057191062969821 ) ) ;
#43172 = EDGE_CURVE ( 'NONE', #91492, #52184, #46998, .T. ) ;
#43173 = CARTESIAN_POINT ( 'NONE',  ( 1.717432448265000078, 1516.836638729160086, 211.4041475482669910 ) ) ;
#43174 = CARTESIAN_POINT ( 'NONE',  ( 28.97550801065250781, 1510.035835560405985, 201.3478078290377198 ) ) ;
#43175 = EDGE_CURVE ( 'NONE', #31041, #90450, #62298, .T. ) ;
#43176 = CARTESIAN_POINT ( 'NONE',  ( -20.56164794690000264, 1453.151875980330033, 207.7900157754679924 ) ) ;
#43177 = CARTESIAN_POINT ( 'NONE',  ( -43.50118324600000363, 1438.239418340559951, 263.8966221458980499 ) ) ;
#43178 = CARTESIAN_POINT ( 'NONE',  ( -12.31949146158819985, 1378.253793448930082, 209.5105130821430066 ) ) ;
#43179 = EDGE_CURVE ( 'NONE', #80823, #44004, #81121, .T. ) ;
#43180 = CARTESIAN_POINT ( 'NONE',  ( 18.07609654799121301, 1459.453657016485749, 227.9871296375955581 ) ) ;
#43181 = CARTESIAN_POINT ( 'NONE',  ( -5.022927203800000129, 1391.808120115790189, 214.6810046976989952 ) ) ;
#43182 = CARTESIAN_POINT ( 'NONE',  ( -37.21137227029399952, 1438.039346661569880, 136.5665973368240032 ) ) ;
#43183 = ORIENTED_EDGE ( 'NONE', *, *, #90855, .T. ) ;
#43184 = CARTESIAN_POINT ( 'NONE',  ( 8.869149785548881226, 1397.558652790959968, 219.0168133846440242 ) ) ;
#43185 = CARTESIAN_POINT ( 'NONE',  ( -19.65244154950000066, 1464.918788182289973, 211.1248570675190024 ) ) ;
#43186 = CARTESIAN_POINT ( 'NONE',  ( -16.78608357809999774, 1458.775951820630098, 230.6691475833980007 ) ) ;
#43187 = VERTEX_POINT ( 'NONE', #64352 ) ;
#43188 = EDGE_LOOP ( 'NONE', ( #6670, #59668, #66185, #85848 ) ) ;
#43189 = CARTESIAN_POINT ( 'NONE',  ( 9.099844284766479774, 1451.227735247490045, 210.8294423051630133 ) ) ;
#43190 = DIRECTION ( 'NONE',  ( 0.6670494068259388287, 0.5110419776299538475, 0.5421080943439499089 ) ) ;
#43191 = AXIS2_PLACEMENT_3D ( 'NONE', #58157, #27168, #61352 ) ;
#43192 = CARTESIAN_POINT ( 'NONE',  ( -14.17879220992960043, 1380.120661394760191, 210.8840528948799999 ) ) ;
#43193 = CARTESIAN_POINT ( 'NONE',  ( -10.83335895338246146, 1417.972034830828079, 198.1741477617316036 ) ) ;
#43194 = DIRECTION ( 'NONE',  ( 0.000000000000000000, 0.000000000000000000, 1.000000000000000000 ) ) ;
#43195 = CARTESIAN_POINT ( 'NONE',  ( -1.568400560060000171, 1461.197012475930023, 235.1144211530979931 ) ) ;
#43196 = CARTESIAN_POINT ( 'NONE',  ( 5.984345098296709686, 1508.551704613440052, 202.1093217104930204 ) ) ;
#43197 = CARTESIAN_POINT ( 'NONE',  ( 9.146213936677568768, 1449.998330935229887, 208.1168021020649803 ) ) ;
#43198 = CARTESIAN_POINT ( 'NONE',  ( -12.43710052089999962, 1391.584050381710085, 209.7498261801929971 ) ) ;
#43199 = ADVANCED_FACE ( 'NONE', ( #39111 ), #102777, .F. ) ;
#43200 = CARTESIAN_POINT ( 'NONE',  ( -106.7956374490409956, 1384.894787335530054, 297.0320324003700421 ) ) ;
#43201 = ORIENTED_EDGE ( 'NONE', *, *, #43940, .F. ) ;
#43202 =( BOUNDED_SURFACE ( )  B_SPLINE_SURFACE ( 3, 2, ( 
 ( #47115, #38690, #66550 ),
 ( #72865, #46577, #21861 ),
 ( #106458, #23938, #72328 ),
 ( #67094, #56060, #47661 ),
 ( #58133, #74941, #7166 ),
 ( #49734, #5090, #81241 ),
 ( #55521, #58682, #39243 ),
 ( #4020, #38147, #30289 ),
 ( #21317, #100652, #92816 ),
 ( #7707, #12391, #90187 ) ),
 .UNSPECIFIED., .F., .F., .F. ) 
 B_SPLINE_SURFACE_WITH_KNOTS ( ( 4, 2, 2, 2, 4 ),
 ( 3, 3 ),
 ( 1.570796326794896558, 1.963495408493620697, 2.356194490192344837, 2.748893571891068976, 3.141592653589793116 ),
 ( 0.000000000000000000, 1.000000000000000000 ),
 .UNSPECIFIED. ) 
 GEOMETRIC_REPRESENTATION_ITEM ( )  RATIONAL_B_SPLINE_SURFACE ( (
 ( 1.000000000000000000, 0.7071067811865872077, 1.000000000000000000),
 ( 1.000000000000000000, 0.7166207884826032437, 1.000000000000000000),
 ( 1.000000000000000000, 0.7259222650901892004, 1.000000000000000000),
 ( 1.000000000000000000, 0.7428408967935505869, 1.000000000000000000),
 ( 1.000000000000000000, 0.7504512394523125129, 1.000000000000000000),
 ( 1.000000000000000000, 0.7630177051951873013, 1.000000000000000000),
 ( 1.000000000000000000, 0.7679730451971447103, 1.000000000000000000),
 ( 1.000000000000000000, 0.7746454561799092087, 1.000000000000000000),
 ( 1.000000000000000000, 0.7763684247033758590, 1.000000000000000000),
 ( 1.000000000000000000, 0.7763623250684337229, 1.000000000000000000) ) ) 
 REPRESENTATION_ITEM ( '' )  SURFACE ( )  );
#43203 = CARTESIAN_POINT ( 'NONE',  ( -0.01244697378919850002, 1516.939646076049939, 203.3402601539570185 ) ) ;
#43204 = CARTESIAN_POINT ( 'NONE',  ( -7.337297350114999617, 1517.135701590510052, 208.3821536943570152 ) ) ;
#43205 = ORIENTED_EDGE ( 'NONE', *, *, #70155, .T. ) ;
#43206 = CARTESIAN_POINT ( 'NONE',  ( 11.80565717473840159, 1428.511365933469961, 148.4624678142999983 ) ) ;
#43207 = AXIS2_PLACEMENT_3D ( 'NONE', #43542, #77687, #62019 ) ;
#43208 = CARTESIAN_POINT ( 'NONE',  ( 19.88163472539999788, 1487.529703934430245, 227.8197638940980028 ) ) ;
#43209 = ORIENTED_EDGE ( 'NONE', *, *, #40772, .T. ) ;
#43210 = CARTESIAN_POINT ( 'NONE',  ( -1.463277806657410141, 1481.197952492230115, 182.6166260140540203 ) ) ;
#43211 = CARTESIAN_POINT ( 'NONE',  ( -16.68533971102617741, 1442.773887286371291, 162.0931267225411148 ) ) ;
#43212 = CARTESIAN_POINT ( 'NONE',  ( 6.925614559599999609, 1507.258869698729995, 235.3367835963979928 ) ) ;
#43213 = ADVANCED_FACE ( 'NONE', ( #5529 ), #91729, .F. ) ;
#43214 = CARTESIAN_POINT ( 'NONE',  ( -10.46250751532009993, 1491.356802638789986, 212.5409670664860187 ) ) ;
#43215 = CARTESIAN_POINT ( 'NONE',  ( -5.374640472830000348, 1422.289355296129997, 186.1135859276980113 ) ) ;
#43216 = CARTESIAN_POINT ( 'NONE',  ( 10.52707133736559975, 1469.924776803789882, 207.1255290707819938 ) ) ;
#43217 = CARTESIAN_POINT ( 'NONE',  ( -10.06450494029999909, 1472.332863763290106, 203.5506889703189870 ) ) ;
#43218 = EDGE_CURVE ( 'NONE', #87081, #93372, #2020, .T. ) ;
#43219 = CARTESIAN_POINT ( 'NONE',  ( 6.287037606400000200, 1493.763477428889928, 218.4859723337289950 ) ) ;
#43220 = CARTESIAN_POINT ( 'NONE',  ( -21.09588753150000073, 1379.716440018399908, 209.7902992619769975 ) ) ;
#43221 = CARTESIAN_POINT ( 'NONE',  ( -15.78501546999999938, 1473.845615658229917, 223.6172981401979882 ) ) ;
#43223 = DIRECTION ( 'NONE',  ( -1.755985294532469921E-16, 1.000000000000000000, -1.338183447452831989E-16 ) ) ;
#43222 = CARTESIAN_POINT ( 'NONE',  ( 17.87824514789999952, 1457.869968850630130, 229.1928660837979805 ) ) ;
#43224 = CARTESIAN_POINT ( 'NONE',  ( 15.57943184246149926, 1507.275788652510073, 225.6169562388830059 ) ) ;
#43225 = CARTESIAN_POINT ( 'NONE',  ( 12.16734073514860093, 1492.598615756489835, 211.2522116035209763 ) ) ;
#43226 = CARTESIAN_POINT ( 'NONE',  ( -5.796746189644780500, 1423.410246674609880, 91.23000440890038476 ) ) ;
#43227 = ORIENTED_EDGE ( 'NONE', *, *, #98682, .T. ) ;
#43228 = CIRCLE ( 'NONE', #9250, 1.999999999999998668 ) ;
#43229 = CARTESIAN_POINT ( 'NONE',  ( 18.06216501867849900, 1424.493447207169993, 224.2377043503520042 ) ) ;
#43230 = CARTESIAN_POINT ( 'NONE',  ( -18.15646965371467658, 1522.906363951597314, 180.0767137688672221 ) ) ;
#43231 = CARTESIAN_POINT ( 'NONE',  ( -2.944200527638781928, 1485.258749652005463, 183.0025506695369870 ) ) ;
#43232 = FACE_OUTER_BOUND ( 'NONE', #98246, .T. ) ;
#43234 = VERTEX_POINT ( 'NONE', #101767 ) ;
#43233 = CARTESIAN_POINT ( 'NONE',  ( -0.8282867551389770933, 1515.122054816080208, 204.7938966422100009 ) ) ;
#43235 = CARTESIAN_POINT ( 'NONE',  ( 0.9156123318609999950, 1507.627022993330229, 186.2283749853979771 ) ) ;
#43236 = CARTESIAN_POINT ( 'NONE',  ( -12.59650064061658981, 1416.818673809773827, 194.8446894363833906 ) ) ;
#43237 = CARTESIAN_POINT ( 'NONE',  ( -11.53336845399999966, 1429.132254792629965, 150.3949716609980101 ) ) ;
#43238 = CYLINDRICAL_SURFACE ( 'NONE', #18232, 13.00000000000000355 ) ;
#43239 = CARTESIAN_POINT ( 'NONE',  ( -3.665756889290000320, 1509.038615934189920, 213.6090957346689834 ) ) ;
#43240 = CARTESIAN_POINT ( 'NONE',  ( 16.90776328024010056, 1509.516719368900112, 233.6187669235270050 ) ) ;
#43241 = CARTESIAN_POINT ( 'NONE',  ( -1.336801414592336812, 1526.382868172864164, 239.5691425648093116 ) ) ;
#43242 = CARTESIAN_POINT ( 'NONE',  ( -15.99263756166499917, 1514.225267046429963, 224.1757580215669918 ) ) ;
#43243 = CARTESIAN_POINT ( 'NONE',  ( 13.85654454600000030, 1410.401893713229811, 228.0973156211979926 ) ) ;
#43245 = CARTESIAN_POINT ( 'NONE',  ( -10.37333465676420019, 1481.132217322410270, 207.0983991584610067 ) ) ;
#43244 = CARTESIAN_POINT ( 'NONE',  ( -109.5177468959999914, 1385.290589466009806, 297.1412373070589865 ) ) ;
#43246 = CARTESIAN_POINT ( 'NONE',  ( -12.79440631669999995, 1464.855048088789999, 225.0716344319989730 ) ) ;
#43247 = CARTESIAN_POINT ( 'NONE',  ( -5.788097265284999793, 1517.099836525840146, 206.6397780718770036 ) ) ;
#43248 = CARTESIAN_POINT ( 'NONE',  ( 30.02767535379999941, 1414.536195395429786, 266.6069031101980045 ) ) ;
#43249 = LINE ( 'NONE', #51646, #55407 ) ;
#43250 = CARTESIAN_POINT ( 'NONE',  ( 17.96041831760000207, 1430.310057063830072, 191.8733975052979872 ) ) ;
#43251 = CARTESIAN_POINT ( 'NONE',  ( 7.204249177822559247, 1506.516057208486473, 229.9648155173111945 ) ) ;
#43253 = B_SPLINE_CURVE_WITH_KNOTS ( 'NONE', 3,
 ( #69161, #103265, #52911, #60771 ),
 .UNSPECIFIED., .F., .F.,
 ( 4, 4 ),
 ( 0.000000000000000000, 0.0002220129587134788318 ),
 .UNSPECIFIED. ) ;
#43252 = CARTESIAN_POINT ( 'NONE',  ( -15.59069434664220211, 1418.231165713569908, 203.0305569057429693 ) ) ;
#43254 = CARTESIAN_POINT ( 'NONE',  ( -1.503967762139999831, 1452.143910241330104, 183.9258428494979682 ) ) ;
#43255 = CARTESIAN_POINT ( 'NONE',  ( -16.89233068642501934, 1526.349684470114653, 183.3465479968500631 ) ) ;
#43256 = CARTESIAN_POINT ( 'NONE',  ( -15.90345171279999903, 1418.061017481300269, 203.7331489593690037 ) ) ;
#43257 = CARTESIAN_POINT ( 'NONE',  ( -13.28024027740000079, 1444.654401305939928, 186.6935413929979859 ) ) ;
#43258 = CARTESIAN_POINT ( 'NONE',  ( -5.786158641081859955, 1484.802378851279855, 198.7188167466890150 ) ) ;
#43259 = CARTESIAN_POINT ( 'NONE',  ( 4.095224926770001161, 1416.176064121729951, 162.4091932246979866 ) ) ;
#43260 = CARTESIAN_POINT ( 'NONE',  ( -9.612987031380001213, 1499.623719321889894, 216.9466790759489925 ) ) ;
#43261 = VERTEX_POINT ( 'NONE', #69316 ) ;
#43262 = CARTESIAN_POINT ( 'NONE',  ( -2.258825589925000266, 1511.942942747529969, 201.5330432499970073 ) ) ;
#43263 = CARTESIAN_POINT ( 'NONE',  ( -13.31148314272640043, 1409.377907621740178, 202.3438456377509738 ) ) ;
#43264 = ADVANCED_FACE ( 'NONE', ( #43549 ), #26732, .T. ) ;
#43265 = CARTESIAN_POINT ( 'NONE',  ( -12.13242141250689876, 1508.441653837850026, 209.3107298190460028 ) ) ;
#43266 = CARTESIAN_POINT ( 'NONE',  ( -33.23571934791658578, 1511.187213306747708, 219.4842663281467026 ) ) ;
#43267 = VECTOR ( 'NONE', #84167, 999.9999999999998863 ) ;
#43268 = CARTESIAN_POINT ( 'NONE',  ( -23.65409152669999671, 1471.025497520530052, 267.0034733968980163 ) ) ;
#43269 = CARTESIAN_POINT ( 'NONE',  ( -7.500000019064999357, 1516.934643012909874, 209.1218459511669892 ) ) ;
#43270 = CARTESIAN_POINT ( 'NONE',  ( -14.81821971718517439, 1514.585417787315237, 192.8869359013385747 ) ) ;
#43271 = EDGE_CURVE ( 'NONE', #33967, #7065, #82098, .T. ) ;
#43272 = CARTESIAN_POINT ( 'NONE',  ( -20.12564951288307213, 1511.187213306747708, 180.7149624981946658 ) ) ;
#43273 = CARTESIAN_POINT ( 'NONE',  ( -78.73633071742699485, 1384.641256474020111, 302.9908934104659579 ) ) ;
#43274 = CARTESIAN_POINT ( 'NONE',  ( -26.53150723579640058, 1384.962365308560038, 203.8867581072389896 ) ) ;
#43275 = CYLINDRICAL_SURFACE ( 'NONE', #47909, 1.000000000000001110 ) ;
#43276 = CARTESIAN_POINT ( 'NONE',  ( 11.26466625542379951, 1415.020374538979922, 222.5877601533069878 ) ) ;
#43277 = CARTESIAN_POINT ( 'NONE',  ( 1.556370309037290012, 1414.996442620790276, 191.7142051069610034 ) ) ;
#43278 = CARTESIAN_POINT ( 'NONE',  ( -15.80168118454438542, 1415.804992922690644, 209.5032348057993090 ) ) ;
#43279 = CARTESIAN_POINT ( 'NONE',  ( -1.581901184577762409, 1426.946688134061105, 137.0999999980979567 ) ) ;
#43280 = CARTESIAN_POINT ( 'NONE',  ( -21.87473849839999929, 1409.676943088129974, 205.8784099853780276 ) ) ;
#43281 = CARTESIAN_POINT ( 'NONE',  ( 16.47341461499999937, 1414.971287085330005, 206.4938333208580161 ) ) ;
#43282 = CIRCLE ( 'NONE', #84348, 1.000000000000000888 ) ;
#43283 = CARTESIAN_POINT ( 'NONE',  ( 16.66231036550703593, 1523.604703353109699, 180.4882076302513099 ) ) ;
#43284 = EDGE_CURVE ( 'NONE', #2813, #35962, #30040, .T. ) ;
#43285 = B_SPLINE_CURVE_WITH_KNOTS ( 'NONE', 5,
 ( #40733, #93330, #16058, #16593, #75989, #74363, #58649, #41290, #65962, #84390, #6583, #25010 ),
 .UNSPECIFIED., .F., .F.,
 ( 6, 3, 3, 6 ),
 ( 0.000000000000000000, 0.4382291140948913477, 0.7277099922235745755, 1.000000000000000000 ),
 .UNSPECIFIED. ) ;
#43286 = LINE ( 'NONE', #77976, #26505 ) ;
#43287 = CARTESIAN_POINT ( 'NONE',  ( 1.657615632539999773, 1440.444625599219989, 150.6406752848980091 ) ) ;
#43288 = CARTESIAN_POINT ( 'NONE',  ( 11.27337545052449919, 1433.557891923710031, 225.8166880305549853 ) ) ;
#43289 = CARTESIAN_POINT ( 'NONE',  ( 17.44952998132189848, 1525.163457223744217, 181.0033690456834847 ) ) ;
#43290 = CARTESIAN_POINT ( 'NONE',  ( 5.076283890887699712, 1469.790178735639984, 187.8425608536880134 ) ) ;
#43292 = CARTESIAN_POINT ( 'NONE',  ( -8.755267316439999448, 1383.867798405919984, 200.0220800673290000 ) ) ;
#43291 = CARTESIAN_POINT ( 'NONE',  ( -22.43804543029999721, 1409.696614199630176, 210.2088496164680009 ) ) ;
#43293 = CARTESIAN_POINT ( 'NONE',  ( 11.73043893254989989, 1426.700124572799950, 143.6977314769600014 ) ) ;
#43294 = CARTESIAN_POINT ( 'NONE',  ( 9.716708914843909639, 1436.182072645820199, 210.6488788081859980 ) ) ;
#43295 = CARTESIAN_POINT ( 'NONE',  ( -10.62228157299999864, 1490.415513672490079, 212.3812309668689977 ) ) ;
#43296 = CARTESIAN_POINT ( 'NONE',  ( 9.522150312267969596, 1450.466928359630174, 204.8643194434029908 ) ) ;
#43297 = CARTESIAN_POINT ( 'NONE',  ( -0.3400762940194579920, 1420.320061791650005, 183.9482503623439982 ) ) ;
#43298 = CARTESIAN_POINT ( 'NONE',  ( -5.782749439735000330, 1516.858301627840092, 203.3453548368569841 ) ) ;
#43299 = CARTESIAN_POINT ( 'NONE',  ( 2.522951803030079727E-08, 1397.914279477030050, 222.1218461579910297 ) ) ;
#43300 = CARTESIAN_POINT ( 'NONE',  ( 0.4558763517165467793, 1414.913060387330006, 193.0031710580974504 ) ) ;
#43301 = CARTESIAN_POINT ( 'NONE',  ( -18.32982102970000327, 1430.286950519430093, 194.1997649584980081 ) ) ;
#43302 = VECTOR ( 'NONE', #1642, 1000.000000000000000 ) ;
#43303 = CARTESIAN_POINT ( 'NONE',  ( 7.252896346444960507, 1505.517465422420173, 218.2988040474139950 ) ) ;
#43304 = CARTESIAN_POINT ( 'NONE',  ( 40.96767724775679653, 1447.290420510560125, 135.1833091849670154 ) ) ;
#43306 = VERTEX_POINT ( 'NONE', #28955 ) ;
#43305 = CARTESIAN_POINT ( 'NONE',  ( -60.17131492770970169, 1379.724567624519977, 265.9736432342079411 ) ) ;
#43307 = VERTEX_POINT ( 'NONE', #97792 ) ;
#43308 = CARTESIAN_POINT ( 'NONE',  ( 11.42758288567859992, 1434.038670268820169, 151.4105907050079907 ) ) ;
#43309 = CARTESIAN_POINT ( 'NONE',  ( 26.35467955869999912, 1507.985761560129959, 216.6977068428279836 ) ) ;
#43310 = ORIENTED_EDGE ( 'NONE', *, *, #14876, .T. ) ;
#43311 = CARTESIAN_POINT ( 'NONE',  ( -0.0002568563788362631089, 1396.632929649832704, 221.6694727126995303 ) ) ;
#43312 = EDGE_CURVE ( 'NONE', #86829, #69095, #32835, .T. ) ;
#43313 = CARTESIAN_POINT ( 'NONE',  ( -10.36555841800240074, 1448.133745289950184, 208.8105289421490056 ) ) ;
#43314 = FACE_OUTER_BOUND ( 'NONE', #60348, .T. ) ;
#43316 = CARTESIAN_POINT ( 'NONE',  ( 2.244413413239999766, 1428.081157166129969, 101.8807690336980016 ) ) ;
#43315 = DIRECTION ( 'NONE',  ( -0.04204747460233849293, 7.723995777597519186E-18, -0.9991156138703697343 ) ) ;
#43317 = CARTESIAN_POINT ( 'NONE',  ( 18.40075938393449917, 1498.113744106350168, 229.7466415152620129 ) ) ;
#43318 = AXIS2_PLACEMENT_3D ( 'NONE', #110479, #99855, #109934 ) ;
#43319 = EDGE_CURVE ( 'NONE', #85956, #92642, #89116, .T. ) ;
#43320 = B_SPLINE_CURVE_WITH_KNOTS ( 'NONE', 3,
 ( #7271, #24591, #58238, #25701 ),
 .UNSPECIFIED., .F., .F.,
 ( 4, 4 ),
 ( 0.000000000000000000, 1.000000000000000000 ),
 .UNSPECIFIED. ) ;
#43321 = CARTESIAN_POINT ( 'NONE',  ( 5.737348681029999398, 1507.636265651229905, 182.1362798208980109 ) ) ;
#43322 = CARTESIAN_POINT ( 'NONE',  ( -0.2707600216260000470, 1415.088016306429836, 192.1592597442979979 ) ) ;
#43323 = CARTESIAN_POINT ( 'NONE',  ( 1.875672330807159893, 1456.514202357329850, 219.5762932319839820 ) ) ;
#43324 = CARTESIAN_POINT ( 'NONE',  ( 2.493699768634999536, 1516.858326417339867, 211.5985794462469869 ) ) ;
#43325 = CARTESIAN_POINT ( 'NONE',  ( 14.30888197748840085, 1416.029511585970113, 197.0047464494140286 ) ) ;
#43326 = CARTESIAN_POINT ( 'NONE',  ( 11.75825615539999980, 1431.471826025599967, 150.7534513679979966 ) ) ;
#43327 = CARTESIAN_POINT ( 'NONE',  ( 6.321172833974999961, 1513.830194289060273, 201.5514268169769991 ) ) ;
#43328 = EDGE_LOOP ( 'NONE', ( #44001, #28022, #76675, #58449, #70782 ) ) ;
#43329 = CARTESIAN_POINT ( 'NONE',  ( 13.86183822248450070, 1435.004851280240018, 148.8463810403530090 ) ) ;
#43330 = CARTESIAN_POINT ( 'NONE',  ( -0.1361343663501470291, 1432.257650919470052, 200.6952069693479928 ) ) ;
#43331 = ORIENTED_EDGE ( 'NONE', *, *, #81579, .T. ) ;
#43332 = ORIENTED_EDGE ( 'NONE', *, *, #10326, .T. ) ;
#43333 = EDGE_CURVE ( 'NONE', #1304, #7623, #3307, .T. ) ;
#43334 = CARTESIAN_POINT ( 'NONE',  ( 12.98442612396902796, 1444.885683142492098, 169.4237764324444697 ) ) ;
#43335 = CARTESIAN_POINT ( 'NONE',  ( -0.6059034394429999582, 1465.006891022829905, 237.7143252328980054 ) ) ;
#43336 = CARTESIAN_POINT ( 'NONE',  ( 21.14413832960000050, 1497.093652768289985, 210.1540944253389966 ) ) ;
#43337 = CARTESIAN_POINT ( 'NONE',  ( -4.616272334694999202, 1517.030858226499959, 216.4568033268070053 ) ) ;
#43338 = CARTESIAN_POINT ( 'NONE',  ( -8.220050563718016789, 1511.455710047913726, 213.1985981866891677 ) ) ;
#43339 = EDGE_CURVE ( 'NONE', #46370, #77278, #47539, .T. ) ;
#43340 = CARTESIAN_POINT ( 'NONE',  ( -18.98444801177922514, 1443.378814963748482, 211.6381416663761001 ) ) ;
#43341 = CARTESIAN_POINT ( 'NONE',  ( -48.76121443664156629, 1379.684058018070345, 237.2045636776436481 ) ) ;
#43342 = CARTESIAN_POINT ( 'NONE',  ( 4.987078416394999714, 1509.051704408389924, 209.1727295022979831 ) ) ;
#43343 = ORIENTED_EDGE ( 'NONE', *, *, #91070, .F. ) ;
#43344 = CARTESIAN_POINT ( 'NONE',  ( -5.012317106364999830, 1517.020727862619879, 206.2534121335969814 ) ) ;
#43345 = ORIENTED_EDGE ( 'NONE', *, *, #5496, .F. ) ;
#43346 = CARTESIAN_POINT ( 'NONE',  ( -104.5195930981980013, 1379.736861869120048, 305.0059150852220000 ) ) ;
#43347 = CARTESIAN_POINT ( 'NONE',  ( -19.63615623729999982, 1508.568590186330084, 229.6083364675979794 ) ) ;
#43348 = VERTEX_POINT ( 'NONE', #81532 ) ;
#43349 = CARTESIAN_POINT ( 'NONE',  ( -10.72453240200000124, 1409.287569311029984, 189.7722108729980164 ) ) ;
#43350 = CARTESIAN_POINT ( 'NONE',  ( 7.869278964325000736, 1514.500328598809801, 215.5039757893969750 ) ) ;
#43352 = ORIENTED_EDGE ( 'NONE', *, *, #78980, .T. ) ;
#43351 = CARTESIAN_POINT ( 'NONE',  ( -9.380124768717641004, 1428.163396101657781, 134.0999999980979851 ) ) ;
#43353 = CARTESIAN_POINT ( 'NONE',  ( 21.88686710819999703, 1430.321349793229956, 220.0073909120980034 ) ) ;
#43354 = CARTESIAN_POINT ( 'NONE',  ( -16.78006084555529753, 1508.551704408389924, 210.3901253742230040 ) ) ;
#43355 = EDGE_CURVE ( 'NONE', #36205, #61114, #83759, .T. ) ;
#43356 = CARTESIAN_POINT ( 'NONE',  ( -102.7392963879999996, 1384.315214695209761, 311.1957061252590506 ) ) ;
#43357 = CARTESIAN_POINT ( 'NONE',  ( 8.886207544592329199, 1432.346591521910113, 153.1913203755599966 ) ) ;
#43358 = LINE ( 'NONE', #18669, #25263 ) ;
#43359 = B_SPLINE_CURVE_WITH_KNOTS ( 'NONE', 5,
 ( #97762, #29451, #5921, #81498, #20483, #40067, #54693, #37871, #88819, #12105, #55795, #72056 ),
 .UNSPECIFIED., .F., .F.,
 ( 6, 3, 3, 6 ),
 ( 0.000000000000000000, 0.3179072520873084673, 0.5558626742919888786, 1.000000000000000000 ),
 .UNSPECIFIED. ) ;
#43360 = ADVANCED_FACE ( 'NONE', ( #92015 ), #60647, .T. ) ;
#43361 = CARTESIAN_POINT ( 'NONE',  ( 3.262264650305000124, 1516.633288330999903, 215.6694029015669969 ) ) ;
#43362 = CARTESIAN_POINT ( 'NONE',  ( -2.675466344130340346, 1429.100645368589994, 200.1409435021539878 ) ) ;
#43363 = CARTESIAN_POINT ( 'NONE',  ( -20.50902834189999879, 1508.364533681130069, 189.6819253274979928 ) ) ;
#43364 = CARTESIAN_POINT ( 'NONE',  ( -121.2674250099716460, 1379.886883438980021, 304.3447484988897145 ) ) ;
#43365 = CARTESIAN_POINT ( 'NONE',  ( 0.01323701367210150005, 1516.939658295650133, 211.6080660720070341 ) ) ;
#43366 = CARTESIAN_POINT ( 'NONE',  ( 14.22405166870000137, 1409.409775216930029, 192.8963038564980081 ) ) ;
#43367 = CARTESIAN_POINT ( 'NONE',  ( -18.45994912253222253, 1486.199205235777072, 188.8535768566627269 ) ) ;
#43369 = VERTEX_POINT ( 'NONE', #85817 ) ;
#43368 = CARTESIAN_POINT ( 'NONE',  ( -78.77145090140000150, 1390.626937550559887, 293.5766517498590247 ) ) ;
#43370 = CARTESIAN_POINT ( 'NONE',  ( -62.62830543184530541, 1385.053670896650146, 285.2368784993579993 ) ) ;
#43371 = CARTESIAN_POINT ( 'NONE',  ( 32.18003819369999974, 1459.550832481329962, 259.4131166698980451 ) ) ;
#43372 = CARTESIAN_POINT ( 'NONE',  ( 3.674421735066214278, 1450.449123075120724, 184.1280417905258560 ) ) ;
#43373 = FACE_OUTER_BOUND ( 'NONE', #79490, .T. ) ;
#43374 = CARTESIAN_POINT ( 'NONE',  ( -5.283213344790979704, 1507.787234078490201, 236.3252226269889888 ) ) ;
#43375 = CARTESIAN_POINT ( 'NONE',  ( -23.68747534799999954, 1447.176912900409889, 214.7820647780980039 ) ) ;
#43377 = CARTESIAN_POINT ( 'NONE',  ( 17.05553375226330104, 1409.525490177569964, 222.2504613337279977 ) ) ;
#43376 = CARTESIAN_POINT ( 'NONE',  ( -22.30075843119631429, 1411.051997994482235, 202.8314164432181030 ) ) ;
#43378 = CARTESIAN_POINT ( 'NONE',  ( -9.207810800643882132, 1450.012628189060251, 209.2145258953920006 ) ) ;
#43379 = CARTESIAN_POINT ( 'NONE',  ( -109.2945710968669886, 1382.750670875540209, 311.0281563818350037 ) ) ;
#43380 = ORIENTED_EDGE ( 'NONE', *, *, #180, .T. ) ;
#43381 = CARTESIAN_POINT ( 'NONE',  ( -7.720650173434999708, 1516.977993847330026, 203.3422188780170075 ) ) ;
#43382 = CARTESIAN_POINT ( 'NONE',  ( -10.60922226581860173, 1508.438309873620028, 218.5024624024570130 ) ) ;
#43383 = VECTOR ( 'NONE', #109612, 1000.000000000000000 ) ;
#43384 = CARTESIAN_POINT ( 'NONE',  ( 4.490619219238107362, 1508.909942010395071, 211.6097810847319920 ) ) ;
#43385 = CARTESIAN_POINT ( 'NONE',  ( 12.55190973179999858, 1425.728534340630176, 223.8561624606980160 ) ) ;
#43386 = CARTESIAN_POINT ( 'NONE',  ( 5.477776093029999238, 1439.067881875560033, 154.7441050454979745 ) ) ;
#43387 = DIRECTION ( 'NONE',  ( 0.000000000000000000, 0.000000000000000000, -1.000000000000000000 ) ) ;
#43388 = CARTESIAN_POINT ( 'NONE',  ( 18.72979941119999836, 1454.437773883689943, 204.5413093961989830 ) ) ;
#43389 = CARTESIAN_POINT ( 'NONE',  ( 33.30038288836900051, 1436.135148397250077, 136.3179756724720164 ) ) ;
#43390 = CARTESIAN_POINT ( 'NONE',  ( 36.46770289711280100, 1449.819842309009800, 136.2622417282709932 ) ) ;
#43391 = CARTESIAN_POINT ( 'NONE',  ( -45.63713141301216325, 1443.374874937930372, 268.9747502902704355 ) ) ;
#43392 = CARTESIAN_POINT ( 'NONE',  ( -2.521939269659999816, 1431.047916005589968, 201.1291089318189904 ) ) ;
#43393 = CARTESIAN_POINT ( 'NONE',  ( 10.67459791866189889, 1480.672717750939910, 209.7791954089520061 ) ) ;
#43394 = CARTESIAN_POINT ( 'NONE',  ( 19.02270174365926536, 1526.382868172864164, 185.3889643599916610 ) ) ;
#43395 = DIRECTION ( 'NONE',  ( -0.01484500364079610613, 0.5669078173018522460, 0.8236474686107853049 ) ) ;
#43396 = ORIENTED_EDGE ( 'NONE', *, *, #84896, .T. ) ;
#43397 = CARTESIAN_POINT ( 'NONE',  ( -36.99165393039999827, 1427.133824787629919, 268.3665355199980240 ) ) ;
#43398 = CARTESIAN_POINT ( 'NONE',  ( 11.87977127189999926, 1433.311038246140015, 146.7587715624979978 ) ) ;
#43399 = EDGE_CURVE ( 'NONE', #6621, #6510, #61754, .T. ) ;
#43400 = CARTESIAN_POINT ( 'NONE',  ( 2.070952440869999744, 1486.243875337790087, 198.1392447632989899 ) ) ;
#43401 = DIRECTION ( 'NONE',  ( 0.000000000000000000, -1.836970198721029688E-16, -1.000000000000000000 ) ) ;
#43402 = DIRECTION ( 'NONE',  ( 0.7074300732573280959, 0.02470400251971149874, -0.7063514732133270302 ) ) ;
#43404 = CYLINDRICAL_SURFACE ( 'NONE', #92842, 3.999999999999999112 ) ;
#43403 = CARTESIAN_POINT ( 'NONE',  ( 0.6370436997427018078, 1517.051704408389924, 200.3909606286928238 ) ) ;
#43405 = DIRECTION ( 'NONE',  ( -0.8642610224695990162, 0.000000000000000000, 0.5030436214085248769 ) ) ;
#43406 = CARTESIAN_POINT ( 'NONE',  ( 6.870966381969999759, 1425.576645473769986, 212.2423038635290027 ) ) ;
#43407 = CARTESIAN_POINT ( 'NONE',  ( -12.45123913023140005, 1384.883862109669963, 219.0084378725689760 ) ) ;
#43408 = LINE ( 'NONE', #77559, #32422 ) ;
#43409 = CARTESIAN_POINT ( 'NONE',  ( -37.90967934872600154, 1445.000095422659797, 137.0440870150139858 ) ) ;
#43410 = B_SPLINE_CURVE_WITH_KNOTS ( 'NONE', 3,
 ( #78899, #18394, #19511, #60442, #79442, #44187, #28481, #96795, #20065, #37984, #22244, #73238, #48036, #12214, #82174, #56442, #88928, #99512, #106283, #71632, #5474, #39058, #72166 ),
 .UNSPECIFIED., .F., .F.,
 ( 4, 2, 2, 1, 2, 2, 2, 2, 2, 2, 2, 4 ),
 ( 0.000000000000000000, 0.1249999999995614064, 0.1874999999993859079, 0.2187499999992296718, 0.2343749999991104338, 0.2499999999989912236, 0.3749999999990175081, 0.4374999999990306643, 0.4999999999990438759, 0.6249999999993142152, 0.7499999999995846656, 1.000000000000000000 ),
 .UNSPECIFIED. ) ;
#43411 = CARTESIAN_POINT ( 'NONE',  ( -16.78845670593169714, 1414.971513442450032, 208.7062368472520006 ) ) ;
#43412 = CARTESIAN_POINT ( 'NONE',  ( 24.40199393649999848, 1435.349635217629839, 136.1409814179979776 ) ) ;
#43413 = CARTESIAN_POINT ( 'NONE',  ( -13.40387510366765866, 1443.414769640762870, 169.3677538767024089 ) ) ;
#43414 = VERTEX_POINT ( 'NONE', #27572 ) ;
#43415 = ADVANCED_FACE ( 'NONE', ( #69608 ), #8913, .T. ) ;
#43416 = CARTESIAN_POINT ( 'NONE',  ( -16.16280329491559797, 1409.477474777709858, 225.0536677993360115 ) ) ;
#43417 = CARTESIAN_POINT ( 'NONE',  ( -1.031112549849209969, 1488.425549442109968, 217.1473076880390067 ) ) ;
#43418 = ORIENTED_EDGE ( 'NONE', *, *, #5526, .T. ) ;
#43419 = ORIENTED_EDGE ( 'NONE', *, *, #1710, .T. ) ;
#43420 = LINE ( 'NONE', #69745, #23315 ) ;
#43421 = CARTESIAN_POINT ( 'NONE',  ( -15.28485084270191408, 1416.039222364684520, 206.5424821588011923 ) ) ;
#43423 = CARTESIAN_POINT ( 'NONE',  ( -3.056112608387090201, 1457.952188555200109, 219.3550834608830087 ) ) ;
#43422 = CARTESIAN_POINT ( 'NONE',  ( 1.776583262209999958, 1456.341123502790197, 219.1753798273990128 ) ) ;
#43424 = B_SPLINE_CURVE_WITH_KNOTS ( 'NONE', 5,
 ( #76162, #67232, #66683, #34156, #68342, #101328 ),
 .UNSPECIFIED., .F., .F.,
 ( 6, 6 ),
 ( 0.000000000000000000, 1.000000000000000000 ),
 .UNSPECIFIED. ) ;
#43425 = CARTESIAN_POINT ( 'NONE',  ( -11.80982523969999853, 1433.007417310889878, 150.5682162921980023 ) ) ;
#43426 = CARTESIAN_POINT ( 'NONE',  ( -109.9711626006150027, 1384.465720048490084, 311.4368156476579657 ) ) ;
#43427 = CARTESIAN_POINT ( 'NONE',  ( -0.7800921441517141286, 1526.382868172863937, 241.4567505818336031 ) ) ;
#43428 = CARTESIAN_POINT ( 'NONE',  ( -13.05162051250000133, 1467.538720777590015, 191.8992815354989716 ) ) ;
#43429 = CARTESIAN_POINT ( 'NONE',  ( -24.15268595891001979, 1411.115258066103024, 209.2894665055660823 ) ) ;
#43430 = CARTESIAN_POINT ( 'NONE',  ( 2.491648406910000002, 1449.120029875969976, 182.5880893073980076 ) ) ;
#43431 = CARTESIAN_POINT ( 'NONE',  ( 8.808881355756348341, 1364.900047799910453, 210.6218459617142003 ) ) ;
#43433 = ORIENTED_EDGE ( 'NONE', *, *, #78864, .F. ) ;
#43432 = CARTESIAN_POINT ( 'NONE',  ( 5.641423425050000162, 1453.485726096290136, 216.6286100207389893 ) ) ;
#43434 = ORIENTED_EDGE ( 'NONE', *, *, #86959, .F. ) ;
#43435 = CARTESIAN_POINT ( 'NONE',  ( -40.70885756149999679, 1444.085015817089925, 137.1037827856980016 ) ) ;
#43436 = CARTESIAN_POINT ( 'NONE',  ( 7.550704948200230859, 1510.491946830140705, 203.5278907278841700 ) ) ;
#43437 = CYLINDRICAL_SURFACE ( 'NONE', #49342, 2.000000000000001776 ) ;
#43438 = CARTESIAN_POINT ( 'NONE',  ( 10.92766316885620093, 1501.618323021010156, 205.6861136770480130 ) ) ;
#43439 = CARTESIAN_POINT ( 'NONE',  ( -3.520666757299999894, 1486.235012026530057, 181.9081341745979898 ) ) ;
#43440 = CARTESIAN_POINT ( 'NONE',  ( 20.12564951288265647, 1512.187213306747481, 180.7149624981944100 ) ) ;
#43441 = EDGE_CURVE ( 'NONE', #60672, #1788, #11338, .T. ) ;
#43442 = CARTESIAN_POINT ( 'NONE',  ( -8.629930135849999573, 1384.437861499620112, 199.9043374725989963 ) ) ;
#43443 = CARTESIAN_POINT ( 'NONE',  ( 21.74754144930000166, 1409.672501264029961, 207.1047251593579972 ) ) ;
#43444 =( LENGTH_UNIT ( ) NAMED_UNIT ( * ) SI_UNIT ( .MILLI., .METRE. ) );
#43445 = CARTESIAN_POINT ( 'NONE',  ( -22.94032544519359718, 1507.620489270479993, 207.7960379221760263 ) ) ;
#43446 = CARTESIAN_POINT ( 'NONE',  ( 9.353206833242573737, 1367.891569019600183, 207.6218459616987673 ) ) ;
#43447 = CARTESIAN_POINT ( 'NONE',  ( 14.46065478178650032, 1409.241212025219966, 204.2271823003410134 ) ) ;
#43448 = CARTESIAN_POINT ( 'NONE',  ( -8.363319336106780355, 1406.549798397139966, 266.9339146100829794 ) ) ;
#43449 = EDGE_CURVE ( 'NONE', #71455, #10257, #38174, .T. ) ;
#43450 = CARTESIAN_POINT ( 'NONE',  ( -14.40366254822449932, 1435.998939573110192, 149.9111377689429787 ) ) ;
#43451 = ORIENTED_EDGE ( 'NONE', *, *, #104822, .T. ) ;
#43452 = CARTESIAN_POINT ( 'NONE',  ( -11.86584295870000183, 1432.318020648750007, 149.9824182359980114 ) ) ;
#43453 = CARTESIAN_POINT ( 'NONE',  ( 13.44142854779999929, 1443.469795417129944, 187.9564574482980106 ) ) ;
#43454 = ORIENTED_EDGE ( 'NONE', *, *, #66582, .F. ) ;
#43455 = EDGE_LOOP ( 'NONE', ( #53817, #53392, #79784, #57830 ) ) ;
#43456 = EDGE_CURVE ( 'NONE', #36699, #40040, #30318, .T. ) ;
#43457 = CARTESIAN_POINT ( 'NONE',  ( -24.25895011704391990, 1512.187213306747481, 247.1119212070238405 ) ) ;
#43458 = CARTESIAN_POINT ( 'NONE',  ( -9.209502321770001387, 1366.683160837839978, 207.6218459616989946 ) ) ;
#43459 = CARTESIAN_POINT ( 'NONE',  ( 3.459156578084999989, 1516.769879638719885, 213.7318425517769924 ) ) ;
#43460 = CARTESIAN_POINT ( 'NONE',  ( -13.52062872760000012, 1485.480753740029968, 186.3238177837980061 ) ) ;
#43461 = EDGE_CURVE ( 'NONE', #81049, #13345, #42597, .T. ) ;
#43462 = VERTEX_POINT ( 'NONE', #63959 ) ;
#43463 = CARTESIAN_POINT ( 'NONE',  ( -105.7600639359999946, 1378.531805229619977, 302.0293825393590055 ) ) ;
#43464 = B_SPLINE_CURVE_WITH_KNOTS ( 'NONE', 3,
 ( #99708, #108680, #98069, #39827 ),
 .UNSPECIFIED., .F., .F.,
 ( 4, 4 ),
 ( 0.000000000000000000, 0.0002960034161023838636 ),
 .UNSPECIFIED. ) ;
#43465 = CARTESIAN_POINT ( 'NONE',  ( -106.5231981154489915, 1378.913060387289988, 301.8480351107359638 ) ) ;
#43466 = CARTESIAN_POINT ( 'NONE',  ( 3.257220602695000355, 1517.040132827679827, 203.3350082531769942 ) ) ;
#43467 = B_SPLINE_CURVE_WITH_KNOTS ( 'NONE', 3,
 ( #99047, #23985, #58727, #22327, #92308, #74440, #13383, #47570, #81695, #39146, #91214, #73322, #7758 ),
 .UNSPECIFIED., .F., .F.,
 ( 4, 2, 1, 1, 1, 2, 2, 4 ),
 ( 0.000000000000000000, 0.2499999999999759082, 0.3749999999999673039, 0.4374999999999629741, 0.4687499999999663602, 0.4843749999999606426, 0.4999999999999549249, 1.000000000000000000 ),
 .UNSPECIFIED. ) ;
#43468 = CARTESIAN_POINT ( 'NONE',  ( -27.71749578960000093, 1508.609859370430058, 205.9131467889379792 ) ) ;
#43469 = CARTESIAN_POINT ( 'NONE',  ( -7.683535681777359905, 1517.051704408389924, 208.6863461652989997 ) ) ;
#43470 = CARTESIAN_POINT ( 'NONE',  ( -68.71261127229999488, 1384.854887445129862, 263.4295281439590326 ) ) ;
#43471 = CARTESIAN_POINT ( 'NONE',  ( -56.07122076218969653, 1384.649968191290100, 235.9257209178720132 ) ) ;
#43472 = CARTESIAN_POINT ( 'NONE',  ( -3.870783063939999380, 1407.691700113030038, 196.5444094325980302 ) ) ;
#43473 = CARTESIAN_POINT ( 'NONE',  ( -13.04207607270000047, 1409.368499719529837, 225.9431834757980084 ) ) ;
#43475 = VERTEX_POINT ( 'NONE', #22439 ) ;
#43474 = CARTESIAN_POINT ( 'NONE',  ( -1.438891081339280120, 1452.191228260170192, 183.8587004481619829 ) ) ;
#43476 = EDGE_CURVE ( 'NONE', #80494, #86711, #104842, .T. ) ;
#43477 = CARTESIAN_POINT ( 'NONE',  ( 5.945307986799999611, 1451.422783942589831, 210.3535049228189848 ) ) ;
#43478 = CARTESIAN_POINT ( 'NONE',  ( 27.30475511630000085, 1508.128822474129947, 213.8345258920280116 ) ) ;
#43479 = CARTESIAN_POINT ( 'NONE',  ( 19.96891611054200055, 1487.423520469470077, 226.6552576108419998 ) ) ;
#43480 = CARTESIAN_POINT ( 'NONE',  ( -25.50352605559999830, 1436.178832785409895, 137.0488846515980015 ) ) ;
#43481 = APPLICATION_CONTEXT ( 'automotive_design' ) ;
#43482 = EDGE_CURVE ( 'NONE', #29531, #83952, #2957, .T. ) ;
#43483 = CARTESIAN_POINT ( 'NONE',  ( 7.337153768115000751, 1517.119374999550018, 212.3815752680669959 ) ) ;
#43484 = CARTESIAN_POINT ( 'NONE',  ( -68.47455138450000334, 1379.747378330220045, 279.4267273018589890 ) ) ;
#43485 = CARTESIAN_POINT ( 'NONE',  ( -14.79571947709999868, 1410.747178383630171, 226.7235372410980005 ) ) ;
#43486 = LINE ( 'NONE', #1482, #3868 ) ;
#43487 = CARTESIAN_POINT ( 'NONE',  ( -4.044319925355000400, 1517.073005577650065, 208.0013022344469960 ) ) ;
#43488 = EDGE_CURVE ( 'NONE', #23634, #88920, #77535, .T. ) ;
#43489 = ORIENTED_EDGE ( 'NONE', *, *, #94808, .F. ) ;
#43490 = DIRECTION ( 'NONE',  ( -2.191843104705535248E-06, -0.9999999999950412999, 2.261297895848575335E-06 ) ) ;
#43491 = CARTESIAN_POINT ( 'NONE',  ( 2.470168521978398424, 1523.382868172864164, 242.8787258963054683 ) ) ;
#43492 = CARTESIAN_POINT ( 'NONE',  ( -73.55347204870000155, 1384.772439966069896, 298.9553539304589549 ) ) ;
#43493 = ORIENTED_EDGE ( 'NONE', *, *, #83137, .T. ) ;
#43494 = CARTESIAN_POINT ( 'NONE',  ( -8.106555885276549134, 1438.741351455190170, 205.9368832915250209 ) ) ;
#43495 = DIRECTION ( 'NONE',  ( 0.9996573249755517088, -0.02617694830808747070, 0.000000000000000000 ) ) ;
#43496 = CARTESIAN_POINT ( 'NONE',  ( 12.05521173712990013, 1435.480315805250029, 151.1576910952140054 ) ) ;
#43497 = CARTESIAN_POINT ( 'NONE',  ( 12.09098897718920007, 1459.298984292019895, 231.2999770925069924 ) ) ;
#43498 = CARTESIAN_POINT ( 'NONE',  ( 1.742626220133139947, 1466.605724716640225, 234.7106070719929960 ) ) ;
#43499 = CARTESIAN_POINT ( 'NONE',  ( -2.883410139480000023, 1409.181735915330137, 187.1726403038979925 ) ) ;
#43500 = CARTESIAN_POINT ( 'NONE',  ( 2.561313721290320089, 1430.951449648099924, 218.2616813023740008 ) ) ;
#43501 = CARTESIAN_POINT ( 'NONE',  ( 4.233744409028489919, 1441.501406244219879, 164.0921308226519955 ) ) ;
#43503 = CARTESIAN_POINT ( 'NONE',  ( -3.910864687060000122, 1421.809797752930081, 185.0240497693979762 ) ) ;
#43502 = CARTESIAN_POINT ( 'NONE',  ( -6.549762485114999144, 1516.729202374750002, 213.7405950387170037 ) ) ;
#43504 = CARTESIAN_POINT ( 'NONE',  ( 20.49660127010000110, 1509.524916156329937, 188.2007677697980057 ) ) ;
#43505 = CARTESIAN_POINT ( 'NONE',  ( -7.329303116114999739, 1516.857992118400034, 216.4524001036569985 ) ) ;
#43506 = EDGE_LOOP ( 'NONE', ( #105005, #31323, #62679 ) ) ;
#43507 = CARTESIAN_POINT ( 'NONE',  ( -12.86122366611309964, 1416.830086716310007, 196.3807296669870084 ) ) ;
#43508 = DIRECTION ( 'NONE',  ( -1.000000000000000000, 0.000000000000000000, 0.000000000000000000 ) ) ;
#43509 = EDGE_LOOP ( 'NONE', ( #58565, #16121, #28617, #14370, #99889, #46253 ) ) ;
#43510 = CARTESIAN_POINT ( 'NONE',  ( -114.2775825618903696, 1308.913060387289988, 303.7424204186547740 ) ) ;
#43511 =( BOUNDED_SURFACE ( )  B_SPLINE_SURFACE ( 1, 2, ( 
 ( #67091, #109084, #91712, #57588, #32895, #49182, #110168 ),
 ( #6608, #32365, #66547, #100649, #92262, #15533, #102849 ) ),
 .UNSPECIFIED., .F., .F., .F. ) 
 B_SPLINE_SURFACE_WITH_KNOTS ( ( 2, 2 ),
 ( 3, 2, 2, 3 ),
 ( -10000.00000000000000, 10000.00000000000000 ),
 ( 5.770213214421419323, 6.283185307179590673, 7.853981633974480125, 8.911805878012049931 ),
 .UNSPECIFIED. ) 
 GEOMETRIC_REPRESENTATION_ITEM ( )  RATIONAL_B_SPLINE_SURFACE ( (
 ( 0.8711730249286460115, 0.9043503954990910199, 1.000000000000000000, 0.7071067811865480168, 1.000000000000000000, 0.8027563838226849935, 0.8711730262222899812),
 ( 0.8711730249286460115, 0.9043503954990910199, 1.000000000000000000, 0.7071067811865480168, 1.000000000000000000, 0.8027563838226849935, 0.8711730262222899812) ) ) 
 REPRESENTATION_ITEM ( '' )  SURFACE ( )  );
#43512 = CARTESIAN_POINT ( 'NONE',  ( -21.56904447630000021, 1506.866154825289868, 209.3454515566180021 ) ) ;
#43513 = CARTESIAN_POINT ( 'NONE',  ( -113.4000000000000057, 1306.413060387289988, 304.2218459572590064 ) ) ;
#43514 = UNCERTAINTY_MEASURE_WITH_UNIT (LENGTH_MEASURE( 1.000000000000000082E-05 ), #45546, 'distance_accuracy_value', 'NONE');
#43515 = CARTESIAN_POINT ( 'NONE',  ( -2.826458050128489941, 1435.843485468609970, 222.4962428573750230 ) ) ;
#43516 = CARTESIAN_POINT ( 'NONE',  ( -31.47409394596237320, 1526.278758871497757, 199.6577681796610761 ) ) ;
#43517 = CARTESIAN_POINT ( 'NONE',  ( -3.637603509031002158, 1508.126921005884469, 220.7408464239917407 ) ) ;
#43518 = B_SPLINE_CURVE_WITH_KNOTS ( 'NONE', 3,
 ( #87245, #9429, #43593, #2168, #17239, #69923 ),
 .UNSPECIFIED., .F., .F.,
 ( 4, 2, 4 ),
 ( 0.000000000000000000, 0.5000000000000000000, 1.000000000000000000 ),
 .UNSPECIFIED. ) ;
#43519 = CARTESIAN_POINT ( 'NONE',  ( -3.148243355340000438, 1447.343022729889981, 154.4222316151980010 ) ) ;
#43520 = CARTESIAN_POINT ( 'NONE',  ( 19.18343150420380994, 1507.776529595233569, 229.7058341636958971 ) ) ;
#43521 = CARTESIAN_POINT ( 'NONE',  ( -6.785334565741740320, 1457.914568211761662, 215.8412113930604335 ) ) ;
#43522 = CARTESIAN_POINT ( 'NONE',  ( -27.43355922089999765, 1507.980920696130170, 210.8261541407979962 ) ) ;
#43523 = CARTESIAN_POINT ( 'NONE',  ( 17.38341196999999738, 1410.833858183129905, 192.4620098003979933 ) ) ;
#43525 = CARTESIAN_POINT ( 'NONE',  ( -3.054816033052110136, 1485.996906143959905, 182.1538611115439892 ) ) ;
#43524 = CARTESIAN_POINT ( 'NONE',  ( -10.16243888589800015, 1472.559490735430018, 209.8188024594959984 ) ) ;
#43526 = CARTESIAN_POINT ( 'NONE',  ( -3.250000000000000000, 1524.051704408389924, 209.1218459616989946 ) ) ;
#43527 = ORIENTED_EDGE ( 'NONE', *, *, #109539, .F. ) ;
#43528 = CARTESIAN_POINT ( 'NONE',  ( -8.356240136749999436, 1508.431981883589970, 219.3528788934989961 ) ) ;
#43529 = CARTESIAN_POINT ( 'NONE',  ( 26.10596347299999920, 1488.578367652129828, 206.7493494209179801 ) ) ;
#43530 = CARTESIAN_POINT ( 'NONE',  ( -27.92328169199999977, 1509.198544188530150, 210.7148123472180146 ) ) ;
#43531 = CARTESIAN_POINT ( 'NONE',  ( 9.651066088509999474, 1425.440658930580184, 195.4941615409990163 ) ) ;
#43532 = CARTESIAN_POINT ( 'NONE',  ( 5.145309177750649887, 1422.426130283250131, 194.5914460530619863 ) ) ;
#43533 = CARTESIAN_POINT ( 'NONE',  ( -11.39446592756109844, 1470.674086296440009, 209.5209556861319982 ) ) ;
#43534 = LINE ( 'NONE', #444, #45137 ) ;
#43535 = CARTESIAN_POINT ( 'NONE',  ( 20.33508558929999666, 1432.834457682990205, 214.7556889579689994 ) ) ;
#43536 = CARTESIAN_POINT ( 'NONE',  ( -65.85453692722450114, 1383.789513244699947, 289.6320689311420438 ) ) ;
#43537 = CARTESIAN_POINT ( 'NONE',  ( 21.07905887619999774, 1451.363990295029907, 144.5323817167979996 ) ) ;
#43538 = CARTESIAN_POINT ( 'NONE',  ( 3.835404308833624043, 1396.046995657106436, 216.1425064568209677 ) ) ;
#43539 = CARTESIAN_POINT ( 'NONE',  ( -1.458596267000419999, 1516.574598972179956, 201.4117590633649968 ) ) ;
#43541 = ORIENTED_EDGE ( 'NONE', *, *, #62860, .T. ) ;
#43540 = PLANE ( 'NONE',  #53287 ) ;
#43542 = CARTESIAN_POINT ( 'NONE',  ( -20.12564951288246107, 1512.187213306747481, 237.5287294252017603 ) ) ;
#43543 = CARTESIAN_POINT ( 'NONE',  ( -89.15684587290000707, 1384.835666735910081, 292.2581851215589950 ) ) ;
#43544 = CARTESIAN_POINT ( 'NONE',  ( 20.40137755018059806, 1509.563325793020113, 230.2999756913229987 ) ) ;
#43545 = VERTEX_POINT ( 'NONE', #12418 ) ;
#43546 = VERTEX_POINT ( 'NONE', #89676 ) ;
#43547 = CARTESIAN_POINT ( 'NONE',  ( 12.59782697949999886, 1446.921545761879770, 188.3055334180980083 ) ) ;
#43548 = LINE ( 'NONE', #50838, #52875 ) ;
#43549 = FACE_OUTER_BOUND ( 'NONE', #30098, .T. ) ;
#43551 = CARTESIAN_POINT ( 'NONE',  ( -27.41410062850000173, 1466.213783604629953, 262.1295771318979746 ) ) ;
#43550 = CARTESIAN_POINT ( 'NONE',  ( 18.06710007320000244, 1416.825245919329973, 208.8994639621759859 ) ) ;
#43552 = CARTESIAN_POINT ( 'NONE',  ( 8.626226792742770044, 1436.875340518389976, 208.7668036561229883 ) ) ;
#43553 = CARTESIAN_POINT ( 'NONE',  ( -108.4836655010000186, 1381.983168677669937, 297.9253098464590153 ) ) ;
#43554 = DIRECTION ( 'NONE',  ( 0.8775825618903700942, 0.000000000000000000, -0.4794255386042075018 ) ) ;
#43555 = DIRECTION ( 'NONE',  ( -0.8826905754104281687, -0.3875151742776350439, -0.2658746655591340269 ) ) ;
#43556 = CARTESIAN_POINT ( 'NONE',  ( 2.214595992090000021, 1409.158101833729916, 186.0729899510980090 ) ) ;
#43557 = CARTESIAN_POINT ( 'NONE',  ( 12.78776258891489981, 1416.851343896290018, 222.2791104166909975 ) ) ;
#43558 = CARTESIAN_POINT ( 'NONE',  ( -8.251909913180000444, 1439.861448988760003, 153.7181667749979965 ) ) ;
#43559 = CARTESIAN_POINT ( 'NONE',  ( 11.39453196610000063, 1435.362097760900042, 151.5417152564980086 ) ) ;
#43560 = CARTESIAN_POINT ( 'NONE',  ( -12.25922289946369936, 1422.754725847070176, 204.0266690164509953 ) ) ;
#43561 = CARTESIAN_POINT ( 'NONE',  ( -23.70762051470000031, 1451.657018865829968, 140.3727388198980179 ) ) ;
#43562 = CARTESIAN_POINT ( 'NONE',  ( 0.1446574667840000161, 1466.770087014230057, 235.6259499557980064 ) ) ;
#43563 = ORIENTED_EDGE ( 'NONE', *, *, #60673, .T. ) ;
#43564 = CARTESIAN_POINT ( 'NONE',  ( -2.487922401834420594, 1508.551704408489968, 213.9544572570970047 ) ) ;
#43565 = CARTESIAN_POINT ( 'NONE',  ( 22.20352485945739929, 1475.168806475580141, 209.9014948442749926 ) ) ;
#43566 = CARTESIAN_POINT ( 'NONE',  ( -43.35450150260000157, 1444.057287291979947, 270.3367522392980504 ) ) ;
#43567 = DIRECTION ( 'NONE',  ( -1.000000000000000000, 0.000000000000000000, 0.000000000000000000 ) ) ;
#43568 = CARTESIAN_POINT ( 'NONE',  ( 3.240637488290000423, 1434.541222282480021, 155.4779008716980115 ) ) ;
#43569 = CARTESIAN_POINT ( 'NONE',  ( -8.862056518773441027, 1384.892951007370129, 218.6851137863439760 ) ) ;
#43570 = CARTESIAN_POINT ( 'NONE',  ( 11.73230603450000054, 1475.513060387329915, 191.9145371412979841 ) ) ;
#43571 = EDGE_CURVE ( 'NONE', #104547, #38215, #26533, .T. ) ;
#43572 = CARTESIAN_POINT ( 'NONE',  ( -19.97968237250000101, 1483.906011188890034, 214.0068283976289933 ) ) ;
#43573 = CARTESIAN_POINT ( 'NONE',  ( -1.121465867070000177, 1416.819756528530206, 228.0845568296979877 ) ) ;
#43574 = CARTESIAN_POINT ( 'NONE',  ( -2.999143295649999708, 1416.435214488830070, 232.8852738930980024 ) ) ;
#43575 = CARTESIAN_POINT ( 'NONE',  ( -106.2139324000000045, 1390.828638221579922, 307.6609436900590140 ) ) ;
#43576 = CARTESIAN_POINT ( 'NONE',  ( -0.9196686337267430122, 1485.046405773928882, 182.0632183934076807 ) ) ;
#43577 = CARTESIAN_POINT ( 'NONE',  ( -4.337097717182941459, 1358.915629873471289, 208.3718459617010978 ) ) ;
#43578 = CARTESIAN_POINT ( 'NONE',  ( -45.55790118172819803, 1438.878221330320002, 268.9770245028310001 ) ) ;
#43579 = CARTESIAN_POINT ( 'NONE',  ( -4.150360165000000379, 1431.492714444460034, 185.8659833644979926 ) ) ;
#43580 = CARTESIAN_POINT ( 'NONE',  ( -8.403628046679999741, 1423.510048004620103, 210.2177463927289978 ) ) ;
#43581 = CIRCLE ( 'NONE', #106157, 1.999999999999999556 ) ;
#43582 = ORIENTED_EDGE ( 'NONE', *, *, #4893, .T. ) ;
#43583 = CARTESIAN_POINT ( 'NONE',  ( 4.623892060624999800, 1517.066898074209803, 209.8584071487349831 ) ) ;
#43584 = DIRECTION ( 'NONE',  ( 0.1402804634202828582, -0.9901118076169937998, 0.000000000000000000 ) ) ;
#43585 = CARTESIAN_POINT ( 'NONE',  ( -26.75392516979539792, 1441.320991203599988, 137.5422828455679962 ) ) ;
#43586 = CARTESIAN_POINT ( 'NONE',  ( 7.531010940995349401, 1425.504834242530023, 212.1895840461209843 ) ) ;
#43587 = CARTESIAN_POINT ( 'NONE',  ( -25.79053548221810388, 1451.562458167700015, 136.3675287681099917 ) ) ;
#43588 = ORIENTED_EDGE ( 'NONE', *, *, #50906, .F. ) ;
#43589 = EDGE_CURVE ( 'NONE', #2493, #2466, #70180, .T. ) ;
#43590 = CARTESIAN_POINT ( 'NONE',  ( -15.08937679799999998, 1488.812149332929721, 194.1581390134980154 ) ) ;
#43592 = CARTESIAN_POINT ( 'NONE',  ( 13.72746433319999859, 1452.819461535329992, 195.0715466040980175 ) ) ;
#43591 = CARTESIAN_POINT ( 'NONE',  ( -3.351183042480982976, 1524.075000532256581, 176.2264671304546368 ) ) ;
#43593 = CARTESIAN_POINT ( 'NONE',  ( 6.375244903274786878, 1427.171875868285724, 214.3396874122583711 ) ) ;
#43594 = CARTESIAN_POINT ( 'NONE',  ( -18.95466419752950316, 1508.523044920219718, 209.9298748376089918 ) ) ;
#43595 = CARTESIAN_POINT ( 'NONE',  ( -23.43613533817220329, 1452.094652507430055, 137.8989582699280163 ) ) ;
#43596 = DIRECTION ( 'NONE',  ( 0.9455185755993178454, 0.000000000000000000, -0.3255681544571537578 ) ) ;
#43597 = VERTEX_POINT ( 'NONE', #80186 ) ;
#43598 = CARTESIAN_POINT ( 'NONE',  ( -0.5924040333921269941, 1410.239981589289982, 269.6149254805689566 ) ) ;
#43599 = CARTESIAN_POINT ( 'NONE',  ( 3.449647440015000122, 1516.829948096479939, 208.3645479958780129 ) ) ;
#43600 = CARTESIAN_POINT ( 'NONE',  ( 8.991145853091611073, 1419.232555150580083, 232.5600238179060000 ) ) ;
#43601 = FACE_OUTER_BOUND ( 'NONE', #36306, .T. ) ;
#43603 = VERTEX_POINT ( 'NONE', #47688 ) ;
#43602 = CARTESIAN_POINT ( 'NONE',  ( -4.517103279549999684, 1368.953374755989898, 207.6218459616989946 ) ) ;
#43604 = EDGE_LOOP ( 'NONE', ( #90192, #109547, #105668 ) ) ;
#43605 = CARTESIAN_POINT ( 'NONE',  ( -30.51231035492510557, 1526.382868172863937, 218.1578534183722979 ) ) ;
#43606 = CARTESIAN_POINT ( 'NONE',  ( -0.2484258432390819560, 1408.921735608980043, 186.5246867112969937 ) ) ;
#43607 = CARTESIAN_POINT ( 'NONE',  ( 3.827327165375219664, 1424.046157828239984, 183.3886487722830054 ) ) ;
#43608 = CARTESIAN_POINT ( 'NONE',  ( -11.44291537990000052, 1428.994970000029980, 123.0297916884979941 ) ) ;
#43609 = EDGE_CURVE ( 'NONE', #68294, #85474, #49808, .T. ) ;
#43610 = CARTESIAN_POINT ( 'NONE',  ( -20.94637264616769556, 1505.073634949130110, 192.2640080708209780 ) ) ;
#43611 = CARTESIAN_POINT ( 'NONE',  ( -19.18810533770000148, 1425.814069711829916, 223.9739304577979908 ) ) ;
#43612 = CARTESIAN_POINT ( 'NONE',  ( 38.95530193960379961, 1459.246772374329794, 268.9606472942739970 ) ) ;
#43613 = B_SPLINE_CURVE_WITH_KNOTS ( 'NONE', 5,
 ( #82714, #88908, #30089, #89460, #4896, #91109 ),
 .UNSPECIFIED., .F., .F.,
 ( 6, 6 ),
 ( 172.3296575809999922, 177.0697656899999970 ),
 .UNSPECIFIED. ) ;
#43614 = CARTESIAN_POINT ( 'NONE',  ( -4.019478480316913682, 1466.624674277336908, 234.7461397303189869 ) ) ;
#43615 = CARTESIAN_POINT ( 'NONE',  ( -4.734430706410000411, 1428.274085907389917, 201.8092844071990157 ) ) ;
#43616 = CARTESIAN_POINT ( 'NONE',  ( 7.710285837685000310, 1516.582197289609894, 205.8614676770269796 ) ) ;
#43617 = EDGE_CURVE ( 'NONE', #26609, #98841, #34027, .T. ) ;
#43618 = VERTEX_POINT ( 'NONE', #108684 ) ;
#43619 = CARTESIAN_POINT ( 'NONE',  ( -14.03764155707720107, 1452.555513769060099, 223.0320990030590167 ) ) ;
#43620 = CARTESIAN_POINT ( 'NONE',  ( -5.761714458496140168, 1516.919864955513731, 204.2610115332772409 ) ) ;
#43621 = CARTESIAN_POINT ( 'NONE',  ( 23.71139080889999917, 1410.394892077029908, 208.2669468599999902 ) ) ;
#43622 = ORIENTED_EDGE ( 'NONE', *, *, #41452, .F. ) ;
#43623 = CARTESIAN_POINT ( 'NONE',  ( -0.5805478584864469660, 1457.956445091640035, 229.5817085807559863 ) ) ;
#43624 = CARTESIAN_POINT ( 'NONE',  ( 25.09476263457070289, 1451.973863162750149, 136.0431116258349959 ) ) ;
#43625 = CARTESIAN_POINT ( 'NONE',  ( -3.704457720420359923, 1508.551704408389924, 213.7941704926340094 ) ) ;
#43626 = CARTESIAN_POINT ( 'NONE',  ( -4.265932623502749891E-16, 1391.052076539619975, 208.7094039267549874 ) ) ;
#43627 = CARTESIAN_POINT ( 'NONE',  ( 7.472825078389999653, 1423.077329920680086, 195.6326666296990027 ) ) ;
#43628 = CARTESIAN_POINT ( 'NONE',  ( 17.53538859780000081, 1410.022483724830181, 193.0866497752979853 ) ) ;
#43629 = CARTESIAN_POINT ( 'NONE',  ( 20.24673233129999872, 1444.324653571829913, 162.1129423953979938 ) ) ;
#43630 = LINE ( 'NONE', #28480, #67853 ) ;
#43632 = CARTESIAN_POINT ( 'NONE',  ( -18.99019980698101051, 1424.920940954418484, 224.2460923394500867 ) ) ;
#43631 = CARTESIAN_POINT ( 'NONE',  ( 31.32995031131189378, 1523.678648413191922, 196.3423562208913324 ) ) ;
#43633 = CARTESIAN_POINT ( 'NONE',  ( 0.9973831003862488886, 1450.902295810800069, 182.0851543307630038 ) ) ;
#43634 = CARTESIAN_POINT ( 'NONE',  ( 18.77802067605560055, 1476.445422708370188, 228.3675973292809829 ) ) ;
#43635 = CARTESIAN_POINT ( 'NONE',  ( -9.949232747880000005, 1381.968568543130004, 217.5033713529390127 ) ) ;
#43636 = ORIENTED_EDGE ( 'NONE', *, *, #88550, .F. ) ;
#43637 = CARTESIAN_POINT ( 'NONE',  ( 11.57735155927789883, 1414.971513442450032, 221.2869575672650058 ) ) ;
#43638 = CARTESIAN_POINT ( 'NONE',  ( 11.65870934109939938, 1432.338283370469981, 150.9211944259870108 ) ) ;
#43639 = SPHERICAL_SURFACE ( 'NONE', #67798, 2.000000000000000000 ) ;
#43640 = CARTESIAN_POINT ( 'NONE',  ( -11.15555666070000029, 1388.626024522959824, 202.3683382543690072 ) ) ;
#43641 = CARTESIAN_POINT ( 'NONE',  ( 0.6255730392936860174, 1421.220699880276015, 193.7286507490917415 ) ) ;
#43642 = DIRECTION ( 'NONE',  ( 0.6456624059335341892, -0.004098122786874927245, -0.7636119845535058737 ) ) ;
#43643 = CARTESIAN_POINT ( 'NONE',  ( -11.06589456340000055, 1457.157324861229881, 234.3916895958979865 ) ) ;
#43644 = CARTESIAN_POINT ( 'NONE',  ( -29.30029655192939586, 1525.907212628473872, 196.8717316207790589 ) ) ;
#43645 = CARTESIAN_POINT ( 'NONE',  ( 11.46353857769999962, 1433.470779071320067, 151.3229031972979897 ) ) ;
#43646 = CARTESIAN_POINT ( 'NONE',  ( 14.97660096209999914, 1451.660971648529767, 219.6133834379979817 ) ) ;
#43647 = CARTESIAN_POINT ( 'NONE',  ( 12.57270521885200054, 1416.218865267220053, 196.2615492320400108 ) ) ;
#43648 =( BOUNDED_CURVE ( )  B_SPLINE_CURVE ( 3, ( #61286, #105460, #62954, #52864 ),
 .UNSPECIFIED., .F., .T. ) 
 B_SPLINE_CURVE_WITH_KNOTS ( ( 4, 4 ),
 ( 6.031750469185639396, 6.430154089112100735 ),
 .UNSPECIFIED. ) 
 CURVE ( )  GEOMETRIC_REPRESENTATION_ITEM ( )  RATIONAL_B_SPLINE_CURVE ( ( 1.000000000000000000, 0.9868165610007129107, 0.9868165610007129107, 1.000000000000000000 ) ) 
 REPRESENTATION_ITEM ( '' )  );
#43649 = CARTESIAN_POINT ( 'NONE',  ( -17.71128632129999758, 1420.275165550689962, 207.4128878226090080 ) ) ;
#43650 = CARTESIAN_POINT ( 'NONE',  ( 11.09566315855570018, 1425.086810962289974, 203.0248004916680031 ) ) ;
#43651 = CIRCLE ( 'NONE', #77623, 1.999999999999999556 ) ;
#43652 = CARTESIAN_POINT ( 'NONE',  ( 9.774680401711808742, 1462.791281439700242, 210.7173239812339887 ) ) ;
#43653 = CARTESIAN_POINT ( 'NONE',  ( 22.69544225309999774, 1409.705575941829920, 209.0104250642420141 ) ) ;
#43654 = CARTESIAN_POINT ( 'NONE',  ( 9.382156933674025368, 1398.191381926702661, 200.1155936601079190 ) ) ;
#43655 = CARTESIAN_POINT ( 'NONE',  ( 1.742626186960000156, 1466.605724540429947, 234.7106070974979843 ) ) ;
#43656 = CARTESIAN_POINT ( 'NONE',  ( 25.71796661899999847, 1449.805629472589999, 209.6503985265360086 ) ) ;
#43657 = AXIS2_PLACEMENT_3D ( 'NONE', #71820, #37065, #71260 ) ;
#43658 = CARTESIAN_POINT ( 'NONE',  ( -0.001293896702980919895, 1473.458796427790048, 216.6124729060890104 ) ) ;
#43659 = CARTESIAN_POINT ( 'NONE',  ( -21.62164173379369814, 1519.551704408389924, 210.2163513719069954 ) ) ;
#43660 = CARTESIAN_POINT ( 'NONE',  ( -12.94530514837170010, 1383.860467683670095, 218.9034580252159969 ) ) ;
#43661 = CARTESIAN_POINT ( 'NONE',  ( -0.03315910861134309384, 1502.038559631680073, 233.2541124739660177 ) ) ;
#43662 = CARTESIAN_POINT ( 'NONE',  ( -4.028630622785000170, 1516.812923327049930, 212.5819478221170016 ) ) ;
#43663 = CARTESIAN_POINT ( 'NONE',  ( -16.21109120713730078, 1420.416353679290069, 206.3072091156649890 ) ) ;
#43664 = CARTESIAN_POINT ( 'NONE',  ( 9.105494218695110220, 1451.204579960250157, 210.7726874829440078 ) ) ;
#43666 = ORIENTED_EDGE ( 'NONE', *, *, #9075, .T. ) ;
#43665 = CARTESIAN_POINT ( 'NONE',  ( 3.533229526830000022, 1442.898285365590027, 217.2834840181990046 ) ) ;
#43667 = CARTESIAN_POINT ( 'NONE',  ( 16.37730527473435060, 1414.913060387329779, 210.1804486578982676 ) ) ;
#43668 = B_SPLINE_CURVE_WITH_KNOTS ( 'NONE', 5,
 ( #1826, #29208, #78515, #71809, #79081, #96975 ),
 .UNSPECIFIED., .F., .F.,
 ( 6, 6 ),
 ( 0.000000000000000000, 1.000000000000000000 ),
 .UNSPECIFIED. ) ;
#43669 = CARTESIAN_POINT ( 'NONE',  ( -9.851472566700000044, 1384.510545767029953, 199.8981574268189831 ) ) ;
#43670 = CARTESIAN_POINT ( 'NONE',  ( -4.796874865469999527, 1476.201330746690019, 199.9539643786289957 ) ) ;
#43671 = CARTESIAN_POINT ( 'NONE',  ( -36.14177852645050137, 1451.331926750479852, 134.0999999986410103 ) ) ;
#43672 = CARTESIAN_POINT ( 'NONE',  ( -6.168107933492159134, 1508.551704408389924, 219.3995182160069817 ) ) ;
#43673 = VERTEX_POINT ( 'NONE', #33070 ) ;
#43674 = B_SPLINE_SURFACE_WITH_KNOTS ( 'NONE', 5, 5, ( 
 ( #31596, #13124, #64685, #48981, #47308, #65774 ),
 ( #22064, #81431, #99891, #23189, #91515, #12604 ),
 ( #64130, #98251, #83114, #6408, #40554, #89308 ),
 ( #46782, #90390, #80913, #21521, #55733, #38885 ),
 ( #73066, #6948, #83654, #66887, #57929, #92061 ),
 ( #49529, #41105, #25940, #92601, #16427, #109973 ) ),
 .UNSPECIFIED., .F., .F., .F.,
 ( 6, 6 ),
 ( 6, 6 ),
 ( 37.80270741440000393, 108.0413671919999956 ),
 ( -3.367982578744440036E-05, 2.000002141449999993 ),
 .UNSPECIFIED. ) ;
#43675 = CARTESIAN_POINT ( 'NONE',  ( -4.987078426973329925, 1508.551704408389924, 206.6339106789369851 ) ) ;
#43676 = CARTESIAN_POINT ( 'NONE',  ( -11.89318647318120092, 1391.758398471429928, 212.5295707731389996 ) ) ;
#43677 = CARTESIAN_POINT ( 'NONE',  ( -13.49734247349999983, 1415.088275290130014, 220.8629234729979771 ) ) ;
#43678 = CARTESIAN_POINT ( 'NONE',  ( 11.59870872757815086, 1426.255586768791318, 138.4426008133268908 ) ) ;
#43679 = CARTESIAN_POINT ( 'NONE',  ( 4.478041536509679510, 1465.868555709299926, 203.7095503217849739 ) ) ;
#43680 = CARTESIAN_POINT ( 'NONE',  ( -107.8451728718519718, 1380.542607501936118, 309.8189202647981233 ) ) ;
#43681 = PLANE ( 'NONE',  #19089 ) ;
#43682 = CARTESIAN_POINT ( 'NONE',  ( -12.91238682329999854, 1379.507757257049889, 211.2365369345390036 ) ) ;
#43683 = CARTESIAN_POINT ( 'NONE',  ( -12.30988125380000042, 1391.742651319489823, 209.2308626440040200 ) ) ;
#43684 = CARTESIAN_POINT ( 'NONE',  ( -79.74802494709490475, 1385.156543383609915, 282.7772545974189597 ) ) ;
#43685 = CARTESIAN_POINT ( 'NONE',  ( -17.59962683420000218, 1413.995480048929949, 192.5357147007979961 ) ) ;
#43686 = CARTESIAN_POINT ( 'NONE',  ( -19.04120737539122388, 1379.714756628304485, 209.1757808297589918 ) ) ;
#43687 = EDGE_LOOP ( 'NONE', ( #11977, #48517, #58163, #44579 ) ) ;
#43688 = CARTESIAN_POINT ( 'NONE',  ( 12.94068535313422430, 1442.831169986190616, 169.4787936161906430 ) ) ;
#43690 = VERTEX_POINT ( 'NONE', #76189 ) ;
#43689 = CARTESIAN_POINT ( 'NONE',  ( 3.028503249993359958, 1440.533662647540041, 157.2362874162160153 ) ) ;
#43691 = DIRECTION ( 'NONE',  ( -0.5877852522924629231, 0.000000000000000000, 0.8090169943749548898 ) ) ;
#43692 = ORIENTED_EDGE ( 'NONE', *, *, #4362, .T. ) ;
#43693 = CARTESIAN_POINT ( 'NONE',  ( 26.35476029009999976, 1507.985741737729995, 216.6974866551179844 ) ) ;
#43694 = CARTESIAN_POINT ( 'NONE',  ( -6.729522994862413121, 1363.632850206206285, 208.3718459617061285 ) ) ;
#43695 = CARTESIAN_POINT ( 'NONE',  ( -7.537381089459999295, 1495.227545663890169, 200.7918938288690072 ) ) ;
#43696 = CARTESIAN_POINT ( 'NONE',  ( 37.04966271671443678, 1455.306136334554367, 269.5612861309130039 ) ) ;
#43697 = FACE_OUTER_BOUND ( 'NONE', #109026, .T. ) ;
#43698 = CARTESIAN_POINT ( 'NONE',  ( 6.220301990569999440, 1397.477102019330232, 220.4683151594979904 ) ) ;
#43699 = CARTESIAN_POINT ( 'NONE',  ( 33.28034951413933129, 1501.977400791986611, 217.4407153818819722 ) ) ;
#43700 = CARTESIAN_POINT ( 'NONE',  ( -7.018605345631014458, 1516.569754971243356, 211.7654319798640188 ) ) ;
#43701 = CARTESIAN_POINT ( 'NONE',  ( -20.87069991009999725, 1506.658021081189872, 214.5368842940590071 ) ) ;
#43702 = CARTESIAN_POINT ( 'NONE',  ( -9.632230605042634508, 1367.664641040586275, 207.6218459616987673 ) ) ;
#43703 = CARTESIAN_POINT ( 'NONE',  ( -13.62888597016050163, 1517.051704413129983, 226.2994540733420195 ) ) ;
#43704 = CARTESIAN_POINT ( 'NONE',  ( -2.299656354225000143, 1516.843453247299749, 206.6453952679669896 ) ) ;
#43705 = CARTESIAN_POINT ( 'NONE',  ( 4.225063846580001226, 1446.249084106590090, 165.9135352184979979 ) ) ;
#43706 = B_SPLINE_SURFACE_WITH_KNOTS ( 'NONE', 5, 5, ( 
 ( #21517, #23185, #57386, #40550, #57926, #41662, #33247, #102102, #74177, #108307, #100993, #31592 ),
 ( #59029, #65769, #92058, #15330, #24289, #50074, #99887, #5858, #84748, #24824, #39999, #91512 ),
 ( #14792, #58470, #67437, #48978, #32703, #82566, #83650, #75818, #92597, #83110, #6404, #74724 ),
 ( #109426, #109970, #108857, #49525, #8046, #32151, #66339, #101535, #93154, #16423, #15871, #84203 ),
 ( #7500, #100455, #23738, #66883, #50616, #33796, #42214, #110514, #76365, #6945, #25382, #90948 ),
 ( #14234, #41100, #67990, #75279, #48423, #70218, #59574, #94252, #51729, #17526, #60133, #44997 ),
 ( #93688, #18095, #36567, #35463, #61802, #16968, #27077, #778, #70765, #34907, #78576, #52289 ),
 ( #85295, #95375, #8594, #61260, #44432, #68538, #77477, #86414, #42766, #76926, #51167, #9704 ),
 ( #85864, #103194, #26499, #10825, #235, #69093, #95923, #104876, #1891, #60695, #94818, #34362 ),
 ( #102636, #104322, #79141, #43329, #9165, #25937, #69653, #27616, #1322, #2451, #36028, #43872 ),
 ( #78015, #103774, #18639, #52838, #86965, #10256, #19184, #53388, #87537, #19758, #30357, #97038 ),
 ( #81307, #53960, #98667, #39317, #29812, #21929, #80780, #64549, #106525, #38758, #46647, #71875 ) ),
 .UNSPECIFIED., .F., .F., .F.,
 ( 6, 3, 3, 6 ),
 ( 6, 3, 3, 6 ),
 ( 5.812567949725580441, 6.561021380799999747, 7.569428689259999565, 8.073660213293690546 ),
 ( -6.147585442244000271E-05, 0.3720032648969999745, 1.117748131209999940, 1.738394476804420163 ),
 .UNSPECIFIED. ) ;
#43707 = DIRECTION ( 'NONE',  ( -0.6736849260863841948, 0.000000000000000000, 0.7390186874254148774 ) ) ;
#43708 = CARTESIAN_POINT ( 'NONE',  ( 13.79565896120000090, 1416.830000968330069, 196.3348345146980023 ) ) ;
#43710 = ORIENTED_EDGE ( 'NONE', *, *, #26107, .F. ) ;
#43709 = CARTESIAN_POINT ( 'NONE',  ( -2.658323007379999936, 1496.524950806489869, 220.4400205060989890 ) ) ;
#43711 = DIRECTION ( 'NONE',  ( -1.755985294532469921E-16, 1.000000000000000000, -1.338183447452831989E-16 ) ) ;
#43712 = ORIENTED_EDGE ( 'NONE', *, *, #10108, .F. ) ;
#43713 = ADVANCED_FACE ( 'NONE', ( #73994 ), #5687, .F. ) ;
#43714 = CARTESIAN_POINT ( 'NONE',  ( 18.32011816680000038, 1412.375214688430106, 259.8063374112979886 ) ) ;
#43715 = CARTESIAN_POINT ( 'NONE',  ( -18.41411252810000221, 1430.349328007529948, 194.3797768215980000 ) ) ;
#43717 = CARTESIAN_POINT ( 'NONE',  ( 16.32525169496349804, 1409.508281775810019, 192.9210035046159817 ) ) ;
#43716 = CARTESIAN_POINT ( 'NONE',  ( -10.76776797470689928, 1424.951090220029982, 141.1922884968350047 ) ) ;
#43718 = CARTESIAN_POINT ( 'NONE',  ( 2.493073829755000137, 1516.826109302209943, 211.9861720575370043 ) ) ;
#43719 = CARTESIAN_POINT ( 'NONE',  ( 27.87530505112587775, 1509.998252036734357, 198.0047724899852994 ) ) ;
#43720 = CARTESIAN_POINT ( 'NONE',  ( -22.16059216520000419, 1489.466620110029908, 207.7982630164780176 ) ) ;
#43721 = CARTESIAN_POINT ( 'NONE',  ( -12.38376459812810104, 1378.578895824120082, 209.2319221572759886 ) ) ;
#43722 = CARTESIAN_POINT ( 'NONE',  ( 29.68037260111940157, 1509.976800593680082, 209.6726210628699789 ) ) ;
#43723 = EDGE_CURVE ( 'NONE', #11508, #13046, #65879, .T. ) ;
#43724 = CARTESIAN_POINT ( 'NONE',  ( -5.026420246739999875, 1391.797184865090003, 214.5825844794689772 ) ) ;
#43725 = CARTESIAN_POINT ( 'NONE',  ( -37.68692244320210705, 1438.373698044699950, 136.5893188863019816 ) ) ;
#43726 = VERTEX_POINT ( 'NONE', #50454 ) ;
#43727 = CARTESIAN_POINT ( 'NONE',  ( 8.217383325229510760, 1396.379639214240115, 218.2416968472290080 ) ) ;
#43728 = CARTESIAN_POINT ( 'NONE',  ( 9.941518348215939938, 1460.939688249500023, 207.2380014999110074 ) ) ;
#43729 = CARTESIAN_POINT ( 'NONE',  ( -16.41679994470000281, 1458.914834253029994, 230.3641776037980264 ) ) ;
#43730 = ORIENTED_EDGE ( 'NONE', *, *, #17890, .F. ) ;
#43731 = EDGE_LOOP ( 'NONE', ( #16809, #46175, #20720, #39013 ) ) ;
#43732 = AXIS2_PLACEMENT_3D ( 'NONE', #33964, #75974, #23356 ) ;
#43733 = CARTESIAN_POINT ( 'NONE',  ( -29.24937076371160671, 1509.934532405178516, 211.7291565801588149 ) ) ;
#43734 = CARTESIAN_POINT ( 'NONE',  ( 9.242927444819999394, 1424.975928711410006, 196.2247933120989956 ) ) ;
#43735 = VERTEX_POINT ( 'NONE', #82388 ) ;
#43736 = CARTESIAN_POINT ( 'NONE',  ( -7.756928808066270165, 1508.430203411700177, 219.4938965895260026 ) ) ;
#43737 = CARTESIAN_POINT ( 'NONE',  ( -9.335045448769683674, 1418.488145321254478, 196.8730397695123884 ) ) ;
#43738 = AXIS2_PLACEMENT_3D ( 'NONE', #6389, #75803, #31579 ) ;
#43739 = CARTESIAN_POINT ( 'NONE',  ( -12.30608628080000067, 1442.741623762909967, 186.5150421474980078 ) ) ;
#43740 = AXIS2_PLACEMENT_3D ( 'NONE', #69856, #51932, #62009 ) ;
#43741 = CARTESIAN_POINT ( 'NONE',  ( 28.45107529421216697, 1509.906593692594470, 206.0415051226699177 ) ) ;
#43742 = LINE ( 'NONE', #10131, #6364 ) ;
#43743 = CARTESIAN_POINT ( 'NONE',  ( 10.54229472710979998, 1452.173451298499913, 208.4873773006349893 ) ) ;
#43744 = CARTESIAN_POINT ( 'NONE',  ( -32.86802468386298415, 1512.187213306747481, 201.0396662540046577 ) ) ;
#43745 = CARTESIAN_POINT ( 'NONE',  ( -96.21043572509938713, 1384.861607426979845, 295.3416321102220081 ) ) ;
#43746 = VERTEX_POINT ( 'NONE', #14058 ) ;
#43747 = CARTESIAN_POINT ( 'NONE',  ( 1.708102589285000139, 1517.199196846569976, 202.5572672468869939 ) ) ;
#43748 = CARTESIAN_POINT ( 'NONE',  ( -4.042388539304999640, 1517.045004075700035, 208.3857484934819979 ) ) ;
#43749 = VERTEX_POINT ( 'NONE', #82928 ) ;
#43750 = CARTESIAN_POINT ( 'NONE',  ( 11.74655472833119951, 1426.725573876949966, 144.8372549033489918 ) ) ;
#43751 = CARTESIAN_POINT ( 'NONE',  ( 2.983377196939291043, 1512.076549611913379, 217.0139528183213997 ) ) ;
#43752 = ORIENTED_EDGE ( 'NONE', *, *, #24716, .T. ) ;
#43753 = CARTESIAN_POINT ( 'NONE',  ( 4.487249753905000027, 1509.038615934169911, 212.6094383991670043 ) ) ;
#43754 = CARTESIAN_POINT ( 'NONE',  ( 17.17241001986506888, 1518.913060387330006, 238.6251415217915337 ) ) ;
#43755 = CARTESIAN_POINT ( 'NONE',  ( 5.190825549110000381, 1509.094328009829951, 237.6860785186979967 ) ) ;
#43756 = CARTESIAN_POINT ( 'NONE',  ( -1.811252493420050014, 1468.887500306539778, 219.1128618160599899 ) ) ;
#43757 = CARTESIAN_POINT ( 'NONE',  ( -5.755370776679999523, 1424.283853029129887, 186.4664930395979923 ) ) ;
#43758 = CARTESIAN_POINT ( 'NONE',  ( 4.112859965242409821, 1410.383928704729897, 269.6166979547700180 ) ) ;
#43759 = LINE ( 'NONE', #77911, #110347 ) ;
#43760 = CARTESIAN_POINT ( 'NONE',  ( -110.0634901748029932, 1384.899971912700039, 296.9512050915229793 ) ) ;
#43761 = CARTESIAN_POINT ( 'NONE',  ( 8.185540730390000519, 1494.061971860590120, 217.8458731800789963 ) ) ;
#43762 = CARTESIAN_POINT ( 'NONE',  ( -37.86125039060000574, 1379.639043232470158, 220.5631543556590088 ) ) ;
#43763 = CARTESIAN_POINT ( 'NONE',  ( 8.107340703835214768, 1424.171636185274110, 195.7651162605105810 ) ) ;
#43765 = CARTESIAN_POINT ( 'NONE',  ( 9.751541468637160648, 1469.019378510909974, 203.4839537346510099 ) ) ;
#43764 = CARTESIAN_POINT ( 'NONE',  ( -3.617573937782270210, 1497.333809982809953, 198.4503636364750037 ) ) ;
#43766 = CARTESIAN_POINT ( 'NONE',  ( -68.77278092737650184, 1379.747928288920093, 280.3133413970129482 ) ) ;
#43767 = FACE_OUTER_BOUND ( 'NONE', #15870, .T. ) ;
#43768 = CARTESIAN_POINT ( 'NONE',  ( -2.499957258650039815, 1419.547118819750267, 136.6619867572729845 ) ) ;
#43769 = ORIENTED_EDGE ( 'NONE', *, *, #106248, .F. ) ;
#43770 = CARTESIAN_POINT ( 'NONE',  ( 18.11762544937269936, 1424.498479437349943, 224.0223624214009988 ) ) ;
#43771 = CARTESIAN_POINT ( 'NONE',  ( -17.44374831407532866, 1524.130440953581001, 180.7216696960686591 ) ) ;
#43772 = CARTESIAN_POINT ( 'NONE',  ( -2.898163115812544710, 1484.340737685897466, 183.3113270340765837 ) ) ;
#43773 = CARTESIAN_POINT ( 'NONE',  ( -14.68224678300000008, 1416.181292664740113, 213.8220209240589895 ) ) ;
#43774 = AXIS2_PLACEMENT_3D ( 'NONE', #58919, #58369, #48882 ) ;
#43776 = VERTEX_POINT ( 'NONE', #101915 ) ;
#43775 = CARTESIAN_POINT ( 'NONE',  ( 1.694729585907490010, 1515.066341861380124, 204.7924377471120181 ) ) ;
#43777 = CARTESIAN_POINT ( 'NONE',  ( -15.85288220972839035, 1415.900318358362483, 209.7246934675221723 ) ) ;
#43778 = CARTESIAN_POINT ( 'NONE',  ( -24.42830362399999800, 1444.284632803539807, 211.0503697367179825 ) ) ;
#43779 = CARTESIAN_POINT ( 'NONE',  ( -11.46173801930000025, 1425.627560988929872, 146.1134360337979956 ) ) ;
#43780 = DIRECTION ( 'NONE',  ( 0.000000000000000000, 0.000000000000000000, -1.000000000000000000 ) ) ;
#43781 = CARTESIAN_POINT ( 'NONE',  ( -11.03352341481849841, 1462.446812322350070, 208.7213867630900097 ) ) ;
#43782 = CARTESIAN_POINT ( 'NONE',  ( 27.01382310970000233, 1451.969724731730139, 134.9184576876980088 ) ) ;
#43783 = CARTESIAN_POINT ( 'NONE',  ( 31.23437356469435144, 1512.187213306747481, 196.3468678195113739 ) ) ;
#43784 = CARTESIAN_POINT ( 'NONE',  ( -16.46592305696500347, 1512.456207068040158, 220.8712538603669771 ) ) ;
#43785 = CARTESIAN_POINT ( 'NONE',  ( 14.00845289490000134, 1415.082769112230153, 228.2443160964980109 ) ) ;
#43786 = CARTESIAN_POINT ( 'NONE',  ( -10.22273176409999884, 1479.690303922389830, 215.0709727714090036 ) ) ;
#43787 = CARTESIAN_POINT ( 'NONE',  ( -15.90941686800000099, 1459.206357706029848, 229.9918337653980132 ) ) ;
#43788 = CARTESIAN_POINT ( 'NONE',  ( 5.771149074885000729, 1516.616791731099966, 206.6334853027970269 ) ) ;
#43789 = CARTESIAN_POINT ( 'NONE',  ( 29.91696786530000196, 1414.743747860729854, 269.1810462695979709 ) ) ;
#43790 = CARTESIAN_POINT ( 'NONE',  ( 7.269615798715341803, 1508.603735221739498, 214.6352815282469351 ) ) ;
#43791 = CARTESIAN_POINT ( 'NONE',  ( 18.77981283949999991, 1430.305403855530130, 193.1839142650980250 ) ) ;
#43792 = CARTESIAN_POINT ( 'NONE',  ( -20.93923811180000172, 1428.771874825830082, 221.3173514296979931 ) ) ;
#43793 = DIRECTION ( 'NONE',  ( 5.980589973904019347E-17, -1.000000000000000000, 1.736889445713099699E-16 ) ) ;
#43794 = EDGE_CURVE ( 'NONE', #87329, #3165, #68764, .T. ) ;
#43795 = CARTESIAN_POINT ( 'NONE',  ( 5.360207926212690488, 1422.242713656610022, 144.1549664376839814 ) ) ;
#43796 = CARTESIAN_POINT ( 'NONE',  ( -1.708753861699999987, 1450.488287334239885, 182.5123027767980091 ) ) ;
#43797 = CARTESIAN_POINT ( 'NONE',  ( -16.73628186595857059, 1526.382868172863937, 184.0591879540917546 ) ) ;
#43798 = CARTESIAN_POINT ( 'NONE',  ( -15.99522875749999962, 1414.971279908829956, 203.4402680263180230 ) ) ;
#43799 = CARTESIAN_POINT ( 'NONE',  ( -13.19176083819999867, 1443.059844678469972, 186.7785638985979801 ) ) ;
#43800 = ADVANCED_FACE ( 'NONE', ( #109253 ), #59903, .F. ) ;
#43801 = CARTESIAN_POINT ( 'NONE',  ( -2.487935123034410001, 1509.038615930399828, 213.6090957347729784 ) ) ;
#43802 = EDGE_CURVE ( 'NONE', #75670, #78107, #66200, .T. ) ;
#43803 = CARTESIAN_POINT ( 'NONE',  ( -33.53719164820000032, 1436.564435420739983, 136.5219720490979967 ) ) ;
#43804 = DIRECTION ( 'NONE',  ( 0.000000000000000000, 1.000000000000000000, 0.000000000000000000 ) ) ;
#43805 = VERTEX_POINT ( 'NONE', #61080 ) ;
#43806 = CARTESIAN_POINT ( 'NONE',  ( -2.711770233124999763, 1512.058324472099912, 201.4383516934770171 ) ) ;
#43807 = CARTESIAN_POINT ( 'NONE',  ( -14.68124966667719988, 1409.425740922790055, 211.8641606095099803 ) ) ;
#43808 = B_SPLINE_SURFACE_WITH_KNOTS ( 'NONE', 2, 5, ( 
 ( #82720, #31756, #49686, #83269, #23352, #40715 ),
 ( #110123, #32320, #66503, #41270, #109580, #32851 ),
 ( #67042, #67591, #35614, #96078, #33961, #17124 ) ),
 .UNSPECIFIED., .F., .F., .F.,
 ( 3, 3 ),
 ( 6, 6 ),
 ( 1.399803019519999969, 2.016961153520000050 ),
 ( 0.000000000000000000, 1.000000000000000000 ),
 .UNSPECIFIED. ) ;
#43809 = VECTOR ( 'NONE', #11780, 1000.000000000000227 ) ;
#43810 = CARTESIAN_POINT ( 'NONE',  ( -12.28097721992999958, 1508.220391055730033, 209.1123848330070132 ) ) ;
#43811 = CARTESIAN_POINT ( 'NONE',  ( -38.50379591154272418, 1443.086052842849085, 136.9552667236205821 ) ) ;
#43812 = CARTESIAN_POINT ( 'NONE',  ( -7.090184954099999715, 1475.703047307030147, 267.8325052247980125 ) ) ;
#43813 = CARTESIAN_POINT ( 'NONE',  ( 30.31052258194586102, 1523.604703353109699, 195.7506062427368079 ) ) ;
#43814 = DIRECTION ( 'NONE',  ( 0.9858563016923833633, 0.000000000000000000, 0.1675928173085483863 ) ) ;
#43815 = AXIS2_PLACEMENT_3D ( 'NONE', #91285, #5071, #100241 ) ;
#43816 = CARTESIAN_POINT ( 'NONE',  ( 18.16574811487310015, 1421.104903170840089, 223.5180812899619980 ) ) ;
#43817 = CARTESIAN_POINT ( 'NONE',  ( -80.39701180146140302, 1384.637746234069937, 304.1167271054749790 ) ) ;
#43818 = FACE_OUTER_BOUND ( 'NONE', #4502, .T. ) ;
#43819 = CARTESIAN_POINT ( 'NONE',  ( 17.30469233084960123, 1424.057501815570049, 228.1010343377980121 ) ) ;
#43820 = CARTESIAN_POINT ( 'NONE',  ( 15.98493104980000190, 1416.216252248729916, 217.5912660269380012 ) ) ;
#43821 = CARTESIAN_POINT ( 'NONE',  ( -11.89522282729999958, 1434.541161981840105, 151.0452005854980086 ) ) ;
#43822 = DIRECTION ( 'NONE',  ( 0.4999999999998399614, -0.7071067811867740582, -0.4999999999998399614 ) ) ;
#43823 = CARTESIAN_POINT ( 'NONE',  ( -3.909710721586109550, 1517.151704408390060, 197.7672215555029993 ) ) ;
#43824 = CARTESIAN_POINT ( 'NONE',  ( -8.156454811679999750, 1384.924237574090057, 199.6468110712790178 ) ) ;
#43825 = B_SPLINE_CURVE_WITH_KNOTS ( 'NONE', 3,
 ( #100243, #50952, #7283, #82882, #49301, #85077, #99666, #23521, #92934, #83426 ),
 .UNSPECIFIED., .F., .F.,
 ( 4, 2, 2, 2, 4 ),
 ( 2.065250908360339998E-07, 0.03315402003890329657, 0.05105978556791049977, 0.05919766143195339531, 0.06630775015685380636 ),
 .UNSPECIFIED. ) ;
#43826 = CARTESIAN_POINT ( 'NONE',  ( -23.16614514220000132, 1409.886532898030055, 207.1837266853979997 ) ) ;
#43827 = CARTESIAN_POINT ( 'NONE',  ( 12.70717284289999860, 1414.913060387329779, 197.8159508449980137 ) ) ;
#43828 = CARTESIAN_POINT ( 'NONE',  ( 4.070747692530000350, 1486.294283939790148, 219.1124398665789954 ) ) ;
#43829 = CARTESIAN_POINT ( 'NONE',  ( 11.24836030156600053, 1479.301895909970199, 207.8159963017580196 ) ) ;
#43830 = B_SPLINE_SURFACE_WITH_KNOTS ( 'NONE', 5, 3, ( 
 ( #22951, #90723, #22389, #98571 ),
 ( #64994, #81218, #21840, #72304 ),
 ( #98019, #57156, #38668, #91281 ),
 ( #56037, #73392, #14561, #82875 ),
 ( #6168, #106976, #40322, #30264 ),
 ( #74504, #90164, #30817, #13445 ),
 ( #47636, #81764, #5067, #39214 ),
 ( #16200, #8362, #33557, #66659 ),
 ( #109202, #16739, #15640, #84530 ) ),
 .UNSPECIFIED., .F., .F., .F.,
 ( 6, 3, 6 ),
 ( 4, 4 ),
 ( 0.000000000000000000, 5.782490304330000441, 11.25975508159999983 ),
 ( 37.69911184309999896, 40.20365518519999881 ),
 .UNSPECIFIED. ) ;
#43831 = CARTESIAN_POINT ( 'NONE',  ( 0.8307690413430001142, 1441.600846913440137, 150.7224806086979640 ) ) ;
#43832 = CARTESIAN_POINT ( 'NONE',  ( 20.79429048353240006, 1456.232304843699922, 207.0687085352159897 ) ) ;
#43834 = ADVANCED_FACE ( 'NONE', ( #77846 ), #93826, .T. ) ;
#43833 = CARTESIAN_POINT ( 'NONE',  ( 17.19739463999635021, 1525.960063244516959, 181.9833109756549163 ) ) ;
#43835 = CARTESIAN_POINT ( 'NONE',  ( -17.55008888293159686, 1487.029577683950038, 194.9701234137779977 ) ) ;
#43837 = CARTESIAN_POINT ( 'NONE',  ( -13.48418208170959964, 1379.644826002420132, 211.5188789427980112 ) ) ;
#43836 = CARTESIAN_POINT ( 'NONE',  ( -22.74352257909999864, 1409.874439094229956, 210.5210124972680035 ) ) ;
#43838 = CARTESIAN_POINT ( 'NONE',  ( -4.992439177819999685, 1391.624324237289784, 203.6930817768189854 ) ) ;
#43839 = DIRECTION ( 'NONE',  ( 0.000000000000000000, 0.000000000000000000, 1.000000000000000000 ) ) ;
#43840 = CARTESIAN_POINT ( 'NONE',  ( -11.71397067460000052, 1489.483176008789997, 212.5377880877490213 ) ) ;
#43841 = CARTESIAN_POINT ( 'NONE',  ( 9.833400138500138610, 1450.823812866140088, 205.5646184881250065 ) ) ;
#43842 = CARTESIAN_POINT ( 'NONE',  ( -0.8668663496707069704, 1420.136354665399949, 184.5670725461910138 ) ) ;
#43843 = CARTESIAN_POINT ( 'NONE',  ( 1.121383591734999907, 1517.104192383289956, 204.4960559556369901 ) ) ;
#43844 = FILL_AREA_STYLE_COLOUR ( '', #62329 ) ;
#43845 = FACE_OUTER_BOUND ( 'NONE', #106508, .T. ) ;
#43846 = CARTESIAN_POINT ( 'NONE',  ( 2.324758082599999831, 1508.994242728630070, 237.7951232945979996 ) ) ;
#43847 = CARTESIAN_POINT ( 'NONE',  ( 8.147371244622188868, 1505.597128609329957, 217.5190773777700031 ) ) ;
#43848 = CARTESIAN_POINT ( 'NONE',  ( -9.821980025724538876, 1422.689482519856483, 210.6756101855388863 ) ) ;
#43850 = ORIENTED_EDGE ( 'NONE', *, *, #4155, .T. ) ;
#43849 = CARTESIAN_POINT ( 'NONE',  ( -62.66283327366161160, 1379.734827332920077, 270.6325249849410284 ) ) ;
#43851 = VERTEX_POINT ( 'NONE', #10080 ) ;
#43852 = CARTESIAN_POINT ( 'NONE',  ( 11.16030059240809891, 1434.071225047799999, 151.6430048918290083 ) ) ;
#43853 = ORIENTED_EDGE ( 'NONE', *, *, #95934, .F. ) ;
#43854 = CARTESIAN_POINT ( 'NONE',  ( -0.0002548899671389549728, 1396.374106340500475, 221.3992528296966213 ) ) ;
#43855 = CIRCLE ( 'NONE', #61700, 1.999999999999999556 ) ;
#43856 = CARTESIAN_POINT ( 'NONE',  ( -21.23228437720000272, 1508.977225839029870, 191.9851283159979971 ) ) ;
#43857 = CARTESIAN_POINT ( 'NONE',  ( -7.791194074889999932, 1385.469146237939867, 218.8820831402890121 ) ) ;
#43859 = CARTESIAN_POINT ( 'NONE',  ( 11.01124415049999961, 1428.984115384829920, 91.31218443469779800 ) ) ;
#43858 = CARTESIAN_POINT ( 'NONE',  ( 16.59201921935060042, 1441.947058765370002, 190.5569223725519805 ) ) ;
#43860 = CARTESIAN_POINT ( 'NONE',  ( 18.99471019034560015, 1488.414476589019841, 228.8317491358870086 ) ) ;
#43861 =( BOUNDED_CURVE ( )  B_SPLINE_CURVE ( 3, ( #13644, #31572, #97136, #80341 ),
 .UNSPECIFIED., .F., .T. ) 
 B_SPLINE_CURVE_WITH_KNOTS ( ( 4, 4 ),
 ( 0.9002477009696591148, 1.144704976403996710 ),
 .UNSPECIFIED. ) 
 CURVE ( )  GEOMETRIC_REPRESENTATION_ITEM ( )  RATIONAL_B_SPLINE_CURVE ( ( 1.000000000000000000, 0.9950262502543076870, 0.9950262502543076870, 1.000000000000000000 ) ) 
 REPRESENTATION_ITEM ( '' )  );
#43862 = CARTESIAN_POINT ( 'NONE',  ( 13.86663486569999826, 1507.632686203329968, 185.8229747852979870 ) ) ;
#43863 = CARTESIAN_POINT ( 'NONE',  ( -2.859824010850000153, 1416.824060884929850, 191.2754762073979862 ) ) ;
#43864 = CARTESIAN_POINT ( 'NONE',  ( -24.35354770432089921, 1444.782666551750026, 211.2047157338469958 ) ) ;
#43865 = EDGE_CURVE ( 'NONE', #42097, #32377, #53210, .T. ) ;
#43866 = CARTESIAN_POINT ( 'NONE',  ( 1.136004274065000041, 1516.815173273089840, 211.9874827793370287 ) ) ;
#43868 = AXIS2_PLACEMENT_3D ( 'NONE', #76781, #86280, #99 ) ;
#43867 = CARTESIAN_POINT ( 'NONE',  ( 13.43786152523319899, 1415.007830323630060, 197.8851484046579969 ) ) ;
#43869 = CARTESIAN_POINT ( 'NONE',  ( -14.92548077329999856, 1420.621803361759930, 210.5949619620589885 ) ) ;
#43870 = CARTESIAN_POINT ( 'NONE',  ( 7.843966614384998870, 1513.355826799099759, 201.5485691027769803 ) ) ;
#43871 = ORIENTED_EDGE ( 'NONE', *, *, #1145, .F. ) ;
#43872 = CARTESIAN_POINT ( 'NONE',  ( 14.44259369381050107, 1436.255177350019949, 149.9682632730880130 ) ) ;
#43873 = CARTESIAN_POINT ( 'NONE',  ( 1.248319867352440049, 1432.832940376729994, 200.7627304351539976 ) ) ;
#43874 = VERTEX_POINT ( 'NONE', #104693 ) ;
#43875 = EDGE_LOOP ( 'NONE', ( #64128, #31796, #108957, #102909 ) ) ;
#43876 = CARTESIAN_POINT ( 'NONE',  ( -8.788316527315000570, 1511.741868877540128, 215.3741124244170067 ) ) ;
#43877 = CARTESIAN_POINT ( 'NONE',  ( -2.751894522449999769, 1465.785413735030033, 235.3217997380980080 ) ) ;
#43878 = DIRECTION ( 'NONE',  ( 0.000000000000000000, 0.000000000000000000, 1.000000000000000000 ) ) ;
#43879 = CARTESIAN_POINT ( 'NONE',  ( -5.779627092215000594, 1516.977993847330026, 216.8424961055369806 ) ) ;
#43880 = CARTESIAN_POINT ( 'NONE',  ( 9.831195298860000875, 1461.796653712189936, 208.3421129825899811 ) ) ;
#43881 = CARTESIAN_POINT ( 'NONE',  ( -18.97929560748146827, 1443.421918779768930, 211.6863114044098211 ) ) ;
#43882 = CARTESIAN_POINT ( 'NONE',  ( -48.22222548969896394, 1379.682101389173340, 236.1980132620304289 ) ) ;
#43883 = CARTESIAN_POINT ( 'NONE',  ( 4.242807150219759293, 1446.407532295220108, 162.3334345628060191 ) ) ;
#43884 = CARTESIAN_POINT ( 'NONE',  ( 0.6603057237680000080, 1507.898464389029868, 237.4637152757979948 ) ) ;
#43885 = VERTEX_POINT ( 'NONE', #8413 ) ;
#43886 = CARTESIAN_POINT ( 'NONE',  ( 6.934528529765000116, 1516.588006113850042, 206.2478870805069846 ) ) ;
#43887 = ORIENTED_EDGE ( 'NONE', *, *, #9792, .F. ) ;
#43888 = CARTESIAN_POINT ( 'NONE',  ( 23.03224585666420055, 1440.913060387330006, 231.8929951805789926 ) ) ;
#43889 = CARTESIAN_POINT ( 'NONE',  ( -19.06717646990000148, 1508.525021831829918, 229.8525292550980055 ) ) ;
#43890 = ORIENTED_EDGE ( 'NONE', *, *, #106127, .T. ) ;
#43891 = CARTESIAN_POINT ( 'NONE',  ( -5.513211403820640122, 1508.731183031489991, 201.6768811751110206 ) ) ;
#43892 = CARTESIAN_POINT ( 'NONE',  ( -14.33997081240000071, 1409.413823202629828, 191.5153657412979840 ) ) ;
#43893 = CARTESIAN_POINT ( 'NONE',  ( -24.49087403330000257, 1441.667334617299957, 211.0234093942380014 ) ) ;
#43895 = VERTEX_POINT ( 'NONE', #18455 ) ;
#43894 = CARTESIAN_POINT ( 'NONE',  ( 4.144810350071930216, 1423.945503712369828, 193.0065599516869952 ) ) ;
#43896 = CARTESIAN_POINT ( 'NONE',  ( 0.0002635607284424891939, 1396.409786001411021, 196.8022392320345375 ) ) ;
#43897 = CARTESIAN_POINT ( 'NONE',  ( -11.89384099105951087, 1433.284007347989927, 147.6487936648496770 ) ) ;
#43898 = CARTESIAN_POINT ( 'NONE',  ( -109.9987472819999965, 1383.757409383979848, 311.0847451122589860 ) ) ;
#43900 = EDGE_CURVE ( 'NONE', #93500, #10365, #739, .T. ) ;
#43899 = LINE ( 'NONE', #1350, #8745 ) ;
#43902 = CARTESIAN_POINT ( 'NONE',  ( -1.880981557899999990, 1491.684224442789855, 188.2614447320989939 ) ) ;
#43901 = CARTESIAN_POINT ( 'NONE',  ( 21.13130013988266853, 1524.397344074319108, 180.8335768739904381 ) ) ;
#43903 = EDGE_CURVE ( 'NONE', #14195, #88662, #80853, .T. ) ;
#43904 = CARTESIAN_POINT ( 'NONE',  ( -6.551643424905000401, 1516.807958722750072, 214.9033365145770063 ) ) ;
#43905 = CARTESIAN_POINT ( 'NONE',  ( -3.259994511801839856, 1428.775419947709906, 200.3424632861539862 ) ) ;
#43906 = CARTESIAN_POINT ( 'NONE',  ( -20.86054011819999943, 1508.959477709930070, 190.3575368045979985 ) ) ;
#43907 = DIRECTION ( 'NONE',  ( -0.9948834766775040972, 0.000000000000000000, 0.1010290445074205484 ) ) ;
#43908 = CARTESIAN_POINT ( 'NONE',  ( 0.7579843820170020230, 1516.883361325900069, 211.4083188566570186 ) ) ;
#43909 = AXIS2_PLACEMENT_3D ( 'NONE', #104813, #87475, #27553 ) ;
#43910 = CARTESIAN_POINT ( 'NONE',  ( 14.80326726320000041, 1409.939845482530018, 191.7219674997980121 ) ) ;
#43911 = CARTESIAN_POINT ( 'NONE',  ( 30.01483979338928165, 1525.231887713385959, 221.6074839523207345 ) ) ;
#43913 = VERTEX_POINT ( 'NONE', #47555 ) ;
#43912 = CARTESIAN_POINT ( 'NONE',  ( -82.03511417020000351, 1389.474284752290032, 290.2139668048590124 ) ) ;
#43914 = CARTESIAN_POINT ( 'NONE',  ( 40.57815444089999346, 1448.614255965100028, 261.6157397843979879 ) ) ;
#43915 = CARTESIAN_POINT ( 'NONE',  ( 10.88673685277470149, 1490.602448971980039, 210.5186076668310022 ) ) ;
#43916 = FACE_OUTER_BOUND ( 'NONE', #61241, .T. ) ;
#43917 = CARTESIAN_POINT ( 'NONE',  ( -2.626137216361650317, 1508.420410720970040, 237.4127342639979759 ) ) ;
#43918 = CARTESIAN_POINT ( 'NONE',  ( -22.15139830520000075, 1451.884836738830245, 222.5180298456980097 ) ) ;
#43920 = CARTESIAN_POINT ( 'NONE',  ( 17.32269403890969883, 1409.630503568620043, 222.4515702929919883 ) ) ;
#43919 = CARTESIAN_POINT ( 'NONE',  ( 11.30340088569999857, 1432.444851987580023, 151.5218631127980018 ) ) ;
#43921 = CARTESIAN_POINT ( 'NONE',  ( 0.2751658889820000065, 1506.798305107329952, 186.8348836488979998 ) ) ;
#43922 = CARTESIAN_POINT ( 'NONE',  ( -109.0942519332729859, 1382.194178918040052, 310.8938292817809952 ) ) ;
#43923 = VERTEX_POINT ( 'NONE', #30176 ) ;
#43924 = CARTESIAN_POINT ( 'NONE',  ( 2.480187016714999970, 1517.025470194390209, 204.4964864072570094 ) ) ;
#43925 = EDGE_CURVE ( 'NONE', #55354, #6757, #10038, .T. ) ;
#43926 = CARTESIAN_POINT ( 'NONE',  ( 0.3342173453870000421, 1406.778501198230060, 269.6500372471979858 ) ) ;
#43927 = CARTESIAN_POINT ( 'NONE',  ( 28.70471845000000144, 1509.915451243230109, 206.7904320628580024 ) ) ;
#43929 = EDGE_CURVE ( 'NONE', #7138, #57302, #64813, .T. ) ;
#43928 = AXIS2_PLACEMENT_3D ( 'NONE', #68603, #18166, #60199 ) ;
#43930 = CARTESIAN_POINT ( 'NONE',  ( -4.927642603766289224E-06, 1473.264982651129912, 270.4290828326839460 ) ) ;
#43931 = CARTESIAN_POINT ( 'NONE',  ( 2.478804629799999937, 1434.635234717510002, 157.5856215605979855 ) ) ;
#43932 = CARTESIAN_POINT ( 'NONE',  ( 3.395043742270000386, 1466.412111213989874, 219.6384586637989855 ) ) ;
#43933 = CARTESIAN_POINT ( 'NONE',  ( 8.759801967190000482, 1450.891143041990063, 191.6269498783990173 ) ) ;
#43934 = ADVANCED_FACE ( 'NONE', ( #29634 ), #42907, .F. ) ;
#43935 = CARTESIAN_POINT ( 'NONE',  ( -39.59018362911489675, 1440.913060399770075, 258.6997408151970603 ) ) ;
#43936 = CARTESIAN_POINT ( 'NONE',  ( -26.41481021949999786, 1448.998476365520219, 136.8839732230979962 ) ) ;
#43937 = DIRECTION ( 'NONE',  ( 0.000000000000000000, 0.000000000000000000, 1.000000000000000000 ) ) ;
#43938 = CARTESIAN_POINT ( 'NONE',  ( 0.7579935661000010150, 1432.645091882289989, 200.6977994915789907 ) ) ;
#43939 = CARTESIAN_POINT ( 'NONE',  ( 10.95552075894139854, 1480.084818102109921, 209.3730989235789934 ) ) ;
#43940 = EDGE_CURVE ( 'NONE', #59669, #99476, #103422, .T. ) ;
#43941 = CARTESIAN_POINT ( 'NONE',  ( -21.55808780550650283, 1523.844782250843537, 183.9826089808311735 ) ) ;
#43942 = VECTOR ( 'NONE', #65371, 1000.000000000000000 ) ;
#43943 = DIRECTION ( 'NONE',  ( -0.3363363969981663093, -0.6659120918162475533, 0.6659120918163308200 ) ) ;
#43944 = EDGE_LOOP ( 'NONE', ( #76486, #99336, #10506 ) ) ;
#43945 = CARTESIAN_POINT ( 'NONE',  ( 2.431412526649999961, 1428.647745098929818, 149.4227846719979880 ) ) ;
#43946 = CARTESIAN_POINT ( 'NONE',  ( 12.91337836679999995, 1434.774321454559868, 146.9205881264979894 ) ) ;
#43947 = ADVANCED_FACE ( 'NONE', ( #92295 ), #76646, .T. ) ;
#43948 = CARTESIAN_POINT ( 'NONE',  ( 3.197956043390000058, 1485.326915628889992, 198.8549714615990069 ) ) ;
#43949 = CARTESIAN_POINT ( 'NONE',  ( 16.19903696008579885, 1484.264179847840069, 188.8259855492240149 ) ) ;
#43950 = CARTESIAN_POINT ( 'NONE',  ( -0.4915625660039999456, 1417.355248640930085, 235.5475657494979771 ) ) ;
#43951 = CARTESIAN_POINT ( 'NONE',  ( 11.36432067319999994, 1502.559788237589828, 210.8834125687090193 ) ) ;
#43952 = DIRECTION ( 'NONE',  ( -0.02616798426500960631, -0.9993150019883682011, -0.02616798426500960631 ) ) ;
#43953 = CARTESIAN_POINT ( 'NONE',  ( 8.044556495430001064, 1427.503828071409998, 212.2292562717090050 ) ) ;
#43954 = CARTESIAN_POINT ( 'NONE',  ( -18.21186767409350082, 1384.867739624789920, 220.2868233047339857 ) ) ;
#43955 = EDGE_CURVE ( 'NONE', #89851, #37990, #44463, .T. ) ;
#43956 = FACE_OUTER_BOUND ( 'NONE', #66347, .T. ) ;
#43957 = CARTESIAN_POINT ( 'NONE',  ( -9.069247167689999500, 1483.910511149589865, 201.2456827287589931 ) ) ;
#43958 = CARTESIAN_POINT ( 'NONE',  ( 26.67084063728509591, 1435.736201010440254, 136.2273027514239914 ) ) ;
#43959 = CARTESIAN_POINT ( 'NONE',  ( -9.581540676829499503, 1396.247655162970204, 203.5967411505729956 ) ) ;
#43960 = VERTEX_POINT ( 'NONE', #103445 ) ;
#43961 = EDGE_CURVE ( 'NONE', #79464, #88339, #1030, .T. ) ;
#43962 = CARTESIAN_POINT ( 'NONE',  ( 3.145310910306181373, 1370.220870732725871, 208.0282141261312461 ) ) ;
#43963 = CARTESIAN_POINT ( 'NONE',  ( 2.482344662330000062, 1440.444625599219989, 150.5580151863979950 ) ) ;
#43964 = ORIENTED_EDGE ( 'NONE', *, *, #6559, .F. ) ;
#43965 = VERTEX_POINT ( 'NONE', #50859 ) ;
#43966 = FACE_OUTER_BOUND ( 'NONE', #33775, .T. ) ;
#43968 = EDGE_CURVE ( 'NONE', #1945, #47514, #19339, .T. ) ;
#43967 = CARTESIAN_POINT ( 'NONE',  ( -14.48519483975229960, 1416.181292564900104, 203.8595933512790168 ) ) ;
#43970 = CARTESIAN_POINT ( 'NONE',  ( -1.604553179929740114, 1457.465057722440179, 219.6491839707440192 ) ) ;
#43969 = CARTESIAN_POINT ( 'NONE',  ( 11.03848064059999956, 1426.925978087529984, 93.46471121569780394 ) ) ;
#43971 = LINE ( 'NONE', #41891, #21722 ) ;
#43972 = ADVANCED_FACE ( 'NONE', ( #44125 ), #101785, .T. ) ;
#43973 = CARTESIAN_POINT ( 'NONE',  ( 0.02089856015480650100, 1507.111761549349922, 237.3522809668369860 ) ) ;
#43974 = DIRECTION ( 'NONE',  ( 0.9996573249755574819, -0.02617694830786557875, 0.000000000000000000 ) ) ;
#43975 = CARTESIAN_POINT ( 'NONE',  ( 7.597901083480000040, 1425.607998949240027, 212.0366610610989824 ) ) ;
#43976 = CARTESIAN_POINT ( 'NONE',  ( -20.43379408400000230, 1466.940146741789931, 211.2182734472289951 ) ) ;
#43977 = DIRECTION ( 'NONE',  ( 0.000000000000000000, 1.000000000000000000, 0.000000000000000000 ) ) ;
#43978 = CARTESIAN_POINT ( 'NONE',  ( -101.6919322582379976, 1379.485316433199841, 304.9628827255460237 ) ) ;
#43979 = ADVANCED_FACE ( 'NONE', ( #61488 ), #84988, .F. ) ;
#43981 = CARTESIAN_POINT ( 'NONE',  ( 9.704582620035441920, 1366.001145740646052, 210.6218459616987957 ) ) ;
#43980 = ADVANCED_BREP_SHAPE_REPRESENTATION ( '', ( #45166, #21632 ), #91264 ) ;
#43983 = ORIENTED_EDGE ( 'NONE', *, *, #65812, .F. ) ;
#43982 = CARTESIAN_POINT ( 'NONE',  ( 4.594279763170000308, 1454.322381208490015, 217.3118965033989980 ) ) ;
#43984 = ORIENTED_EDGE ( 'NONE', *, *, #107533, .T. ) ;
#43985 = CIRCLE ( 'NONE', #85121, 33.13701971169416538 ) ;
#43986 = CARTESIAN_POINT ( 'NONE',  ( -12.01638156518240130, 1440.881463477919851, 187.8051726210379968 ) ) ;
#43987 = AXIS2_PLACEMENT_3D ( 'NONE', #22236, #99503, #105741 ) ;
#43988 = CYLINDRICAL_SURFACE ( 'NONE', #18881, 2.000000000000003553 ) ;
#43989 = CARTESIAN_POINT ( 'NONE',  ( -1.462229769779999966, 1473.574695470329971, 270.3922974155980228 ) ) ;
#43990 = CARTESIAN_POINT ( 'NONE',  ( 7.527142396971010285, 1500.274912714168295, 200.5649840229101812 ) ) ;
#43991 = CARTESIAN_POINT ( 'NONE',  ( -0.5927006846649999217, 1486.019493224930102, 182.0006702160980012 ) ) ;
#43992 = CARTESIAN_POINT ( 'NONE',  ( -32.16567119605149827, 1524.523992613102564, 202.1429910727728725 ) ) ;
#43993 = CARTESIAN_POINT ( 'NONE',  ( -8.389212874609999204, 1384.445125336340197, 199.8059234258990102 ) ) ;
#43994 = CARTESIAN_POINT ( 'NONE',  ( 7.717505752974999744, 1516.857914730730045, 216.8393517232070167 ) ) ;
#43995 = B_SPLINE_SURFACE_WITH_KNOTS ( 'NONE', 5, 5, ( 
 ( #79369, #86648, #94485, #69885, #26176, #103435 ),
 ( #78814, #88315, #17757, #87209, #78250, #11609 ),
 ( #10501, #19436, #95607, #53636, #60929, #62036 ),
 ( #87780, #468, #11060, #96159, #26741, #52517 ),
 ( #18326, #69327, #2129, #105117, #45230, #44673 ),
 ( #1018, #60363, #43558, #68777, #18874, #36253 ),
 ( #51960, #1564, #9943, #104561, #95059, #35696 ),
 ( #9395, #86102, #44115, #77708, #19996, #2684 ),
 ( #77166, #104001, #34592, #27298, #102878, #61479 ) ),
 .UNSPECIFIED., .F., .F., .F.,
 ( 6, 3, 6 ),
 ( 6, 6 ),
 ( 6.014757930710000089, 12.35992132620000028, 20.20875810949999973 ),
 ( -8.881784197010000791E-16, 10.00000000000000000 ),
 .UNSPECIFIED. ) ;
#43996 = CARTESIAN_POINT ( 'NONE',  ( -2.500000000000000000, 1448.251506100900087, 165.7051602490600146 ) ) ;
#43997 = CARTESIAN_POINT ( 'NONE',  ( 9.339950631061057607, 1369.158344092944390, 209.6218459617033432 ) ) ;
#43998 = CARTESIAN_POINT ( 'NONE',  ( 13.56949689579999863, 1407.458599673630033, 211.9076660747180085 ) ) ;
#43999 = CARTESIAN_POINT ( 'NONE',  ( -5.276338247293970163, 1406.998453906240002, 269.6412759965049872 ) ) ;
#44000 = CARTESIAN_POINT ( 'NONE',  ( -14.59287591719009924, 1436.244828798179924, 149.8708817315680051 ) ) ;
#44001 = ORIENTED_EDGE ( 'NONE', *, *, #31203, .T. ) ;
#44002 = CARTESIAN_POINT ( 'NONE',  ( -11.86607074870000034, 1432.333944652370064, 149.9824168324979894 ) ) ;
#44003 = CARTESIAN_POINT ( 'NONE',  ( 13.21847508789999992, 1443.021094946160019, 188.0964758581980050 ) ) ;
#44004 = VERTEX_POINT ( 'NONE', #60939 ) ;
#44005 = EDGE_LOOP ( 'NONE', ( #7092, #57092, #100662, #98488, #86274 ) ) ;
#44006 = CARTESIAN_POINT ( 'NONE',  ( -4.062020363349999386, 1454.690385904389814, 200.4959040790290032 ) ) ;
#44007 = CARTESIAN_POINT ( 'NONE',  ( 8.476942927299997876, 1362.523913559720086, 207.6218459616989946 ) ) ;
#44008 = CARTESIAN_POINT ( 'NONE',  ( -3.448206916814999801, 1516.904492006980036, 213.1642637479369853 ) ) ;
#44009 = CARTESIAN_POINT ( 'NONE',  ( 4.522891059284999571, 1511.193640125469983, 216.9700256452169924 ) ) ;
#44010 = EDGE_CURVE ( 'NONE', #69312, #55354, #65444, .T. ) ;
#44011 = AXIS2_PLACEMENT_3D ( 'NONE', #75472, #57569, #40189 ) ;
#44012 = ORIENTED_EDGE ( 'NONE', *, *, #1741, .F. ) ;
#44013 = CARTESIAN_POINT ( 'NONE',  ( -72.27662900180000349, 1379.712643070530021, 284.7775436246590175 ) ) ;
#44014 = CIRCLE ( 'NONE', #58317, 1.000000000000000000 ) ;
#44015 = EDGE_CURVE ( 'NONE', #108309, #7222, #65963, .T. ) ;
#44016 = CARTESIAN_POINT ( 'NONE',  ( 7.090792818829999788, 1414.913060387329779, 223.8701622068980157 ) ) ;
#44017 = CARTESIAN_POINT ( 'NONE',  ( -7.721907926364999675, 1517.026025493960105, 204.1173703575669833 ) ) ;
#44018 = CARTESIAN_POINT ( 'NONE',  ( -29.51517718210000041, 1509.962164600430015, 206.4717076456580003 ) ) ;
#44019 = CARTESIAN_POINT ( 'NONE',  ( -2.930838077694999821, 1510.983859056260144, 201.5581577403170002 ) ) ;
#44020 = CARTESIAN_POINT ( 'NONE',  ( -89.15725962140000149, 1385.072235092599840, 292.2573307935589924 ) ) ;
#44021 = CARTESIAN_POINT ( 'NONE',  ( -58.46619516613409928, 1384.663721486439954, 240.7616066048800008 ) ) ;
#44022 = CARTESIAN_POINT ( 'NONE',  ( -1.369507862000000076, 1408.899449949929931, 194.7487734720979802 ) ) ;
#44023 = CARTESIAN_POINT ( 'NONE',  ( -10.28013528708800095, 1471.607561417190027, 209.6293381314150110 ) ) ;
#44025 = ORIENTED_EDGE ( 'NONE', *, *, #66456, .F. ) ;
#44024 = CARTESIAN_POINT ( 'NONE',  ( -7.412346052360000215, 1445.966532708270051, 184.7546665820979968 ) ) ;
#44026 = CARTESIAN_POINT ( 'NONE',  ( 26.57328462079999909, 1469.248969691330103, 209.5010851783610235 ) ) ;
#44027 = CARTESIAN_POINT ( 'NONE',  ( 19.34119489396760017, 1467.092958138930044, 225.7365580626360213 ) ) ;
#44028 = ADVANCED_FACE ( 'NONE', ( #1573 ), #78410, .T. ) ;
#44029 = CARTESIAN_POINT ( 'NONE',  ( -24.99442991419999771, 1435.370276030620062, 135.8317735983980015 ) ) ;
#44030 = CARTESIAN_POINT ( 'NONE',  ( -2.864326125434999870, 1516.826109302209943, 211.6149197999869784 ) ) ;
#44031 = CARTESIAN_POINT ( 'NONE',  ( -68.54762064409999311, 1379.747581803159846, 279.6462198773589876 ) ) ;
#44032 = CARTESIAN_POINT ( 'NONE',  ( -14.06572158429999853, 1410.763503225130080, 226.9651548780980193 ) ) ;
#44033 = CARTESIAN_POINT ( 'NONE',  ( 4.363292141028189519, 1485.773534554989965, 215.9131765237970058 ) ) ;
#44034 = CARTESIAN_POINT ( 'NONE',  ( -11.60004869885203682, 1423.462184080423640, 135.7647354700178255 ) ) ;
#44035 = CARTESIAN_POINT ( 'NONE',  ( 6.550870144104999682, 1516.727502608469877, 208.3674577492799926 ) ) ;
#44036 = ORIENTED_EDGE ( 'NONE', *, *, #98919, .T. ) ;
#44037 = CARTESIAN_POINT ( 'NONE',  ( -1.910768082022130221, 1451.940451724439981, 184.3264785220040096 ) ) ;
#44038 = CARTESIAN_POINT ( 'NONE',  ( -11.44752262699999790, 1410.292588858030058, 228.7853414855979963 ) ) ;
#44039 = CARTESIAN_POINT ( 'NONE',  ( -25.94961989419999782, 1385.251886777470190, 224.2307850120589876 ) ) ;
#44040 = ORIENTED_EDGE ( 'NONE', *, *, #75729, .F. ) ;
#44041 = CARTESIAN_POINT ( 'NONE',  ( -11.90445094143569982, 1385.305240112880028, 218.9163558013920010 ) ) ;
#44042 = ADVANCED_FACE ( 'NONE', ( #25075 ), #94495, .T. ) ;
#44043 = CYLINDRICAL_SURFACE ( 'NONE', #54966, 0.5000000000000022204 ) ;
#44044 = CARTESIAN_POINT ( 'NONE',  ( 12.31419433885969994, 1434.254980775230024, 149.8258268142650138 ) ) ;
#44045 = CARTESIAN_POINT ( 'NONE',  ( 4.528451146867410237, 1478.701329350719789, 234.4837791156560058 ) ) ;
#44046 = CARTESIAN_POINT ( 'NONE',  ( -22.82526493734260242, 1509.659686721229946, 227.0554986310429797 ) ) ;
#44047 = EDGE_CURVE ( 'NONE', #93939, #80118, #8691, .T. ) ;
#44048 = FACE_OUTER_BOUND ( 'NONE', #17580, .T. ) ;
#44049 = CARTESIAN_POINT ( 'NONE',  ( 0.3074360972340000053, 1409.850187049029955, 233.1714481110979875 ) ) ;
#44050 = CARTESIAN_POINT ( 'NONE',  ( -0.1562598024478560055, 1420.468994851849857, 182.7540538292380177 ) ) ;
#44052 = CARTESIAN_POINT ( 'NONE',  ( -3.613094777869999774, 1419.785023685729811, 186.2978470366979877 ) ) ;
#44051 = CARTESIAN_POINT ( 'NONE',  ( 4.618749068485000109, 1516.729202374750002, 215.6716084172169872 ) ) ;
#44053 = CARTESIAN_POINT ( 'NONE',  ( 20.16473730159999889, 1508.103700731429853, 189.3367716560979943 ) ) ;
#44054 = CARTESIAN_POINT ( 'NONE',  ( 18.27965585607352494, 1424.887530935828636, 223.6444487662844267 ) ) ;
#44055 = ORIENTED_EDGE ( 'NONE', *, *, #21255, .T. ) ;
#44056 = CARTESIAN_POINT ( 'NONE',  ( -12.93261306534080113, 1416.826860677879949, 196.5036138660090046 ) ) ;
#44057 = CARTESIAN_POINT ( 'NONE',  ( -11.63188697299999852, 1495.113783641430018, 182.9907808364980042 ) ) ;
#44058 = ORIENTED_EDGE ( 'NONE', *, *, #82080, .T. ) ;
#44059 = CARTESIAN_POINT ( 'NONE',  ( 3.784406612299999750, 1421.548653729329999, 184.8121101002980140 ) ) ;
#44060 = B_SPLINE_CURVE_WITH_KNOTS ( 'NONE', 3,
 ( #69008, #43241, #86880, #103685, #44914, #94729 ),
 .UNSPECIFIED., .F., .F.,
 ( 4, 2, 4 ),
 ( -1.285435071114489149E-05, 0.001079388306740552582, 0.002171630964192249828 ),
 .UNSPECIFIED. ) ;
#44061 = EDGE_CURVE ( 'NONE', #88474, #63875, #39063, .T. ) ;
#44062 = CARTESIAN_POINT ( 'NONE',  ( -12.73491051959999965, 1505.539654372990071, 209.0093621724030015 ) ) ;
#44063 = CARTESIAN_POINT ( 'NONE',  ( 7.950581774744748920, 1511.645396655840159, 203.1073707467290319 ) ) ;
#44064 = CARTESIAN_POINT ( 'NONE',  ( 2.833473913299999758, 1441.452951622389946, 218.6297931320189889 ) ) ;
#44065 = CARTESIAN_POINT ( 'NONE',  ( -34.31402925621634381, 1524.244163922423695, 200.2096061136544165 ) ) ;
#44066 = CARTESIAN_POINT ( 'NONE',  ( -16.13536806862473227, 1409.511687815599998, 192.6629801062032072 ) ) ;
#44067 = CARTESIAN_POINT ( 'NONE',  ( 17.36801834879999973, 1414.983773852829927, 210.5058389443579756 ) ) ;
#44069 = EDGE_CURVE ( 'NONE', #26627, #3898, #18884, .T. ) ;
#44068 = CARTESIAN_POINT ( 'NONE',  ( -8.907440304760756433, 1432.353341358200169, 149.1004941874240330 ) ) ;
#44070 = CARTESIAN_POINT ( 'NONE',  ( -9.361711274563111473, 1459.704131987939718, 211.5409763055165797 ) ) ;
#44071 = CARTESIAN_POINT ( 'NONE',  ( 76.99707197885321364, 1524.382868172863937, 398.8876973329328735 ) ) ;
#44072 = FACE_OUTER_BOUND ( 'NONE', #71583, .T. ) ;
#44074 = CARTESIAN_POINT ( 'NONE',  ( -26.79413167943010166, 1436.761919080860025, 136.7821860765010058 ) ) ;
#44073 = CARTESIAN_POINT ( 'NONE',  ( -4.153788892804460176, 1419.995762630720037, 194.1221349337969855 ) ) ;
#44075 = CARTESIAN_POINT ( 'NONE',  ( 11.58615099567862572, 1433.820869185889478, 151.2068889330676598 ) ) ;
#44076 = ORIENTED_EDGE ( 'NONE', *, *, #72781, .F. ) ;
#44077 = CARTESIAN_POINT ( 'NONE',  ( 0.8911620065751310049, 1507.483750996730123, 186.2752927782370023 ) ) ;
#44078 = CARTESIAN_POINT ( 'NONE',  ( -4.987078446123650366, 1508.551704408389924, 211.6097672649169681 ) ) ;
#44079 = EDGE_CURVE ( 'NONE', #21233, #7608, #55473, .T. ) ;
#44080 = CARTESIAN_POINT ( 'NONE',  ( -23.84094907769999949, 1436.644390274100260, 212.4895236289980005 ) ) ;
#44081 = CARTESIAN_POINT ( 'NONE',  ( -9.956645445956299412, 1522.051704408389924, 185.5808665542169820 ) ) ;
#44082 = CARTESIAN_POINT ( 'NONE',  ( -3.819952067502766280, 1426.014366150848446, 186.0245215687357359 ) ) ;
#44083 = CARTESIAN_POINT ( 'NONE',  ( 33.28034951413933129, 1522.382868172863937, 217.4407153818819722 ) ) ;
#44084 = CARTESIAN_POINT ( 'NONE',  ( -11.38839566446790030, 1470.646819187970095, 209.6436936467169687 ) ) ;
#44085 = EDGE_CURVE ( 'NONE', #101117, #96069, #108863, .T. ) ;
#44087 = STYLED_ITEM ( 'NONE', ( #19160 ), #8479 ) ;
#44086 = CARTESIAN_POINT ( 'NONE',  ( -4.636579742356272682, 1378.025655545858172, 203.9278500733525732 ) ) ;
#44088 = CARTESIAN_POINT ( 'NONE',  ( 13.36059443969999982, 1414.988015881329829, 197.8813518256980046 ) ) ;
#44089 = CARTESIAN_POINT ( 'NONE',  ( -97.16214200120590760, 1383.765811092889862, 310.2586638610929413 ) ) ;
#44090 = DIRECTION ( 'NONE',  ( -0.9455185755993168462, -1.224646799147349756E-16, 0.3255681544571569219 ) ) ;
#44091 = CARTESIAN_POINT ( 'NONE',  ( -15.71383117100744897, 1506.606278695164519, 224.7011522283434033 ) ) ;
#44092 = CARTESIAN_POINT ( 'NONE',  ( -2.691174921192619696, 1516.547507499529956, 201.4124685881550079 ) ) ;
#44094 = EDGE_LOOP ( 'NONE', ( #7776, #96896, #60013, #58818 ) ) ;
#44093 = CARTESIAN_POINT ( 'NONE',  ( 10.35455463498039919, 1451.650344723270109, 207.2882537262890139 ) ) ;
#44095 = CARTESIAN_POINT ( 'NONE',  ( -1.547463840030000037, 1414.913060387329779, 225.9340782259980074 ) ) ;
#44096 = CARTESIAN_POINT ( 'NONE',  ( -62.63809935099999393, 1382.333481460739904, 284.4251248683589779 ) ) ;
#44097 = DIRECTION ( 'NONE',  ( -1.049689422327477382E-06, 0.03085829058775882774, 0.9995237695527303678 ) ) ;
#44098 = ORIENTED_EDGE ( 'NONE', *, *, #96325, .F. ) ;
#44099 = ORIENTED_EDGE ( 'NONE', *, *, #104518, .F. ) ;
#44100 = CARTESIAN_POINT ( 'NONE',  ( 20.04661031711670205, 1509.276535231649859, 229.7844010504510095 ) ) ;
#44101 = CARTESIAN_POINT ( 'NONE',  ( 29.82178186784435425, 1526.306647125543122, 201.3257788173809786 ) ) ;
#44102 = CARTESIAN_POINT ( 'NONE',  ( 38.03973805443759915, 1438.663203083320013, 136.6110655224219954 ) ) ;
#44103 = VECTOR ( 'NONE', #67845, 1000.000000000000227 ) ;
#44105 = CARTESIAN_POINT ( 'NONE',  ( -42.46017262339999832, 1454.582918749130158, 266.3334795814980112 ) ) ;
#44104 = CARTESIAN_POINT ( 'NONE',  ( 15.89205235460757315, 1412.672487590961282, 269.3685437928070883 ) ) ;
#44106 = EDGE_CURVE ( 'NONE', #59255, #6406, #71353, .T. ) ;
#44107 = B_SPLINE_CURVE_WITH_KNOTS ( 'NONE', 5,
 ( #71611, #20578, #105168, #95107, #28458, #54778, #27344, #87261, #79420 ),
 .UNSPECIFIED., .F., .F.,
 ( 6, 3, 6 ),
 ( 0.000000000000000000, 0.6011310882172063996, 1.000000000000000000 ),
 .UNSPECIFIED. ) ;
#44108 = CARTESIAN_POINT ( 'NONE',  ( 8.591050007833809232, 1437.123692357109803, 208.1883534641620201 ) ) ;
#44109 = B_SPLINE_CURVE_WITH_KNOTS ( 'NONE', 5,
 ( #22690, #98874, #45752, #56339, #13747, #3752 ),
 .UNSPECIFIED., .F., .F.,
 ( 6, 6 ),
 ( 14.91778147325059933, 22.01924661119420890 ),
 .UNSPECIFIED. ) ;
#44110 = CARTESIAN_POINT ( 'NONE',  ( -109.4610122139999930, 1384.463034823889984, 297.1307535903590065 ) ) ;
#44111 = CARTESIAN_POINT ( 'NONE',  ( -11.29932808600985972, 1434.474993683731782, 151.5487048912618206 ) ) ;
#44112 = CARTESIAN_POINT ( 'NONE',  ( 19.63722818094939981, 1517.051704408389924, 218.2362632588020119 ) ) ;
#44113 = CARTESIAN_POINT ( 'NONE',  ( 2.025968481520000086, 1408.983808766029824, 186.4771966811979951 ) ) ;
#44114 = CARTESIAN_POINT ( 'NONE',  ( 4.714441181029999761, 1423.953913941430073, 185.0673980490979886 ) ) ;
#44116 = EDGE_CURVE ( 'NONE', #55027, #63956, #19400, .T. ) ;
#44115 = CARTESIAN_POINT ( 'NONE',  ( -6.686616183240000844, 1441.247408104989972, 154.4574209342979998 ) ) ;
#44117 = CARTESIAN_POINT ( 'NONE',  ( -9.207216801295770026, 1450.122646856020083, 208.9920191583770190 ) ) ;
#44118 = CARTESIAN_POINT ( 'NONE',  ( -12.67427553544369800, 1422.533749357050056, 203.9427823080079918 ) ) ;
#44119 = CARTESIAN_POINT ( 'NONE',  ( 0.004285590335689999815, 1452.913210043329855, 152.9533009523979956 ) ) ;
#44120 = FACE_OUTER_BOUND ( 'NONE', #102301, .T. ) ;
#44121 = ORIENTED_EDGE ( 'NONE', *, *, #40687, .F. ) ;
#44122 = CARTESIAN_POINT ( 'NONE',  ( -11.64264026049999856, 1508.093831663089986, 207.6305009244389908 ) ) ;
#44123 = CARTESIAN_POINT ( 'NONE',  ( 4.831085042146060715, 1471.573324702249920, 187.7042132603309881 ) ) ;
#44124 = CARTESIAN_POINT ( 'NONE',  ( -44.50818758269999620, 1445.910501413080055, 269.6919245774980141 ) ) ;
#44125 = FACE_OUTER_BOUND ( 'NONE', #3365, .T. ) ;
#44126 = CARTESIAN_POINT ( 'NONE',  ( 9.587366264599999965, 1440.450814879359996, 153.1449006345979740 ) ) ;
#44127 = DIRECTION ( 'NONE',  ( 0.000000000000000000, 0.000000000000000000, -1.000000000000000000 ) ) ;
#44128 = CARTESIAN_POINT ( 'NONE',  ( -2.330134118790000208, 1515.551704408389924, 212.9514660756190096 ) ) ;
#44129 = CARTESIAN_POINT ( 'NONE',  ( 2.801091625889360337, 1409.037716335049936, 230.4781056456209853 ) ) ;
#44130 = CARTESIAN_POINT ( 'NONE',  ( 31.23437356469435144, 1511.187213306747708, 195.3468678195113739 ) ) ;
#44131 = CARTESIAN_POINT ( 'NONE',  ( -4.245035385839999620, 1415.991794987329968, 232.3966682199979914 ) ) ;
#44132 = B_SPLINE_CURVE_WITH_KNOTS ( 'NONE', 5,
 ( #55229, #22118, #48481, #31649, #46832, #38937 ),
 .UNSPECIFIED., .F., .F.,
 ( 6, 6 ),
 ( -2.000000000000000000, -9.120498578596425432E-09 ),
 .UNSPECIFIED. ) ;
#44133 = CARTESIAN_POINT ( 'NONE',  ( -1.229877626282320779, 1484.645096144196486, 182.2669562530408598 ) ) ;
#44134 = CARTESIAN_POINT ( 'NONE',  ( -4.360754392635079135, 1358.792723554605345, 209.6218459617033432 ) ) ;
#44135 = CARTESIAN_POINT ( 'NONE',  ( -46.00986170831419741, 1439.835802669839950, 268.4966223753010581 ) ) ;
#44136 = LINE ( 'NONE', #10520, #24691 ) ;
#44137 = ORIENTED_EDGE ( 'NONE', *, *, #33831, .T. ) ;
#44138 = CARTESIAN_POINT ( 'NONE',  ( -9.200421029710000198, 1422.937291652149952, 210.7384574684489849 ) ) ;
#44139 = EDGE_LOOP ( 'NONE', ( #59855, #51605, #16347, #42094 ) ) ;
#44140 = CARTESIAN_POINT ( 'NONE',  ( -3.449647478144999724, 1516.829948096479939, 209.8791439064560223 ) ) ;
#44141 = CARTESIAN_POINT ( 'NONE',  ( -9.216856378879999312, 1385.697103985929971, 200.0334226857090130 ) ) ;
#44142 = CARTESIAN_POINT ( 'NONE',  ( -27.22940015632950050, 1441.374094644329944, 137.3495836813739857 ) ) ;
#44143 = CARTESIAN_POINT ( 'NONE',  ( 7.479962015650619023, 1426.053219697059831, 212.3726218137090029 ) ) ;
#44144 = VECTOR ( 'NONE', #64077, 1000.000000000000227 ) ;
#44145 = CARTESIAN_POINT ( 'NONE',  ( -2.670576961741749855, 1496.965622226749929, 221.2123459303559798 ) ) ;
#44146 = VERTEX_POINT ( 'NONE', #72111 ) ;
#44147 = FACE_OUTER_BOUND ( 'NONE', #61674, .T. ) ;
#44149 = CARTESIAN_POINT ( 'NONE',  ( 15.95383384960000228, 1506.798305107329952, 193.5571554442980187 ) ) ;
#44148 = CARTESIAN_POINT ( 'NONE',  ( -14.45750500688560081, 1416.828039245989885, 221.3916439204320170 ) ) ;
#44150 = CARTESIAN_POINT ( 'NONE',  ( 6.942354273414999888, 1516.905946377369901, 201.4030824261969883 ) ) ;
#44151 = CARTESIAN_POINT ( 'NONE',  ( -11.58491445499556072, 1426.183919005333564, 138.6952712166350352 ) ) ;
#44152 = CARTESIAN_POINT ( 'NONE',  ( -17.60611312488026670, 1410.890515041045774, 194.4989067822270101 ) ) ;
#44153 = CARTESIAN_POINT ( 'NONE',  ( -8.510946600262379036, 1439.450974936100238, 206.5611942902239946 ) ) ;
#44154 = VERTEX_POINT ( 'NONE', #45797 ) ;
#44155 = CARTESIAN_POINT ( 'NONE',  ( -6.865870934037390683, 1408.020560016030004, 270.1275732224370358 ) ) ;
#44156 = CARTESIAN_POINT ( 'NONE',  ( 5.000329995535000016, 1516.770163853809890, 208.3657552043160024 ) ) ;
#44157 = CARTESIAN_POINT ( 'NONE',  ( 4.872266624350030106, 1418.137296580060138, 233.6603738433760213 ) ) ;
#44158 = CARTESIAN_POINT ( 'NONE',  ( 8.534077335428490230, 1434.919601520179867, 206.3687546489890110 ) ) ;
#44160 = VERTEX_POINT ( 'NONE', #46351 ) ;
#44159 = CARTESIAN_POINT ( 'NONE',  ( -4.105920213440668931, 1367.121443183097654, 208.3718459617061285 ) ) ;
#44161 = VERTEX_POINT ( 'NONE', #105694 ) ;
#44162 = CARTESIAN_POINT ( 'NONE',  ( -23.52688643275999780, 1410.415118700949961, 210.2554788044750183 ) ) ;
#44163 = CARTESIAN_POINT ( 'NONE',  ( -4.193899600139999961, 1425.337788341129908, 186.1504193666980029 ) ) ;
#44164 = CARTESIAN_POINT ( 'NONE',  ( -22.08622291482314282, 1523.456872492435195, 233.8253038720786776 ) ) ;
#44165 = CARTESIAN_POINT ( 'NONE',  ( 0.0001408309371566590163, 1408.913070111550269, 186.4658721391990071 ) ) ;
#44166 = CIRCLE ( 'NONE', #79965, 1.000000000000000888 ) ;
#44167 = CARTESIAN_POINT ( 'NONE',  ( -19.25467140439389624, 1450.982098615540281, 193.9791526570050166 ) ) ;
#44168 = CARTESIAN_POINT ( 'NONE',  ( -19.73265327440000050, 1425.811828412130126, 222.9530360735979855 ) ) ;
#44169 = CARTESIAN_POINT ( 'NONE',  ( 30.03031303698100274, 1467.498499503609992, 266.8645947477900222 ) ) ;
#44170 = CARTESIAN_POINT ( 'NONE',  ( -11.67229379317850047, 1391.913060387289988, 209.5769804851749996 ) ) ;
#44171 = DIRECTION ( 'NONE',  ( -1.744230429721540409E-14, -1.000000000000000000, -3.290755053036525162E-15 ) ) ;
#44172 =( BOUNDED_CURVE ( )  B_SPLINE_CURVE ( 3, ( #103025, #42589, #16255, #76742 ),
 .UNSPECIFIED., .F., .T. ) 
 B_SPLINE_CURVE_WITH_KNOTS ( ( 4, 4 ),
 ( 1.704095840793119931, 2.349013555596815017 ),
 .UNSPECIFIED. ) 
 CURVE ( )  GEOMETRIC_REPRESENTATION_ITEM ( )  RATIONAL_B_SPLINE_CURVE ( ( 1.000000000000000000, 0.9656393833455322318, 0.9656393833455322318, 1.000000000000000000 ) ) 
 REPRESENTATION_ITEM ( '' )  );
#44173 = CARTESIAN_POINT ( 'NONE',  ( -4.042729840925000317, 1516.919782530640077, 205.8674445284970034 ) ) ;
#44174 = ORIENTED_EDGE ( 'NONE', *, *, #2886, .T. ) ;
#44175 = CARTESIAN_POINT ( 'NONE',  ( 23.59369949126165622, 1411.097251101419033, 211.5720139885703190 ) ) ;
#44176 = CARTESIAN_POINT ( 'NONE',  ( 1.501870405408500142, 1464.999530953469957, 182.9509895119559815 ) ) ;
#44177 = CARTESIAN_POINT ( 'NONE',  ( 22.77443950849999865, 1409.708263161830018, 208.9272941533559731 ) ) ;
#44178 = ORIENTED_EDGE ( 'NONE', *, *, #69455, .T. ) ;
#44179 = CARTESIAN_POINT ( 'NONE',  ( 2.487924095911270062, 1509.038643251730036, 204.6345969343269928 ) ) ;
#44180 = CARTESIAN_POINT ( 'NONE',  ( 25.91250833790000030, 1451.849349898129958, 135.8364949240979911 ) ) ;
#44181 = CARTESIAN_POINT ( 'NONE',  ( -22.43804543029999721, 1409.696614199630176, 210.2088496164680009 ) ) ;
#44182 = CARTESIAN_POINT ( 'NONE',  ( -4.649084002151809292E-16, 1389.634744113780243, 202.9789274992690196 ) ) ;
#44183 = DIRECTION ( 'NONE',  ( -0.6742693640208961003, 0.000000000000000000, -0.7384854939285241393 ) ) ;
#44184 = CARTESIAN_POINT ( 'NONE',  ( 17.37384703899999749, 1410.444760247230079, 192.4767873331980184 ) ) ;
#44185 = CARTESIAN_POINT ( 'NONE',  ( 27.68130203340000151, 1444.740067931809790, 168.8183730152979933 ) ) ;
#44187 = CARTESIAN_POINT ( 'NONE',  ( -14.04273730155982847, 1379.586150356219150, 211.8481849348019921 ) ) ;
#44186 = CARTESIAN_POINT ( 'NONE',  ( 1.665296718610000060, 1417.520169485130054, 234.6989198356980069 ) ) ;
#44188 = CARTESIAN_POINT ( 'NONE',  ( 1.127302894264770039, 1450.859558279620160, 182.1360551162379977 ) ) ;
#44189 = VECTOR ( 'NONE', #10734, 1000.000000000000227 ) ;
#44190 = DIRECTION ( 'NONE',  ( -1.000000000000000000, 0.000000000000000000, 0.000000000000000000 ) ) ;
#44191 = CARTESIAN_POINT ( 'NONE',  ( -9.137732587340000379, 1383.146477076719975, 218.2898102310589934 ) ) ;
#44192 = CARTESIAN_POINT ( 'NONE',  ( 0.7560907277860019482, 1516.770163853809890, 214.1221759657669850 ) ) ;
#44193 = CARTESIAN_POINT ( 'NONE',  ( 2.214867471995963566, 1525.730671948510917, 241.5483233331381427 ) ) ;
#44194 = ORIENTED_EDGE ( 'NONE', *, *, #97844, .T. ) ;
#44195 = DIRECTION ( 'NONE',  ( 0.000000000000000000, 1.000000000000000000, 0.000000000000000000 ) ) ;
#44196 = CARTESIAN_POINT ( 'NONE',  ( 0.8903091994049979752, 1462.735716105790061, 228.8847082000989985 ) ) ;
#44198 = DIRECTION ( 'NONE',  ( 0.000000000000000000, 1.000000000000000000, 0.000000000000000000 ) ) ;
#44197 = B_SPLINE_CURVE_WITH_KNOTS ( 'NONE', 3,
 ( #23899, #49145, #23362, #91125, #40173, #84381, #59203, #68166, #57552, #92226, #93321, #110131, #101707, #49695, #91675, #14948, #66512, #100615, #16583, #83824 ),
 .UNSPECIFIED., .F., .F.,
 ( 4, 2, 1, 2, 2, 1, 1, 1, 1, 1, 2, 2, 4 ),
 ( 0.000000000000000000, 0.2500000000002167155, 0.3750000000003254064, 0.4375000000003794187, 0.5000000000004334311, 0.6250000000005402345, 0.6875000000005936363, 0.7187500000006207257, 0.7343750000006342704, 0.7421875000006368239, 0.7460937500006337153, 0.7500000000006307177, 1.000000000000000000 ),
 .UNSPECIFIED. ) ;
#44199 = DIRECTION ( 'NONE',  ( -0.01484500364079635246, -0.5669078173018518019, 0.8236474686107856380 ) ) ;
#44200 = DIRECTION ( 'NONE',  ( -1.699538841806929935E-33, 1.000000000000000000, -1.698192320643030073E-16 ) ) ;
#44201 = CARTESIAN_POINT ( 'NONE',  ( -4.329448776040000446, 1515.064792882589927, 207.3534014088789945 ) ) ;
#44202 = EDGE_CURVE ( 'NONE', #27485, #53857, #8635, .T. ) ;
#44203 = CARTESIAN_POINT ( 'NONE',  ( -18.57221552470000248, 1447.675799122940134, 219.6133833292979887 ) ) ;
#44204 = CARTESIAN_POINT ( 'NONE',  ( -14.42895190569277730, 1415.865101995087116, 203.8800253993052536 ) ) ;
#44206 = EDGE_CURVE ( 'NONE', #65542, #4206, #79378, .T. ) ;
#44205 = CARTESIAN_POINT ( 'NONE',  ( 11.89943377740000052, 1433.335282505560144, 150.1709607732979919 ) ) ;
#44207 = CARTESIAN_POINT ( 'NONE',  ( 3.114882401749999641, 1454.846680951630105, 214.3676144197979738 ) ) ;
#44208 = CARTESIAN_POINT ( 'NONE',  ( 26.33767527485199977, 1440.913060395190087, 223.6248100573809836 ) ) ;
#44209 = CARTESIAN_POINT ( 'NONE',  ( -17.22999524109999925, 1421.609273190410022, 201.8193996009690068 ) ) ;
#44210 = CARTESIAN_POINT ( 'NONE',  ( -32.66476241579324125, 1526.382868172863937, 199.1278258474841891 ) ) ;
#44211 = CARTESIAN_POINT ( 'NONE',  ( 24.97896770994293547, 1436.441713528391574, 137.9167425154915918 ) ) ;
#44212 = FACE_OUTER_BOUND ( 'NONE', #87766, .T. ) ;
#44213 = CARTESIAN_POINT ( 'NONE',  ( -1.488474718485068182, 1526.348417187222367, 239.9133697138384775 ) ) ;
#44214 = CARTESIAN_POINT ( 'NONE',  ( -25.47742517682650032, 1509.802751679349967, 193.2942475626609848 ) ) ;
#44215 = CARTESIAN_POINT ( 'NONE',  ( 22.97761738710000046, 1449.791915361709925, 218.1846805547179997 ) ) ;
#44216 = VECTOR ( 'NONE', #43555, 1000.000000000000227 ) ;
#44217 = EDGE_CURVE ( 'NONE', #68701, #48151, #5103, .T. ) ;
#44218 = CARTESIAN_POINT ( 'NONE',  ( -17.47221698915792487, 1419.835909614559569, 206.8863186588654060 ) ) ;
#44219 = CARTESIAN_POINT ( 'NONE',  ( -41.62601876731983452, 1442.681032278104794, 135.5698701779593023 ) ) ;
#44220 = CARTESIAN_POINT ( 'NONE',  ( -14.04325441188020207, 1383.859464698529791, 219.0769673503140211 ) ) ;
#44221 = CARTESIAN_POINT ( 'NONE',  ( -22.15968324266369649, 1485.573346209269857, 217.2083651811669824 ) ) ;
#44222 = CARTESIAN_POINT ( 'NONE',  ( 5.010422963235000360, 1516.929569650079884, 213.1529883219070030 ) ) ;
#44223 = CARTESIAN_POINT ( 'NONE',  ( 203.9558787908000284, -8382.262153571269664, -1760.903728536709878 ) ) ;
#44224 = CARTESIAN_POINT ( 'NONE',  ( 0.1670098483671519918, 1482.089753829420033, 182.0046196815349901 ) ) ;
#44225 = B_SPLINE_CURVE_WITH_KNOTS ( 'NONE', 3,
 ( #4477, #45393, #3389, #5008, #62196, #106372, #39155, #79532, #29660, #37517, #2835, #71720 ),
 .UNSPECIFIED., .F., .F.,
 ( 4, 2, 2, 2, 2, 4 ),
 ( -0.1123552150373909875, -0.09789198304339560841, -0.08346217084110789386, -0.05408911861973839802, -0.02844403185827369673, -2.821858199469895467E-07 ),
 .UNSPECIFIED. ) ;
#44227 = ORIENTED_EDGE ( 'NONE', *, *, #65051, .T. ) ;
#44226 = CARTESIAN_POINT ( 'NONE',  ( 2.999852707240000083, 1441.831684494889942, 217.8331580874990152 ) ) ;
#44228 = CARTESIAN_POINT ( 'NONE',  ( -0.7130990469979998636, 1416.837309316629899, 227.9189225404980164 ) ) ;
#44229 = CARTESIAN_POINT ( 'NONE',  ( -9.104488441191636028, 1388.370946186080118, 200.6891223300711431 ) ) ;
#44230 = CARTESIAN_POINT ( 'NONE',  ( 5.386185205460879644, 1432.347042709529887, 154.6076275981190236 ) ) ;
#44232 = ORIENTED_EDGE ( 'NONE', *, *, #66245, .T. ) ;
#44231 = CARTESIAN_POINT ( 'NONE',  ( -32.36539537780667786, 1523.843271061948144, 216.1095012219382454 ) ) ;
#44233 = CARTESIAN_POINT ( 'NONE',  ( 14.43087674896799832, 1426.807405976119981, 195.4949895358049901 ) ) ;
#44234 = ORIENTED_EDGE ( 'NONE', *, *, #107818, .T. ) ;
#44235 = CARTESIAN_POINT ( 'NONE',  ( -14.42899799073379974, 1380.189325286879921, 209.0990684340630139 ) ) ;
#44236 = CARTESIAN_POINT ( 'NONE',  ( -15.60349157319999769, 1415.087797054229895, 216.5108232632080103 ) ) ;
#44237 = CARTESIAN_POINT ( 'NONE',  ( -8.991629940588330427, 1509.227055023859975, 237.0095830223739881 ) ) ;
#44238 = CARTESIAN_POINT ( 'NONE',  ( 22.57319362359999815, 1409.701316935530031, 208.7927549349429910 ) ) ;
#44239 = CARTESIAN_POINT ( 'NONE',  ( 0.1274077701469989998, 1431.278402656690105, 217.8904900432389979 ) ) ;
#44240 = CARTESIAN_POINT ( 'NONE',  ( -10.84355950384670209, 1471.555694810890145, 206.8501174806650056 ) ) ;
#44241 = CONICAL_SURFACE ( 'NONE', #110411, 12.49999999999999467, 0.02617993877989872875 ) ;
#44242 = CARTESIAN_POINT ( 'NONE',  ( 14.66484709975379985, 1409.425168132260069, 211.9475575867689940 ) ) ;
#44243 = CARTESIAN_POINT ( 'NONE',  ( -12.46299153120000014, 1391.583714740810137, 209.2286840156340020 ) ) ;
#44244 = CARTESIAN_POINT ( 'NONE',  ( -76.82411996085400574, 1385.144362471309933, 278.4876237131520043 ) ) ;
#44245 = EDGE_CURVE ( 'NONE', #81044, #10869, #58749, .T. ) ;
#44246 = CARTESIAN_POINT ( 'NONE',  ( -17.36186237040000080, 1412.953349025430043, 192.1948984129979863 ) ) ;
#44247 = CARTESIAN_POINT ( 'NONE',  ( -65.30777065759998834, 1379.749275567730137, 273.2377066393590326 ) ) ;
#44248 = ORIENTED_EDGE ( 'NONE', *, *, #26107, .T. ) ;
#44249 = CARTESIAN_POINT ( 'NONE',  ( 11.68008220344320058, 1491.335982786950126, 207.1828859132960190 ) ) ;
#44251 = EDGE_LOOP ( 'NONE', ( #38977, #32973, #10328, #100053 ) ) ;
#44250 = CARTESIAN_POINT ( 'NONE',  ( -0.4151546846821903003, 1512.187213306747481, 175.3106345060153046 ) ) ;
#44252 = CARTESIAN_POINT ( 'NONE',  ( -19.50375265270000114, 1467.690089012490034, 205.2528463378490073 ) ) ;
#44253 = ORIENTED_EDGE ( 'NONE', *, *, #14410, .F. ) ;
#44254 = ADVANCED_FACE ( 'NONE', ( #45241 ), #35557, .T. ) ;
#44255 = CARTESIAN_POINT ( 'NONE',  ( -18.50490982315079691, 1441.562997674779808, 211.9760908666659986 ) ) ;
#44256 = CARTESIAN_POINT ( 'NONE',  ( -8.622403150219998480, 1362.632156860360055, 207.6218459616989946 ) ) ;
#44257 = DIRECTION ( 'NONE',  ( 0.000000000000000000, -1.000000000000000000, 0.000000000000000000 ) ) ;
#44258 = CARTESIAN_POINT ( 'NONE',  ( 32.58707754757925557, 1460.160100176146443, 269.5002707768942400 ) ) ;
#44259 = DIRECTION ( 'NONE',  ( 5.312590645178966993E-15, 0.000000000000000000, 1.000000000000000000 ) ) ;
#44260 = CARTESIAN_POINT ( 'NONE',  ( -28.04656858090000071, 1508.051246290529889, 210.1181873726100093 ) ) ;
#44261 = CARTESIAN_POINT ( 'NONE',  ( 32.35345263957275108, 1524.872178180562969, 201.1945832501413634 ) ) ;
#44262 = CARTESIAN_POINT ( 'NONE',  ( -7.078000874848796364, 1516.557769095839603, 211.6025370379481672 ) ) ;
#44263 = CARTESIAN_POINT ( 'NONE',  ( -8.323380306660000727, 1512.192073244490075, 211.6849953306190173 ) ) ;
#44264 = CARTESIAN_POINT ( 'NONE',  ( -8.297911554434026726, 1368.614765545475393, 207.6218459616987673 ) ) ;
#44265 = CARTESIAN_POINT ( 'NONE',  ( -15.90854778520130175, 1487.107804145120099, 195.7315998840579994 ) ) ;
#44266 = CARTESIAN_POINT ( 'NONE',  ( 1.186695575399999925, 1456.165747688890178, 198.6030552828989926 ) ) ;
#44267 = CARTESIAN_POINT ( 'NONE',  ( -4.043990345725000601, 1516.983612918759945, 206.6425990843970055 ) ) ;
#44268 = AXIS2_PLACEMENT_3D ( 'NONE', #18831, #68728, #87162 ) ;
#44269 = DIRECTION ( 'NONE',  ( -0.000000000000000000, -1.000000000000000000, -0.000000000000000000 ) ) ;
#44270 = CARTESIAN_POINT ( 'NONE',  ( -15.68560764121220252, 1410.853875961199947, 226.7268370761429992 ) ) ;
#44271 = CARTESIAN_POINT ( 'NONE',  ( -2.924124371280000023, 1495.932676772589957, 197.5380625559990051 ) ) ;
#44273 = ORIENTED_EDGE ( 'NONE', *, *, #75563, .T. ) ;
#44272 = CARTESIAN_POINT ( 'NONE',  ( -2.781330248550000217, 1495.730979733589948, 219.9850975371990103 ) ) ;
#44274 = CARTESIAN_POINT ( 'NONE',  ( -33.92723111727409702, 1435.682240498233568, 135.5030908501479985 ) ) ;
#44275 = VERTEX_POINT ( 'NONE', #90516 ) ;
#44276 = CARTESIAN_POINT ( 'NONE',  ( 13.49160166387382453, 1516.729020965289010, 192.0695843282071849 ) ) ;
#44277 = CARTESIAN_POINT ( 'NONE',  ( -25.75587219220000179, 1449.806259877490220, 208.7857563948580264 ) ) ;
#44279 = CARTESIAN_POINT ( 'NONE',  ( 17.20497987027239972, 1410.737466176999988, 192.2100592557800098 ) ) ;
#44278 = CARTESIAN_POINT ( 'NONE',  ( -11.24451365029999828, 1426.879224447430033, 108.4514502916979950 ) ) ;
#44280 = CARTESIAN_POINT ( 'NONE',  ( -2.477373643995000485, 1516.891731298979948, 212.0030687278169808 ) ) ;
#44281 = CARTESIAN_POINT ( 'NONE',  ( 15.70278030267772351, 1509.582838606658015, 183.5495200154611837 ) ) ;
#44282 = CARTESIAN_POINT ( 'NONE',  ( -21.99073835760000151, 1489.474306033830089, 208.3865218840309979 ) ) ;
#44283 = CARTESIAN_POINT ( 'NONE',  ( -33.60183515869999837, 1438.777037856849802, 248.0844435640979668 ) ) ;
#44284 = CARTESIAN_POINT ( 'NONE',  ( 17.06289018075510100, 1509.516276409990041, 233.1776295764580027 ) ) ;
#44285 = CARTESIAN_POINT ( 'NONE',  ( 28.75826058055400125, 1509.399771093630079, 209.5084960995969823 ) ) ;
#44286 = CARTESIAN_POINT ( 'NONE',  ( 4.860123680919410383, 1508.551704408389924, 212.3962593222019848 ) ) ;
#44287 = CARTESIAN_POINT ( 'NONE',  ( 30.80316622530000004, 1451.837341253830118, 134.8070091183980139 ) ) ;
#44288 = ORIENTED_EDGE ( 'NONE', *, *, #29464, .F. ) ;
#44289 = CARTESIAN_POINT ( 'NONE',  ( 5.776208867308529449, 1396.296062051389981, 219.5799282863600013 ) ) ;
#44290 = CARTESIAN_POINT ( 'NONE',  ( 9.170246928576359480, 1461.406349500210126, 205.9599371887860002 ) ) ;
#44291 = CARTESIAN_POINT ( 'NONE',  ( -17.93598132460000016, 1458.546043109529819, 228.2699785320980084 ) ) ;
#44292 = ORIENTED_EDGE ( 'NONE', *, *, #108894, .F. ) ;
#44293 = ORIENTED_EDGE ( 'NONE', *, *, #41252, .F. ) ;
#44294 = CIRCLE ( 'NONE', #58601, 0.5869955059086555682 ) ;
#44295 = FACE_OUTER_BOUND ( 'NONE', #93979, .T. ) ;
#44296 = CARTESIAN_POINT ( 'NONE',  ( -3.181555658762940109, 1425.362665593959946, 153.9433765262999998 ) ) ;
#44297 = ORIENTED_EDGE ( 'NONE', *, *, #87963, .T. ) ;
#44298 = CARTESIAN_POINT ( 'NONE',  ( 0.5133923723890000401, 1410.300673476330076, 185.0724364044980348 ) ) ;
#44299 = B_SPLINE_CURVE_WITH_KNOTS ( 'NONE', 3,
 ( #84400, #83845, #7144, #42959, #41301, #41845, #67619, #67072, #51346, #57570, #85479, #24472, #60315, #19947, #54140, #11010, #1515, #18280, #88269, #35648, #78203, #70953, #69837, #86056, #61435 ),
 .UNSPECIFIED., .F., .F.,
 ( 4, 3, 3, 3, 3, 3, 3, 3, 4 ),
 ( -3.202470023179999625, -2.306874149981480215, -1.412366672554860036, -0.5199827250689450509, -0.01259353077460012571, 0.6689285225653880396, 1.550313525218030453, 2.444820790987910275, 3.202470023179999625 ),
 .UNSPECIFIED. ) ;
#44300 = DIRECTION ( 'NONE',  ( -0.6736849260863841948, 0.000000000000000000, 0.7390186874254148774 ) ) ;
#44301 = CARTESIAN_POINT ( 'NONE',  ( -0.02516806119179999801, 1415.404723302029879, 233.4400559027980080 ) ) ;
#44302 = CARTESIAN_POINT ( 'NONE',  ( 27.23667244607642601, 1509.093166509125922, 206.1841183845450587 ) ) ;
#44303 = CARTESIAN_POINT ( 'NONE',  ( 5.513222313296060051, 1508.611138448520023, 201.8002184229020202 ) ) ;
#44304 = CARTESIAN_POINT ( 'NONE',  ( 9.229093028962669365, 1450.500814747789946, 209.1422214426999915 ) ) ;
#44305 = CARTESIAN_POINT ( 'NONE',  ( 19.40352163639999716, 1457.233006875389947, 208.1928089228509862 ) ) ;
#44306 = CARTESIAN_POINT ( 'NONE',  ( -97.97730939973499176, 1384.867588345430022, 295.8314372660599929 ) ) ;
#44307 = CARTESIAN_POINT ( 'NONE',  ( 3.452289182574999948, 1517.069378699710114, 202.5601595088670024 ) ) ;
#44308 = CARTESIAN_POINT ( 'NONE',  ( 7.339107202615000602, 1517.203017563489766, 210.2473558205170150 ) ) ;
#44309 = EDGE_LOOP ( 'NONE', ( #61847, #81063, #52305, #73759, #25608, #76225, #31136, #19027, #72141, #3681, #27673, #38883, #30100, #31442, #66796, #21577, #78989, #74053, #82243, #101700, #10116, #55124, #97602, #95550, #82925, #17655, #10409, #100125, #74874, #41784, #36848, #86784, #86679, #5210, #87196, #50894, #90912, #100526, #22609, #67417 ) ) ;
#44310 = CARTESIAN_POINT ( 'NONE',  ( 11.84842883606899910, 1431.111952647210046, 149.8465606311750093 ) ) ;
#44311 = B_SPLINE_CURVE_WITH_KNOTS ( 'NONE', 3,
 ( #46714, #21453, #39939, #23118, #6335, #55664, #22547, #108239, #48915, #14171, #89786, #71938, #98736, #30429, #106050, #14725, #29327, #21996, #13057 ),
 .UNSPECIFIED., .F., .F.,
 ( 4, 3, 3, 3, 3, 3, 4 ),
 ( -7.154418202789190495, -6.862826068025819737, -5.884430753544330095, -5.043863493629519468, -4.380177091811430223, -3.634519997509699785, -2.933308256780000178 ),
 .UNSPECIFIED. ) ;
#44312 = CARTESIAN_POINT ( 'NONE',  ( -9.129808743239919977, 1383.863787745319996, 218.5279288296370055 ) ) ;
#44313 = CARTESIAN_POINT ( 'NONE',  ( 5.513435558552500559, 1508.909942010212490, 201.6124651694741488 ) ) ;
#44314 = ORIENTED_EDGE ( 'NONE', *, *, #109775, .T. ) ;
#44315 = CARTESIAN_POINT ( 'NONE',  ( -1.459250905673769916, 1476.185953128230267, 182.8314277312189802 ) ) ;
#44316 = CARTESIAN_POINT ( 'NONE',  ( -5.904615859283640411, 1508.524893063339960, 219.7761321644620125 ) ) ;
#44317 = FACE_OUTER_BOUND ( 'NONE', #109151, .T. ) ;
#44318 = CARTESIAN_POINT ( 'NONE',  ( -31.81407709660762606, 1522.862737210649811, 221.9534378623334874 ) ) ;
#44319 = CARTESIAN_POINT ( 'NONE',  ( -5.549327278860000767, 1424.136432490230163, 186.3245620642980214 ) ) ;
#44320 = CARTESIAN_POINT ( 'NONE',  ( 3.437535550059239942, 1409.880280454960257, 270.0719098211940263 ) ) ;
#44321 = CARTESIAN_POINT ( 'NONE',  ( -104.3158487040000040, 1389.466353268959892, 300.6607691406589993 ) ) ;
#44322 = CARTESIAN_POINT ( 'NONE',  ( -2.956771579574999809, 1512.877808311729950, 201.2153269223470033 ) ) ;
#44323 = CARTESIAN_POINT ( 'NONE',  ( 8.810981746659999558, 1493.003242455989721, 216.1956613704689971 ) ) ;
#44324 = CARTESIAN_POINT ( 'NONE',  ( -25.92022873519999848, 1379.720561049090065, 211.6907041564289784 ) ) ;
#44325 = CARTESIAN_POINT ( 'NONE',  ( -113.4000000000000057, 1309.713060387289943, 304.2218459572590064 ) ) ;
#44327 = DIRECTION ( 'NONE',  ( 0.000000000000000000, 1.000000000000000000, -1.836970198721029688E-16 ) ) ;
#44326 = CARTESIAN_POINT ( 'NONE',  ( -18.13339771048960003, 1456.359500463610175, 190.4520856073839923 ) ) ;
#44328 = B_SPLINE_CURVE_WITH_KNOTS ( 'NONE', 3,
 ( #26408, #60600, #41010, #32622, #100897, #24194, #7412, #37020, #78484, #44341, #35371, #70119, #96386, #63367, #104783, #11827, #69559, #53298, #28069, #44906, #62829, #62258, #1234, #18546, #43777, #19663, #10168, #103679, #2357, #105897, #52740, #71778, #53867, #87439, #26978, #1798, #37577, #88007 ),
 .UNSPECIFIED., .F., .F.,
 ( 4, 2, 2, 1, 2, 2, 2, 2, 1, 2, 2, 2, 2, 2, 2, 2, 1, 1, 2, 2, 4 ),
 ( 0.000000000000000000, 0.1250000000021257163, 0.1875000000032436553, 0.2187500000037996550, 0.2343750000041891490, 0.2500000000045786153, 0.3750000000091979757, 0.4375000000115244481, 0.4687500000129335986, 0.4843750000136203271, 0.5000000000143071111, 0.6250000000158285607, 0.6406250000158579816, 0.6562500000158874025, 0.6875000000159626756, 0.7187500000160379487, 0.7343750000153863589, 0.7421875000150697232, 0.7460937500149279478, 0.7500000000147862833, 1.000000000000000000 ),
 .UNSPECIFIED. ) ;
#44329 = CARTESIAN_POINT ( 'NONE',  ( -68.66492675561440251, 1379.747814238210822, 280.2579952115759170 ) ) ;
#44330 = CONICAL_SURFACE ( 'NONE', #13831, 0.9999999999999962252, 0.7853981633970000820 ) ;
#44331 = CARTESIAN_POINT ( 'NONE',  ( 17.85481329854330212, 1418.946007097159963, 225.0424457944430117 ) ) ;
#44332 = CARTESIAN_POINT ( 'NONE',  ( -5.792969890798230992, 1423.404851848579938, 91.44995330505670950 ) ) ;
#44333 = VERTEX_POINT ( 'NONE', #7069 ) ;
#44334 = CARTESIAN_POINT ( 'NONE',  ( 40.73184307449999864, 1436.263014496900041, 268.3665355202980436 ) ) ;
#44335 = DIRECTION ( 'NONE',  ( 1.755985294532469921E-16, -1.000000000000000000, 1.338183447452831989E-16 ) ) ;
#44336 = CARTESIAN_POINT ( 'NONE',  ( -20.70484064406351621, 1525.907212628473644, 233.2025904124107569 ) ) ;
#44337 = CARTESIAN_POINT ( 'NONE',  ( 3.958201235949999841, 1505.664173997190119, 220.8429677841990042 ) ) ;
#44338 = CARTESIAN_POINT ( 'NONE',  ( -14.41799994660000017, 1415.865102022439942, 214.3937196626189916 ) ) ;
#44340 = ORIENTED_EDGE ( 'NONE', *, *, #44607, .F. ) ;
#44339 = CARTESIAN_POINT ( 'NONE',  ( -1.037000659099919897, 1515.105800736289893, 204.7934710141580013 ) ) ;
#44341 = CARTESIAN_POINT ( 'NONE',  ( -15.63150152900681711, 1415.710789684446127, 209.6412575786757486 ) ) ;
#44342 = CARTESIAN_POINT ( 'NONE',  ( -24.63624201280000037, 1442.774873945370018, 210.7765137803880009 ) ) ;
#44343 = CARTESIAN_POINT ( 'NONE',  ( -16.12211571039999924, 1416.421578853600067, 209.3062130255779891 ) ) ;
#44344 = CARTESIAN_POINT ( 'NONE',  ( -10.95935098528551244, 1431.615009654569576, 151.7698559583776330 ) ) ;
#44345 = CARTESIAN_POINT ( 'NONE',  ( 12.38398709303499956, 1512.136030808819896, 224.0418830982669931 ) ) ;
#44346 = DIRECTION ( 'NONE',  ( 0.08330058266261865241, -0.04363816413316890658, 0.9955685428734450948 ) ) ;
#44347 = DIRECTION ( 'NONE',  ( 0.02617694830785712717, 0.9996573249755577040, -1.162479441679614436E-17 ) ) ;
#44348 = DIRECTION ( 'NONE',  ( 0.7414773880254711402, -0.000000000000000000, 0.6709778558543678662 ) ) ;
#44349 = CARTESIAN_POINT ( 'NONE',  ( -16.44145560006500162, 1512.902436350919970, 220.7137343290669946 ) ) ;
#44350 = CARTESIAN_POINT ( 'NONE',  ( 9.315195566419999906, 1415.075089874329933, 230.3176940828979866 ) ) ;
#44351 = CARTESIAN_POINT ( 'NONE',  ( -10.46078355659999914, 1480.011043621090039, 213.7014894041190018 ) ) ;
#44353 = CARTESIAN_POINT ( 'NONE',  ( -16.68599179869999816, 1461.161699058230170, 228.2799821568980008 ) ) ;
#44352 = VECTOR ( 'NONE', #12026, 1000.000000000000227 ) ;
#44354 = CARTESIAN_POINT ( 'NONE',  ( 1.701027822874999984, 1516.937508036699910, 206.6270879340970055 ) ) ;
#44355 = CARTESIAN_POINT ( 'NONE',  ( 36.00838277309999569, 1418.547366844530188, 267.3063737350979636 ) ) ;
#44356 = DIRECTION ( 'NONE',  ( -0.9455185755993178454, 0.000000000000000000, 0.3255681544571539243 ) ) ;
#44357 = DIRECTION ( 'NONE',  ( -0.9998780035959983215, 8.712314624148121749E-33, 0.01561979272847786350 ) ) ;
#44358 = CARTESIAN_POINT ( 'NONE',  ( 23.93712380200000212, 1508.007210533329953, 195.6926836911979990 ) ) ;
#44359 = CARTESIAN_POINT ( 'NONE',  ( -23.03512223430000105, 1433.464687408990130, 215.3644030352079994 ) ) ;
#44360 = EDGE_CURVE ( 'NONE', #75410, #94873, #58045, .T. ) ;
#44361 = DIRECTION ( 'NONE',  ( 0.7071067811865475727, 2.497298964526426743E-16, 0.7071067811865475727 ) ) ;
#44362 = CARTESIAN_POINT ( 'NONE',  ( -15.21142308021189926, 1418.043559783950059, 203.1433581529450123 ) ) ;
#44363 = CARTESIAN_POINT ( 'NONE',  ( 11.68596223914080490, 1479.116955846581277, 226.2253689540566484 ) ) ;
#44364 = CARTESIAN_POINT ( 'NONE',  ( -16.68563267514501192, 1506.380977038190167, 194.8185150136861807 ) ) ;
#44365 = CARTESIAN_POINT ( 'NONE',  ( -3.750000000000000000, 1516.051704408390151, 209.1218459616989946 ) ) ;
#44366 = CARTESIAN_POINT ( 'NONE',  ( -12.84783018959999978, 1441.405291080990082, 188.1530445986979885 ) ) ;
#44367 = EDGE_CURVE ( 'NONE', #54639, #108510, #100566, .T. ) ;
#44368 = CARTESIAN_POINT ( 'NONE',  ( -7.686381689219429880, 1383.591223628860007, 218.9353989820789934 ) ) ;
#44369 = CARTESIAN_POINT ( 'NONE',  ( 18.16492559431619824, 1429.493622211720094, 208.0479421485399882 ) ) ;
#44370 = CARTESIAN_POINT ( 'NONE',  ( 32.28466283162156714, 1511.187213306747708, 219.1752493337713190 ) ) ;
#44371 = VERTEX_POINT ( 'NONE', #4857 ) ;
#44372 = CARTESIAN_POINT ( 'NONE',  ( -3.167889856915000024, 1511.297452611760036, 201.5028532582269918 ) ) ;
#44373 = CARTESIAN_POINT ( 'NONE',  ( -14.69536968390760023, 1409.426234004640037, 206.4567448585879959 ) ) ;
#44374 = ORIENTED_EDGE ( 'NONE', *, *, #109651, .T. ) ;
#44375 = AXIS2_PLACEMENT_3D ( 'NONE', #36098, #63534, #46720 ) ;
#44376 = CARTESIAN_POINT ( 'NONE',  ( 31.34137657934019927, 1523.382868172864164, 221.9025654077410081 ) ) ;
#44377 = FACE_OUTER_BOUND ( 'NONE', #14894, .T. ) ;
#44378 = CARTESIAN_POINT ( 'NONE',  ( -41.92232120730000133, 1455.764491110230210, 269.0823108244979949 ) ) ;
#44379 = CARTESIAN_POINT ( 'NONE',  ( -11.60766219054749904, 1481.111691938549939, 211.3876766262449962 ) ) ;
#44380 = CARTESIAN_POINT ( 'NONE',  ( 0.1600851318103049814, 1420.194783999099855, 183.7319659859389844 ) ) ;
#44381 = CARTESIAN_POINT ( 'NONE',  ( -24.09814616333339998, 1444.255785637029931, 212.5772553280679915 ) ) ;
#44382 = CARTESIAN_POINT ( 'NONE',  ( -72.88182616411249626, 1384.654869595349965, 298.0902554268950553 ) ) ;
#44383 = CARTESIAN_POINT ( 'NONE',  ( -9.094910673856409389, 1384.931050598509955, 199.9427862989620053 ) ) ;
#44384 = LINE ( 'NONE', #2946, #30070 ) ;
#44385 = CARTESIAN_POINT ( 'NONE',  ( 13.25708502300000013, 1414.913060387329779, 218.7345124127879785 ) ) ;
#44386 = VECTOR ( 'NONE', #14029, 1000.000000000000000 ) ;
#44387 = CARTESIAN_POINT ( 'NONE',  ( 15.56483135290000064, 1506.802866805429858, 224.9286410369979876 ) ) ;
#44388 = LINE ( 'NONE', #35977, #74992 ) ;
#44389 = CARTESIAN_POINT ( 'NONE',  ( 4.038582018749999669, 1515.598601288590089, 208.7452592413320076 ) ) ;
#44390 = CARTESIAN_POINT ( 'NONE',  ( -10.28933532049999933, 1509.343598223630124, 180.9832471055979966 ) ) ;
#44391 = AXIS2_PLACEMENT_3D ( 'NONE', #54475, #62900, #62326 ) ;
#44392 = CARTESIAN_POINT ( 'NONE',  ( -23.42828032239999914, 1409.895749727629891, 208.2087021844820072 ) ) ;
#44393 = CARTESIAN_POINT ( 'NONE',  ( 15.86930212090000047, 1414.913060387329779, 206.5958717475980109 ) ) ;
#44394 = CARTESIAN_POINT ( 'NONE',  ( 3.577381990939999756, 1484.682277373190118, 220.4174637111989909 ) ) ;
#44395 = CARTESIAN_POINT ( 'NONE',  ( 3.844095850890000055, 1423.015328829079863, 194.0309013266989950 ) ) ;
#44396 = CARTESIAN_POINT ( 'NONE',  ( 3.920879176457659820, 1439.701872010520219, 184.6839060028229937 ) ) ;
#44397 = CARTESIAN_POINT ( 'NONE',  ( 10.19122987350000109, 1454.066670175989884, 189.8474967225990042 ) ) ;
#44398 = CARTESIAN_POINT ( 'NONE',  ( -7.508705023303230419, 1508.884117426920056, 214.6350462346350128 ) ) ;
#44399 = CARTESIAN_POINT ( 'NONE',  ( -5.221955786979189718, 1489.269541097040019, 185.8916489436120116 ) ) ;
#44401 = CARTESIAN_POINT ( 'NONE',  ( -10.73113664029999903, 1382.357287394640252, 201.1356155892590039 ) ) ;
#44400 = CARTESIAN_POINT ( 'NONE',  ( -16.63063656698919957, 1417.185604235359961, 208.3711397553730365 ) ) ;
#44402 = CARTESIAN_POINT ( 'NONE',  ( -5.249805860389999523, 1391.918259904190109, 203.6797944339089952 ) ) ;
#44403 = CARTESIAN_POINT ( 'NONE',  ( 9.682511080499990541, 1436.279831232390052, 210.8541354582289955 ) ) ;
#44404 = CARTESIAN_POINT ( 'NONE',  ( -12.16056974390000001, 1489.995349075190006, 210.5160904517290135 ) ) ;
#44405 = DIRECTION ( 'NONE',  ( -0.000000000000000000, 1.836970198721029688E-16, 1.000000000000000000 ) ) ;
#44406 = CARTESIAN_POINT ( 'NONE',  ( -9.690020260109999839, 1366.026910387849966, 210.6218459616991936 ) ) ;
#44407 = CARTESIAN_POINT ( 'NONE',  ( -2.877744984375000037, 1516.723920667490120, 204.5127816287269980 ) ) ;
#44408 = CIRCLE ( 'NONE', #73091, 2.000000000000000000 ) ;
#44409 = CARTESIAN_POINT ( 'NONE',  ( -18.08515272772859817, 1485.385435469039976, 188.9366095778659940 ) ) ;
#44410 = CARTESIAN_POINT ( 'NONE',  ( 1.427799582350000041, 1507.072958340530022, 236.7919270625980346 ) ) ;
#44411 = CARTESIAN_POINT ( 'NONE',  ( 10.53612673599999994, 1504.170325135620033, 214.0656471538289907 ) ) ;
#44412 = CARTESIAN_POINT ( 'NONE',  ( -14.55278341820118904, 1420.461940006850000, 213.8336615198852542 ) ) ;
#44414 = VERTEX_POINT ( 'NONE', #108428 ) ;
#44413 = CARTESIAN_POINT ( 'NONE',  ( -63.24753723578009357, 1379.733506366819938, 271.8172255436770115 ) ) ;
#44415 = VERTEX_POINT ( 'NONE', #108986 ) ;
#44416 = CARTESIAN_POINT ( 'NONE',  ( 11.89956535492810019, 1433.601946136900096, 150.4842440392990000 ) ) ;
#44417 = CARTESIAN_POINT ( 'NONE',  ( 21.14964295068612898, 1525.231887713385959, 184.4343113153503566 ) ) ;
#44418 = VERTEX_POINT ( 'NONE', #48540 ) ;
#44419 = CARTESIAN_POINT ( 'NONE',  ( -2.117392871511483143, 1456.721470742955034, 199.8652278568989971 ) ) ;
#44420 = CARTESIAN_POINT ( 'NONE',  ( -109.8253978320000073, 1384.918090075649843, 311.3807729152589445 ) ) ;
#44422 = CARTESIAN_POINT ( 'NONE',  ( 11.74015320060000001, 1428.979986575930070, 144.1938086916980239 ) ) ;
#44421 = CARTESIAN_POINT ( 'NONE',  ( 17.93144346440610093, 1487.353935485449938, 189.1550781922330202 ) ) ;
#44423 = CARTESIAN_POINT ( 'NONE',  ( 6.559971419567009576, 1464.740524891430141, 211.2618235806450002 ) ) ;
#44424 = CARTESIAN_POINT ( 'NONE',  ( -0.3393288214439999506, 1507.645777512030008, 180.8011794364980176 ) ) ;
#44425 = CARTESIAN_POINT ( 'NONE',  ( 0.1354934564249989926, 1469.338281066689888, 219.1920829782989983 ) ) ;
#44426 = CARTESIAN_POINT ( 'NONE',  ( -24.58339591430969762, 1444.771579268069900, 210.9170101329549993 ) ) ;
#44427 = CARTESIAN_POINT ( 'NONE',  ( 3.461360093275000160, 1516.874084700499907, 212.3753080308970311 ) ) ;
#44428 = CARTESIAN_POINT ( 'NONE',  ( 14.14026437185819951, 1415.666200591919960, 197.1771109711220049 ) ) ;
#44429 = FACE_OUTER_BOUND ( 'NONE', #73061, .T. ) ;
#44430 = CARTESIAN_POINT ( 'NONE',  ( 6.715925843064999512, 1514.199187793459942, 201.3425812415170242 ) ) ;
#44431 = ORIENTED_EDGE ( 'NONE', *, *, #36996, .T. ) ;
#44432 = CARTESIAN_POINT ( 'NONE',  ( 13.80425961236019994, 1435.071252090369853, 149.2278468116170131 ) ) ;
#44433 = CARTESIAN_POINT ( 'NONE',  ( 0.5120954883415810288, 1432.537586748190051, 200.6984891597549847 ) ) ;
#44434 = ORIENTED_EDGE ( 'NONE', *, *, #87037, .F. ) ;
#44435 = ORIENTED_EDGE ( 'NONE', *, *, #61025, .T. ) ;
#44436 = EDGE_LOOP ( 'NONE', ( #57053, #72157, #59959, #57206 ) ) ;
#44437 = CARTESIAN_POINT ( 'NONE',  ( -6.781132916885000306, 1512.686126173240154, 216.3888413780769895 ) ) ;
#44438 = CARTESIAN_POINT ( 'NONE',  ( -2.896739157130000297, 1464.852796890729905, 236.4445922117980103 ) ) ;
#44439 = CARTESIAN_POINT ( 'NONE',  ( 12.68571948835449881, 1500.401381075140080, 208.6071435724910259 ) ) ;
#44440 = CARTESIAN_POINT ( 'NONE',  ( -20.98459803374077026, 1519.551704408389924, 201.4854660376508377 ) ) ;
#44441 = CARTESIAN_POINT ( 'NONE',  ( 10.52615244620000112, 1461.364316732390080, 209.2693891041070060 ) ) ;
#44442 = CARTESIAN_POINT ( 'NONE',  ( 12.26969082843189973, 1421.718210678810010, 208.0791346696769892 ) ) ;
#44443 = CARTESIAN_POINT ( 'NONE',  ( -35.41186141649757246, 1379.641460143238646, 218.3720869345321489 ) ) ;
#44444 = CARTESIAN_POINT ( 'NONE',  ( 4.222016814108400240, 1446.225616327549915, 168.0534523820770119 ) ) ;
#44445 = B_SPLINE_CURVE_WITH_KNOTS ( 'NONE', 3,
 ( #16915, #9104, #1270, #84694, #52231, #42715, #33739, #35409, #9641, #76868, #51670, #17469, #58965, #34852, #69597, #95320, #103715, #93098, #181, #60082, #42159, #34301, #102040, #25327, #59523, #85243, #68483, #94198, #10205, #16370, #85807, #44381 ),
 .UNSPECIFIED., .F., .F.,
 ( 4, 2, 2, 1, 1, 2, 2, 2, 2, 1, 1, 2, 2, 2, 2, 2, 2, 4 ),
 ( 0.000000000000000000, 0.1249999999980515863, 0.1874999999970757558, 0.2187499999965558106, 0.2343749999963441188, 0.2421874999961906305, 0.2499999999960371699, 0.3749999999951986185, 0.4374999999947972729, 0.4687499999946139750, 0.4843749999945410889, 0.4921874999944861329, 0.4999999999944311213, 0.6249999999958106844, 0.6874999999965263342, 0.7187499999969048092, 0.7499999999972831732, 1.000000000000000000 ),
 .UNSPECIFIED. ) ;
#44446 = CARTESIAN_POINT ( 'NONE',  ( 8.659233064277689351, 1437.759822022720073, 209.5177019368769891 ) ) ;
#44447 = ORIENTED_EDGE ( 'NONE', *, *, #41315, .F. ) ;
#44448 = CARTESIAN_POINT ( 'NONE',  ( -3.268235758764999943, 1516.890356958860139, 206.2562572478169898 ) ) ;
#44449 = ORIENTED_EDGE ( 'NONE', *, *, #106519, .T. ) ;
#44450 = CARTESIAN_POINT ( 'NONE',  ( 24.07817550441599863, 1440.913060387330006, 235.9284644500330046 ) ) ;
#44451 = CARTESIAN_POINT ( 'NONE',  ( -19.81193674840000085, 1509.671936380629859, 186.7489041350980017 ) ) ;
#44452 = VERTEX_POINT ( 'NONE', #75396 ) ;
#44453 = CARTESIAN_POINT ( 'NONE',  ( -7.321630743333059854, 1508.611141564370200, 203.6086204835860087 ) ) ;
#44454 = CARTESIAN_POINT ( 'NONE',  ( -14.12627676950000044, 1409.406360842129970, 191.9008118980979987 ) ) ;
#44455 = CARTESIAN_POINT ( 'NONE',  ( -24.63623744410000072, 1442.774865482090036, 210.7765178920280107 ) ) ;
#44456 = CARTESIAN_POINT ( 'NONE',  ( 4.387855888652730130, 1424.007127652020017, 193.0709937674239995 ) ) ;
#44457 = CARTESIAN_POINT ( 'NONE',  ( 1.326713953160000070, 1454.806608698389937, 218.4390644836289823 ) ) ;
#44458 = CARTESIAN_POINT ( 'NONE',  ( -2.372478608332516892, 1522.862737210649811, 174.8996806668726549 ) ) ;
#44459 = CARTESIAN_POINT ( 'NONE',  ( -13.19852776819999995, 1434.900412999929813, 149.2724498062979990 ) ) ;
#44460 = CARTESIAN_POINT ( 'NONE',  ( 19.62004841539999944, 1435.182524171729938, 143.5804541147979876 ) ) ;
#44462 = CARTESIAN_POINT ( 'NONE',  ( -3.088437838665793578, 1369.578208569719209, 207.6586240303519162 ) ) ;
#44461 = CARTESIAN_POINT ( 'NONE',  ( 22.41686883764370464, 1524.667648926078527, 181.9773018742387194 ) ) ;
#44463 = CIRCLE ( 'NONE', #105261, 15.09021984820000029 ) ;
#44464 = CARTESIAN_POINT ( 'NONE',  ( -6.939219520934999608, 1516.783701990830195, 214.9027072062869763 ) ) ;
#44465 = AXIS2_PLACEMENT_3D ( 'NONE', #23460, #49241, #100711 ) ;
#44466 = CARTESIAN_POINT ( 'NONE',  ( -3.701520565116230177, 1428.523979340189953, 200.5242126073240172 ) ) ;
#44467 = CARTESIAN_POINT ( 'NONE',  ( 5.822794770344668969, 1511.432897564909808, 217.0586008862449887 ) ) ;
#44468 = DIRECTION ( 'NONE',  ( -0.6736849260863841948, 0.000000000000000000, 0.7390186874254148774 ) ) ;
#44469 = CARTESIAN_POINT ( 'NONE',  ( 6.562635822504999439, 1517.111322026010157, 211.9927976380170094 ) ) ;
#44470 = CARTESIAN_POINT ( 'NONE',  ( -11.73826079527449906, 1482.415590711050072, 207.1601296673129866 ) ) ;
#44471 = CARTESIAN_POINT ( 'NONE',  ( 30.77244971921734873, 1524.972613296803956, 221.6912005025092753 ) ) ;
#44473 = VERTEX_POINT ( 'NONE', #15447 ) ;
#44472 = CARTESIAN_POINT ( 'NONE',  ( -96.71789436439999577, 1389.284422085869892, 307.9725871335590455 ) ) ;
#44474 = PLANE ( 'NONE',  #33437 ) ;
#44475 = CARTESIAN_POINT ( 'NONE',  ( 5.301749024639999419, 1468.084175537029978, 248.5896189578980113 ) ) ;
#44476 = CARTESIAN_POINT ( 'NONE',  ( -11.57648288090000044, 1432.337770414690112, 151.1968906810979831 ) ) ;
#44477 = CARTESIAN_POINT ( 'NONE',  ( -7.594039287445000674, 1512.142919181319940, 211.3515775794370199 ) ) ;
#44478 = CARTESIAN_POINT ( 'NONE',  ( -7.489162529773470744, 1508.654039492000038, 236.0717299073370157 ) ) ;
#44479 = CARTESIAN_POINT ( 'NONE',  ( -19.04969050960000132, 1456.540524118229996, 228.2072777489979956 ) ) ;
#44481 = CARTESIAN_POINT ( 'NONE',  ( 17.45016910582259939, 1409.714858682069917, 222.5484171803500146 ) ) ;
#44480 = CARTESIAN_POINT ( 'NONE',  ( -12.23489994130180136, 1490.237666497490181, 209.6383001777070092 ) ) ;
#44482 = CARTESIAN_POINT ( 'NONE',  ( -0.08793211890650000362, 1470.815019615130041, 188.6578406787979816 ) ) ;
#44483 = CARTESIAN_POINT ( 'NONE',  ( -105.7656562948000101, 1380.972838942760063, 308.6606380284670195 ) ) ;
#44484 = VECTOR ( 'NONE', #20155, 999.9999999999998863 ) ;
#44485 = VERTEX_POINT ( 'NONE', #109535 ) ;
#44486 = CARTESIAN_POINT ( 'NONE',  ( -2.488360667435000284, 1516.616791731099966, 203.3506968572170308 ) ) ;
#44487 = CARTESIAN_POINT ( 'NONE',  ( 8.723134474349999223, 1451.781317889190177, 212.2855316608589931 ) ) ;
#44488 = CARTESIAN_POINT ( 'NONE',  ( -4.500000000000000000, 1418.913060387330006, 172.2701767054979882 ) ) ;
#44489 = CARTESIAN_POINT ( 'NONE',  ( 19.76075415080629938, 1471.422017333550230, 270.0618168504850019 ) ) ;
#44490 =( BOUNDED_CURVE ( )  B_SPLINE_CURVE ( 3, ( #7879, #91890, #33619, #15703 ),
 .UNSPECIFIED., .F., .F. ) 
 B_SPLINE_CURVE_WITH_KNOTS ( ( 4, 4 ),
 ( 4.129383272231839541, 5.295394741052569465 ),
 .UNSPECIFIED. ) 
 CURVE ( )  GEOMETRIC_REPRESENTATION_ITEM ( )  RATIONAL_B_SPLINE_CURVE ( ( 1.000000000000000000, 0.8898744396721667282, 0.8898744396721667282, 1.000000000000000000 ) ) 
 REPRESENTATION_ITEM ( '' )  );
#44491 = CARTESIAN_POINT ( 'NONE',  ( -23.91014234936227467, 1436.885471179933802, 212.4210152180790772 ) ) ;
#44492 = CARTESIAN_POINT ( 'NONE',  ( 20.65270365140000308, 1496.273551523690003, 204.7144476429189979 ) ) ;
#44493 = CARTESIAN_POINT ( 'NONE',  ( -116.8159439063953045, 1378.913060387289988, 306.3030300501105785 ) ) ;
#44494 = CARTESIAN_POINT ( 'NONE',  ( -39.77527677378599691, 1440.913060401030179, 258.9675477506260108 ) ) ;
#44495 = CARTESIAN_POINT ( 'NONE',  ( 35.35472037963140224, 1450.224566512450110, 136.2317276167839850 ) ) ;
#44496 = DIRECTION ( 'NONE',  ( -0.000000000000000000, 1.000000000000000000, -0.000000000000000000 ) ) ;
#44497 = CARTESIAN_POINT ( 'NONE',  ( 0.3714955681550010103, 1430.530475112889917, 199.6801487385589837 ) ) ;
#44498 = CARTESIAN_POINT ( 'NONE',  ( -15.92986207429999901, 1416.139014782290133, 209.7537124246929920 ) ) ;
#44499 = CARTESIAN_POINT ( 'NONE',  ( -21.55489959617492346, 1524.059547553519451, 184.0356378790828273 ) ) ;
#44500 = DIRECTION ( 'NONE',  ( 1.000000000000000000, 0.000000000000000000, 0.000000000000000000 ) ) ;
#44501 = ORIENTED_EDGE ( 'NONE', *, *, #31522, .T. ) ;
#44502 = CARTESIAN_POINT ( 'NONE',  ( 3.452230076589999808, 1448.972367684420078, 184.0844731014979914 ) ) ;
#44503 = CARTESIAN_POINT ( 'NONE',  ( 1.066336734320000090, 1485.534576645189873, 198.2622823792990232 ) ) ;
#44504 = CARTESIAN_POINT ( 'NONE',  ( 9.740996373304689371, 1468.658287592850002, 206.6114599079629670 ) ) ;
#44505 = CARTESIAN_POINT ( 'NONE',  ( -0.2975168056209999690, 1416.438871972429979, 233.7075449661979860 ) ) ;
#44506 = CARTESIAN_POINT ( 'NONE',  ( 11.43524938500000054, 1502.933412134090077, 210.4930575720590014 ) ) ;
#44507 = CARTESIAN_POINT ( 'NONE',  ( -31.02592223166987395, 1526.278758871497075, 198.2784374727513352 ) ) ;
#44508 = CARTESIAN_POINT ( 'NONE',  ( 7.338784656529999673, 1425.472921401149961, 211.8656132916889874 ) ) ;
#44509 = CARTESIAN_POINT ( 'NONE',  ( -14.54449344532160104, 1384.878238794750132, 219.3450228996460112 ) ) ;
#44510 = B_SPLINE_SURFACE_WITH_KNOTS ( 'NONE', 5, 5, ( 
 ( #46151, #79191, #36615, #28771, #12518, #98164 ),
 ( #96529, #90308, #30410, #106036, #3596, #72443 ),
 ( #37720, #38807, #64599, #4135, #28213, #20897 ),
 ( #62972, #4669, #62402, #89223, #46696, #107120 ),
 ( #71922, #11428, #21978, #13039, #70815, #20350 ),
 ( #55647, #19804, #54554, #80826, #56170, #88688 ),
 ( #21436, #29860, #104928, #64046, #54009, #88140 ),
 ( #29313, #63511, #45597, #97629, #55096, #39368 ),
 ( #75192, #83559, #7415, #23100, #74090, #5779 ) ),
 .UNSPECIFIED., .F., .F., .F.,
 ( 6, 3, 6 ),
 ( 6, 6 ),
 ( 3.966820261850000140, 8.905289209860001165, 13.57492324310000065 ),
 ( 0.000000000000000000, 0.5000000000000000000 ),
 .UNSPECIFIED. ) ;
#44511 = CARTESIAN_POINT ( 'NONE',  ( -18.83207817909999804, 1416.311719782429918, 207.5739159116880046 ) ) ;
#44512 = CARTESIAN_POINT ( 'NONE',  ( -11.41675737880000163, 1482.775670507890027, 205.7339588576290055 ) ) ;
#44513 = CARTESIAN_POINT ( 'NONE',  ( 26.46121328487780033, 1436.564390249430062, 136.7873533364920036 ) ) ;
#44514 = CARTESIAN_POINT ( 'NONE',  ( -9.446360030840120103, 1396.242934550719838, 203.3640226473000041 ) ) ;
#44515 = ORIENTED_EDGE ( 'NONE', *, *, #36006, .F. ) ;
#44516 =( BOUNDED_CURVE ( )  B_SPLINE_CURVE ( 3, ( #13460, #40886, #108088, #71388 ),
 .UNSPECIFIED., .F., .T. ) 
 B_SPLINE_CURVE_WITH_KNOTS ( ( 4, 4 ),
 ( 2.021799836360349989, 2.259315975108074692 ),
 .UNSPECIFIED. ) 
 CURVE ( )  GEOMETRIC_REPRESENTATION_ITEM ( )  RATIONAL_B_SPLINE_CURVE ( ( 1.000000000000000000, 0.9953043629482734023, 0.9953043629482734023, 1.000000000000000000 ) ) 
 REPRESENTATION_ITEM ( '' )  );
#44517 = CARTESIAN_POINT ( 'NONE',  ( -16.17741046092470114, 1409.477982791400109, 225.0323175894529868 ) ) ;
#44518 = CARTESIAN_POINT ( 'NONE',  ( 9.740283752330000766, 1438.194204504490017, 148.7998369308980102 ) ) ;
#44519 = ORIENTED_EDGE ( 'NONE', *, *, #68243, .F. ) ;
#44520 = CARTESIAN_POINT ( 'NONE',  ( -11.32820085813967381, 1502.497619087743260, 207.1796466604740488 ) ) ;
#44521 = CARTESIAN_POINT ( 'NONE',  ( -14.87047397674367488, 1416.119917872056249, 205.0110095938617292 ) ) ;
#44522 = CARTESIAN_POINT ( 'NONE',  ( -22.08622291487980149, 1523.456924617336199, 233.8253038720280301 ) ) ;
#44524 = DIRECTION ( 'NONE',  ( 3.164571201028890223E-15, -1.000000000000000000, 0.000000000000000000 ) ) ;
#44523 = CARTESIAN_POINT ( 'NONE',  ( 10.65150121880000178, 1425.724714984030015, 91.14980631569790148 ) ) ;
#44525 = CARTESIAN_POINT ( 'NONE',  ( -1.663182004820000115, 1450.571104617790070, 190.0477235955989954 ) ) ;
#44526 = CARTESIAN_POINT ( 'NONE',  ( -8.669013948499998179, 1451.120073550389861, 205.1633857913290058 ) ) ;
#44527 = EDGE_CURVE ( 'NONE', #78872, #46325, #31455, .T. ) ;
#44528 = CARTESIAN_POINT ( 'NONE',  ( 7.329303077985000137, 1516.857992118400034, 201.7912917986770083 ) ) ;
#44529 = AXIS2_PLACEMENT_3D ( 'NONE', #66308, #90358, #64649 ) ;
#44530 = CARTESIAN_POINT ( 'NONE',  ( 7.850505384759999039, 1425.611863130590109, 211.6471506695990001 ) ) ;
#44531 = CARTESIAN_POINT ( 'NONE',  ( -19.86622903030000131, 1443.388330262490172, 213.1207022696590059 ) ) ;
#44532 = CARTESIAN_POINT ( 'NONE',  ( -24.16126736702833000, 1411.115437147818739, 208.9405857977035339 ) ) ;
#44533 = CARTESIAN_POINT ( 'NONE',  ( 7.588802682105000308, 1511.942942747529969, 206.8630203803070060 ) ) ;
#44534 = CARTESIAN_POINT ( 'NONE',  ( -113.4000000000000057, 1379.413087040579967, 305.1680626132370548 ) ) ;
#44535 = CARTESIAN_POINT ( 'NONE',  ( 7.945025989411964140, 1365.048221891109279, 209.6218459617148824 ) ) ;
#44537 = VERTEX_POINT ( 'NONE', #30618 ) ;
#44536 = CARTESIAN_POINT ( 'NONE',  ( 6.168648949850000562, 1454.757917196489871, 216.8023148204190136 ) ) ;
#44538 = ORIENTED_EDGE ( 'NONE', *, *, #99547, .F. ) ;
#44539 = CARTESIAN_POINT ( 'NONE',  ( -41.65668282690000268, 1444.004026777709896, 136.1262226100980115 ) ) ;
#44540 = CIRCLE ( 'NONE', #14401, 1.999999999999999556 ) ;
#44541 = CARTESIAN_POINT ( 'NONE',  ( -0.2658355946003779779, 1507.129453219969946, 237.3293658036959926 ) ) ;
#44542 = CARTESIAN_POINT ( 'NONE',  ( -0.4896151268140000457, 1473.897694200829847, 270.2927087789979623 ) ) ;
#44543 = CARTESIAN_POINT ( 'NONE',  ( -4.227540919128129460, 1441.218328383909920, 201.3833897788859986 ) ) ;
#44544 = CARTESIAN_POINT ( 'NONE',  ( -2.790497053790000237, 1486.234749837029995, 181.8136913017980021 ) ) ;
#44545 = CARTESIAN_POINT ( 'NONE',  ( -32.35368859299580180, 1524.871836253796118, 201.1945538962762896 ) ) ;
#44546 = CARTESIAN_POINT ( 'NONE',  ( -8.179930528059999872, 1384.351712228729866, 199.6861502166489970 ) ) ;
#44547 = DIRECTION ( 'NONE',  ( 0.6665120492724535550, 0.000000000000000000, -0.7454942576402816545 ) ) ;
#44548 = CARTESIAN_POINT ( 'NONE',  ( -2.500000000000000000, 1448.415523929209940, 161.9475238664840049 ) ) ;
#44549 = CARTESIAN_POINT ( 'NONE',  ( -12.95793659252135654, 1435.633131908374480, 150.6734405774689662 ) ) ;
#44550 = CARTESIAN_POINT ( 'NONE',  ( 3.114442184824649740, 1407.350062395909845, 196.1192100924239980 ) ) ;
#44551 = CARTESIAN_POINT ( 'NONE',  ( 5.471684509034499571E-05, 1406.265030819799904, 269.2947838974420165 ) ) ;
#44552 = CARTESIAN_POINT ( 'NONE',  ( -14.33374980507880103, 1435.338667551370008, 149.4045105969410088 ) ) ;
#44553 = EDGE_LOOP ( 'NONE', ( #74743, #94406, #41873, #106948, #63606, #88794, #85208, #67651, #64800, #38541, #41746, #106647 ) ) ;
#44554 = CARTESIAN_POINT ( 'NONE',  ( -61.47464146408020014, 1511.504763168490172, 211.0950333733410105 ) ) ;
#44555 = CARTESIAN_POINT ( 'NONE',  ( 13.28694838949999912, 1443.173555058169995, 187.6984227527979954 ) ) ;
#44556 = ORIENTED_EDGE ( 'NONE', *, *, #63060, .F. ) ;
#44557 = ORIENTED_EDGE ( 'NONE', *, *, #28541, .F. ) ;
#44558 = CARTESIAN_POINT ( 'NONE',  ( -4.146473569399999448, 1455.609540686289847, 200.6301625394189898 ) ) ;
#44559 = CARTESIAN_POINT ( 'NONE',  ( -4.745098151869999725, 1360.923919868640041, 207.6218459616989946 ) ) ;
#44560 = CIRCLE ( 'NONE', #51668, 2.000000000000007550 ) ;
#44561 = CARTESIAN_POINT ( 'NONE',  ( -4.999456428534999830, 1516.830644417779922, 213.7431138541670066 ) ) ;
#44562 = CARTESIAN_POINT ( 'NONE',  ( 2.229731609205000353, 1512.142919181319940, 216.7158852195469763 ) ) ;
#44563 = ORIENTED_EDGE ( 'NONE', *, *, #34619, .F. ) ;
#44564 = CARTESIAN_POINT ( 'NONE',  ( -84.31096497629998510, 1374.600296256690172, 298.0935392271590558 ) ) ;
#44565 = ADVANCED_FACE ( 'NONE', ( #82678 ), #31710, .T. ) ;
#44566 = EDGE_CURVE ( 'NONE', #10255, #26097, #100848, .T. ) ;
#44567 = EDGE_CURVE ( 'NONE', #67802, #26163, #3327, .T. ) ;
#44568 = CARTESIAN_POINT ( 'NONE',  ( 7.723895006289999365, 1416.216596894629902, 225.6857186377980042 ) ) ;
#44569 = CARTESIAN_POINT ( 'NONE',  ( 4.612507273904999039, 1516.886345593249871, 204.1123678647870179 ) ) ;
#44570 = CARTESIAN_POINT ( 'NONE',  ( -11.71397076299980000, 1489.483175994190105, 212.5377881273170146 ) ) ;
#44571 = EDGE_CURVE ( 'NONE', #575, #4737, #91556, .T. ) ;
#44572 = CYLINDRICAL_SURFACE ( 'NONE', #57034, 2.000000000000003553 ) ;
#44574 = EDGE_CURVE ( 'NONE', #15990, #47552, #73068, .T. ) ;
#44573 = CARTESIAN_POINT ( 'NONE',  ( -92.78423182619999920, 1385.084188629489972, 294.1460543437590331 ) ) ;
#44575 = CARTESIAN_POINT ( 'NONE',  ( -52.84305079022620077, 1384.633012693340106, 229.9587693130270054 ) ) ;
#44576 = DIRECTION ( 'NONE',  ( 0.000000000000000000, -1.000000000000000000, 0.000000000000000000 ) ) ;
#44577 = CARTESIAN_POINT ( 'NONE',  ( -6.153079222899999756, 1409.127930650229928, 230.3577016067980026 ) ) ;
#44579 = ORIENTED_EDGE ( 'NONE', *, *, #6036, .T. ) ;
#44578 = CARTESIAN_POINT ( 'NONE',  ( -5.805250577859999872, 1446.068923017249972, 184.0668530776979992 ) ) ;
#44580 = DIRECTION ( 'NONE',  ( 1.000000000000000000, 0.000000000000000000, 0.000000000000000000 ) ) ;
#44581 = CARTESIAN_POINT ( 'NONE',  ( -25.11643266749259595, 1440.913060493619923, 216.7860662917659909 ) ) ;
#44582 = CARTESIAN_POINT ( 'NONE',  ( -27.74315420650000164, 1383.844892876249787, 225.5041886164589755 ) ) ;
#44583 = CARTESIAN_POINT ( 'NONE',  ( 10.51055398149999931, 1471.685891510089959, 212.2894657440390063 ) ) ;
#44584 = CARTESIAN_POINT ( 'NONE',  ( -24.93438155140000134, 1435.649195298570248, 136.9390313255980232 ) ) ;
#44585 = CARTESIAN_POINT ( 'NONE',  ( -3.251888867474999945, 1516.793978928989873, 211.6142896211370044 ) ) ;
#44586 = CIRCLE ( 'NONE', #87513, 4.250000000000000000 ) ;
#44587 = CARTESIAN_POINT ( 'NONE',  ( -67.63612853559999394, 1379.748709736400087, 277.8550023105590299 ) ) ;
#44588 = CARTESIAN_POINT ( 'NONE',  ( -109.9850573467474106, 1384.919979545036085, 311.4561262142244686 ) ) ;
#44589 = CARTESIAN_POINT ( 'NONE',  ( -29.95987888842740787, 1525.317359687841190, 221.5595086622937799 ) ) ;
#44590 = CARTESIAN_POINT ( 'NONE',  ( 21.19090038262594433, 1411.012220291270069, 200.4862705368239233 ) ) ;
#44591 = CARTESIAN_POINT ( 'NONE',  ( 2.292217010694999946, 1516.941178807709775, 209.1086494233340147 ) ) ;
#44592 = ORIENTED_EDGE ( 'NONE', *, *, #56916, .T. ) ;
#44593 = CARTESIAN_POINT ( 'NONE',  ( -7.965680540240001051, 1384.926148861439970, 199.4891222871690104 ) ) ;
#44595 = EDGE_CURVE ( 'NONE', #12262, #75688, #55252, .T. ) ;
#44594 = CARTESIAN_POINT ( 'NONE',  ( 3.008618833319030017, 1440.893622201600010, 157.1951523134509898 ) ) ;
#44596 = CARTESIAN_POINT ( 'NONE',  ( -22.68470003930000090, 1385.128694769440017, 222.0359864906590133 ) ) ;
#44597 = VERTEX_POINT ( 'NONE', #85978 ) ;
#44598 = CARTESIAN_POINT ( 'NONE',  ( -14.01427947078130032, 1385.298181900520149, 219.2221585896700162 ) ) ;
#44599 = CIRCLE ( 'NONE', #30265, 2.000000000000000000 ) ;
#44600 = CARTESIAN_POINT ( 'NONE',  ( -4.545982226927982595, 1508.783371655784777, 206.6339107757056581 ) ) ;
#44601 = CARTESIAN_POINT ( 'NONE',  ( 12.32076549412740007, 1434.285059378609958, 149.9228593313019644 ) ) ;
#44602 = B_SPLINE_SURFACE_WITH_KNOTS ( 'NONE', 5, 5, ( 
 ( #49272, #68296, #83399, #58222, #76662, #7796, #16717, #58767, #50918, #110812, #102404, #110256 ),
 ( #40852, #33531, #83955, #50380, #109178, #25686, #32463, #7255, #59880, #100739, #67732, #75027 ),
 ( #92346, #94006, #17271, #51462, #66084, #109715, #66638, #57685, #16178, #40298, #74482, #108609 ),
 ( #15618, #49825, #31898, #23493, #41417, #75583, #32990, #67179, #92905, #9458, #533, #34657 ),
 ( #102944, #60434, #79434, #35210, #69952, #52583, #69396, #104066, #68841, #20058, #53707, #17825 ),
 ( #62102, #43071, #87275, #26810, #85594, #44180, #52028, #53137, #10569, #78891, #36311, #86717 ),
 ( #10009, #87846, #86166, #35769, #36866, #26246, #77772, #18386, #45294, #2745, #104623, #60997 ),
 ( #94552, #11134, #8892, #27360, #43624, #71059, #105182, #78318, #77231, #1083, #61543, #95673 ),
 ( #103507, #18942, #70507, #1632, #28473, #62667, #95123, #44741, #2197, #27919, #96788, #96226 ),
 ( #19503, #12772, #11668, #79977, #29563, #80536, #39052, #65401, #97321, #55343, #89476, #72160 ),
 ( #105745, #56437, #13846, #73232, #88378, #46949, #29029, #55898, #98965, #31219, #37978, #107375 ),
 ( #99507, #22239, #20591, #81069, #30670, #45844, #90016, #106277, #54252, #4384, #54790, #21691 ) ),
 .UNSPECIFIED., .F., .F., .F.,
 ( 6, 3, 3, 6 ),
 ( 6, 3, 3, 6 ),
 ( 13.03551675900000006, 13.93909308159999938, 15.74624572679999979, 17.56257963661519739 ),
 ( -0.0002656258151532139909, 0.3080049601120000147, 0.9240148803369999664, 1.597676193965150038 ),
 .UNSPECIFIED. ) ;
#44603 = CARTESIAN_POINT ( 'NONE',  ( 16.55300517245429859, 1488.409285182970052, 230.4335696866129979 ) ) ;
#44604 = EDGE_CURVE ( 'NONE', #92713, #100110, #1531, .T. ) ;
#44605 = CARTESIAN_POINT ( 'NONE',  ( -23.90590786130449885, 1509.492427560550141, 224.2268974937140058 ) ) ;
#44606 = CARTESIAN_POINT ( 'NONE',  ( -21.84020450222076448, 1501.977400791986611, 183.2638850454220858 ) ) ;
#44607 = EDGE_CURVE ( 'NONE', #32152, #44860, #69766, .T. ) ;
#44608 = CARTESIAN_POINT ( 'NONE',  ( -2.775557561559999991E-17, 1408.913060387329779, 231.7748916200980034 ) ) ;
#44609 = CARTESIAN_POINT ( 'NONE',  ( 2.961376673209999755, 1417.751980673930120, 234.4067280231980135 ) ) ;
#44611 = CARTESIAN_POINT ( 'NONE',  ( -2.829338567090000200, 1421.191772942729813, 185.4464042013979963 ) ) ;
#44610 = CARTESIAN_POINT ( 'NONE',  ( -5.002593397454999646, 1516.960844870249957, 215.6810146069769871 ) ) ;
#44612 = CARTESIAN_POINT ( 'NONE',  ( 18.84923899389999846, 1508.518338803630058, 188.3455786348980041 ) ) ;
#44613 = EDGE_LOOP ( 'NONE', ( #20537, #8595, #80911, #21288, #107300 ) ) ;
#44614 = CARTESIAN_POINT ( 'NONE',  ( 6.554778533645000849, 1516.929962200689943, 201.4024535497269994 ) ) ;
#44615 = CARTESIAN_POINT ( 'NONE',  ( -19.92228370630000001, 1485.913060387229962, 190.2096421728979863 ) ) ;
#44616 = ORIENTED_EDGE ( 'NONE', *, *, #101505, .F. ) ;
#44617 = AXIS2_PLACEMENT_3D ( 'NONE', #86051, #2629, #36755 ) ;
#44618 = EDGE_CURVE ( 'NONE', #64533, #73065, #52687, .T. ) ;
#44619 = CARTESIAN_POINT ( 'NONE',  ( 4.363122647530000009, 1421.971318475729959, 183.8271342376980044 ) ) ;
#44620 = AXIS2_PLACEMENT_3D ( 'NONE', #31143, #47416, #23287 ) ;
#44621 = CARTESIAN_POINT ( 'NONE',  ( 10.20727470078544030, 1435.399071415931758, 152.3495190223391091 ) ) ;
#44622 = CARTESIAN_POINT ( 'NONE',  ( 7.494431743707549387, 1510.714321716100130, 203.0291457976910010 ) ) ;
#44623 = UNCERTAINTY_MEASURE_WITH_UNIT (LENGTH_MEASURE( 1.000000000000000082E-05 ), #45674, 'distance_accuracy_value', 'NONE');
#44624 = CARTESIAN_POINT ( 'NONE',  ( -2.472546472639999937, 1422.360492461730018, 192.6709265742990169 ) ) ;
#44625 = CARTESIAN_POINT ( 'NONE',  ( 7.821732060355000016, 1513.613303996360173, 216.8564630578470087 ) ) ;
#44626 = DIRECTION ( 'NONE',  ( 1.000000000000000000, 0.000000000000000000, 0.000000000000000000 ) ) ;
#44627 = CARTESIAN_POINT ( 'NONE',  ( 17.62728127150000290, 1415.048591094029916, 210.5990483032680061 ) ) ;
#44628 = CARTESIAN_POINT ( 'NONE',  ( -18.26675077970000061, 1424.840336371829835, 227.6848321215980206 ) ) ;
#44629 = CARTESIAN_POINT ( 'NONE',  ( -15.90533261240000051, 1435.486427895659972, 148.6044062959979897 ) ) ;
#44630 = CARTESIAN_POINT ( 'NONE',  ( -0.5987183604784179769, 1507.212886163649955, 231.7504617458309895 ) ) ;
#44631 = CARTESIAN_POINT ( 'NONE',  ( 16.24504166639999880, 1416.217127671729941, 191.3512804590980068 ) ) ;
#44633 = CARTESIAN_POINT ( 'NONE',  ( -19.02402554036360627, 1439.750327254491367, 209.9292271237399916 ) ) ;
#44632 = CARTESIAN_POINT ( 'NONE',  ( 3.830726099870000123, 1487.263094006890014, 197.7783884857990131 ) ) ;
#44634 = CARTESIAN_POINT ( 'NONE',  ( 10.82295897259685269, 1424.914574748641826, 144.7906534265950143 ) ) ;
#44635 = ORIENTED_EDGE ( 'NONE', *, *, #9671, .T. ) ;
#44636 = CARTESIAN_POINT ( 'NONE',  ( 0.6474875409317040198, 1507.275794996420018, 186.4417145385390029 ) ) ;
#44637 = CARTESIAN_POINT ( 'NONE',  ( -9792.142915468795763, 50.28429875023824280, -1105.735995892511028 ) ) ;
#44638 = DIRECTION ( 'NONE',  ( 0.7071067811865492381, 0.000000000000000000, 0.7071067811865457964 ) ) ;
#44639 = CARTESIAN_POINT ( 'NONE',  ( -4.165129268920000349, 1485.181570780589936, 197.9537754904989981 ) ) ;
#44640 = CIRCLE ( 'NONE', #87571, 8.102416131500007168 ) ;
#44641 = CARTESIAN_POINT ( 'NONE',  ( -3.522208045919057451, 1426.008235538924737, 185.8885408405282931 ) ) ;
#44642 = B_SPLINE_SURFACE_WITH_KNOTS ( 'NONE', 5, 5, ( 
 ( #17332, #18440, #44799, #79497, #61065, #62159 ),
 ( #46458, #20652, #61599, #54854, #45900, #2260 ),
 ( #28531, #103574, #71686, #78953, #19563, #27975 ),
 ( #80590, #70563, #80035, #52640, #62729, #88977 ),
 ( #11731, #96851, #96286, #105805, #12266, #35271 ),
 ( #10066, #36374, #104681, #2804, #105240, #86777 ),
 ( #29085, #3357, #95182, #44239, #27416, #78384 ),
 ( #53194, #1692, #87905, #26875, #53769, #20119 ),
 ( #35832, #95732, #70016, #63270, #11194, #54312 ) ),
 .UNSPECIFIED., .F., .F., .F.,
 ( 6, 3, 6 ),
 ( 6, 6 ),
 ( 3.809711666910000183, 7.545169656169999683, 12.51705759590000078 ),
 ( 0.000000000000000000, 2.000000000000000000 ),
 .UNSPECIFIED. ) ;
#44643 = DIRECTION ( 'NONE',  ( -0.9901118076173108795, 0.1402804634180439824, 0.000000000000000000 ) ) ;
#44644 = CARTESIAN_POINT ( 'NONE',  ( -11.21334730859030060, 1470.344185174209997, 211.0928785205099985 ) ) ;
#44645 = CARTESIAN_POINT ( 'NONE',  ( -6.943975500687450619, 1487.611661080929935, 219.0757446383669844 ) ) ;
#44646 = CARTESIAN_POINT ( 'NONE',  ( -4.290508147279999740, 1515.379315998089851, 209.1218459617929852 ) ) ;
#44647 = CARTESIAN_POINT ( 'NONE',  ( -88.89087977607839264, 1383.771024000470106, 308.1318186344960282 ) ) ;
#44648 = CARTESIAN_POINT ( 'NONE',  ( -109.3980338099009941, 1384.227017930330021, 311.2250570124659816 ) ) ;
#44649 = B_SPLINE_CURVE_WITH_KNOTS ( 'NONE', 3,
 ( #10030, #63233, #2216, #95694, #3866, #27380, #26831, #71077, #69418, #61017, #52602, #96806, #78344 ),
 .UNSPECIFIED., .F., .F.,
 ( 4, 2, 2, 1, 2, 2, 4 ),
 ( 0.000000000000000000, 0.2499999999996690425, 0.3749999999995077271, 0.4374999999994769184, 0.4687499999994652056, 0.4999999999994535482, 1.000000000000000000 ),
 .UNSPECIFIED. ) ;
#44650 = DIRECTION ( 'NONE',  ( -0.8090169943751894799, 3.009330011589934659E-31, -0.5877852522921398482 ) ) ;
#44651 = CARTESIAN_POINT ( 'NONE',  ( -2.454407622921550125, 1516.534924556719943, 201.4127979744969821 ) ) ;
#44653 = ORIENTED_EDGE ( 'NONE', *, *, #71279, .F. ) ;
#44652 = CARTESIAN_POINT ( 'NONE',  ( 24.04921614290000065, 1508.500197933130039, 195.9136757570979910 ) ) ;
#44654 = CARTESIAN_POINT ( 'NONE',  ( -1.326919697740000181, 1414.988015876829877, 226.4745228867980131 ) ) ;
#44655 = VECTOR ( 'NONE', #23711, 1000.000000000000114 ) ;
#44656 = CARTESIAN_POINT ( 'NONE',  ( -77.33784092209999983, 1381.010457831459917, 299.7574715306590178 ) ) ;
#44657 = CARTESIAN_POINT ( 'NONE',  ( 20.06110565012859936, 1509.143991300649986, 229.7914472179430163 ) ) ;
#44658 = ORIENTED_EDGE ( 'NONE', *, *, #15924, .F. ) ;
#44659 = ORIENTED_EDGE ( 'NONE', *, *, #25237, .T. ) ;
#44660 = CARTESIAN_POINT ( 'NONE',  ( 19.47176263695120113, 1508.319487713160015, 229.5268495768910100 ) ) ;
#44661 = CARTESIAN_POINT ( 'NONE',  ( -31.81407709660787830, 1522.862737210649811, 196.2902540610632229 ) ) ;
#44662 = CARTESIAN_POINT ( 'NONE',  ( 13.40432466244523013, 1443.415710732174603, 169.3677059354045866 ) ) ;
#44664 = CARTESIAN_POINT ( 'NONE',  ( -13.01666421170000021, 1472.524044086929962, 262.4458738597979846 ) ) ;
#44663 = CARTESIAN_POINT ( 'NONE',  ( 18.84387474539999729, 1434.822844257309953, 208.7548053377890085 ) ) ;
#44665 = B_SPLINE_CURVE_WITH_KNOTS ( 'NONE', 3,
 ( #85498, #103972, #86072, #27269, #42978, #76565, #27827, #77137, #86618, #44082, #9368, #78221, #95576, #18846, #16623, #77675, #10468, #44641, #78784, #2097, #62007, #50819, #34009, #102306, #84951, #68203, #8242, #42411, #59784, #37888, #87749, #88835, #80986, #106186, #28375, #88285, #70970, #13202, #3756 ),
 .UNSPECIFIED., .F., .F.,
 ( 4, 2, 2, 1, 1, 2, 2, 2, 2, 1, 1, 2, 2, 2, 2, 2, 1, 1, 1, 2, 2, 2, 4 ),
 ( 0.000000000000000000, 0.06249999999957017716, 0.09374999999935659800, 0.1093749999992551653, 0.1171874999992067318, 0.1210937499991825289, 0.1249999999991583122, 0.1874999999988822830, 0.2187499999987529697, 0.2343749999986922405, 0.2421874999986679544, 0.2460937499986559640, 0.2499999999986439736, 0.3749999999982069343, 0.4374999999979756748, 0.4687499999978566589, 0.4843749999978096965, 0.4921874999977803866, 0.4960937499977566834, 0.4980468749977415288, 0.4999999999977263743, 0.7499999999988631316, 1.000000000000000000 ),
 .UNSPECIFIED. ) ;
#44666 = CARTESIAN_POINT ( 'NONE',  ( 9.819193384514399270, 1435.740382366890117, 209.6674245052340098 ) ) ;
#44667 = CARTESIAN_POINT ( 'NONE',  ( -109.0924835130000048, 1382.770673418189972, 297.4849455732589831 ) ) ;
#44668 = EDGE_CURVE ( 'NONE', #4755, #54175, #12032, .T. ) ;
#44669 = CARTESIAN_POINT ( 'NONE',  ( 27.59998756409999743, 1509.654128750629980, 206.1402511112580100 ) ) ;
#44670 = CARTESIAN_POINT ( 'NONE',  ( 8.515581525185789147, 1517.151704408390060, 191.3277396192498543 ) ) ;
#44671 = CARTESIAN_POINT ( 'NONE',  ( 6.506310070979999693, 1410.514241582030081, 186.9556225147979944 ) ) ;
#44672 = CARTESIAN_POINT ( 'NONE',  ( 5.554866099599999885, 1421.644415044730067, 186.0588715001979949 ) ) ;
#44673 = CARTESIAN_POINT ( 'NONE',  ( -8.766760704440001106, 1437.289887460749924, 153.2969298518980281 ) ) ;
#44674 = CARTESIAN_POINT ( 'NONE',  ( 10.43358995060000005, 1436.699218567949856, 152.2773048147980148 ) ) ;
#44675 = CARTESIAN_POINT ( 'NONE',  ( -10.95819916725939969, 1423.467759776100138, 204.3045060729880049 ) ) ;
#44676 = CARTESIAN_POINT ( 'NONE',  ( 19.03110457515579768, 1457.047041246000163, 226.1578386336209974 ) ) ;
#44677 = CARTESIAN_POINT ( 'NONE',  ( 3.883237672519999517, 1472.390963103490094, 218.5418498176989885 ) ) ;
#44678 = ORIENTED_EDGE ( 'NONE', *, *, #22611, .T. ) ;
#44679 = CARTESIAN_POINT ( 'NONE',  ( -11.71078717319999996, 1508.002514750790169, 208.1938872918760239 ) ) ;
#44680 = CARTESIAN_POINT ( 'NONE',  ( 18.46111193188719923, 1471.786021244009817, 195.2229615556349813 ) ) ;
#44681 = CARTESIAN_POINT ( 'NONE',  ( -44.13011771299999708, 1440.913068107089885, 270.2165841919979812 ) ) ;
#44682 = CARTESIAN_POINT ( 'NONE',  ( -23.93711277806432847, 1435.908512379617378, 211.2583651232883710 ) ) ;
#44683 = CARTESIAN_POINT ( 'NONE',  ( 17.11609659350000001, 1409.675656910730140, 223.5180517379979790 ) ) ;
#44684 = DIRECTION ( 'NONE',  ( -0.9786619618251657382, 0.000000000000000000, 0.2054769195713184449 ) ) ;
#44685 = VECTOR ( 'NONE', #43402, 1000.000000000000000 ) ;
#44686 = EDGE_CURVE ( 'NONE', #16269, #76640, #55273, .T. ) ;
#44687 = CARTESIAN_POINT ( 'NONE',  ( 4.329448776040000446, 1515.064792882589927, 210.8902905144720137 ) ) ;
#44688 = DIRECTION ( 'NONE',  ( 0.3363363969981477131, -0.6659120918162938496, 0.6659120918162938496 ) ) ;
#44689 = CARTESIAN_POINT ( 'NONE',  ( 2.279486851180000162, 1508.935250639130118, 237.8394454172980090 ) ) ;
#44690 = CARTESIAN_POINT ( 'NONE',  ( -7.702505263429999971, 1417.009600301830005, 231.0840807062979820 ) ) ;
#44691 = CARTESIAN_POINT ( 'NONE',  ( -7.806477655520000170, 1459.630680128490212, 215.5618046700689945 ) ) ;
#44692 = CARTESIAN_POINT ( 'NONE',  ( -0.8296751164775166831, 1358.402594231689591, 209.6218459617033432 ) ) ;
#44693 = CARTESIAN_POINT ( 'NONE',  ( -44.58457768240119634, 1432.195838635359905, 268.5431226110130183 ) ) ;
#44694 = CYLINDRICAL_SURFACE ( 'NONE', #39017, 2.000000000000003109 ) ;
#44695 = TOROIDAL_SURFACE ( 'NONE', #16027, 10.10241613150000006, 2.000000000000000000 ) ;
#44696 = ORIENTED_EDGE ( 'NONE', *, *, #18739, .F. ) ;
#44697 = CARTESIAN_POINT ( 'NONE',  ( -8.223595257310000406, 1424.414600115449957, 208.7481938478530026 ) ) ;
#44698 = VERTEX_POINT ( 'NONE', #12584 ) ;
#44699 = CARTESIAN_POINT ( 'NONE',  ( -1.704170752255000032, 1516.927039499179955, 209.8797722570040207 ) ) ;
#44700 = LINE ( 'NONE', #79394, #57339 ) ;
#44701 = CARTESIAN_POINT ( 'NONE',  ( -2.472529913803022783, 1523.678648413191695, 242.8674788698241400 ) ) ;
#44702 = DIRECTION ( 'NONE',  ( 0.000000000000000000, 0.000000000000000000, 1.000000000000000000 ) ) ;
#44703 = CARTESIAN_POINT ( 'NONE',  ( -1.555742980830479905, 1496.627161338389897, 221.3873943028199847 ) ) ;
#44704 = EDGE_LOOP ( 'NONE', ( #76979, #3043, #13917, #38266 ) ) ;
#44705 = FACE_OUTER_BOUND ( 'NONE', #71394, .T. ) ;
#44707 = CARTESIAN_POINT ( 'NONE',  ( 12.74111566449999877, 1416.823634022829992, 196.2610674185980031 ) ) ;
#44706 = CARTESIAN_POINT ( 'NONE',  ( -3.350338079455627671, 1523.604703353109926, 176.1628856388066708 ) ) ;
#44708 = ADVANCED_FACE ( 'NONE', ( #104437 ), #19468, .T. ) ;
#44709 = CARTESIAN_POINT ( 'NONE',  ( 0.07151796957733484728, 1487.750177387291160, 219.9735200923185801 ) ) ;
#44710 = CARTESIAN_POINT ( 'NONE',  ( -17.11766752880160070, 1508.551704408389924, 212.4296625737950137 ) ) ;
#44711 = EDGE_CURVE ( 'NONE', #32822, #95978, #108294, .T. ) ;
#44712 = CARTESIAN_POINT ( 'NONE',  ( 8.351583721560000839, 1472.370645083189856, 215.7586204441390123 ) ) ;
#44713 = CARTESIAN_POINT ( 'NONE',  ( -8.986849192036190814, 1439.553571704909928, 207.2559198570870080 ) ) ;
#44714 = VERTEX_POINT ( 'NONE', #108844 ) ;
#44715 = CARTESIAN_POINT ( 'NONE',  ( -23.40572486892139992, 1412.384539677990233, 270.0161358559570317 ) ) ;
#44716 = CARTESIAN_POINT ( 'NONE',  ( -7.339749373344999661, 1517.224900789629828, 207.4124613591469881 ) ) ;
#44717 = CARTESIAN_POINT ( 'NONE',  ( 7.889072528545669094, 1418.815176736690091, 232.2028265587920259 ) ) ;
#44718 = CARTESIAN_POINT ( 'NONE',  ( 8.457168192900248016, 1436.776849429390040, 207.4172901971049896 ) ) ;
#44720 = EDGE_LOOP ( 'NONE', ( #46513, #64327, #44234, #73720, #105437, #5629 ) ) ;
#44719 = CARTESIAN_POINT ( 'NONE',  ( -7.215824617674233998, 1365.903927215113299, 208.3718459617061285 ) ) ;
#44721 = ORIENTED_EDGE ( 'NONE', *, *, #88500, .F. ) ;
#44722 = CARTESIAN_POINT ( 'NONE',  ( -23.30090455988580089, 1410.145525358959958, 210.1953146085759840 ) ) ;
#44723 = EDGE_CURVE ( 'NONE', #23258, #91497, #37333, .T. ) ;
#44724 = CARTESIAN_POINT ( 'NONE',  ( -0.3188903335409049578, 1408.924196283109950, 186.5730539788620206 ) ) ;
#44725 = CARTESIAN_POINT ( 'NONE',  ( -20.30830883940000220, 1486.101309849389736, 213.0663049186690046 ) ) ;
#44726 = AXIS2_PLACEMENT_3D ( 'NONE', #86232, #64232, #87348 ) ;
#44727 = CARTESIAN_POINT ( 'NONE',  ( -20.53128328073639253, 1409.661528479226718, 266.7934139810452621 ) ) ;
#44728 = B_SPLINE_CURVE_WITH_KNOTS ( 'NONE', 3,
 ( #3434, #106962, #96930, #3985, #20197, #30247, #38654, #71199, #80115, #64441, #105882, #29705, #71765, #63889, #21275, #89609, #53853, #47079, #98557, #87990, #87425, #104771, #62245, #73929, #49282, #82318, #91269, #5054, #64982, #39199, #99646, #22376, #75593, #66647, #109188, #108059, #32473, #91810, #31908, #47622, #48736, #48180, #99098, #82862, #83411, #49834, #56025, #21826, #74492, #90150, #108620, #66096, #13432, #24034, #56576, #107514, #73376, #100748, #31355, #5616, #65539, #100223, #22936, #67188, #6706, #33001, #109724, #75037, #6153, #14547, #81748, #13993, #57141, #30804, #90707, #92356 ),
 .UNSPECIFIED., .F., .F.,
 ( 4, 3, 3, 3, 3, 3, 3, 3, 3, 3, 3, 3, 3, 3, 3, 3, 3, 3, 3, 3, 3, 3, 3, 3, 3, 4 ),
 ( -2.999999896493359852, -2.911009666304300136, -2.785025217194290192, -2.657589902942280258, -2.529356606326549795, -2.400046307149580116, -2.270317747582839996, -2.140430810404549966, -2.010654507406799851, -1.881600297076270190, -1.753346563294839955, -1.626095977948739835, -1.500000865187030019, -1.500000000000000000, -1.410945979647750148, -1.284708769301650122, -1.157056726448419948, -1.028638210627399907, -0.8992145056076812359, -0.7694284976191689829, -0.6395434986963102197, -0.5098282392343080893, -0.3809216422371468624, -0.2528616211501977240, -0.1258403872535915902, 4.440892098500626162E-16 ),
 .UNSPECIFIED. ) ;
#44729 = EDGE_CURVE ( 'NONE', #39065, #25781, #3377, .T. ) ;
#44730 = CARTESIAN_POINT ( 'NONE',  ( 1.968601690575629615, 1498.935401749600032, 197.9561509338619771 ) ) ;
#44731 = CARTESIAN_POINT ( 'NONE',  ( -18.75133052940000411, 1415.856152504829879, 223.8867772891979939 ) ) ;
#44732 = CARTESIAN_POINT ( 'NONE',  ( 5.341581777923300578, 1476.076623253339903, 267.5369962912580490 ) ) ;
#44733 = CARTESIAN_POINT ( 'NONE',  ( -11.67615777976660141, 1391.913060387279984, 209.2633225133189967 ) ) ;
#44734 = CARTESIAN_POINT ( 'NONE',  ( 10.37306595179999924, 1445.891253827790251, 186.4156611468980032 ) ) ;
#44735 = CARTESIAN_POINT ( 'NONE',  ( -3.461047329755000401, 1516.858765657450249, 205.6745815831370123 ) ) ;
#44736 = VERTEX_POINT ( 'NONE', #57912 ) ;
#44737 = CARTESIAN_POINT ( 'NONE',  ( -14.14968278069630081, 1452.475144026350108, 223.0094203056700053 ) ) ;
#44738 = CARTESIAN_POINT ( 'NONE',  ( 1.481821286034419982, 1476.734267533799994, 182.4382444874360090 ) ) ;
#44739 = VERTEX_POINT ( 'NONE', #29922 ) ;
#44740 = CARTESIAN_POINT ( 'NONE',  ( 4.987078416414999715, 1508.551704408389924, 212.6094384009469707 ) ) ;
#44741 = CARTESIAN_POINT ( 'NONE',  ( 25.20984846640109822, 1451.589895632459957, 136.8724018194579912 ) ) ;
#44742 = CARTESIAN_POINT ( 'NONE',  ( 14.20165756390000134, 1416.819756528530206, 196.5061806366979908 ) ) ;
#44743 = CARTESIAN_POINT ( 'NONE',  ( -46.14048177419999774, 1390.858208826580039, 234.9404857890590108 ) ) ;
#44744 = CARTESIAN_POINT ( 'NONE',  ( 7.489828918510000655, 1422.964606643100069, 195.6540423083989992 ) ) ;
#44745 = CARTESIAN_POINT ( 'NONE',  ( 18.79898005950000339, 1410.492675419430043, 194.9234042622980212 ) ) ;
#44746 = CARTESIAN_POINT ( 'NONE',  ( 12.73318793669440829, 1444.994950788470533, 164.6858276811441328 ) ) ;
#44747 = CARTESIAN_POINT ( 'NONE',  ( 2.603541569773797359, 1439.644274085440657, 183.4060696333851865 ) ) ;
#44749 = CARTESIAN_POINT ( 'NONE',  ( -22.07883734336632742, 1430.373802828663202, 217.8216703382841501 ) ) ;
#44748 = CARTESIAN_POINT ( 'NONE',  ( 0.4773158509259999849, 1416.462031948630056, 233.6651878465979735 ) ) ;
#44750 = EDGE_CURVE ( 'NONE', #65500, #97980, #46815, .T. ) ;
#44751 = DIRECTION ( 'NONE',  ( -1.000000000000000000, 0.000000000000000000, 0.000000000000000000 ) ) ;
#44752 = CARTESIAN_POINT ( 'NONE',  ( -8.270195822719999867, 1382.590927455500150, 218.4495833107989995 ) ) ;
#44753 = CARTESIAN_POINT ( 'NONE',  ( -5.773668852974999766, 1516.734985836460055, 213.1604834329569940 ) ) ;
#44754 = EDGE_CURVE ( 'NONE', #18368, #59235, #56649, .T. ) ;
#44755 = CARTESIAN_POINT ( 'NONE',  ( -21.05711716160297797, 1526.748660780343471, 233.6123052680180194 ) ) ;
#44756 = VERTEX_POINT ( 'NONE', #74713 ) ;
#44757 = CARTESIAN_POINT ( 'NONE',  ( -17.11904635710000022, 1417.409719763429848, 207.3632845816489976 ) ) ;
#44758 = CARTESIAN_POINT ( 'NONE',  ( 7.271052316819551109, 1517.151704408390060, 192.9032753742981470 ) ) ;
#44759 = CARTESIAN_POINT ( 'NONE',  ( -0.4465890250242970372, 1409.330979278389805, 232.7383886707189902 ) ) ;
#44760 = CARTESIAN_POINT ( 'NONE',  ( 3.727807031261289872, 1517.051706634850007, 202.5053387368750180 ) ) ;
#44761 = CARTESIAN_POINT ( 'NONE',  ( 1.711055448681089940E-31, 1424.874073124720098, 209.1218459616989946 ) ) ;
#44762 = CARTESIAN_POINT ( 'NONE',  ( 19.41157449629999832, 1457.417846740989944, 209.1218459616989946 ) ) ;
#44763 = CARTESIAN_POINT ( 'NONE',  ( -13.84930592310000108, 1450.388901282120059, 209.1218459616979999 ) ) ;
#44764 = CIRCLE ( 'NONE', #35875, 0.9999999999999971134 ) ;
#44765 = CARTESIAN_POINT ( 'NONE',  ( -2.908753373654089813, 1451.958507811900063, 184.7558797852969690 ) ) ;
#44766 = CARTESIAN_POINT ( 'NONE',  ( 11.87694622159999902, 1433.083833627729973, 150.0917096319979862 ) ) ;
#44767 = CARTESIAN_POINT ( 'NONE',  ( -2.115953714250000228, 1475.022810911229953, 269.6431591146979940 ) ) ;
#44768 = B_SPLINE_SURFACE_WITH_KNOTS ( 'NONE', 5, 1, ( 
 ( #66162, #21339 ),
 ( #22434, #74547 ),
 ( #4042, #14052 ),
 ( #90771, #65596 ),
 ( #89669, #73443 ),
 ( #21882, #12955 ),
 ( #47137, #30314 ),
 ( #20804, #13493 ),
 ( #14614, #63955 ) ),
 .UNSPECIFIED., .F., .F., .F.,
 ( 6, 3, 6 ),
 ( 2, 2 ),
 ( 0.000000000000000000, 4.040465094930000056, 8.068209695480000221 ),
 ( 0.000000000000000000, 14.00000000000000000 ),
 .UNSPECIFIED. ) ;
#44769 = CARTESIAN_POINT ( 'NONE',  ( 26.79041820568939869, 1440.913060391970021, 225.8523074638320054 ) ) ;
#44770 = CARTESIAN_POINT ( 'NONE',  ( -17.20183000400000140, 1421.414648929949863, 201.7791951163490012 ) ) ;
#44771 = EDGE_LOOP ( 'NONE', ( #17546, #59741, #8870, #3013, #48775 ) ) ;
#44772 = CARTESIAN_POINT ( 'NONE',  ( 0.1681681984989999989, 1418.913060387330006, 172.2701767054979882 ) ) ;
#44773 = CARTESIAN_POINT ( 'NONE',  ( -1.925297167936410148, 1521.951704408389787, 187.5582988455250018 ) ) ;
#44774 = CARTESIAN_POINT ( 'NONE',  ( -4.682538493039999139, 1486.134978737730080, 182.1338541308979870 ) ) ;
#44775 = CARTESIAN_POINT ( 'NONE',  ( 7.975931650403921935, 1398.149953820521660, 198.8561492682118228 ) ) ;
#44776 = CARTESIAN_POINT ( 'NONE',  ( -15.07933690175220143, 1509.452906090019951, 236.3415195119960117 ) ) ;
#44777 = TOROIDAL_SURFACE ( 'NONE', #107343, 2.000000000000000000, 1.000000000000000000 ) ;
#44778 = CARTESIAN_POINT ( 'NONE',  ( 21.80621299799999946, 1469.235547599130086, 222.1300559395980088 ) ) ;
#44779 = CARTESIAN_POINT ( 'NONE',  ( -15.90172418499818541, 1420.263238377089237, 209.8660166653201600 ) ) ;
#44780 = CARTESIAN_POINT ( 'NONE',  ( -8.365380114920000665, 1508.201457570829916, 235.3635179348979989 ) ) ;
#44781 = CARTESIAN_POINT ( 'NONE',  ( -34.81854416728349833, 1383.835731978919966, 233.6493107493720061 ) ) ;
#44782 = CARTESIAN_POINT ( 'NONE',  ( 20.66053749647389992, 1495.927313020109750, 225.6903912862549930 ) ) ;
#44783 = CARTESIAN_POINT ( 'NONE',  ( 10.45855884280000048, 1409.218564510729720, 219.7594970117980040 ) ) ;
#44784 = DIRECTION ( 'NONE',  ( 0.000000000000000000, 1.000000000000000000, 0.000000000000000000 ) ) ;
#44785 = CARTESIAN_POINT ( 'NONE',  ( 0.1674239622419670115, 1481.845507357109909, 182.0151124697109992 ) ) ;
#44787 = ORIENTED_EDGE ( 'NONE', *, *, #54326, .F. ) ;
#44786 = CARTESIAN_POINT ( 'NONE',  ( 4.077869218320000044, 1442.578371693189865, 217.0097321978689990 ) ) ;
#44788 = CARTESIAN_POINT ( 'NONE',  ( -0.5697963391879999895, 1450.893162800530263, 181.2886238165980046 ) ) ;
#44789 = FACE_OUTER_BOUND ( 'NONE', #78662, .T. ) ;
#44790 = CARTESIAN_POINT ( 'NONE',  ( -4.878146142590000345, 1474.403035727189945, 198.7818668649990173 ) ) ;
#44792 = ORIENTED_EDGE ( 'NONE', *, *, #15827, .T. ) ;
#44791 = CARTESIAN_POINT ( 'NONE',  ( -32.32092748916725355, 1524.075132568164918, 216.0999031672498063 ) ) ;
#44793 = CARTESIAN_POINT ( 'NONE',  ( -9.573057217335119162, 1423.428048935199740, 192.3355792750039939 ) ) ;
#44794 = VERTEX_POINT ( 'NONE', #66326 ) ;
#44795 = CARTESIAN_POINT ( 'NONE',  ( -12.36595038414849945, 1391.700200887409892, 209.7453690616009965 ) ) ;
#44796 = CARTESIAN_POINT ( 'NONE',  ( 0.1548802053370030019, 1489.973220511089949, 188.2279286174990034 ) ) ;
#44797 = CARTESIAN_POINT ( 'NONE',  ( 27.33789150208756524, 1509.867720594859293, 198.5752084302989147 ) ) ;
#44798 = EDGE_CURVE ( 'NONE', #62492, #67163, #99893, .T. ) ;
#44799 = CARTESIAN_POINT ( 'NONE',  ( -3.163732031489999930, 1432.489031102390072, 217.0770860277189911 ) ) ;
#44800 = VECTOR ( 'NONE', #52784, 1000.000000000000000 ) ;
#44801 = CARTESIAN_POINT ( 'NONE',  ( -10.96092256686609900, 1471.477682962149856, 206.8110093702159986 ) ) ;
#44802 = CARTESIAN_POINT ( 'NONE',  ( 12.21909990819059999, 1409.339760750069900, 217.7291232207390124 ) ) ;
#44803 = DIRECTION ( 'NONE',  ( 0.000000000000000000, 1.000000000000000000, 0.000000000000000000 ) ) ;
#44804 = CARTESIAN_POINT ( 'NONE',  ( -101.4799880583079954, 1385.224571067029956, 296.5271061909010086 ) ) ;
#44805 = CARTESIAN_POINT ( 'NONE',  ( -17.56738044160000101, 1412.957744255030093, 192.5650100598980146 ) ) ;
#44806 = CARTESIAN_POINT ( 'NONE',  ( 9.931488721813659382, 1423.381267080859971, 209.2494160290190166 ) ) ;
#44807 = ORIENTED_EDGE ( 'NONE', *, *, #43175, .T. ) ;
#44808 = CARTESIAN_POINT ( 'NONE',  ( 10.98780082597929919, 1490.670427006609998, 209.0313451347890066 ) ) ;
#44810 = ORIENTED_EDGE ( 'NONE', *, *, #20207, .T. ) ;
#44809 = DIRECTION ( 'NONE',  ( 1.755985294532464991E-16, -1.000000000000000000, 1.338183447452830017E-16 ) ) ;
#44811 = CARTESIAN_POINT ( 'NONE',  ( -113.4000000000000057, 1384.913060387289988, 304.2218459572590064 ) ) ;
#44812 = ORIENTED_EDGE ( 'NONE', *, *, #82003, .F. ) ;
#44813 = B_SPLINE_CURVE_WITH_KNOTS ( 'NONE', 3,
 ( #69685, #3580, #21963, #38791, #89754, #74623 ),
 .UNSPECIFIED., .F., .F.,
 ( 4, 2, 4 ),
 ( -0.03892040104653909927, -0.01978009174228249900, -5.188642626663408919E-09 ),
 .UNSPECIFIED. ) ;
#44814 = CARTESIAN_POINT ( 'NONE',  ( 24.72376531809999989, 1509.776433298830170, 223.3047247638980082 ) ) ;
#44815 = CARTESIAN_POINT ( 'NONE',  ( 5.037373810890384718, 1363.064638354549515, 209.6218459617148824 ) ) ;
#44816 = CARTESIAN_POINT ( 'NONE',  ( -11.17933822150000012, 1434.140065272970105, 151.6287470207980164 ) ) ;
#44817 = AXIS2_PLACEMENT_3D ( 'NONE', #86749, #36344, #78922 ) ;
#44818 = EDGE_CURVE ( 'NONE', #72801, #75901, #4727, .T. ) ;
#44819 = CARTESIAN_POINT ( 'NONE',  ( 35.05450822442378467, 1457.715342177672028, 269.5322532702526246 ) ) ;
#44820 = CARTESIAN_POINT ( 'NONE',  ( -8.656560647815000564, 1514.517422889970021, 203.9087166159570188 ) ) ;
#44821 = CARTESIAN_POINT ( 'NONE',  ( 4.717917756090000303, 1396.259829913929934, 220.1600754375980102 ) ) ;
#44822 = CARTESIAN_POINT ( 'NONE',  ( 2.715010028530000064, 1417.669881552329798, 234.6652376653979957 ) ) ;
#44823 = CARTESIAN_POINT ( 'NONE',  ( -7.081311148617888129, 1516.557149304009954, 211.5931455169218793 ) ) ;
#44824 = CARTESIAN_POINT ( 'NONE',  ( -1.182076869679999920, 1452.180487653529781, 183.6023549528979686 ) ) ;
#44825 = CARTESIAN_POINT ( 'NONE',  ( -7.450033292399999674, 1367.931913175460068, 207.6218459616989946 ) ) ;
#44826 = CARTESIAN_POINT ( 'NONE',  ( -26.47803665465272260, 1436.726639266544453, 136.8122681834409207 ) ) ;
#44827 = CARTESIAN_POINT ( 'NONE',  ( -29.30029655192934257, 1525.907212628473644, 221.3719603026177367 ) ) ;
#44828 = CARTESIAN_POINT ( 'NONE',  ( 1.118353215965000036, 1516.977201124959947, 206.6281488911770055 ) ) ;
#44829 = CARTESIAN_POINT ( 'NONE',  ( -13.02114638533239876, 1434.814403427030129, 149.4658423292819975 ) ) ;
#44830 = CARTESIAN_POINT ( 'NONE',  ( -1.154631945609999823E-14, 1421.542806690330053, 144.1893924737979944 ) ) ;
#44831 = CARTESIAN_POINT ( 'NONE',  ( -0.3757451851924459851, 1473.184910198040143, 188.5980016707920299 ) ) ;
#44832 = CARTESIAN_POINT ( 'NONE',  ( -3.685264706689999947, 1496.073670527689728, 219.7127572917990221 ) ) ;
#44833 = CARTESIAN_POINT ( 'NONE',  ( 40.38134792428180475, 1444.189104679979891, 137.0917438250710063 ) ) ;
#44834 = ORIENTED_EDGE ( 'NONE', *, *, #12307, .T. ) ;
#44835 = CARTESIAN_POINT ( 'NONE',  ( 43.50119000050000295, 1440.913060359109977, 263.8966302655979916 ) ) ;
#44836 = CARTESIAN_POINT ( 'NONE',  ( -26.39526639180000345, 1469.246565964829870, 207.8134133741079950 ) ) ;
#44838 = CARTESIAN_POINT ( 'NONE',  ( 16.68432847059190038, 1409.595862666960102, 192.9240629956530029 ) ) ;
#44837 = CARTESIAN_POINT ( 'NONE',  ( -10.96674589548630152, 1426.064964913880203, 96.72801120346360904 ) ) ;
#44839 = CARTESIAN_POINT ( 'NONE',  ( 0.01328393942530149870, 1516.939580991450157, 212.3834982571270018 ) ) ;
#44840 =( BOUNDED_CURVE ( )  B_SPLINE_CURVE ( 3, ( #12574, #106622, #29909, #1995 ),
 .UNSPECIFIED., .F., .F. ) 
 B_SPLINE_CURVE_WITH_KNOTS ( ( 4, 4 ),
 ( 1.282864256197260078, 2.438226007366384618 ),
 .UNSPECIFIED. ) 
 CURVE ( )  GEOMETRIC_REPRESENTATION_ITEM ( )  RATIONAL_B_SPLINE_CURVE ( ( 1.000000000000000000, 0.8918208900530331107, 0.8918208900530331107, 1.000000000000000000 ) ) 
 REPRESENTATION_ITEM ( '' )  );
#44841 = CARTESIAN_POINT ( 'NONE',  ( 1.175130270553210066, 1395.954096840620196, 198.1774300419000099 ) ) ;
#44842 = AXIS2_PLACEMENT_3D ( 'NONE', #63692, #98359, #79923 ) ;
#44843 = DIRECTION ( 'NONE',  ( 1.733298337313369794E-15, -0.8730714504182227609, -0.4875922912276409171 ) ) ;
#44844 = CARTESIAN_POINT ( 'NONE',  ( -25.82475784780000083, 1425.523015327230041, 244.3435519318979914 ) ) ;
#44845 = CARTESIAN_POINT ( 'NONE',  ( -1.121951540329999775, 1488.104705274990010, 219.9473760328990011 ) ) ;
#44847 = ADVANCED_FACE ( 'NONE', ( #107191 ), #59072, .F. ) ;
#44846 = CARTESIAN_POINT ( 'NONE',  ( 28.53735979763590080, 1509.098833403789740, 209.4635936774309926 ) ) ;
#44848 = CARTESIAN_POINT ( 'NONE',  ( -4.992349863779999453, 1391.620913471789891, 214.4361776263990009 ) ) ;
#44849 = CARTESIAN_POINT ( 'NONE',  ( 33.52142403570000084, 1451.742483455429920, 134.7272099485979879 ) ) ;
#44850 = ORIENTED_EDGE ( 'NONE', *, *, #25595, .F. ) ;
#44851 = CARTESIAN_POINT ( 'NONE',  ( 3.515651971320000069, 1396.218664545030151, 197.1791320925980244 ) ) ;
#44852 = CARTESIAN_POINT ( 'NONE',  ( 10.90988536168999978, 1460.796490171650021, 208.2422925045810018 ) ) ;
#44853 = EDGE_CURVE ( 'NONE', #59125, #61195, #62387, .T. ) ;
#44854 = CARTESIAN_POINT ( 'NONE',  ( -16.51558990230000035, 1459.313172484830147, 228.9821122170980061 ) ) ;
#44855 = ORIENTED_EDGE ( 'NONE', *, *, #58388, .F. ) ;
#44856 = ORIENTED_EDGE ( 'NONE', *, *, #72941, .T. ) ;
#44857 = CARTESIAN_POINT ( 'NONE',  ( 9.047070330427949614, 1452.614645995950013, 211.8941571659140095 ) ) ;
#44858 = CARTESIAN_POINT ( 'NONE',  ( 8.855603127469999336, 1423.529354507180187, 196.4827216600990027 ) ) ;
#44859 = EDGE_CURVE ( 'NONE', #69308, #11716, #34345, .T. ) ;
#44860 = VERTEX_POINT ( 'NONE', #59560 ) ;
#44861 = CARTESIAN_POINT ( 'NONE',  ( -3.364077551112700348, 1507.415397232589839, 221.5352637752980058 ) ) ;
#44862 = CARTESIAN_POINT ( 'NONE',  ( -9.843249962089998917, 1461.614812224390107, 208.6141224610979918 ) ) ;
#44863 = VECTOR ( 'NONE', #41823, 1000.000000000000000 ) ;
#44864 = CARTESIAN_POINT ( 'NONE',  ( -19.46624395007912156, 1486.378570646362505, 189.7119165574182205 ) ) ;
#44865 = EDGE_CURVE ( 'NONE', #63875, #32555, #75804, .T. ) ;
#44866 = CARTESIAN_POINT ( 'NONE',  ( 27.33695563809355633, 1509.220067111051776, 206.1721638638696561 ) ) ;
#44867 = CARTESIAN_POINT ( 'NONE',  ( 0.6444153132796710537, 1420.643208713479908, 182.8466803230259927 ) ) ;
#44868 = CARTESIAN_POINT ( 'NONE',  ( 9.172898573127410415, 1450.102442297790049, 208.3180252651680178 ) ) ;
#44869 = CARTESIAN_POINT ( 'NONE',  ( 1.702379247829999942, 1501.792222158089999, 230.4488007676989980 ) ) ;
#44870 = FACE_OUTER_BOUND ( 'NONE', #19044, .T. ) ;
#44871 = CARTESIAN_POINT ( 'NONE',  ( -1.710004586925000236, 1516.557392317769882, 202.5758445815369839 ) ) ;
#44872 = CARTESIAN_POINT ( 'NONE',  ( 7.339749335215000059, 1517.224900789629828, 210.8312305431869902 ) ) ;
#44873 = ORIENTED_EDGE ( 'NONE', *, *, #45205, .F. ) ;
#44874 = CARTESIAN_POINT ( 'NONE',  ( 11.86350184823050036, 1432.154420217069855, 149.9793174209499966 ) ) ;
#44875 = B_SPLINE_CURVE_WITH_KNOTS ( 'NONE', 3,
 ( #49274, #83403, #22927, #108611, #73921, #6699, #40854, #31900, #100741, #57132, #84509, #75585, #75029, #31346, #57687, #65530, #99637, #91801, #91259, #49827, #109180, #24025, #14539, #48728, #82854, #58225, #92349, #16181, #15621, #73367, #83957, #107506, #24577, #7257, #109717, #101282, #30796, #17273, #18944, #7798, #9461, #59882, #18388 ),
 .UNSPECIFIED., .F., .F.,
 ( 4, 3, 3, 3, 3, 3, 3, 3, 3, 3, 3, 3, 3, 3, 4 ),
 ( 2.099667498829999878E-15, 1.406846277637760156, 2.814198252419170210, 4.220686603073059651, 5.623444216349149372, 7.022781117988579958, 8.415638966051240288, 8.942376872057339554, 10.31946110557949936, 11.69383206961379962, 13.06413089926859961, 14.42602073298239773, 15.78206364908349890, 17.12804210909719771, 17.88475318529999925 ),
 .UNSPECIFIED. ) ;
#44876 = DIRECTION ( 'NONE',  ( 0.000000000000000000, 0.000000000000000000, -1.000000000000000000 ) ) ;
#44877 = ORIENTED_EDGE ( 'NONE', *, *, #78189, .T. ) ;
#44878 = CARTESIAN_POINT ( 'NONE',  ( -15.56469051740000076, 1506.798305107229908, 193.1680121121979994 ) ) ;
#44879 = CARTESIAN_POINT ( 'NONE',  ( -6.528218896545719296, 1508.485824417290132, 219.7230302621430269 ) ) ;
#44880 = CARTESIAN_POINT ( 'NONE',  ( -11.90008666459999986, 1434.920851464509951, 147.6452002888979962 ) ) ;
#44881 = VECTOR ( 'NONE', #95578, 1000.000000000000000 ) ;
#44882 = CARTESIAN_POINT ( 'NONE',  ( -9.541786836099248603, 1471.456755149039736, 212.5898191071979966 ) ) ;
#44883 = CARTESIAN_POINT ( 'NONE',  ( -4.593646130120000670, 1423.772470591829915, 184.4006771823979989 ) ) ;
#44884 = CARTESIAN_POINT ( 'NONE',  ( 1.469863004249710059, 1407.943267555710008, 270.2923612881479585 ) ) ;
#44885 = CARTESIAN_POINT ( 'NONE',  ( 9.157303188274740435, 1450.042022675190083, 208.2002544115800049 ) ) ;
#44886 = CARTESIAN_POINT ( 'NONE',  ( -6.694418385159999652, 1473.791160286789818, 199.7891180969089930 ) ) ;
#44887 = CARTESIAN_POINT ( 'NONE',  ( -2.434348319423109697, 1422.283838751350004, 192.8362627702539953 ) ) ;
#44888 = CARTESIAN_POINT ( 'NONE',  ( -32.53397683490000247, 1379.726329037039932, 216.1069825312089847 ) ) ;
#44889 = CARTESIAN_POINT ( 'NONE',  ( 8.360704762653028865, 1424.462288153377131, 195.7412347175665559 ) ) ;
#44891 = CARTESIAN_POINT ( 'NONE',  ( 10.78499426627680080, 1469.831216462720022, 205.6638516619669872 ) ) ;
#44890 = CARTESIAN_POINT ( 'NONE',  ( -18.93088166866530031, 1481.225508140669945, 189.7381378927790081 ) ) ;
#44892 = CARTESIAN_POINT ( 'NONE',  ( -67.84113287130467995, 1379.747601269228880, 279.1899061518716394 ) ) ;
#44893 = CARTESIAN_POINT ( 'NONE',  ( -9.937510298460209057, 1439.652175453890095, 208.0161710764309930 ) ) ;
#44894 = ADVANCED_FACE ( 'NONE', ( #15855 ), #16954, .T. ) ;
#44895 = CARTESIAN_POINT ( 'NONE',  ( -7.194888370995000670, 1513.142795523600171, 201.8217789698469744 ) ) ;
#44896 = ORIENTED_EDGE ( 'NONE', *, *, #3684, .T. ) ;
#44897 = CARTESIAN_POINT ( 'NONE',  ( 36.06124927020000115, 1436.776486031050126, 262.6648722463980334 ) ) ;
#44898 = CARTESIAN_POINT ( 'NONE',  ( 13.72150112095459917, 1434.975563626920120, 148.6100187623320039 ) ) ;
#44899 = CARTESIAN_POINT ( 'NONE',  ( -20.88378052025218068, 1525.556089352309073, 233.6619250012938380 ) ) ;
#44900 = AXIS2_PLACEMENT_3D ( 'NONE', #85520, #57613, #109106 ) ;
#44901 = CARTESIAN_POINT ( 'NONE',  ( -9.094129269030000629, 1384.954944735329946, 199.9429221374590213 ) ) ;
#44902 = EDGE_CURVE ( 'NONE', #2433, #15049, #25872, .T. ) ;
#44903 = CARTESIAN_POINT ( 'NONE',  ( 11.79348306668460111, 1408.364582718329984, 270.1182552284680014 ) ) ;
#44905 = VERTEX_POINT ( 'NONE', #84735 ) ;
#44904 = CARTESIAN_POINT ( 'NONE',  ( -1.251490820319690167, 1515.089511802750167, 204.7930444736340121 ) ) ;
#44906 = CARTESIAN_POINT ( 'NONE',  ( -15.79765598458050491, 1415.826759071379229, 209.7038822556229434 ) ) ;
#44907 = CIRCLE ( 'NONE', #73512, 1.000000000000000888 ) ;
#44908 = CARTESIAN_POINT ( 'NONE',  ( -24.09704111839999996, 1443.988162845919987, 212.1154897055279775 ) ) ;
#44909 = FACE_OUTER_BOUND ( 'NONE', #63732, .T. ) ;
#44910 = CARTESIAN_POINT ( 'NONE',  ( 1.302631559684990004, 1430.876257361340095, 199.7563870752120181 ) ) ;
#44911 = CARTESIAN_POINT ( 'NONE',  ( 10.96015508933500016, 1512.830284628050094, 225.0317485278669949 ) ) ;
#44912 = CARTESIAN_POINT ( 'NONE',  ( 4.107457091549650663, 1370.394943853835002, 209.7763353197741480 ) ) ;
#44913 = CARTESIAN_POINT ( 'NONE',  ( 6.588559639229999654, 1509.276047527829860, 179.0991342149980028 ) ) ;
#44914 = CARTESIAN_POINT ( 'NONE',  ( -1.909779004914694767, 1526.107876515966382, 240.8769758466254132 ) ) ;
#44915 = CARTESIAN_POINT ( 'NONE',  ( -11.16733641199999916, 1453.313060387329870, 225.4924597496980141 ) ) ;
#44916 = CARTESIAN_POINT ( 'NONE',  ( 14.66309662039999928, 1412.744218893529933, 227.7783495036979957 ) ) ;
#44917 = CARTESIAN_POINT ( 'NONE',  ( -6.769446762680000340, 1477.849490981190229, 218.6333586432590153 ) ) ;
#44918 = DIRECTION ( 'NONE',  ( -0.9991331916196766194, 0.04162763470901477414, -7.370489309664139796E-05 ) ) ;
#44919 = CARTESIAN_POINT ( 'NONE',  ( -7.725372170364999569, 1517.158319634930194, 206.2490093095770192 ) ) ;
#44920 = CARTESIAN_POINT ( 'NONE',  ( 41.33291310559999943, 1425.226874449430170, 266.5540610868980025 ) ) ;
#44921 = CARTESIAN_POINT ( 'NONE',  ( 5.923682464646780943, 1517.051704408389924, 194.3813127491490036 ) ) ;
#44922 = CARTESIAN_POINT ( 'NONE',  ( 18.25065742789999845, 1435.135490642300056, 145.6248056324979814 ) ) ;
#44923 = CARTESIAN_POINT ( 'NONE',  ( 20.60562827940000119, 1469.157082743329966, 193.0059214098980078 ) ) ;
#44924 = CARTESIAN_POINT ( 'NONE',  ( -22.49610135040000003, 1431.913548303140033, 217.2868528580380030 ) ) ;
#44925 = CARTESIAN_POINT ( 'NONE',  ( -12.23665942925899941, 1377.661379157180136, 207.7791151321639802 ) ) ;
#44926 = CARTESIAN_POINT ( 'NONE',  ( -0.8855859651640000108, 1475.830651730830141, 266.9608409856979847 ) ) ;
#44927 = CARTESIAN_POINT ( 'NONE',  ( 32.38845791999501245, 1523.382868172864164, 216.1254071228445639 ) ) ;
#44928 = CARTESIAN_POINT ( 'NONE',  ( -41.66467407060099504, 1443.190448348939981, 136.0675278794840040 ) ) ;
#44929 = CARTESIAN_POINT ( 'NONE',  ( -17.04521562810680280, 1526.211523310372513, 182.6481121783497770 ) ) ;
#44930 = CARTESIAN_POINT ( 'NONE',  ( -16.32386383359999726, 1416.417362032049823, 209.4515642215840217 ) ) ;
#44931 = CARTESIAN_POINT ( 'NONE',  ( -12.31367500480000032, 1442.688057702260039, 186.5150438736980050 ) ) ;
#44932 = CARTESIAN_POINT ( 'NONE',  ( -27.80059196791649967, 1508.274126421260007, 210.4902684585850068 ) ) ;
#44933 = CARTESIAN_POINT ( 'NONE',  ( 18.09194291044959613, 1429.328450707060028, 207.2811966920800160 ) ) ;
#44934 = SPHERICAL_SURFACE ( 'NONE', #22825, 0.5000000000000000000 ) ;
#44935 = ORIENTED_EDGE ( 'NONE', *, *, #103543, .T. ) ;
#44936 = CARTESIAN_POINT ( 'NONE',  ( 5.818054393111782296, 1510.580107409934271, 216.6577242164569839 ) ) ;
#44937 = CARTESIAN_POINT ( 'NONE',  ( -14.92887067431809989, 1409.434388038909901, 209.5123278269470006 ) ) ;
#44938 = CARTESIAN_POINT ( 'NONE',  ( -13.59512978074699951, 1507.703334056939866, 209.3532892538999874 ) ) ;
#44939 = CARTESIAN_POINT ( 'NONE',  ( -5.371114210517032639, 1422.361293165692587, 138.9481839148339759 ) ) ;
#44940 = CARTESIAN_POINT ( 'NONE',  ( -44.47031950239999532, 1451.019422310730079, 266.2216427720979937 ) ) ;
#44941 = CARTESIAN_POINT ( 'NONE',  ( -30.77244971921803085, 1524.972613296804866, 196.5524914208872644 ) ) ;
#44942 = CARTESIAN_POINT ( 'NONE',  ( 0.4823992292522150116, 1418.714218680099975, 184.7113719357920161 ) ) ;
#44943 = CARTESIAN_POINT ( 'NONE',  ( -22.57318049250000058, 1409.701333220029937, 209.4509250479570142 ) ) ;
#44944 = CARTESIAN_POINT ( 'NONE',  ( -60.29191067893739842, 1384.694631598589922, 281.4556533462259722 ) ) ;
#44945 = CARTESIAN_POINT ( 'NONE',  ( -42.22056685433029344, 1384.995465601839896, 215.1295050435799965 ) ) ;
#44946 = CARTESIAN_POINT ( 'NONE',  ( 16.94821773669399789, 1422.804739068089930, 226.9354301654539938 ) ) ;
#44947 = CARTESIAN_POINT ( 'NONE',  ( 14.63039435740000016, 1416.519106787730152, 219.7110180114979983 ) ) ;
#44948 = CARTESIAN_POINT ( 'NONE',  ( 15.48562912010000048, 1495.933122566730162, 224.0697311691979792 ) ) ;
#44949 = CARTESIAN_POINT ( 'NONE',  ( -8.752495015159368563, 1495.068115196657800, 202.1315847339255356 ) ) ;
#44950 = CARTESIAN_POINT ( 'NONE',  ( -2.162165485562111300, 1370.150135755310203, 206.8746041456742830 ) ) ;
#44951 = CARTESIAN_POINT ( 'NONE',  ( -8.371438403939999162, 1384.922510205190065, 199.7749754636789987 ) ) ;
#44952 = CARTESIAN_POINT ( 'NONE',  ( -106.4020496450190052, 1391.913060387289988, 304.2007955189830568 ) ) ;
#44953 = CLOSED_SHELL ( 'NONE', ( #103341, #78275, #55892, #1415, #16716, #10437, #32090, #50326, #44254, #16482, #41997, #79005, #78874, #42169, #98700, #62851, #93080, #65449, #76023, #9780, #72017, #104540, #26349, #109046, #67933, #107495, #73044, #102068, #7710, #71322, #34310, #66560, #96671, #26719, #65819, #90864, #23607, #49818, #8524, #58177, #33307, #98730, #62666, #15249, #6259, #39925, #54222, #52080, #34469, #7156, #39788, #63269, #99538, #34241, #79549, #69861, #51042, #81663, #30586, #21260, #87158, #38895, #72296, #71565, #14568, #46560, #63066, #108048, #78824, #109570, #105768, #87674, #22284, #14445, #7917, #70803, #101106, #61960, #93467, #8880, #46613, #67888, #6171, #22019, #64830, #936, #25551, #101428, #30937, #91062, #66719, #88224, #3156, #103527, #3180, #7808, #86372, #83616, #26121, #61105, #67076, #29038, #46112, #106288, #63904, #40601, #93830, #81053, #98166, #21933, #109181, #84349, #97414, #98823, #90455, #42528, #59753, #91216, #106119, #70427, #18804, #25706, #57398, #74655, #59902, #78353, #33620, #81721, #77480, #106389, #84506, #80856, #35749, #106422, #85255, #4854, #45357, #108819, #110353, #51383, #60360, #77118, #100094, #35789, #46161, #63953, #87145, #91196, #78153, #20599, #71454, #36952, #21212, #100317, #31335, #75696, #72132, #55852, #65773, #13364, #76069, #73407, #76783, #24468, #38627, #99489, #8501, #89722, #91472, #47477, #7635, #53561, #37189, #54240, #5756, #28265, #17083, #65225, #102374, #50678, #106079, #31556, #62458, #1496, #16007, #92554, #16012, #58976, #10568, #63353, #81234, #67946, #50845, #99541, #29821, #88740, #63827, #13714, #102769, #67831, #22071, #42046, #20916, #79752, #96818, #104851, #42956, #104094, #1885, #39092, #99996, #97378, #45971, #101913, #77069, #76203, #47500, #4994, #68081, #4885, #64650, #40142, #106121, #68396, #54516, #37224, #83564, #84510, #43834, #19569, #70679, #65972, #61743, #101920, #97684, #29926, #42714, #25722, #109038, #58973, #80848, #50636, #73673, #39990, #59716, #8248, #49327, #108937, #102058, #83028, #97309, #90694, #89365, #9654, #80213, #70797, #39216, #6567, #65893, #22178, #102240, #29619, #49374, #103572, #37146, #36620, #23411, #84337, #40582, #14319, #2516, #46915, #36367, #54155, #44847, #65469, #88505, #19893, #67226, #89674, #71554, #105269, #9935, #64873, #94566, #5913, #33815, #40506, #43199, #9166, #41178, #87077, #86537, #10469, #94593, #104089, #66897, #17211, #30364, #44042, #51024, #31620, #75204, #70923, #33826, #36515, #26215, #37024, #95122, #107523, #6413, #88543 ) ) ;
#44954 = CARTESIAN_POINT ( 'NONE',  ( 17.63393959649999942, 1415.931784856029935, 206.2978456718479947 ) ) ;
#44955 = CARTESIAN_POINT ( 'NONE',  ( -12.26979136719999985, 1416.828040475729949, 194.6643372668980021 ) ) ;
#44956 = CARTESIAN_POINT ( 'NONE',  ( 3.242267180889999878, 1423.555505585929950, 193.2269609960989953 ) ) ;
#44957 = CARTESIAN_POINT ( 'NONE',  ( 23.77260840609999804, 1411.103764635429798, 210.9084169415280030 ) ) ;
#44958 = CARTESIAN_POINT ( 'NONE',  ( -106.9324727664809984, 1391.913060387289988, 306.5339839144160123 ) ) ;
#44959 = CARTESIAN_POINT ( 'NONE',  ( 18.74597378714840090, 1457.928134532490049, 220.6238524344490202 ) ) ;
#44960 = CARTESIAN_POINT ( 'NONE',  ( -15.49281651649999958, 1421.632445824929846, 227.2929371620980135 ) ) ;
#44962 = CARTESIAN_POINT ( 'NONE',  ( -8.407515995729999858, 1383.335842388670017, 199.9217961407289863 ) ) ;
#44961 = CARTESIAN_POINT ( 'NONE',  ( -11.58425284650000009, 1432.866144662169972, 151.1952032978979901 ) ) ;
#44963 = CARTESIAN_POINT ( 'NONE',  ( 0.3007953952340000070, 1410.295994791430076, 233.2561088422980049 ) ) ;
#44964 = CARTESIAN_POINT ( 'NONE',  ( -113.4000000000000057, 1375.179104070690073, 291.9637869975589979 ) ) ;
#44965 = CARTESIAN_POINT ( 'NONE',  ( -10.90539778630000001, 1489.991646564889834, 212.3805117938089779 ) ) ;
#44966 = CARTESIAN_POINT ( 'NONE',  ( -22.52609268272879817, 1509.699688877640028, 190.9355248210520131 ) ) ;
#44967 = CARTESIAN_POINT ( 'NONE',  ( -0.8004569503022459509, 1420.698947351120069, 183.5197807342519809 ) ) ;
#44968 = AXIS2_PLACEMENT_3D ( 'NONE', #88718, #97112, #89800 ) ;
#44969 = CARTESIAN_POINT ( 'NONE',  ( -6.559798094425000059, 1516.987478262539980, 204.5068286042669854 ) ) ;
#44970 = CARTESIAN_POINT ( 'NONE',  ( -18.59208672289999953, 1425.224709566930187, 227.1497469740980080 ) ) ;
#44971 = CARTESIAN_POINT ( 'NONE',  ( -14.71962813352180000, 1485.852042466279954, 186.4453625732280102 ) ) ;
#44972 = CARTESIAN_POINT ( 'NONE',  ( 7.656493703591820577, 1504.159369564410099, 219.4142504822630144 ) ) ;
#44973 = CARTESIAN_POINT ( 'NONE',  ( -13.77489446762966097, 1421.087469475355419, 210.6290704798021522 ) ) ;
#44975 = ORIENTED_EDGE ( 'NONE', *, *, #80239, .F. ) ;
#44974 = CARTESIAN_POINT ( 'NONE',  ( -65.84351248663899980, 1379.744198721029989, 276.1294122088469862 ) ) ;
#44976 = ORIENTED_EDGE ( 'NONE', *, *, #27798, .T. ) ;
#44977 = CARTESIAN_POINT ( 'NONE',  ( 11.40351120802290019, 1433.961723248389944, 151.4265909395499818 ) ) ;
#44978 = CARTESIAN_POINT ( 'NONE',  ( 21.83550407203902921, 1523.678648413191468, 183.2743720722706939 ) ) ;
#44979 = ORIENTED_EDGE ( 'NONE', *, *, #63202, .F. ) ;
#44980 = DIRECTION ( 'NONE',  ( 0.000000000000000000, 0.000000000000000000, 1.000000000000000000 ) ) ;
#44981 = CARTESIAN_POINT ( 'NONE',  ( 1.547463840030000037, 1414.913060387329779, 192.3096136973980208 ) ) ;
#44983 = CARTESIAN_POINT ( 'NONE',  ( 0.1578430167310000132, 1507.631289506030271, 180.9061429542980193 ) ) ;
#44982 = CARTESIAN_POINT ( 'NONE',  ( 15.98819541800289912, 1421.269252389829944, 191.1953072301890018 ) ) ;
#44984 = CARTESIAN_POINT ( 'NONE',  ( 5.258395203887199720, 1466.657720361110023, 214.1037399434610222 ) ) ;
#44985 = AXIS2_PLACEMENT_3D ( 'NONE', #90574, #6581, #14956 ) ;
#44986 = CARTESIAN_POINT ( 'NONE',  ( 2.829025757189999712, 1488.172259156529890, 182.2276165502979950 ) ) ;
#44987 = CARTESIAN_POINT ( 'NONE',  ( -105.9555828394970121, 1378.913060388860004, 305.1986518409329960 ) ) ;
#44988 = CARTESIAN_POINT ( 'NONE',  ( -24.14169241750170158, 1444.792590611489913, 211.6367681704030019 ) ) ;
#44989 = EDGE_CURVE ( 'NONE', #61631, #50836, #89207, .T. ) ;
#44990 = CARTESIAN_POINT ( 'NONE',  ( -4.609064341505000328, 1516.723920667490120, 211.9995909164769898 ) ) ;
#44991 = CARTESIAN_POINT ( 'NONE',  ( 34.31734398635919803, 1435.703512753839959, 134.0999999980490145 ) ) ;
#44994 =( BOUNDED_CURVE ( )  B_SPLINE_CURVE ( 3, ( #94277, #16446, #101562, #103220 ),
 .UNSPECIFIED., .F., .T. ) 
 B_SPLINE_CURVE_WITH_KNOTS ( ( 4, 4 ),
 ( 1.003383811351443944, 2.138208849194395356 ),
 .UNSPECIFIED. ) 
 CURVE ( )  GEOMETRIC_REPRESENTATION_ITEM ( )  RATIONAL_B_SPLINE_CURVE ( ( 1.000000000000000000, 0.8955296286887992618, 0.8955296286887992618, 1.000000000000000000 ) ) 
 REPRESENTATION_ITEM ( '' )  );
#44993 = CIRCLE ( 'NONE', #58289, 28.41070217520000440 ) ;
#44992 = CARTESIAN_POINT ( 'NONE',  ( -3.365241614647759949, 1429.250033114370126, 207.0884890221589956 ) ) ;
#44995 = DIRECTION ( 'NONE',  ( 2.081668171172166620E-14, 0.000000000000000000, 1.000000000000000000 ) ) ;
#44996 = VERTEX_POINT ( 'NONE', #16409 ) ;
#44997 = CARTESIAN_POINT ( 'NONE',  ( 13.74453438472139943, 1436.216212073029965, 150.3798774187329741 ) ) ;
#44998 = CARTESIAN_POINT ( 'NONE',  ( 0.2579780539924840244, 1432.430230534230077, 200.6906244575169751 ) ) ;
#44999 = ORIENTED_EDGE ( 'NONE', *, *, #87105, .F. ) ;
#45000 = ORIENTED_EDGE ( 'NONE', *, *, #107812, .F. ) ;
#45001 = ORIENTED_EDGE ( 'NONE', *, *, #79567, .T. ) ;
#45002 = CARTESIAN_POINT ( 'NONE',  ( -7.660003975705000023, 1511.444830760690138, 215.2207434837270057 ) ) ;
#45003 = CARTESIAN_POINT ( 'NONE',  ( 16.77006244281658809, 1513.317537412908678, 196.3881396080545585 ) ) ;
#45004 = CARTESIAN_POINT ( 'NONE',  ( 12.68026019944470129, 1500.377008822790231, 208.5091319790680018 ) ) ;
#45005 = CARTESIAN_POINT ( 'NONE',  ( -8.862244220539999162, 1384.927755921120252, 218.6851219245690174 ) ) ;
#45006 = CARTESIAN_POINT ( 'NONE',  ( 9.694557698469999707, 1462.254025601890135, 208.2085395626110085 ) ) ;
#45007 = AXIS2_PLACEMENT_3D ( 'NONE', #11987, #37195, #87605 ) ;
#45008 = CARTESIAN_POINT ( 'NONE',  ( -12.34597541399999976, 1378.750906298520249, 209.0838709649310090 ) ) ;
#45009 = CARTESIAN_POINT ( 'NONE',  ( -16.42994098213877052, 1379.596574317858085, 208.1847039279784610 ) ) ;
#45010 = CARTESIAN_POINT ( 'NONE',  ( 3.168476225200000052, 1465.480445073689907, 199.6310402015890020 ) ) ;
#45011 = ADVANCED_FACE ( 'NONE', ( #43314 ), #3441, .F. ) ;
#45012 = CARTESIAN_POINT ( 'NONE',  ( 20.20959865099471031, 1512.187213306747481, 182.0120230947219966 ) ) ;
#45013 = ORIENTED_EDGE ( 'NONE', *, *, #24212, .F. ) ;
#45014 = CARTESIAN_POINT ( 'NONE',  ( -0.01319654689839849966, 1516.941178807709775, 206.8296289214069930 ) ) ;
#45015 = ORIENTED_EDGE ( 'NONE', *, *, #42532, .T. ) ;
#45016 = CARTESIAN_POINT ( 'NONE',  ( 23.97023455779339685, 1440.913060387330006, 235.5343584298519772 ) ) ;
#45017 = CARTESIAN_POINT ( 'NONE',  ( -14.12785558649999906, 1509.345507846829832, 183.3895937959979676 ) ) ;
#45018 = ORIENTED_EDGE ( 'NONE', *, *, #100730, .F. ) ;
#45019 = CARTESIAN_POINT ( 'NONE',  ( 25.58350377144139998, 1449.893453280530139, 137.3546802799529871 ) ) ;
#45020 = EDGE_CURVE ( 'NONE', #19394, #92807, #96172, .T. ) ;
#45021 = CARTESIAN_POINT ( 'NONE',  ( -13.41649805129999962, 1409.381574823129995, 191.5176180624980020 ) ) ;
#45022 = CARTESIAN_POINT ( 'NONE',  ( -58.33642492515414091, 1379.720901747983589, 262.5133912307817923 ) ) ;
#45024 = CARTESIAN_POINT ( 'NONE',  ( 15.19278567220069931, 1512.351864386150055, 196.1968638649200329 ) ) ;
#45023 = CARTESIAN_POINT ( 'NONE',  ( -24.36523717070000217, 1440.927836225630017, 211.6868765465779916 ) ) ;
#45025 = CARTESIAN_POINT ( 'NONE',  ( 4.647513230146739893, 1424.072963496759940, 193.1398315391210190 ) ) ;
#45026 = CARTESIAN_POINT ( 'NONE',  ( -6.089577322537190085, 1511.778877376279979, 200.6487354888959942 ) ) ;
#45027 = CARTESIAN_POINT ( 'NONE',  ( -12.48454216434870645, 1434.418201845518297, 147.3004665988038084 ) ) ;
#45028 = DIRECTION ( 'NONE',  ( -6.123233995736769734E-17, -1.000000000000000000, -1.124819836996389922E-32 ) ) ;
#45029 = CARTESIAN_POINT ( 'NONE',  ( 13.80546151116429954, 1434.979654507460054, 148.5370226032280243 ) ) ;
#45031 = CARTESIAN_POINT ( 'NONE',  ( 0.1473420581360029846, 1491.995248389390099, 188.1393154328989965 ) ) ;
#45030 = FACE_OUTER_BOUND ( 'NONE', #110421, .T. ) ;
#45033 = CARTESIAN_POINT ( 'NONE',  ( -5.001338666445000136, 1516.911981270829983, 214.9058546054269812 ) ) ;
#45032 =( GEOMETRIC_REPRESENTATION_CONTEXT ( 3 ) GLOBAL_UNCERTAINTY_ASSIGNED_CONTEXT ( ( #8778 ) ) GLOBAL_UNIT_ASSIGNED_CONTEXT ( ( #93807, #67553, #101655 ) ) REPRESENTATION_CONTEXT ( 'NONE', 'WORKASPACE' ) );
#45034 = CARTESIAN_POINT ( 'NONE',  ( -2.485536755124557740, 1523.919943579690425, 242.8055288421958267 ) ) ;
#45035 = CARTESIAN_POINT ( 'NONE',  ( 6.013128406968769823, 1510.874996213040049, 216.6400301521790084 ) ) ;
#45036 = CARTESIAN_POINT ( 'NONE',  ( 28.27930517080000072, 1508.150008669530052, 208.9705538469389978 ) ) ;
#45037 = CARTESIAN_POINT ( 'NONE',  ( -2.477373643995000485, 1516.891731298979948, 212.0030687278169808 ) ) ;
#45038 = CARTESIAN_POINT ( 'NONE',  ( -11.59678483583009978, 1482.606145766309965, 206.4252640944189920 ) ) ;
#45039 = EDGE_CURVE ( 'NONE', #72142, #49931, #90655, .T. ) ;
#45040 = CARTESIAN_POINT ( 'NONE',  ( 30.51921334599647651, 1524.059663615500540, 221.8697286789197278 ) ) ;
#45042 = EDGE_LOOP ( 'NONE', ( #51149, #103951, #8677, #19458 ) ) ;
#45041 = CARTESIAN_POINT ( 'NONE',  ( -98.33257935689999840, 1389.446463678290229, 299.1634636375590048 ) ) ;
#45043 = CARTESIAN_POINT ( 'NONE',  ( -1.270728281904929924, 1414.996443537369942, 226.4582996361970118 ) ) ;
#45044 = CARTESIAN_POINT ( 'NONE',  ( 21.39592531770000150, 1453.782470550929929, 225.7912808434980150 ) ) ;
#45045 = CARTESIAN_POINT ( 'NONE',  ( -18.32069918539999875, 1457.567609363029987, 229.9399091793980006 ) ) ;
#45046 = CARTESIAN_POINT ( 'NONE',  ( -11.81707110430000007, 1430.266231075130008, 147.2485970657980090 ) ) ;
#45047 = CARTESIAN_POINT ( 'NONE',  ( -6.844637409469999767, 1507.263724706429912, 235.7154609632979714 ) ) ;
#45048 = CARTESIAN_POINT ( 'NONE',  ( -18.97274404719999907, 1457.324312373629937, 226.8825690747979991 ) ) ;
#45049 = AXIS2_PLACEMENT_3D ( 'NONE', #97672, #37223, #96580 ) ;
#45051 = CARTESIAN_POINT ( 'NONE',  ( 5.360351092102419557, 1422.243568082540150, 144.1133778792190014 ) ) ;
#45050 = CARTESIAN_POINT ( 'NONE',  ( -21.70628021907349137, 1411.031453783015195, 201.5216881071951605 ) ) ;
#45052 = CARTESIAN_POINT ( 'NONE',  ( 0.1642147860209999810, 1434.814457747790129, 190.0887174017979930 ) ) ;
#45053 = CARTESIAN_POINT ( 'NONE',  ( -104.0132077409040079, 1379.986693862269931, 305.5692602416439740 ) ) ;
#45054 = ORIENTED_EDGE ( 'NONE', *, *, #30684, .F. ) ;
#45055 = CARTESIAN_POINT ( 'NONE',  ( -6.945490086935000029, 1516.932669162149978, 203.3434733684869968 ) ) ;
#45056 = CARTESIAN_POINT ( 'NONE',  ( 0.7780697151959999891, 1405.754330040730110, 267.5369108394980344 ) ) ;
#45057 = CARTESIAN_POINT ( 'NONE',  ( -19.64992912988063267, 1517.051704408389924, 210.5515370059081022 ) ) ;
#45058 = B_SPLINE_CURVE_WITH_KNOTS ( 'NONE', 3,
 ( #107933, #6026, #31773, #31225, #40730, #13854, #48037, #57003, #49151, #72698, #92231 ),
 .UNSPECIFIED., .F., .F.,
 ( 4, 2, 1, 2, 2, 4 ),
 ( 0.000000000000000000, 0.2499999999999520939, 0.3749999999999407696, 0.4375000000000707212, 0.5000000000002006173, 1.000000000000000000 ),
 .UNSPECIFIED. ) ;
#45059 = CARTESIAN_POINT ( 'NONE',  ( 42.00606667534940186, 1451.376206482430007, 270.3372530110870002 ) ) ;
#45060 = CARTESIAN_POINT ( 'NONE',  ( 2.478410607399999854, 1438.230131886350136, 157.7118229332980093 ) ) ;
#45061 = CARTESIAN_POINT ( 'NONE',  ( -40.27780736350000268, 1444.639155820560063, 137.0225327466980048 ) ) ;
#45062 = AXIS2_PLACEMENT_3D ( 'NONE', #62834, #46000, #3451 ) ;
#45063 = CARTESIAN_POINT ( 'NONE',  ( -20.70484064406366187, 1525.907212628473644, 233.2025904124108706 ) ) ;
#45064 = CARTESIAN_POINT ( 'NONE',  ( -26.57078163029999729, 1448.091204785469927, 137.0346892529979925 ) ) ;
#45065 = CARTESIAN_POINT ( 'NONE',  ( 0.5717981366250000086, 1450.893092756410169, 154.2461502948980012 ) ) ;
#45066 = DIRECTION ( 'NONE',  ( 0.9952216675636860188, -0.01326783003108352073, 0.09673570746121909480 ) ) ;
#45067 = CARTESIAN_POINT ( 'NONE',  ( 0.5718102594343560385, 1450.893092333070172, 154.2421351020080067 ) ) ;
#45068 = CARTESIAN_POINT ( 'NONE',  ( -1.351834365089999990, 1508.907723353190022, 220.8330489178990206 ) ) ;
#45069 = CARTESIAN_POINT ( 'NONE',  ( 19.58711162175621823, 1488.292444595022744, 189.9646409983099602 ) ) ;
#45070 = ORIENTED_EDGE ( 'NONE', *, *, #27023, .T. ) ;
#45071 = DIRECTION ( 'NONE',  ( -1.000000000000000000, 0.000000000000000000, 0.000000000000000000 ) ) ;
#45072 = CARTESIAN_POINT ( 'NONE',  ( -1.612803906969698220, 1450.558055974748413, 182.3143092148731341 ) ) ;
#45073 = CARTESIAN_POINT ( 'NONE',  ( 8.227317073306119610, 1467.971793790919946, 202.5226687861409971 ) ) ;
#45074 = B_SPLINE_CURVE_WITH_KNOTS ( 'NONE', 4,
 ( #14557, #91821, #108629, #75603, #83973 ),
 .UNSPECIFIED., .F., .F.,
 ( 5, 5 ),
 ( 8.673617379884035472E-19, 0.009483690916888026790 ),
 .UNSPECIFIED. ) ;
#45075 = CARTESIAN_POINT ( 'NONE',  ( -0.8824136083850000478, 1475.554964337430192, 269.2944284116979929 ) ) ;
#45076 = CARTESIAN_POINT ( 'NONE',  ( 9.573136282580000156, 1493.454997221290114, 189.9048530042990137 ) ) ;
#45077 = CARTESIAN_POINT ( 'NONE',  ( -31.55762699681141115, 1523.390106123591067, 196.3178534513334341 ) ) ;
#45078 = CARTESIAN_POINT ( 'NONE',  ( -3.730224799879785724, 1448.293533855142186, 184.9867838729743994 ) ) ;
#45079 = CARTESIAN_POINT ( 'NONE',  ( -19.79605902738999745, 1384.862938669949926, 220.8639557539960094 ) ) ;
#45080 = CIRCLE ( 'NONE', #59371, 0.9999999999999927836 ) ;
#45081 = CARTESIAN_POINT ( 'NONE',  ( -18.62061618460000290, 1416.021639796329964, 208.3328397087159942 ) ) ;
#45082 = CARTESIAN_POINT ( 'NONE',  ( -10.56986559679999971, 1482.340628544289984, 205.9074541195790005 ) ) ;
#45083 = CARTESIAN_POINT ( 'NONE',  ( 26.61008156381389966, 1435.426649381249945, 135.3751932008159713 ) ) ;
#45084 = CARTESIAN_POINT ( 'NONE',  ( -7.669900437163190254, 1396.180899213449948, 217.0741413368000110 ) ) ;
#45085 = B_SPLINE_CURVE_WITH_KNOTS ( 'NONE', 5,
 ( #98204, #74681, #108814, #39408, #65177, #39957 ),
 .UNSPECIFIED., .F., .F.,
 ( 6, 6 ),
 ( 0.000000000000000000, 1.000000000000000000 ),
 .UNSPECIFIED. ) ;
#45086 = VECTOR ( 'NONE', #25076, 1000.000000000000000 ) ;
#45087 = CARTESIAN_POINT ( 'NONE',  ( -14.94295326230000143, 1421.973613342230010, 227.7489465375979876 ) ) ;
#45088 = CARTESIAN_POINT ( 'NONE',  ( -16.68455712722449746, 1409.595976310660035, 225.3198650213400072 ) ) ;
#45089 = CARTESIAN_POINT ( 'NONE',  ( 4.978523888090000682, 1441.600846913620217, 150.3430135618980046 ) ) ;
#45090 = ORIENTED_EDGE ( 'NONE', *, *, #78622, .F. ) ;
#45091 = CARTESIAN_POINT ( 'NONE',  ( -3.380779445240819747, 1436.568323192200069, 227.3158197219400165 ) ) ;
#45092 = CARTESIAN_POINT ( 'NONE',  ( 1.984536219169999782, 1410.356878570029949, 232.0128186513979927 ) ) ;
#45093 = CARTESIAN_POINT ( 'NONE',  ( -16.69612950000000140, 1484.879939360330127, 188.0702094165980043 ) ) ;
#45095 = CARTESIAN_POINT ( 'NONE',  ( -9.783936650027678539, 1438.409968310599879, 210.7790528106160082 ) ) ;
#45094 = CARTESIAN_POINT ( 'NONE',  ( 10.77722223709999838, 1425.675087937729813, 99.60349438569788560 ) ) ;
#45096 = DIRECTION ( 'NONE',  ( 0.5877852522924685852, 0.000000000000000000, -0.8090169943749507819 ) ) ;
#45097 = B_SPLINE_CURVE_WITH_KNOTS ( 'NONE', 3,
 ( #100581, #75414, #84875, #49656, #101668, #24958, #25515, #26064, #109004, #84340, #59708, #51290, #50213, #68669, #8171, #92191, #83791, #109553, #42340, #32825, #7086, #110644, #59167, #68127, #16550, #67014, #6535, #101122, #24419, #50740, #7628 ),
 .UNSPECIFIED., .F., .F.,
 ( 4, 3, 3, 3, 3, 3, 3, 3, 3, 3, 4 ),
 ( -31.85201398510000104, -31.81690162971739966, -31.29106762226110305, -30.73012125942219797, -29.75465476144709953, -29.12069379509160072, -28.57063748067939812, -28.09167849124629868, -27.34815097616279900, -26.12566447164610040, -25.28925868605369942 ),
 .UNSPECIFIED. ) ;
#45098 = CARTESIAN_POINT ( 'NONE',  ( -12.53380498098199602, 1442.773887284840612, 205.2015002797237173 ) ) ;
#45099 = CARTESIAN_POINT ( 'NONE',  ( -7.329925260535000042, 1516.833976295079992, 201.4049670291269933 ) ) ;
#45100 = CARTESIAN_POINT ( 'NONE',  ( 7.898683012529999381, 1423.849047743189885, 212.3277966039590012 ) ) ;
#45101 = CARTESIAN_POINT ( 'NONE',  ( -19.58884347349999899, 1465.811382978989968, 204.1485388398990040 ) ) ;
#45102 = DIRECTION ( 'NONE',  ( 0.000000000000000000, -1.736889445713099699E-16, -1.000000000000000000 ) ) ;
#45103 = CARTESIAN_POINT ( 'NONE',  ( -31.23437356469455040, 1512.187213306747481, 195.3468678195118287 ) ) ;
#45104 = CARTESIAN_POINT ( 'NONE',  ( -105.6573924705229928, 1379.461035556120123, 305.1680620773340138 ) ) ;
#45105 = CARTESIAN_POINT ( 'NONE',  ( 7.954477662311944641, 1365.031352125213971, 209.6218459617148824 ) ) ;
#45107 = ORIENTED_EDGE ( 'NONE', *, *, #62600, .F. ) ;
#45106 = CARTESIAN_POINT ( 'NONE',  ( 7.122515158009999681, 1452.871264857790266, 215.2372064891289654 ) ) ;
#45108 = ORIENTED_EDGE ( 'NONE', *, *, #38900, .F. ) ;
#45109 = DIRECTION ( 'NONE',  ( 0.000000000000000000, 1.000000000000000000, 0.000000000000000000 ) ) ;
#45110 = DIRECTION ( 'NONE',  ( -1.000000000000000000, 0.000000000000000000, 0.000000000000000000 ) ) ;
#45111 = CARTESIAN_POINT ( 'NONE',  ( -13.80541478530910027, 1434.979604282769969, 148.5370187744020143 ) ) ;
#45112 = CARTESIAN_POINT ( 'NONE',  ( -7.550503362055001055, 1510.480349266450048, 214.6730346442070072 ) ) ;
#45113 = CARTESIAN_POINT ( 'NONE',  ( -1.188215600249533876, 1410.329429340306433, 185.4357503969870891 ) ) ;
#45114 = CARTESIAN_POINT ( 'NONE',  ( -31.54872587855235722, 1525.317359687841190, 201.5741514857012930 ) ) ;
#45115 = CARTESIAN_POINT ( 'NONE',  ( -2.054137843158699628, 1464.087208514039958, 199.3848561270889945 ) ) ;
#45116 = CYLINDRICAL_SURFACE ( 'NONE', #69868, 1.999999999999995337 ) ;
#45117 = CARTESIAN_POINT ( 'NONE',  ( -2.500000000000000000, 1448.385612528629963, 162.4910655934610020 ) ) ;
#45118 = CARTESIAN_POINT ( 'NONE',  ( 33.91369110979999846, 1435.681798629080049, 135.0664268281979901 ) ) ;
#45119 = CARTESIAN_POINT ( 'NONE',  ( 13.57063579770000139, 1407.765491483530013, 211.9101277129380207 ) ) ;
#45120 = CARTESIAN_POINT ( 'NONE',  ( -6.094615587868089435, 1406.362613768930032, 269.0310553213910225 ) ) ;
#45121 = CARTESIAN_POINT ( 'NONE',  ( -11.87328627558470018, 1482.014094172719979, 208.6022272904490080 ) ) ;
#45122 = ORIENTED_EDGE ( 'NONE', *, *, #63318, .T. ) ;
#45123 = CARTESIAN_POINT ( 'NONE',  ( -11.76924708169999967, 1432.318127236120063, 150.8119212263979989 ) ) ;
#45124 = CARTESIAN_POINT ( 'NONE',  ( 12.38749917709999870, 1442.753158610539913, 186.6620494205980094 ) ) ;
#45125 = EDGE_LOOP ( 'NONE', ( #102649, #25647, #94629, #49030 ) ) ;
#45126 = EDGE_LOOP ( 'NONE', ( #50362, #73629 ) ) ;
#45127 = CARTESIAN_POINT ( 'NONE',  ( 15.69795926444620271, 1522.051704408389924, 222.7678737639049871 ) ) ;
#45128 = CARTESIAN_POINT ( 'NONE',  ( -9.690020260109999839, 1366.026910387849966, 207.6218459616989946 ) ) ;
#45129 = CARTESIAN_POINT ( 'NONE',  ( -6.939219520934999608, 1516.783701990830195, 214.9027072062869763 ) ) ;
#45130 = CARTESIAN_POINT ( 'NONE',  ( 1.491506560153233130, 1512.187213306747481, 175.5704429466618421 ) ) ;
#45131 = VERTEX_POINT ( 'NONE', #27062 ) ;
#45132 = CARTESIAN_POINT ( 'NONE',  ( 4.966881216750000050, 1424.596682289360160, 209.0258764897109813 ) ) ;
#45133 = CARTESIAN_POINT ( 'NONE',  ( -68.69226509189999774, 1374.746858117589909, 280.5557816734590233 ) ) ;
#45134 = ADVANCED_FACE ( 'NONE', ( #61248 ), #16662, .F. ) ;
#45135 = CARTESIAN_POINT ( 'NONE',  ( 11.45335004989999916, 1414.913060387329779, 222.0967534668980079 ) ) ;
#45136 = CARTESIAN_POINT ( 'NONE',  ( 1.121383591734999907, 1517.104192383289956, 204.4960559556369901 ) ) ;
#45137 = VECTOR ( 'NONE', #110170, 1000.000000000000000 ) ;
#45138 = ADVANCED_FACE ( 'NONE', ( #100166 ), #82264, .T. ) ;
#45139 = CARTESIAN_POINT ( 'NONE',  ( -41.27401914175700881, 1435.068058891863529, 269.6337388993341051 ) ) ;
#45140 = CARTESIAN_POINT ( 'NONE',  ( 9.565724157538609163, 1462.394397289459903, 207.2652911505539919 ) ) ;
#45141 = CARTESIAN_POINT ( 'NONE',  ( -3.714969551469999853, 1409.978796437530036, 232.2880016815979900 ) ) ;
#45143 = ORIENTED_EDGE ( 'NONE', *, *, #2344, .F. ) ;
#45142 = CARTESIAN_POINT ( 'NONE',  ( -12.53380499169999851, 1445.052233488290085, 185.6742736857979992 ) ) ;
#45144 = CARTESIAN_POINT ( 'NONE',  ( -4.363122561674769528, 1421.971318449149976, 184.5104913919989826 ) ) ;
#45145 = CARTESIAN_POINT ( 'NONE',  ( 23.59335433618681677, 1519.551704408389924, 208.3625261894497385 ) ) ;
#45146 = CARTESIAN_POINT ( 'NONE',  ( -5.958828918610000080, 1384.900097640590047, 218.5255276338789940 ) ) ;
#45147 = CARTESIAN_POINT ( 'NONE',  ( 22.08622291482331335, 1518.913060387330006, 184.4183880513174927 ) ) ;
#45148 = CARTESIAN_POINT ( 'NONE',  ( -25.36428637739999914, 1436.617909526469930, 137.3808187117979855 ) ) ;
#45149 = CARTESIAN_POINT ( 'NONE',  ( 43.06395268920530128, 1431.911435351959881, 270.2257575559060001 ) ) ;
#45150 = CARTESIAN_POINT ( 'NONE',  ( -4.996642198295000448, 1516.697242742309982, 211.9989590406970024 ) ) ;
#45151 = CIRCLE ( 'NONE', #77345, 8.102416131500007168 ) ;
#45152 = CARTESIAN_POINT ( 'NONE',  ( -67.42914565080000955, 1379.745493734729962, 277.3807740811590179 ) ) ;
#45153 = CARTESIAN_POINT ( 'NONE',  ( 0.01445514656653382191, 1507.861152181168563, 237.5326258831030657 ) ) ;
#45154 = CARTESIAN_POINT ( 'NONE',  ( 5.811960035336429797, 1424.824675250879864, 192.0933432259219842 ) ) ;
#45155 = CARTESIAN_POINT ( 'NONE',  ( 22.35774114936210566, 1411.052082638657112, 204.9822757281434349 ) ) ;
#45156 = SHAPE_REPRESENTATION ( 'Handle Grip', ( #21632 ), #71657 ) ;
#45157 = CARTESIAN_POINT ( 'NONE',  ( -5.006259886824999228, 1516.939723362869927, 209.1347437590049765 ) ) ;
#45158 = ORIENTED_EDGE ( 'NONE', *, *, #80934, .F. ) ;
#45159 = CARTESIAN_POINT ( 'NONE',  ( -4.150225335050000020, 1415.373311228230023, 232.3889413475980064 ) ) ;
#45160 = CARTESIAN_POINT ( 'NONE',  ( -27.62871390899999824, 1385.108881161949967, 225.6286099116589980 ) ) ;
#45161 = VERTEX_POINT ( 'NONE', #48685 ) ;
#45162 = CARTESIAN_POINT ( 'NONE',  ( -19.80402451206670023, 1385.277035965169944, 220.8433670724960223 ) ) ;
#45163 = CARTESIAN_POINT ( 'NONE',  ( -2.810337449649999986, 1429.891394031290019, 201.1534787522990086 ) ) ;
#45164 = CARTESIAN_POINT ( 'NONE',  ( 17.43470154943939932, 1478.709718884490030, 229.3935422930289860 ) ) ;
#45165 = CARTESIAN_POINT ( 'NONE',  ( -23.81112428631299593, 1508.486698750989945, 222.8584575549710109 ) ) ;
#45166 = MANIFOLD_SOLID_BREP ( 'Stock-MAS-682-1', #53918 ) ;
#45167 = CARTESIAN_POINT ( 'NONE',  ( -114.2539859765994237, 1375.913060387289988, 304.7421419804722404 ) ) ;
#45168 = CARTESIAN_POINT ( 'NONE',  ( 4.987078413254999454, 1508.551704408389924, 213.0804953801570036 ) ) ;
#45169 = CARTESIAN_POINT ( 'NONE',  ( -0.1344824551021089887, 1420.462349845229937, 182.7339235605570025 ) ) ;
#45171 = CARTESIAN_POINT ( 'NONE',  ( 16.25496458785010034, 1501.813617903470004, 193.7110474371100111 ) ) ;
#45170 = CARTESIAN_POINT ( 'NONE',  ( -3.258474617075000079, 1517.083030555940013, 215.6838419306269827 ) ) ;
#45172 = CARTESIAN_POINT ( 'NONE',  ( 18.93308395989999937, 1509.362410549930246, 187.5217593452979941 ) ) ;
#45173 = CARTESIAN_POINT ( 'NONE',  ( 11.16829484163620023, 1470.316420363600173, 207.0405923250029900 ) ) ;
#45174 = VERTEX_POINT ( 'NONE', #21043 ) ;
#45175 = CARTESIAN_POINT ( 'NONE',  ( -12.33030208333440036, 1415.427621830080170, 196.6186630558540003 ) ) ;
#45176 = CARTESIAN_POINT ( 'NONE',  ( -11.71447269829999982, 1499.713794938330011, 182.8078852171979918 ) ) ;
#45177 = ORIENTED_EDGE ( 'NONE', *, *, #109197, .T. ) ;
#45178 = CYLINDRICAL_SURFACE ( 'NONE', #44617, 2.000000000000003553 ) ;
#45179 = CARTESIAN_POINT ( 'NONE',  ( 1.546867617820790075, 1416.839692126689897, 190.2222510973109877 ) ) ;
#45180 = CARTESIAN_POINT ( 'NONE',  ( 7.601092399332859628, 1510.855104182140167, 203.4698203236769984 ) ) ;
#45181 = CARTESIAN_POINT ( 'NONE',  ( 2.774825831029999801, 1441.953158150089848, 217.9119417670190160 ) ) ;
#45182 = CARTESIAN_POINT ( 'NONE',  ( -32.40058737600818972, 1524.130440953581001, 201.3079925683071281 ) ) ;
#45183 = DIRECTION ( 'NONE',  ( 0.000000000000000000, 1.000000000000000000, 0.000000000000000000 ) ) ;
#45184 = CARTESIAN_POINT ( 'NONE',  ( 17.60960321790000194, 1415.041103191630100, 210.5185711766079919 ) ) ;
#45185 = CARTESIAN_POINT ( 'NONE',  ( -17.84085719520000168, 1424.376552934430038, 226.3470615041979670 ) ) ;
#45186 = CARTESIAN_POINT ( 'NONE',  ( -22.37341732390000004, 1435.279001492649968, 139.8076879873979976 ) ) ;
#45187 = CARTESIAN_POINT ( 'NONE',  ( -3.363422329630640029, 1464.767212871569882, 198.6335063457190131 ) ) ;
#45188 = CARTESIAN_POINT ( 'NONE',  ( 17.67008274869999696, 1428.766651565430038, 191.5438197617980052 ) ) ;
#45190 = CARTESIAN_POINT ( 'NONE',  ( 0.5931383417482081200, 1491.015063307030005, 187.2060224152310184 ) ) ;
#45189 = CARTESIAN_POINT ( 'NONE',  ( 18.69816095120750532, 1522.382868172863937, 183.3860352823955679 ) ) ;
#45191 = CARTESIAN_POINT ( 'NONE',  ( 0.000000000000000000, 1523.409940573003951, 209.1218459616979999 ) ) ;
#45192 = ORIENTED_EDGE ( 'NONE', *, *, #8680, .T. ) ;
#45193 = CARTESIAN_POINT ( 'NONE',  ( 1.556574321196450006, 1415.089996090870045, 191.4482120491740034 ) ) ;
#45194 = CARTESIAN_POINT ( 'NONE',  ( 26.03031014660000153, 1488.581978119829955, 206.4905525074180161 ) ) ;
#45195 = CARTESIAN_POINT ( 'NONE',  ( -24.08776747539999974, 1437.704999045569821, 212.2548087022379661 ) ) ;
#45196 = CARTESIAN_POINT ( 'NONE',  ( -4.114244456749999834, 1483.278371519489838, 199.2835753141889938 ) ) ;
#45197 = CARTESIAN_POINT ( 'NONE',  ( -18.60392326990000100, 1508.243836138129836, 229.7334999568980152 ) ) ;
#45198 = CARTESIAN_POINT ( 'NONE',  ( -2.599451791485461349, 1525.231887713385959, 241.5259292574780545 ) ) ;
#45199 = CARTESIAN_POINT ( 'NONE',  ( 20.65321958619999876, 1453.313060387329870, 210.0984853413359872 ) ) ;
#45200 = CARTESIAN_POINT ( 'NONE',  ( 28.54794148642324103, 1526.382868172864164, 219.8054320332928171 ) ) ;
#45201 = CARTESIAN_POINT ( 'NONE',  ( -11.04302901312609997, 1470.202560320620023, 211.8432240382399812 ) ) ;
#45202 = CARTESIAN_POINT ( 'NONE',  ( -10.72577289612640072, 1489.848996007629921, 212.9502564920910004 ) ) ;
#45203 = CARTESIAN_POINT ( 'NONE',  ( -11.77905477449999871, 1483.168199375790209, 228.2502073304989949 ) ) ;
#45204 = CARTESIAN_POINT ( 'NONE',  ( -78.94690149131609758, 1383.777751329849934, 302.9268705869330347 ) ) ;
#45205 = EDGE_CURVE ( 'NONE', #45774, #24662, #39143, .T. ) ;
#45206 = EDGE_CURVE ( 'NONE', #35617, #28394, #104666, .T. ) ;
#45207 = DIRECTION ( 'NONE',  ( 1.836970198721029688E-16, 1.000000000000000000, 0.000000000000000000 ) ) ;
#45208 = CARTESIAN_POINT ( 'NONE',  ( 5.551188674472009588, 1510.480349264700180, 216.6723492941099778 ) ) ;
#45209 = CARTESIAN_POINT ( 'NONE',  ( 15.05358515032119904, 1410.831827804430077, 191.5175411757069810 ) ) ;
#45211 = ORIENTED_EDGE ( 'NONE', *, *, #18478, .T. ) ;
#45210 = CARTESIAN_POINT ( 'NONE',  ( 21.39772588749999827, 1509.704957013630064, 188.4542805408979973 ) ) ;
#45212 = CARTESIAN_POINT ( 'NONE',  ( -18.47236838445734719, 1458.829591624305749, 227.6520860182954777 ) ) ;
#45213 = CARTESIAN_POINT ( 'NONE',  ( -67.18675499840000498, 1383.787653363379832, 292.0788269227589922 ) ) ;
#45214 = EDGE_CURVE ( 'NONE', #79230, #12203, #48124, .T. ) ;
#45215 = CARTESIAN_POINT ( 'NONE',  ( 20.28959732197790089, 1509.463221166710127, 230.1365879813909885 ) ) ;
#45216 = VERTEX_POINT ( 'NONE', #106180 ) ;
#45217 = ORIENTED_EDGE ( 'NONE', *, *, #13448, .T. ) ;
#45218 = EDGE_CURVE ( 'NONE', #55731, #72815, #107830, .T. ) ;
#45219 = CARTESIAN_POINT ( 'NONE',  ( -20.64559663309999848, 1487.101925495689784, 207.0915929621590124 ) ) ;
#45220 = CARTESIAN_POINT ( 'NONE',  ( 22.69876404240077505, 1501.977400791986611, 181.3483716558180276 ) ) ;
#45221 = CARTESIAN_POINT ( 'NONE',  ( 12.54031924683600430, 1442.774810235321866, 169.4746789495621897 ) ) ;
#45223 = CARTESIAN_POINT ( 'NONE',  ( 4.206714493999999137E-09, 1470.400760097329794, 255.2684105280980020 ) ) ;
#45222 = CARTESIAN_POINT ( 'NONE',  ( 21.20812184460000083, 1488.814055420830073, 208.7429176965079876 ) ) ;
#45224 = CARTESIAN_POINT ( 'NONE',  ( 8.725481330957579829, 1436.236045380599990, 208.5030100741789738 ) ) ;
#45225 = CARTESIAN_POINT ( 'NONE',  ( -11.94180911519999988, 1433.516160569599833, 150.0911335117980059 ) ) ;
#45226 = CARTESIAN_POINT ( 'NONE',  ( 24.04911891789999956, 1508.500175175629920, 195.9134722914980102 ) ) ;
#45227 = CARTESIAN_POINT ( 'NONE',  ( 4.363122647530000009, 1421.971318475729959, 178.0486554715980105 ) ) ;
#45228 = CARTESIAN_POINT ( 'NONE',  ( 15.20279577643499991, 1515.867682058960099, 225.0317485278669949 ) ) ;
#45229 = DIRECTION ( 'NONE',  ( 0.9858563016923833633, 0.000000000000000000, 0.1675928173085483863 ) ) ;
#45230 = CARTESIAN_POINT ( 'NONE',  ( -9.012265790579998992, 1437.710537571299938, 153.1651550408980142 ) ) ;
#45231 = DIRECTION ( 'NONE',  ( -0.000000000000000000, 1.000000000000000000, 0.000000000000000000 ) ) ;
#45232 = CARTESIAN_POINT ( 'NONE',  ( -16.20918397789189669, 1420.752430442280001, 203.3157397894999860 ) ) ;
#45233 = CARTESIAN_POINT ( 'NONE',  ( -11.40503443455700072, 1490.739836633030109, 209.6941760169060274 ) ) ;
#45234 = CARTESIAN_POINT ( 'NONE',  ( 4.551482758439999721, 1472.189735705889916, 218.2242021444390048 ) ) ;
#45235 = ORIENTED_EDGE ( 'NONE', *, *, #53238, .F. ) ;
#45236 = CARTESIAN_POINT ( 'NONE',  ( -2.713960167710639967E-10, 1417.262443616730025, 235.9145977375980010 ) ) ;
#45237 = B_SPLINE_CURVE_WITH_KNOTS ( 'NONE', 3,
 ( #92705, #6503, #5958, #66439, #91611, #7602, #40657, #41756, #75915, #40103, #57486, #53494, #87639 ),
 .UNSPECIFIED., .F., .F.,
 ( 4, 2, 2, 1, 2, 2, 4 ),
 ( 0.000000000000000000, 0.2499999999999987232, 0.4999999999999974465, 0.6250000000000086597, 0.6875000000000129896, 0.7500000000000173195, 1.000000000000000000 ),
 .UNSPECIFIED. ) ;
#45238 = CARTESIAN_POINT ( 'NONE',  ( -17.55007421918869781, 1487.029478167789875, 194.9701128493070144 ) ) ;
#45240 = EDGE_CURVE ( 'NONE', #85608, #38935, #13745, .T. ) ;
#45239 = CARTESIAN_POINT ( 'NONE',  ( -34.89169900679999614, 1462.401046348830278, 269.8669090264980355 ) ) ;
#45241 = FACE_OUTER_BOUND ( 'NONE', #21405, .T. ) ;
#45242 = CARTESIAN_POINT ( 'NONE',  ( 6.550315845290000521E-15, 1440.444625599219989, 155.6821044880979912 ) ) ;
#45243 = CARTESIAN_POINT ( 'NONE',  ( -4.623067421070000016, 1470.601194648889987, 189.6761541078989808 ) ) ;
#45244 = CARTESIAN_POINT ( 'NONE',  ( 0.9786431567949999133, 1497.713060387329961, 186.5280767325980094 ) ) ;
#45245 = CARTESIAN_POINT ( 'NONE',  ( 2.823995551231429868, 1409.082596969919905, 230.6442242877770070 ) ) ;
#45246 = CARTESIAN_POINT ( 'NONE',  ( 1.164704066880000166, 1507.351178548329926, 237.0483094473980259 ) ) ;
#45247 = CARTESIAN_POINT ( 'NONE',  ( -11.35628460690000097, 1419.578172898530056, 229.5089160734980283 ) ) ;
#45248 = ADVANCED_FACE ( 'NONE', ( #38955 ), #30007, .F. ) ;
#45249 = CARTESIAN_POINT ( 'NONE',  ( -9.336750167439999970, 1459.654649201290113, 211.6846149272190303 ) ) ;
#45250 = CARTESIAN_POINT ( 'NONE',  ( 7.773062682075623897, 1360.933485754074582, 207.6218459616987673 ) ) ;
#45251 = CARTESIAN_POINT ( 'NONE',  ( -44.26911428083240452, 1430.613050725120047, 267.6606138304829869 ) ) ;
#45253 = CARTESIAN_POINT ( 'NONE',  ( -0.4151546846821903003, 1512.187213306747481, 244.9330574173806951 ) ) ;
#45252 = B_SPLINE_CURVE_WITH_KNOTS ( 'NONE', 3,
 ( #10770, #18579, #44379, #72341, #95864, #105378, #20791, #46039, #28107, #20247, #88584, #54992, #54448, #78522, #53333, #80168, #46589, #106470, #29755, #79088, #2396, #104820, #57612, #23954, #15003 ),
 .UNSPECIFIED., .F., .F.,
 ( 4, 3, 3, 3, 3, 3, 3, 3, 4 ),
 ( -7.627880006969999904, -7.586449332979929849, -6.861103662591740537, -6.094327318213479394, -5.380600910333019904, -5.288135639796470500, -4.615464934644060158, -3.827473140728220091, -3.133321433589999927 ),
 .UNSPECIFIED. ) ;
#45254 = ORIENTED_EDGE ( 'NONE', *, *, #51620, .F. ) ;
#45255 = CARTESIAN_POINT ( 'NONE',  ( -8.440966142320000642, 1423.593311052290119, 209.8619391807339980 ) ) ;
#45256 = EDGE_CURVE ( 'NONE', #18256, #80453, #31118, .T. ) ;
#45257 = VERTEX_POINT ( 'NONE', #90469 ) ;
#45258 = CARTESIAN_POINT ( 'NONE',  ( 7.337297311985000015, 1517.135701590510052, 209.8615382079770200 ) ) ;
#45259 = CARTESIAN_POINT ( 'NONE',  ( 7.589792638401371860, 1507.508085020990166, 200.2016081335497972 ) ) ;
#45260 = CARTESIAN_POINT ( 'NONE',  ( 16.19492570339999915, 1409.478599654730033, 224.8086529783979870 ) ) ;
#45261 = CARTESIAN_POINT ( 'NONE',  ( -7.311252174589999875, 1425.409830198830150, 186.8070320980980057 ) ) ;
#45262 = ORIENTED_EDGE ( 'NONE', *, *, #6835, .F. ) ;
#45264 = CARTESIAN_POINT ( 'NONE',  ( 13.15607067970000088, 1416.813004075630033, 196.3352670360980312 ) ) ;
#45263 = DIRECTION ( 'NONE',  ( -1.755985294532469921E-16, 1.000000000000000000, -1.338183447452831989E-16 ) ) ;
#45265 = CARTESIAN_POINT ( 'NONE',  ( 11.60004869885203682, 1425.327753716559073, 136.8073925826587356 ) ) ;
#45266 = CARTESIAN_POINT ( 'NONE',  ( -18.08355418696270078, 1508.551704408389924, 210.9733555596099848 ) ) ;
#45267 = ADVANCED_FACE ( 'NONE', ( #73134 ), #92099, .T. ) ;
#45268 = CARTESIAN_POINT ( 'NONE',  ( 8.068531700010000307, 1471.978696959290119, 215.6387874036589949 ) ) ;
#45269 = CARTESIAN_POINT ( 'NONE',  ( 4.962911793259999982, 1424.817228554909889, 209.2445736825380038 ) ) ;
#45270 = ORIENTED_EDGE ( 'NONE', *, *, #46868, .T. ) ;
#45271 = CARTESIAN_POINT ( 'NONE',  ( -9.540560617780160513, 1410.806727061010179, 269.8726498066840236 ) ) ;
#45272 = CARTESIAN_POINT ( 'NONE',  ( 4.610079833424999940, 1516.713079096360161, 207.9883289669969884 ) ) ;
#45273 = CARTESIAN_POINT ( 'NONE',  ( -0.8041763403130000043, 1426.566393376330097, 144.1938086916980239 ) ) ;
#45274 = CARTESIAN_POINT ( 'NONE',  ( 9.769960542006101534, 1435.154130655169865, 208.2355606574099909 ) ) ;
#45276 = ORIENTED_EDGE ( 'NONE', *, *, #15968, .F. ) ;
#45275 = CARTESIAN_POINT ( 'NONE',  ( -7.450033292399999674, 1367.931913175460068, 207.6218459616989946 ) ) ;
#45277 = ORIENTED_EDGE ( 'NONE', *, *, #20160, .F. ) ;
#45278 = CARTESIAN_POINT ( 'NONE',  ( 33.30246916720928851, 1464.284855331462268, 269.2880880758933699 ) ) ;
#45279 = CARTESIAN_POINT ( 'NONE',  ( 0.4200850585664279713, 1467.359727432810132, 220.1963459426220027 ) ) ;
#45280 = CARTESIAN_POINT ( 'NONE',  ( 3.627035553931058143, 1424.689726282432957, 184.6936925814563040 ) ) ;
#45281 = CARTESIAN_POINT ( 'NONE',  ( -0.5779273184081722414, 1522.051704408389924, 186.0802614738061607 ) ) ;
#45282 = CARTESIAN_POINT ( 'NONE',  ( -17.80515869325809675, 1415.152886231989896, 207.5654953169710097 ) ) ;
#45283 = CARTESIAN_POINT ( 'NONE',  ( -19.30882480040000004, 1420.833581750830035, 223.3059896308980115 ) ) ;
#45284 = CARTESIAN_POINT ( 'NONE',  ( -34.18677586421173231, 1522.382868172863937, 219.7932833225216882 ) ) ;
#45285 = CARTESIAN_POINT ( 'NONE',  ( -11.67285302236730082, 1391.913060387249971, 209.1401477369450106 ) ) ;
#45286 = CARTESIAN_POINT ( 'NONE',  ( -17.36858564312840869, 1422.635098520762767, 226.5745447126183763 ) ) ;
#45287 = CARTESIAN_POINT ( 'NONE',  ( 5.770883563884999568, 1516.603620185149794, 206.8276363026970159 ) ) ;
#45288 = ORIENTED_EDGE ( 'NONE', *, *, #34733, .F. ) ;
#45289 = CARTESIAN_POINT ( 'NONE',  ( 19.44016575157431603, 1410.953682894560870, 220.9327019326229333 ) ) ;
#45290 = CARTESIAN_POINT ( 'NONE',  ( 1.472587025414080042, 1484.115384728570234, 182.1162732876320263 ) ) ;
#45291 = ORIENTED_EDGE ( 'NONE', *, *, #30216, .T. ) ;
#45293 = B_SPLINE_CURVE_WITH_KNOTS ( 'NONE', 3,
 ( #105891, #29172, #63361, #91684, #52463, #101167, #60304, #67609, #92784, #16059, #86593, #17143, #78192, #9885, #101719, #94424, #35086, #102282, #32871, #58650, #76537, #9342 ),
 .UNSPECIFIED., .F., .F.,
 ( 4, 3, 3, 3, 3, 3, 3, 4 ),
 ( 10.04884080650000122, 10.05925814240000093, 10.16601929647930014, 10.29502131698899881, 10.44078577034700039, 10.52123097808229879, 10.70418225783430088, 10.99321056540000008 ),
 .UNSPECIFIED. ) ;
#45292 = CARTESIAN_POINT ( 'NONE',  ( 4.246466822330620339, 1508.879013277289914, 205.3739042749660086 ) ) ;
#45294 = CARTESIAN_POINT ( 'NONE',  ( 25.98086901942570037, 1451.279931479090010, 136.5097477484009971 ) ) ;
#45295 = CYLINDRICAL_SURFACE ( 'NONE', #97287, 2.000000000000003997 ) ;
#45296 = CARTESIAN_POINT ( 'NONE',  ( -37.19866254769999614, 1386.636863995749991, 210.1929157112890039 ) ) ;
#45297 = CARTESIAN_POINT ( 'NONE',  ( 7.326141149145000142, 1517.051704409989952, 213.3996074426069924 ) ) ;
#45298 = CARTESIAN_POINT ( 'NONE',  ( 16.65035232609999838, 1409.494503502829957, 193.9825473880979985 ) ) ;
#45299 = CARTESIAN_POINT ( 'NONE',  ( 20.17294526779999941, 1444.994950788469851, 161.5349527656980229 ) ) ;
#45300 = FACE_OUTER_BOUND ( 'NONE', #4108, .T. ) ;
#45302 = CARTESIAN_POINT ( 'NONE',  ( -22.83227036410434252, 1432.448231568467236, 215.4813152793481095 ) ) ;
#45301 = CARTESIAN_POINT ( 'NONE',  ( 0.1391290138140000021, 1415.759273717029828, 233.4531323245979877 ) ) ;
#45303 = B_SPLINE_CURVE_WITH_KNOTS ( 'NONE', 3,
 ( #74155, #38863, #4719, #29365, #47284, #20405 ),
 .UNSPECIFIED., .F., .F.,
 ( 4, 2, 4 ),
 ( 0.000000000000000000, 0.5000000000000000000, 1.000000000000000000 ),
 .UNSPECIFIED. ) ;
#45304 = CARTESIAN_POINT ( 'NONE',  ( 0.3611859533326580163, 1452.655354317530055, 183.2864753396520143 ) ) ;
#45305 = ADVANCED_FACE ( 'NONE', ( #2678 ), #45450, .T. ) ;
#45306 = CARTESIAN_POINT ( 'NONE',  ( -8.700971975899999933, 1381.863705729429967, 218.0542239465389969 ) ) ;
#45307 = EDGE_CURVE ( 'NONE', #9799, #102747, #60629, .T. ) ;
#45308 = CARTESIAN_POINT ( 'NONE',  ( 5.781490544344999982, 1516.807958722750072, 215.6734893570070142 ) ) ;
#45309 = DIRECTION ( 'NONE',  ( -0.6736849260863839728, 0.000000000000000000, 0.7390186874254150995 ) ) ;
#45310 = VERTEX_POINT ( 'NONE', #77028 ) ;
#45311 = CARTESIAN_POINT ( 'NONE',  ( 11.73700276120000119, 1426.696009609230032, 144.1682878315979792 ) ) ;
#45312 = B_SPLINE_SURFACE_WITH_KNOTS ( 'NONE', 5, 5, ( 
 ( #103347, #68145, #9314, #101139, #42922, #24433 ),
 ( #68684, #59184, #59724, #17116, #94395, #102255 ),
 ( #92752, #16030, #60848, #25534, #76508, #50759 ),
 ( #18241, #110658, #50229, #51304, #7647, #93303 ),
 ( #387, #75961, #33385, #8739, #33951, #67581 ),
 ( #77079, #86014, #77621, #85441, #71472, #10410 ) ),
 .UNSPECIFIED., .F., .F., .F.,
 ( 6, 6 ),
 ( 6, 6 ),
 ( 30.60719516609999857, 168.0115522031930197 ),
 ( -0.001304583034726280013, 2.000849590660000121 ),
 .UNSPECIFIED. ) ;
#45313 = CARTESIAN_POINT ( 'NONE',  ( -0.2682795917991919743, 1457.891717849350016, 229.2666142623699841 ) ) ;
#45314 = CARTESIAN_POINT ( 'NONE',  ( -8.473114352260500581, 1484.074700721370164, 200.7533846890079872 ) ) ;
#45315 = CARTESIAN_POINT ( 'NONE',  ( 8561.628222780833312, 50.13405481578727318, 11261.64903810669421 ) ) ;
#45316 = CARTESIAN_POINT ( 'NONE',  ( -37.84132625714809706, 1448.955271367279920, 136.3629971985199916 ) ) ;
#45317 = CARTESIAN_POINT ( 'NONE',  ( -4.327096512618029855, 1515.154622198479956, 208.8658927233350084 ) ) ;
#45318 = CARTESIAN_POINT ( 'NONE',  ( -25.65427091389999958, 1447.057116126660048, 243.9198229428980085 ) ) ;
#45319 = EDGE_CURVE ( 'NONE', #101369, #107891, #24480, .T. ) ;
#45320 = CARTESIAN_POINT ( 'NONE',  ( 0.1681681984989999989, 1413.717199569329750, 164.8680577770979880 ) ) ;
#45321 = CARTESIAN_POINT ( 'NONE',  ( 11.79467674799999877, 1433.007546473260163, 150.6262850383980094 ) ) ;
#45322 = CARTESIAN_POINT ( 'NONE',  ( -38.67644254896129752, 1458.284314194199851, 269.8062628433829673 ) ) ;
#45323 = CARTESIAN_POINT ( 'NONE',  ( 27.58375870893669912, 1440.913060388060103, 229.4262493117180099 ) ) ;
#45324 = DIRECTION ( 'NONE',  ( 1.000000000000000000, 1.810374147724000060E-32, 1.224646799147351975E-16 ) ) ;
#45325 = CARTESIAN_POINT ( 'NONE',  ( 14.32856980210140030, 1427.588994036270151, 195.3328737750769903 ) ) ;
#45326 = EDGE_LOOP ( 'NONE', ( #24125, #107093, #73791, #40978 ) ) ;
#45327 = DIRECTION ( 'NONE',  ( -0.7414773880254760252, -0.000000000000000000, -0.6709778558543624261 ) ) ;
#45328 = CARTESIAN_POINT ( 'NONE',  ( 15.23086226699999912, 1495.985335716230111, 224.7399028826979759 ) ) ;
#45329 = CARTESIAN_POINT ( 'NONE',  ( -5.873126364289999124, 1486.384359668930074, 182.2278923802979875 ) ) ;
#45330 = CARTESIAN_POINT ( 'NONE',  ( -1.338895077072838058, 1526.382868172864164, 239.5739613961735586 ) ) ;
#45331 = CARTESIAN_POINT ( 'NONE',  ( 12.12948552422830062, 1501.448489250790089, 211.6227393280869933 ) ) ;
#45332 = EDGE_CURVE ( 'NONE', #42621, #6947, #10554, .T. ) ;
#45333 = CARTESIAN_POINT ( 'NONE',  ( 24.41209542509999864, 1449.795792320089959, 214.5721300427080109 ) ) ;
#45334 = CARTESIAN_POINT ( 'NONE',  ( -15.64806741621447017, 1420.335678436578291, 210.4039352086240626 ) ) ;
#45335 = DIRECTION ( 'NONE',  ( -0.1831271638493041642, -0.06610684103802308420, -0.9808640718409884496 ) ) ;
#45336 = CARTESIAN_POINT ( 'NONE',  ( -29.80992411920399832, 1383.842315663000136, 227.6115284750150067 ) ) ;
#45337 = EDGE_CURVE ( 'NONE', #71158, #107758, #67374, .T. ) ;
#45338 = SPHERICAL_SURFACE ( 'NONE', #42063, 1.999998248449999849 ) ;
#45339 = CARTESIAN_POINT ( 'NONE',  ( 1.704989397879402180, 1417.527060573706422, 233.7744594592636815 ) ) ;
#45340 = CARTESIAN_POINT ( 'NONE',  ( -1766.069695707609526, -8382.262153571264207, -1964.859607327509593 ) ) ;
#45341 = CARTESIAN_POINT ( 'NONE',  ( 9.155703581353909826, 1451.066167471900144, 210.4353983151760019 ) ) ;
#45342 = ADVANCED_FACE ( 'NONE', ( #55150 ), #104011, .F. ) ;
#45344 = ORIENTED_EDGE ( 'NONE', *, *, #14146, .T. ) ;
#45343 = CARTESIAN_POINT ( 'NONE',  ( 3.212280145430000289, 1441.426961928390028, 218.1016817799990122 ) ) ;
#45345 = CARTESIAN_POINT ( 'NONE',  ( -12.29654148988069373, 1445.052233488290085, 164.4841150006940325 ) ) ;
#45346 = CARTESIAN_POINT ( 'NONE',  ( -8.337699078158452792, 1386.911661598467845, 199.8791641365267822 ) ) ;
#45347 = CARTESIAN_POINT ( 'NONE',  ( -28.34436310520023738, 1509.902867357751347, 216.0097923534701749 ) ) ;
#45349 = ORIENTED_EDGE ( 'NONE', *, *, #36650, .T. ) ;
#45348 = DIRECTION ( 'NONE',  ( 0.000000000000000000, 0.000000000000000000, 1.000000000000000000 ) ) ;
#45350 = CARTESIAN_POINT ( 'NONE',  ( -4.379874935479580955, 1508.551704408389924, 219.7958719070109908 ) ) ;
#45351 = ORIENTED_EDGE ( 'NONE', *, *, #80382, .F. ) ;
#45352 = CARTESIAN_POINT ( 'NONE',  ( -12.49220237150879953, 1391.410446187260050, 209.7523967365880253 ) ) ;
#45353 = CARTESIAN_POINT ( 'NONE',  ( -17.84636972919999920, 1416.824060884729988, 211.9816702729980022 ) ) ;
#45354 = CARTESIAN_POINT ( 'NONE',  ( -16.66936639845610557, 1523.456872492435195, 237.7608804993221838 ) ) ;
#45355 = VECTOR ( 'NONE', #80439, 1000.000000000000000 ) ;
#45357 = ADVANCED_FACE ( 'NONE', ( #62459 ), #11460, .T. ) ;
#45356 = CARTESIAN_POINT ( 'NONE',  ( -2.824334885622032054, 1367.715600639032345, 209.0250458202570201 ) ) ;
#45358 = CARTESIAN_POINT ( 'NONE',  ( -23.55087667009999919, 1411.110693366829764, 210.4794020521279947 ) ) ;
#45359 = CARTESIAN_POINT ( 'NONE',  ( -17.88808968309999869, 1422.733202112150138, 207.9839376467890020 ) ) ;
#45360 = CARTESIAN_POINT ( 'NONE',  ( 14.82290709384709970, 1409.430687709029826, 210.9403263768460022 ) ) ;
#45361 = CARTESIAN_POINT ( 'NONE',  ( 18.79226589730000185, 1456.307606824690083, 213.7887498653890077 ) ) ;
#45362 = CARTESIAN_POINT ( 'NONE',  ( -103.0445127499399831, 1385.228392731539770, 296.7348340301609824 ) ) ;
#45363 = CARTESIAN_POINT ( 'NONE',  ( -17.29603831340000042, 1410.862735422030028, 192.2532255665980188 ) ) ;
#45364 = DIRECTION ( 'NONE',  ( 0.000000000000000000, 0.000000000000000000, -1.000000000000000000 ) ) ;
#45365 = EDGE_CURVE ( 'NONE', #64002, #14979, #92783, .T. ) ;
#45366 = CARTESIAN_POINT ( 'NONE',  ( 11.00095395210620097, 1490.665236598310003, 207.4715718885979925 ) ) ;
#45368 = EDGE_LOOP ( 'NONE', ( #60113, #61780, #80081, #20973, #68162, #65626, #67230, #92043 ) ) ;
#45367 = CARTESIAN_POINT ( 'NONE',  ( -0.7910245917146945249, 1426.918876941764893, 137.0999999980979851 ) ) ;
#45369 = ORIENTED_EDGE ( 'NONE', *, *, #90605, .F. ) ;
#45370 = CARTESIAN_POINT ( 'NONE',  ( -11.97935895653369975, 1415.724942525250071, 194.9476232739520185 ) ) ;
#45371 = CARTESIAN_POINT ( 'NONE',  ( -11.88165080699999976, 1433.650567186270109, 150.7135751917980144 ) ) ;
#45372 = CARTESIAN_POINT ( 'NONE',  ( 16.18176546483328337, 1469.066097393567134, 269.3698469196583005 ) ) ;
#45373 = CARTESIAN_POINT ( 'NONE',  ( 12.22507006113399974, 1427.248780726589985, 207.5705273738180097 ) ) ;
#45374 = CARTESIAN_POINT ( 'NONE',  ( 2.228686234730000049, 1395.990887825629898, 219.9947577375980359 ) ) ;
#45375 = CARTESIAN_POINT ( 'NONE',  ( 31.87595007833802896, 1525.042412244735260, 202.1059224821480882 ) ) ;
#45376 = CARTESIAN_POINT ( 'NONE',  ( -5.380079384537971521, 1516.847814776033829, 214.3564748279252115 ) ) ;
#45377 = EDGE_CURVE ( 'NONE', #52269, #39456, #110688, .T. ) ;
#45378 = CARTESIAN_POINT ( 'NONE',  ( -1.447759217700000045, 1462.381657091629904, 183.4226446242979875 ) ) ;
#45379 = CARTESIAN_POINT ( 'NONE',  ( -9.830395177430180098, 1365.769828494181866, 210.6218459616991936 ) ) ;
#45380 = CARTESIAN_POINT ( 'NONE',  ( -20.84167267519909927, 1473.796631674460059, 208.8510855306950020 ) ) ;
#45381 = ADVANCED_FACE ( 'NONE', ( #5830 ), #15184, .T. ) ;
#45382 = CARTESIAN_POINT ( 'NONE',  ( 3.445685077385000294, 1516.778761582560037, 206.6297153089269898 ) ) ;
#45383 = CARTESIAN_POINT ( 'NONE',  ( -12.97884118909520090, 1435.865575512450050, 150.7205278897419873 ) ) ;
#45384 = CARTESIAN_POINT ( 'NONE',  ( 1.546896711520000078, 1416.831925117829996, 190.2226034001980111 ) ) ;
#45385 = CARTESIAN_POINT ( 'NONE',  ( 1.402559146139999990, 1498.352971756790112, 197.8773470515990027 ) ) ;
#45386 = CARTESIAN_POINT ( 'NONE',  ( 9277.788495748482092, 2833.746317950237426, 5939.014819510221969 ) ) ;
#45387 = EDGE_CURVE ( 'NONE', #76248, #39549, #65983, .T. ) ;
#45388 = CARTESIAN_POINT ( 'NONE',  ( -104.4199114259999845, 1380.436187834239945, 300.6363748219590093 ) ) ;
#45389 = ORIENTED_EDGE ( 'NONE', *, *, #40030, .T. ) ;
#45390 = FACE_OUTER_BOUND ( 'NONE', #2247, .T. ) ;
#45391 = CARTESIAN_POINT ( 'NONE',  ( -25.55495559180000242, 1449.803351303929958, 207.8073733729480068 ) ) ;
#45393 = CARTESIAN_POINT ( 'NONE',  ( -1.468632328674980059, 1507.614846039610256, 232.0487233915610261 ) ) ;
#45392 = CARTESIAN_POINT ( 'NONE',  ( 1.448541675109999760, 1507.271700846029944, 181.1064074016979930 ) ) ;
#45394 = CARTESIAN_POINT ( 'NONE',  ( 4.043366220174999803, 1516.951766529250108, 211.9887038632370206 ) ) ;
#45395 = CARTESIAN_POINT ( 'NONE',  ( -121.7571430937320827, 1377.913060387289988, 299.6563178771723415 ) ) ;
#45396 = CARTESIAN_POINT ( 'NONE',  ( 1.007819525709999926E-09, 1413.088571902429976, 250.5651368501980585 ) ) ;
#45397 = CARTESIAN_POINT ( 'NONE',  ( 2.459010662519999890, 1485.097423333889992, 220.7348024981990307 ) ) ;
#45398 = CARTESIAN_POINT ( 'NONE',  ( 2.613924552144012647, 1516.542698303460384, 216.8310974888379405 ) ) ;
#45399 = CARTESIAN_POINT ( 'NONE',  ( -113.4000000000000057, 1391.413060387289988, 304.2218459572590064 ) ) ;
#45400 = CARTESIAN_POINT ( 'NONE',  ( 31.79026207699999773, 1451.347618454329904, 136.0085524639980008 ) ) ;
#45401 = ORIENTED_EDGE ( 'NONE', *, *, #20636, .T. ) ;
#45402 = DIRECTION ( 'NONE',  ( -0.8672669759446595128, 0.000000000000000000, 0.4978433412588795237 ) ) ;
#45403 = CARTESIAN_POINT ( 'NONE',  ( 14.24701162106355135, 1514.160701258722611, 225.6749658073803460 ) ) ;
#45404 = CARTESIAN_POINT ( 'NONE',  ( 5.915282300339999466, 1509.133079420229933, 238.3429575466979884 ) ) ;
#45405 = ORIENTED_EDGE ( 'NONE', *, *, #46098, .T. ) ;
#45406 = EDGE_LOOP ( 'NONE', ( #15874, #6324, #18185, #20750, #1404, #25662, #55842, #28598, #95637, #100478, #81017, #77171 ) ) ;
#45407 = CARTESIAN_POINT ( 'NONE',  ( 9.072576645759729885, 1451.848759158979874, 211.1174303628249902 ) ) ;
#45408 = CARTESIAN_POINT ( 'NONE',  ( -23.56625521110860078, 1410.013281350479929, 208.7413815090230003 ) ) ;
#45409 = VERTEX_POINT ( 'NONE', #69064 ) ;
#45410 = CARTESIAN_POINT ( 'NONE',  ( 0.3641805756409999817, 1424.317995881729985, 227.5054904077979927 ) ) ;
#45411 = CARTESIAN_POINT ( 'NONE',  ( -11.03352341481849841, 1462.446812322350070, 208.7213867630900097 ) ) ;
#45412 = CARTESIAN_POINT ( 'NONE',  ( -0.3409206044646166944, 1415.414754857631124, 233.4258456977717913 ) ) ;
#45413 = CARTESIAN_POINT ( 'NONE',  ( -1.697089624030000188, 1470.485572925830184, 235.4907127086979699 ) ) ;
#45414 = ADVANCED_FACE ( 'NONE', ( #1293 ), #15836, .T. ) ;
#45415 = CARTESIAN_POINT ( 'NONE',  ( 5.513200267037420055, 1508.884117426719968, 201.6131409466659932 ) ) ;
#45416 = ORIENTED_EDGE ( 'NONE', *, *, #32198, .F. ) ;
#45417 = CARTESIAN_POINT ( 'NONE',  ( 11.73650491189999912, 1426.280347616930158, 144.1690576437979985 ) ) ;
#45418 = CARTESIAN_POINT ( 'NONE',  ( -0.3613963699280030029, 1502.117394456789953, 230.5447891057989978 ) ) ;
#45419 = EDGE_CURVE ( 'NONE', #60672, #51752, #100639, .T. ) ;
#45420 = CARTESIAN_POINT ( 'NONE',  ( -108.0465155092619938, 1384.898365638199948, 297.0924029035859348 ) ) ;
#45421 = VERTEX_POINT ( 'NONE', #33216 ) ;
#45422 = CARTESIAN_POINT ( 'NONE',  ( 5.774609621945000271, 1516.777260590120022, 204.5018377250270021 ) ) ;
#45423 = ORIENTED_EDGE ( 'NONE', *, *, #59764, .F. ) ;
#45424 = CARTESIAN_POINT ( 'NONE',  ( 11.85970193668129902, 1431.889404567069960, 149.9640874058029851 ) ) ;
#45425 = CARTESIAN_POINT ( 'NONE',  ( 13.36058313908647044, 1444.493815334265719, 187.6475059284200029 ) ) ;
#45426 = ORIENTED_EDGE ( 'NONE', *, *, #20166, .T. ) ;
#45427 = CARTESIAN_POINT ( 'NONE',  ( 29.37019419317383750, 1526.382868172864164, 200.9844875749016921 ) ) ;
#45428 = CARTESIAN_POINT ( 'NONE',  ( -13.35741048202589809, 1443.913060387329324, 164.9741927960640453 ) ) ;
#45429 = CARTESIAN_POINT ( 'NONE',  ( 10.84641677149999950, 1508.005366378329882, 234.2312760136979648 ) ) ;
#45430 = CARTESIAN_POINT ( 'NONE',  ( -9.535170673477109560, 1471.930435161360037, 212.6674250506980002 ) ) ;
#45431 = CARTESIAN_POINT ( 'NONE',  ( 22.74411444316890041, 1452.118818409569940, 139.2434547346800002 ) ) ;
#45432 = CARTESIAN_POINT ( 'NONE',  ( 4.301461580539999829, 1407.800349814830042, 270.1336327149980434 ) ) ;
#45433 = CARTESIAN_POINT ( 'NONE',  ( -105.3239982070000025, 1388.772974685380177, 299.3169349243589750 ) ) ;
#45434 = CARTESIAN_POINT ( 'NONE',  ( -12.66657887843499886, 1502.203781315570041, 210.6663731483399999 ) ) ;
#45435 = CARTESIAN_POINT ( 'NONE',  ( 9.796230887720000169, 1493.843361169789887, 216.7872332751290116 ) ) ;
#45436 = CARTESIAN_POINT ( 'NONE',  ( -32.71421740720000315, 1379.624840865300030, 215.8883633175389889 ) ) ;
#45437 = VECTOR ( 'NONE', #108456, 1000.000000000000114 ) ;
#45438 = CARTESIAN_POINT ( 'NONE',  ( 0.03183378633081759140, 1410.137908188304209, 233.2064185424406730 ) ) ;
#45440 = CARTESIAN_POINT ( 'NONE',  ( 14.57547838410000018, 1434.997135647729920, 195.8289395455979900 ) ) ;
#45439 = CARTESIAN_POINT ( 'NONE',  ( -14.95480896039999941, 1503.828903730489856, 208.7757359552959997 ) ) ;
#45441 = CARTESIAN_POINT ( 'NONE',  ( -59.67093331520844401, 1379.746016655268022, 264.7494437571154435 ) ) ;
#45442 = EDGE_CURVE ( 'NONE', #107049, #21389, #5254, .T. ) ;
#45443 = DIRECTION ( 'NONE',  ( -1.755985294532469921E-16, 1.000000000000000000, -1.338183447452831989E-16 ) ) ;
#45444 = CARTESIAN_POINT ( 'NONE',  ( -7.585800469905000121, 1513.656171171920050, 202.9549341796069939 ) ) ;
#45445 = ORIENTED_EDGE ( 'NONE', *, *, #107596, .F. ) ;
#45446 = CARTESIAN_POINT ( 'NONE',  ( 25.52872274739999980, 1431.191366579289934, 248.0989693021979861 ) ) ;
#45447 = AXIS2_PLACEMENT_3D ( 'NONE', #71864, #80769, #104313 ) ;
#45448 = CARTESIAN_POINT ( 'NONE',  ( 19.74164504280149757, 1455.376031929259852, 226.0788368184279875 ) ) ;
#45449 = CARTESIAN_POINT ( 'NONE',  ( -73.28822514871049520, 1385.013224671080025, 298.4902431103309937 ) ) ;
#45450 = B_SPLINE_SURFACE_WITH_KNOTS ( 'NONE', 5, 5, ( 
 ( #12144, #98352, #45225, #12697, #29490, #72093, #46879, #105112, #53631, #79916, #87773, #106747 ),
 ( #28959, #21624, #63148, #27850, #47415, #36248, #46335, #80465, #97249, #55829, #20525, #62031 ),
 ( #70436, #3779, #19988, #21074, #28402, #64228, #96153, #45781, #3229, #11054, #19430, #79364 ),
 ( #89950, #88859, #37911, #97796, #106207, #81536, #63685, #55279, #54731, #36802, #72616, #70994 ),
 ( #37356, #4313, #71556, #62602, #105676, #89409, #38441, #30035, #31142, #65329, #82097, #91046 ),
 ( #73162, #98898, #5398, #23286, #109518, #66435, #13772, #99438, #39556, #90497, #22715, #49622 ),
 ( #4838, #57482, #107307, #91607, #64788, #14334, #14884, #74281, #31693, #38986, #47957, #32255 ),
 ( #48524, #23831, #107853, #82663, #49075, #83210, #74824, #24388, #22167, #6499, #5954, #56915 ),
 ( #40099, #40651, #56366, #7052, #108968, #32794, #73730, #108410, #100551, #65876, #30601, #58023 ),
 ( #66978, #99995, #58572, #92158, #15431, #92700, #83755, #41209, #75379, #101089, #15977, #50179 ),
 ( #76459, #7597, #78112, #26031, #35555, #110613, #60226, #69750, #93255, #60795, #77574, #9265 ),
 ( #51827, #8688, #25484, #9806, #43425, #1414, #882, #16519, #103291, #85965, #33338, #17622 ) ),
 .UNSPECIFIED., .F., .F., .F.,
 ( 6, 3, 3, 6 ),
 ( 6, 3, 3, 6 ),
 ( 9.583913663940000660, 9.799048146840000584, 10.22931711260000043, 10.62862691149999961 ),
 ( 0.000000000000000000, 0.5190412869870000279, 1.557123860959999995, 2.181622595539999931 ),
 .UNSPECIFIED. ) ;
#45451 = CARTESIAN_POINT ( 'NONE',  ( -18.00465857450906171, 1523.390106123591067, 180.2140906788921768 ) ) ;
#45452 = CARTESIAN_POINT ( 'NONE',  ( -8.060900218429999597, 1384.928187126620060, 199.5679324677990110 ) ) ;
#45453 = CARTESIAN_POINT ( 'NONE',  ( -14.45258097049999968, 1415.677402202029953, 212.7925583659589677 ) ) ;
#45455 = ORIENTED_EDGE ( 'NONE', *, *, #82845, .T. ) ;
#45454 = CARTESIAN_POINT ( 'NONE',  ( 12.82765434203870036, 1421.015154487590053, 203.4288627072589861 ) ) ;
#45456 = CARTESIAN_POINT ( 'NONE',  ( -16.98474706396019940, 1418.194805350959768, 204.1434201589789836 ) ) ;
#45457 = CARTESIAN_POINT ( 'NONE',  ( -24.28111689179999999, 1443.009146190699994, 211.5138934351579962 ) ) ;
#45458 = EDGE_CURVE ( 'NONE', #1895, #64042, #24791, .T. ) ;
#45459 = CARTESIAN_POINT ( 'NONE',  ( 0.4151546846821903003, 1512.187213306747481, 175.3106345060153046 ) ) ;
#45460 = CARTESIAN_POINT ( 'NONE',  ( 0.8227887822411580343, 1430.698630372429989, 199.7159915099159946 ) ) ;
#45461 = CARTESIAN_POINT ( 'NONE',  ( 31.81407709660777527, 1522.382868172863937, 221.9534378623329758 ) ) ;
#45462 = CARTESIAN_POINT ( 'NONE',  ( 5.368952396500120017, 1422.346041120678137, 139.6186957304907423 ) ) ;
#45463 = CARTESIAN_POINT ( 'NONE',  ( 30.68911337542330031, 1510.023616807530061, 207.3140646301669960 ) ) ;
#45464 = ADVANCED_FACE ( 'NONE', ( #110483 ), #3517, .T. ) ;
#45465 = DIRECTION ( 'NONE',  ( 0.000000000000000000, 0.000000000000000000, -1.000000000000000000 ) ) ;
#45466 = CARTESIAN_POINT ( 'NONE',  ( -13.38643379071410067, 1424.212137269759978, 222.1368579475470142 ) ) ;
#45467 = CARTESIAN_POINT ( 'NONE',  ( 14.08419818750000019, 1417.423210508630063, 228.3178852520979945 ) ) ;
#45468 = CARTESIAN_POINT ( 'NONE',  ( -6.409121316630000287, 1477.410212878089851, 217.9096042521290144 ) ) ;
#45469 = CARTESIAN_POINT ( 'NONE',  ( -15.95951032299999817, 1459.271785846329976, 230.7209114582980192 ) ) ;
#45470 = CARTESIAN_POINT ( 'NONE',  ( -5.014195139944999546, 1517.120861839400050, 207.4163795216369977 ) ) ;
#45471 = CARTESIAN_POINT ( 'NONE',  ( 45.67178907760000328, 1438.934187320510091, 266.1885947808980291 ) ) ;
#45472 = CARTESIAN_POINT ( 'NONE',  ( -17.08792848909999762, 1409.509783999230194, 223.5124184947979984 ) ) ;
#45473 = CARTESIAN_POINT ( 'NONE',  ( 21.52776548289999781, 1435.248012972100014, 141.8788503976979882 ) ) ;
#45474 = CARTESIAN_POINT ( 'NONE',  ( 21.56160677299999762, 1488.583446177329961, 192.9734763627979817 ) ) ;
#45475 = B_SPLINE_CURVE_WITH_KNOTS ( 'NONE', 5,
 ( #99960, #108933, #107269, #106710, #98865, #82631 ),
 .UNSPECIFIED., .F., .F.,
 ( 6, 6 ),
 ( 367.7284095229999821, 372.8603425570000240 ),
 .UNSPECIFIED. ) ;
#45476 = CARTESIAN_POINT ( 'NONE',  ( 22.33217208762076567, 1507.117986420830903, 213.2665276028900223 ) ) ;
#45477 = CARTESIAN_POINT ( 'NONE',  ( -13.05809432774470125, 1379.371362203710078, 208.0847928999789929 ) ) ;
#45478 = FACE_OUTER_BOUND ( 'NONE', #35748, .T. ) ;
#45479 = DIRECTION ( 'NONE',  ( 0.07268319384289673168, 0.1273111294819405659, 0.9891961532693243075 ) ) ;
#45480 = CARTESIAN_POINT ( 'NONE',  ( -35.96078749620780002, 1435.914108659089834, 135.0260228449310205 ) ) ;
#45481 = CARTESIAN_POINT ( 'NONE',  ( -8.177500540760000547, 1409.018193663230022, 197.5736553931980097 ) ) ;
#45482 = CARTESIAN_POINT ( 'NONE',  ( -13.73040295794826626, 1517.051704408389924, 190.6090220196199141 ) ) ;
#45483 = CARTESIAN_POINT ( 'NONE',  ( -12.22014152740000092, 1442.565459838870083, 186.7736584056979723 ) ) ;
#45484 = EDGE_CURVE ( 'NONE', #93138, #43348, #58826, .T. ) ;
#45485 = CARTESIAN_POINT ( 'NONE',  ( -27.83433503068760118, 1508.487004160019978, 210.5257724136350248 ) ) ;
#45486 = CARTESIAN_POINT ( 'NONE',  ( -32.76525573750000575, 1435.801895108220151, 135.9795175970980097 ) ) ;
#45487 = SPHERICAL_SURFACE ( 'NONE', #99727, 2.000000000000000000 ) ;
#45488 = ORIENTED_EDGE ( 'NONE', *, *, #9842, .T. ) ;
#45489 = ADVANCED_FACE ( 'NONE', ( #28135 ), #52805, .F. ) ;
#45490 = CARTESIAN_POINT ( 'NONE',  ( -2.950959360024999700, 1512.115618635729788, 201.2383024395870166 ) ) ;
#45491 = CARTESIAN_POINT ( 'NONE',  ( -5.462998291771629766, 1409.103832491430012, 223.0682412077159995 ) ) ;
#45492 = CARTESIAN_POINT ( 'NONE',  ( 13.04908991639337223, 1414.913372219064513, 198.1359170763897453 ) ) ;
#45494 = EDGE_CURVE ( 'NONE', #8084, #3002, #94384, .T. ) ;
#45493 = DIRECTION ( 'NONE',  ( -1.000000000000000000, 0.000000000000000000, 0.000000000000000000 ) ) ;
#45495 = CARTESIAN_POINT ( 'NONE',  ( -31.69092635890000054, 1466.505745313929992, 267.1138753099980363 ) ) ;
#45496 = B_SPLINE_CURVE_WITH_KNOTS ( 'NONE', 3,
 ( #84118, #30964, #108221, #48899, #58935, #24200 ),
 .UNSPECIFIED., .F., .F.,
 ( 4, 2, 4 ),
 ( 0.000000000000000000, 0.2372834985116590023, 0.4746949337468490127 ),
 .UNSPECIFIED. ) ;
#45497 = CARTESIAN_POINT ( 'NONE',  ( -29.67375891016008893, 1525.697947650397282, 196.9718794197341651 ) ) ;
#45498 = CARTESIAN_POINT ( 'NONE',  ( 0.4850247063263399827, 1418.706296401290047, 184.7123392401769877 ) ) ;
#45499 = CARTESIAN_POINT ( 'NONE',  ( -25.66084629220000224, 1508.559638941529784, 218.3457568381680005 ) ) ;
#45500 = CARTESIAN_POINT ( 'NONE',  ( -86.43903678570190152, 1384.625844868130116, 307.3438020039649814 ) ) ;
#45501 = CARTESIAN_POINT ( 'NONE',  ( -48.09174099008450298, 1385.012596446669932, 222.4136726372699968 ) ) ;
#45502 = CARTESIAN_POINT ( 'NONE',  ( -19.63722818156799832, 1517.151704408390060, 200.0074286628000095 ) ) ;
#45503 = CARTESIAN_POINT ( 'NONE',  ( 15.87297696450000117, 1415.931391677429929, 217.5250545781579774 ) ) ;
#45504 = CARTESIAN_POINT ( 'NONE',  ( 15.82374665889999932, 1506.811133753330068, 224.4050091913979941 ) ) ;
#45505 = EDGE_CURVE ( 'NONE', #101515, #35341, #107613, .T. ) ;
#45506 = CARTESIAN_POINT ( 'NONE',  ( -31.22294729666638347, 1523.678648413191695, 195.3480975247483968 ) ) ;
#45507 = DIRECTION ( 'NONE',  ( -0.8962072375315806028, 8.149454628506528759E-17, 0.4436356471204868090 ) ) ;
#45508 = CARTESIAN_POINT ( 'NONE',  ( -7.965887108789999616, 1384.923044073590063, 199.4891954346890088 ) ) ;
#45509 = CARTESIAN_POINT ( 'NONE',  ( -17.66967187194796551, 1521.951704408389787, 195.1406325242839159 ) ) ;
#45510 =( BOUNDED_CURVE ( )  B_SPLINE_CURVE ( 2, ( #14519, #23477, #57670 ),
 .UNSPECIFIED., .F., .F. ) 
 B_SPLINE_CURVE_WITH_KNOTS ( ( 3, 3 ),
 ( -0.2337410562555060078, -0.1572692978119380192 ),
 .UNSPECIFIED. ) 
 CURVE ( )  GEOMETRIC_REPRESENTATION_ITEM ( )  RATIONAL_B_SPLINE_CURVE ( ( 1.002760198482619991, 1.002448066741719934, 1.002044729649790078 ) ) 
 REPRESENTATION_ITEM ( '' )  );
#45511 = DIRECTION ( 'NONE',  ( -0.000000000000000000, -1.000000000000000000, -0.000000000000000000 ) ) ;
#45512 = CARTESIAN_POINT ( 'NONE',  ( -11.65314573679999910, 1415.128105759529944, 195.5562631955979782 ) ) ;
#45513 = CARTESIAN_POINT ( 'NONE',  ( -0.6756013102099980294, 1422.780067699609845, 192.4727110829989840 ) ) ;
#45514 = CARTESIAN_POINT ( 'NONE',  ( 23.34735829830000142, 1409.892898176630069, 210.3646172626779958 ) ) ;
#45515 = CARTESIAN_POINT ( 'NONE',  ( -8.401877990506491756, 1449.017984408099892, 191.5381300880989954 ) ) ;
#45516 = CARTESIAN_POINT ( 'NONE',  ( 19.02097995950469667, 1454.195557636890044, 200.7033899366429921 ) ) ;
#45517 = CARTESIAN_POINT ( 'NONE',  ( -15.64558125519999798, 1421.345168983629947, 227.1284469843980105 ) ) ;
#45519 = CARTESIAN_POINT ( 'NONE',  ( -12.23669308090000030, 1377.661331661229951, 207.7794332492889851 ) ) ;
#45518 = CARTESIAN_POINT ( 'NONE',  ( -11.76895986610000122, 1432.299385031119982, 150.8120305877979774 ) ) ;
#45520 = CARTESIAN_POINT ( 'NONE',  ( 1.360111617359999858, 1413.043121558629991, 232.7545279162980023 ) ) ;
#45521 = CARTESIAN_POINT ( 'NONE',  ( -1.905692013638440199E-05, 1510.912288461360276, 238.4016852072749941 ) ) ;
#45522 = CARTESIAN_POINT ( 'NONE',  ( -11.12919673650000085, 1490.198289314490012, 211.5851026735989819 ) ) ;
#45523 = EDGE_CURVE ( 'NONE', #27860, #98602, #69417, .T. ) ;
#45524 = CARTESIAN_POINT ( 'NONE',  ( -23.01761228259999825, 1420.939394082029821, 211.7869335952879908 ) ) ;
#45525 = CARTESIAN_POINT ( 'NONE',  ( 9.717824533310780666, 1463.678478211699939, 210.3770741684630252 ) ) ;
#45526 = CARTESIAN_POINT ( 'NONE',  ( 1.704794803334999997, 1517.096587378560116, 204.4952540647470016 ) ) ;
#45527 = CARTESIAN_POINT ( 'NONE',  ( 22.75273496409597485, 1518.913060387330006, 234.5707981297185825 ) ) ;
#45528 = CARTESIAN_POINT ( 'NONE',  ( -18.07065601792569609, 1485.598387672470153, 188.8799623616880012 ) ) ;
#45529 = EDGE_CURVE ( 'NONE', #100109, #82048, #11894, .T. ) ;
#45530 = CARTESIAN_POINT ( 'NONE',  ( -4.237077472001714362, 1454.676950755804683, 200.7191022525509823 ) ) ;
#45531 = CARTESIAN_POINT ( 'NONE',  ( -10.65952630784540389, 1422.351730238593291, 210.6396139690640439 ) ) ;
#45532 = CONICAL_SURFACE ( 'NONE', #38291, 7.500000000000000000, 0.02617993877989872875 ) ;
#45534 = EDGE_LOOP ( 'NONE', ( #3826, #30208, #40296, #4600, #70221 ) ) ;
#45533 = CARTESIAN_POINT ( 'NONE',  ( -61.38583038131619674, 1379.728379092859768, 268.3198502261870431 ) ) ;
#45535 = ORIENTED_EDGE ( 'NONE', *, *, #62570, .T. ) ;
#45536 = CARTESIAN_POINT ( 'NONE',  ( 28.15433651829999917, 1508.637654299029919, 210.1278126086380098 ) ) ;
#45537 = ORIENTED_EDGE ( 'NONE', *, *, #5587, .T. ) ;
#45538 = CARTESIAN_POINT ( 'NONE',  ( -7.649966146998510297, 1507.551694032670184, 219.0282776340299904 ) ) ;
#45539 = CARTESIAN_POINT ( 'NONE',  ( 1.442946131862450132, 1414.913527292460003, 192.0294442267889963 ) ) ;
#45541 = CARTESIAN_POINT ( 'NONE',  ( 15.69039281178419998, 1410.711140847010029, 191.5212508507599978 ) ) ;
#45540 = CARTESIAN_POINT ( 'NONE',  ( 2.409586283469999923, 1426.663880916129983, 144.1938086916980239 ) ) ;
#45542 = CARTESIAN_POINT ( 'NONE',  ( 15.76562750197309981, 1459.955010096749902, 221.8162589312199771 ) ) ;
#45543 = CARTESIAN_POINT ( 'NONE',  ( -25.01942180936440252, 1452.023553701150149, 135.7955166689109774 ) ) ;
#45544 = CARTESIAN_POINT ( 'NONE',  ( -1.511034998550000008, 1467.833985848489874, 220.1514606783989905 ) ) ;
#45545 = CARTESIAN_POINT ( 'NONE',  ( 11.06788630610000013, 1410.673659464129969, 229.4061172066979850 ) ) ;
#45546 =( LENGTH_UNIT ( ) NAMED_UNIT ( * ) SI_UNIT ( .MILLI., .METRE. ) );
#45547 = CARTESIAN_POINT ( 'NONE',  ( 7.724732408895000013, 1517.133889586189980, 212.3822030989969960 ) ) ;
#45548 = CARTESIAN_POINT ( 'NONE',  ( 41.54171725203300269, 1442.308966536529852, 134.0999999980950008 ) ) ;
#45549 = CARTESIAN_POINT ( 'NONE',  ( -3.986282491261569305, 1428.493128888279898, 206.6345495674519839 ) ) ;
#45550 = CARTESIAN_POINT ( 'NONE',  ( -0.5649602707880300168, 1422.725929253230106, 228.0279234539580102 ) ) ;
#45551 = ORIENTED_EDGE ( 'NONE', *, *, #82960, .T. ) ;
#45552 = CARTESIAN_POINT ( 'NONE',  ( -8.229011145687781692, 1439.448126226759996, 228.6152129487579998 ) ) ;
#45553 = CARTESIAN_POINT ( 'NONE',  ( -10.80389986116539980, 1440.331015950379879, 224.4356702096399943 ) ) ;
#45554 = ORIENTED_EDGE ( 'NONE', *, *, #68587, .F. ) ;
#45555 = VERTEX_POINT ( 'NONE', #96451 ) ;
#45556 = ORIENTED_EDGE ( 'NONE', *, *, #71079, .T. ) ;
#45557 = CARTESIAN_POINT ( 'NONE',  ( -7.382751585984999920, 1511.929989569689951, 215.7327168677470013 ) ) ;
#45558 = CARTESIAN_POINT ( 'NONE',  ( -1.371657577609999734, 1464.950064278530135, 237.5599504942979934 ) ) ;
#45559 = CARTESIAN_POINT ( 'NONE',  ( 24.13517773408675637, 1450.842116807829370, 139.9688489162871861 ) ) ;
#45560 = CARTESIAN_POINT ( 'NONE',  ( -7.544889814560000296, 1384.926148861729871, 219.0875907562389955 ) ) ;
#45561 = FACE_OUTER_BOUND ( 'NONE', #100148, .T. ) ;
#45562 = CARTESIAN_POINT ( 'NONE',  ( -13.87256047439999840, 1379.747987721680147, 208.2173326269899860 ) ) ;
#45563 = CARTESIAN_POINT ( 'NONE',  ( -67.76017963322829019, 1379.745894740751737, 277.9423129414287246 ) ) ;
#45564 = CARTESIAN_POINT ( 'NONE',  ( 4.232600372065029148, 1446.314696765329927, 164.3435975946949839 ) ) ;
#45565 = CARTESIAN_POINT ( 'NONE',  ( 8.660201460965680553, 1437.683719626410038, 209.3645222499649776 ) ) ;
#45566 = ORIENTED_EDGE ( 'NONE', *, *, #38978, .T. ) ;
#45567 = CARTESIAN_POINT ( 'NONE',  ( 1.117840086735000016, 1516.949031626070109, 207.4047068479870006 ) ) ;
#45568 = VERTEX_POINT ( 'NONE', #55018 ) ;
#45569 = CARTESIAN_POINT ( 'NONE',  ( 28.76621075204660016, 1440.913060387330006, 249.4063077180399830 ) ) ;
#45570 = CARTESIAN_POINT ( 'NONE',  ( -13.70772810569999933, 1507.648154634329785, 184.2587348614979987 ) ) ;
#45571 = ORIENTED_EDGE ( 'NONE', *, *, #5075, .T. ) ;
#45572 = CARTESIAN_POINT ( 'NONE',  ( 25.40180382489500133, 1449.929728973520014, 137.7573714004559804 ) ) ;
#45573 = CARTESIAN_POINT ( 'NONE',  ( -13.50742185299999853, 1409.384749952230095, 191.0679001674980100 ) ) ;
#45574 = CARTESIAN_POINT ( 'NONE',  ( -40.62152722268042027, 1379.659798262793174, 229.8373908348060866 ) ) ;
#45576 = CARTESIAN_POINT ( 'NONE',  ( -2.086548178679999754, 1515.551704408389924, 205.2922258481490303 ) ) ;
#45575 = CARTESIAN_POINT ( 'NONE',  ( -24.49670940789999918, 1441.012068752339928, 210.9962413173979883 ) ) ;
#45577 = CARTESIAN_POINT ( 'NONE',  ( -4.391745902125429701, 1433.897785981300103, 217.6620401040709964 ) ) ;
#45578 = CARTESIAN_POINT ( 'NONE',  ( -6.253177289296100838, 1511.742575854359984, 200.3335783645690071 ) ) ;
#45579 = CARTESIAN_POINT ( 'NONE',  ( 26.46631635538070171, 1441.292691108139934, 137.7246575186629798 ) ) ;
#45580 = CARTESIAN_POINT ( 'NONE',  ( -0.5624690339869999889, 1416.828040475229955, 227.7677324846980014 ) ) ;
#45581 = CARTESIAN_POINT ( 'NONE',  ( -6.454495265129999382, 1508.590068290189947, 219.7017392546990209 ) ) ;
#45583 = CARTESIAN_POINT ( 'NONE',  ( 0.8344953249080009350, 1498.972540960489823, 200.5991869134590218 ) ) ;
#45582 = CARTESIAN_POINT ( 'NONE',  ( 7.830985173529999344, 1465.248213122329844, 233.1377974544980134 ) ) ;
#45584 = B_SPLINE_SURFACE_WITH_KNOTS ( 'NONE', 5, 5, ( 
 ( #86470, #84262, #9765, #43930, #78074, #110022, #33298, #24881, #61318 ),
 ( #38272, #37188, #63525, #18700, #28785, #2508, #72456, #36632, #80294 ),
 ( #104939, #87026, #97096, #10315, #62985, #46165, #70272, #79202, #88151 ),
 ( #44489, #95436, #19815, #27680, #53453, #28229, #62415, #12531, #78634 ),
 ( #97641, #88701, #20361, #11439, #89236, #1950, #70829, #36087, #106047 ),
 ( #19246, #104382, #46710, #71383, #71935, #3060, #80839, #3610, #61864 ),
 ( #52896, #45613, #4146, #95982, #45059, #106586, #37733, #11982, #96541 ),
 ( #20909, #87598, #29324, #10887, #54021, #79754, #54568, #55114, #105494 ),
 ( #56600, #39993, #59021, #83104, #101529, #6397, #76359, #24281, #67430 ) ),
 .UNSPECIFIED., .F., .F., .F.,
 ( 6, 3, 6 ),
 ( 6, 3, 6 ),
 ( 24.26519376777359938, 81.54878211889999307, 143.5773940184259914 ),
 ( -1.648442643857350279E-05, 1.000000000000000000, 2.000000000000000000 ),
 .UNSPECIFIED. ) ;
#45585 = CARTESIAN_POINT ( 'NONE',  ( 4.618119666265000589, 1516.706638732659940, 216.0591847158069925 ) ) ;
#45586 = CARTESIAN_POINT ( 'NONE',  ( -2.485500793217951809, 1524.600389084707103, 242.5122197736536975 ) ) ;
#45587 = CARTESIAN_POINT ( 'NONE',  ( 5.925858227311150195, 1511.532396045849964, 217.0681951087739776 ) ) ;
#45588 = CARTESIAN_POINT ( 'NONE',  ( 28.30491475510000043, 1508.660124198729818, 209.1118525407709967 ) ) ;
#45589 = CARTESIAN_POINT ( 'NONE',  ( -2.284199401535000007, 1516.940296199220029, 212.3910308785969789 ) ) ;
#45590 = CARTESIAN_POINT ( 'NONE',  ( -11.63852489204760055, 1482.558018235800091, 206.6148454379789996 ) ) ;
#45591 = DIRECTION ( 'NONE',  ( 0.02939029866724141363, 0.9995213403039945321, 0.009659224666439003917 ) ) ;
#45593 = ORIENTED_EDGE ( 'NONE', *, *, #7513, .F. ) ;
#45592 = CARTESIAN_POINT ( 'NONE',  ( -76.12965060780000215, 1386.571707002160110, 301.1838123932589610 ) ) ;
#45594 = CARTESIAN_POINT ( 'NONE',  ( -17.22627300064457145, 1525.856064936156827, 236.4663892367293556 ) ) ;
#45595 = CARTESIAN_POINT ( 'NONE',  ( 12.07243613799999871, 1460.326362140629954, 225.7701189090979881 ) ) ;
#45596 = CARTESIAN_POINT ( 'NONE',  ( 29.67167576299816645, 1526.344110814219903, 216.9865736510273280 ) ) ;
#45597 = CARTESIAN_POINT ( 'NONE',  ( -15.53829606909999939, 1415.702944931670118, 208.9765912623510076 ) ) ;
#45598 = B_SPLINE_CURVE_WITH_KNOTS ( 'NONE', 5,
 ( #7978, #102570, #42145, #91988, #32640, #59509, #7433, #66817, #76295, #32086, #67368, #93620, #110446, #83578, #100918 ),
 .UNSPECIFIED., .F., .F.,
 ( 6, 3, 3, 3, 6 ),
 ( 0.000000000000000000, 0.4627888344713468327, 0.6711646527968716525, 0.8795404711197383207, 1.000000000000000000 ),
 .UNSPECIFIED. ) ;
#45599 = CARTESIAN_POINT ( 'NONE',  ( 2.423063561509999797, 1413.145749552529878, 231.8690496875979932 ) ) ;
#45600 = CARTESIAN_POINT ( 'NONE',  ( -21.85910063620000088, 1453.198086485429940, 221.3407792903979896 ) ) ;
#45601 = TOROIDAL_SURFACE ( 'NONE', #108140, 8.432239102140000497, 0.5000000000000000000 ) ;
#45603 = CARTESIAN_POINT ( 'NONE',  ( 2.500000000000000000, 1419.383622618830032, 144.0642111274979982 ) ) ;
#45602 = CARTESIAN_POINT ( 'NONE',  ( 11.30563928619999992, 1432.585747834659969, 151.5215852997980051 ) ) ;
#45604 = CARTESIAN_POINT ( 'NONE',  ( -9.103468112560660686, 1449.499701819690017, 210.3008494512589834 ) ) ;
#45605 = CARTESIAN_POINT ( 'NONE',  ( -107.3840465399999999, 1380.275172143389909, 309.3291178842590057 ) ) ;
#45606 = ORIENTED_EDGE ( 'NONE', *, *, #29464, .T. ) ;
#45607 = CARTESIAN_POINT ( 'NONE',  ( -3.457266643525000127, 1516.691414181030041, 203.3491180233569935 ) ) ;
#45608 = CARTESIAN_POINT ( 'NONE',  ( 2.764799436670000166, 1406.050782495030035, 266.9581426506979938 ) ) ;
#45609 = VECTOR ( 'NONE', #8358, 1000.000000000000000 ) ;
#45610 = CARTESIAN_POINT ( 'NONE',  ( -0.7322251554670010654, 1515.253704548090127, 213.4463482420090088 ) ) ;
#45611 = B_SPLINE_CURVE_WITH_KNOTS ( 'NONE', 3,
 ( #81170, #63853, #29668, #37527, #54355, #12312, #46502, #2845, #71160, #98524, #20699, #96334, #80635, #12865, #54895, #21790, #105846, #29125, #19612, #97965, #97430, #55992, #47046, #90115, #30210, #21235, #53814, #4485, #45403, #88486, #38616, #3397, #64401, #13398, #38076, #55447, #71729, #105283, #87950, #11771, #3949, #63311, #45940, #79542, #47585, #89020, #2307, #36418, #70610, #72253 ),
 .UNSPECIFIED., .F., .F.,
 ( 4, 2, 2, 1, 1, 2, 2, 2, 2, 1, 1, 1, 2, 2, 2, 2, 1, 1, 1, 2, 2, 2, 2, 1, 1, 1, 1, 2, 2, 2, 4 ),
 ( 0.000000000000000000, 0.1250000000004282963, 0.1875000000006428469, 0.2187500000007644441, 0.2343750000008096579, 0.2421875000008512635, 0.2500000000008928414, 0.3750000000017443824, 0.4375000000021700974, 0.4687500000024091840, 0.4843750000025029423, 0.4921875000025491831, 0.4960937500025454638, 0.5000000000025417446, 0.6250000000030592195, 0.6875000000033516523, 0.7187500000034974246, 0.7343750000035393910, 0.7421875000035882408, 0.7460937500036100012, 0.7500000000036317616, 0.8125000000047263304, 0.8437500000052703397, 0.8593750000055055960, 0.8671875000056231686, 0.8710937500056854521, 0.8730468750057130967, 0.8740234375057269745, 0.8750000000057408522, 0.9375000000028704816, 1.000000000000000000 ),
 .UNSPECIFIED. ) ;
#45612 = AXIS2_PLACEMENT_3D ( 'NONE', #75891, #102178, #61332 ) ;
#45613 = CARTESIAN_POINT ( 'NONE',  ( 43.15564358093790531, 1451.913820396499887, 269.9353367763740721 ) ) ;
#45614 = CARTESIAN_POINT ( 'NONE',  ( 20.12564951288265291, 1511.187213306747708, 180.7149624981943816 ) ) ;
#45615 = CARTESIAN_POINT ( 'NONE',  ( 11.60004869885203682, 1425.703865685336950, 137.2034341738751948 ) ) ;
#45616 = EDGE_CURVE ( 'NONE', #101374, #31336, #33817, .T. ) ;
#45617 = CARTESIAN_POINT ( 'NONE',  ( -42.70248986958939952, 1440.913060410629896, 262.8263052157859647 ) ) ;
#45618 = CARTESIAN_POINT ( 'NONE',  ( -26.10199334550000216, 1450.812712592959997, 136.5826195815980100 ) ) ;
#45619 = CARTESIAN_POINT ( 'NONE',  ( 2.480969307444100824, 1449.204756430078305, 154.5165407172336813 ) ) ;
#45620 = CARTESIAN_POINT ( 'NONE',  ( -1.331958139231829923E-15, 1375.413060387289988, 209.1218459616989946 ) ) ;
#45621 = EDGE_CURVE ( 'NONE', #85474, #61609, #53361, .T. ) ;
#45622 = CARTESIAN_POINT ( 'NONE',  ( 2.428387238925930003, 1449.547206817880124, 154.5200438689840325 ) ) ;
#45623 = CARTESIAN_POINT ( 'NONE',  ( 0.9035508022849989551, 1507.847498519289957, 220.8498822601989957 ) ) ;
#45624 = CARTESIAN_POINT ( 'NONE',  ( 17.61232072907009183, 1419.013269976926495, 192.1957838308312603 ) ) ;
#45625 = VERTEX_POINT ( 'NONE', #35996 ) ;
#45626 = CARTESIAN_POINT ( 'NONE',  ( -8.518323185650000795, 1421.108130360029918, 243.9198229428980085 ) ) ;
#45627 = CARTESIAN_POINT ( 'NONE',  ( -574.7977070613925434, -8383.748406600810995, -1686.503645000492497 ) ) ;
#45629 = CARTESIAN_POINT ( 'NONE',  ( 9.905302590843319877, 1468.559873349059899, 207.6662433566980042 ) ) ;
#45628 = APPLICATION_CONTEXT ( 'automotive_design' ) ;
#45630 = CARTESIAN_POINT ( 'NONE',  ( -0.3370799029359999310, 1475.560362204430021, 269.2946826080980145 ) ) ;
#45631 = CARTESIAN_POINT ( 'NONE',  ( -4.276217621826190474, 1446.770458205470050, 157.0792581084560311 ) ) ;
#45632 = CARTESIAN_POINT ( 'NONE',  ( -29.03008525319999933, 1509.878129414930072, 210.7880756198580059 ) ) ;
#45633 = CARTESIAN_POINT ( 'NONE',  ( -2.581589687633328190, 1448.238659858906885, 183.7528642536733798 ) ) ;
#45634 = CARTESIAN_POINT ( 'NONE',  ( -33.44809598507389836, 1384.815296568380063, 232.0972948743769848 ) ) ;
#45635 = ADVANCED_FACE ( 'NONE', ( #71847 ), #2531, .T. ) ;
#45636 = CARTESIAN_POINT ( 'NONE',  ( -18.26532265589999682, 1415.628674266529742, 208.3526068587169959 ) ) ;
#45637 = CARTESIAN_POINT ( 'NONE',  ( 11.86629848900230044, 1432.349867578880094, 149.9824231379060109 ) ) ;
#45638 = CARTESIAN_POINT ( 'NONE',  ( 26.57100915839980004, 1436.736808227760093, 136.7943505115389939 ) ) ;
#45639 = AXIS2_PLACEMENT_3D ( 'NONE', #98, #35326, #70616 ) ;
#45640 = CARTESIAN_POINT ( 'NONE',  ( -3.600652903801630167, 1396.038797957620091, 219.5432229722080137 ) ) ;
#45641 = CARTESIAN_POINT ( 'NONE',  ( -15.06279246729999954, 1422.388300733229926, 229.4662110884979995 ) ) ;
#45642 = CARTESIAN_POINT ( 'NONE',  ( -15.91967948788279941, 1410.116195902319987, 226.5116202349179844 ) ) ;
#45643 = CARTESIAN_POINT ( 'NONE',  ( 19.35767929529869491, 1455.763342789462740, 225.4551115454407295 ) ) ;
#45644 = ORIENTED_EDGE ( 'NONE', *, *, #9346, .F. ) ;
#45645 = CARTESIAN_POINT ( 'NONE',  ( -11.33909794091723278, 1503.312387898769657, 207.0376778566603377 ) ) ;
#45646 = CARTESIAN_POINT ( 'NONE',  ( -13.58309651533389939, 1508.536267668799837, 210.1614309259379922 ) ) ;
#45647 = CARTESIAN_POINT ( 'NONE',  ( -13.81390074910000010, 1504.365568754290052, 226.5328680220989952 ) ) ;
#45649 = CARTESIAN_POINT ( 'NONE',  ( -14.58906259456500010, 1513.961173499609913, 192.6975966445669712 ) ) ;
#45648 = CARTESIAN_POINT ( 'NONE',  ( 11.17535018360000088, 1426.465084552229882, 103.4411484046980121 ) ) ;
#45650 = DIRECTION ( 'NONE',  ( 0.03489949670250328678, 0.9993908270190956511, 0.000000000000000000 ) ) ;
#45651 = B_SPLINE_CURVE_WITH_KNOTS ( 'NONE', 5,
 ( #24300, #15885, #101546, #94830, #19770, #18106 ),
 .UNSPECIFIED., .F., .F.,
 ( 6, 6 ),
 ( -1.452619041900000019, -2.358414258996077706E-06 ),
 .UNSPECIFIED. ) ;
#45652 = CARTESIAN_POINT ( 'NONE',  ( -9.135474993299999014, 1450.134483540889960, 207.9596447350990047 ) ) ;
#45653 = CARTESIAN_POINT ( 'NONE',  ( 0.7403205670290020635, 1517.139320148880188, 201.3969713189170250 ) ) ;
#45654 = CARTESIAN_POINT ( 'NONE',  ( 7.579106951069999987, 1425.391851912110042, 212.0588301213689988 ) ) ;
#45655 = CARTESIAN_POINT ( 'NONE',  ( 9.992001554820001630, 1491.422527302990147, 188.4943246008990059 ) ) ;
#45656 = CARTESIAN_POINT ( 'NONE',  ( 6.806851077879999323, 1507.558626602530012, 182.5007774465980219 ) ) ;
#45657 = CARTESIAN_POINT ( 'NONE',  ( -0.2223009154971570256, 1416.826860677879949, 191.0546700833079967 ) ) ;
#45658 = CARTESIAN_POINT ( 'NONE',  ( -48.01530467240000633, 1376.719512341220025, 243.5457403057590113 ) ) ;
#45659 = EDGE_CURVE ( 'NONE', #94817, #44756, #4950, .T. ) ;
#45660 = CARTESIAN_POINT ( 'NONE',  ( 4.953742833043618177, 1367.812870383251266, 207.6218459616988241 ) ) ;
#45662 = ORIENTED_EDGE ( 'NONE', *, *, #69339, .F. ) ;
#45661 = CARTESIAN_POINT ( 'NONE',  ( -3.347801439296148818, 1523.456872492435195, 242.0893193391992497 ) ) ;
#45663 = VERTEX_POINT ( 'NONE', #56100 ) ;
#45664 = FACE_OUTER_BOUND ( 'NONE', #81430, .T. ) ;
#45665 = CARTESIAN_POINT ( 'NONE',  ( -0.3345883534476049581, 1474.778737585120098, 235.9370569828869861 ) ) ;
#45666 = CARTESIAN_POINT ( 'NONE',  ( 10.22570915140000025, 1431.113060387329824, 225.5143498067979806 ) ) ;
#45667 = CARTESIAN_POINT ( 'NONE',  ( -7.556074100184999587, 1510.693074690949970, 213.9348573562170088 ) ) ;
#45670 = EDGE_CURVE ( 'NONE', #54763, #21797, #99251, .T. ) ;
#45669 = CARTESIAN_POINT ( 'NONE',  ( -2.055127378149999906, 1486.233656124230038, 181.7623468732980143 ) ) ;
#45668 = CARTESIAN_POINT ( 'NONE',  ( -8.984772871429999697, 1384.158943888290196, 218.6060625040090031 ) ) ;
#45671 = CARTESIAN_POINT ( 'NONE',  ( -31.80537271888373496, 1525.137881624895499, 202.0924996609166158 ) ) ;
#45672 = CARTESIAN_POINT ( 'NONE',  ( 13.15570206748037307, 1428.769203746674748, 222.7935865483545967 ) ) ;
#45673 = CARTESIAN_POINT ( 'NONE',  ( -37.06048519556479448, 1450.125392790749856, 136.1884239245549963 ) ) ;
#45674 =( LENGTH_UNIT ( ) NAMED_UNIT ( * ) SI_UNIT ( .MILLI., .METRE. ) );
#45675 = CARTESIAN_POINT ( 'NONE',  ( -2.500000000000000000, 1448.295519077039899, 164.4141711672770043 ) ) ;
#45676 = CARTESIAN_POINT ( 'NONE',  ( 9.070382607970518762, 1396.229805130280056, 215.4513483083970016 ) ) ;
#45677 = CARTESIAN_POINT ( 'NONE',  ( -39.88064382167599575, 1440.876666208930146, 136.8074513327459840 ) ) ;
#45678 = CARTESIAN_POINT ( 'NONE',  ( -1.520289120366909996, 1406.276897935829993, 269.2942228619830303 ) ) ;
#45679 = ORIENTED_EDGE ( 'NONE', *, *, #87713, .T. ) ;
#45680 = DIRECTION ( 'NONE',  ( 0.000000000000000000, 0.000000000000000000, -1.000000000000000000 ) ) ;
#45681 = CARTESIAN_POINT ( 'NONE',  ( 13.02183306049999878, 1441.592108930330141, 188.8634220520980023 ) ) ;
#45682 = EDGE_LOOP ( 'NONE', ( #76489, #20105, #83806, #110567, #43666, #38064, #104363, #91079 ) ) ;
#45683 = ORIENTED_EDGE ( 'NONE', *, *, #79276, .T. ) ;
#45684 = LINE ( 'NONE', #37259, #25069 ) ;
#45685 = CARTESIAN_POINT ( 'NONE',  ( 4.262353028419999745, 1360.811275533920025, 207.6218459616989946 ) ) ;
#45686 = CARTESIAN_POINT ( 'NONE',  ( 4.618749068485000109, 1516.729202374750002, 215.6716084172169872 ) ) ;
#45687 = CARTESIAN_POINT ( 'NONE',  ( 2.942029631075000040, 1512.314860029340025, 217.0136234567869735 ) ) ;
#45688 = ORIENTED_EDGE ( 'NONE', *, *, #64741, .F. ) ;
#45689 = CARTESIAN_POINT ( 'NONE',  ( 8.136848112800000976, 1426.803698133580156, 211.7678967111889961 ) ) ;
#45690 = CARTESIAN_POINT ( 'NONE',  ( -85.89269277900000077, 1377.100296256970068, 295.7491691192589656 ) ) ;
#45691 = CIRCLE ( 'NONE', #17000, 2.000000000000001776 ) ;
#45692 = CARTESIAN_POINT ( 'NONE',  ( -106.5776706074079954, 1378.913060387289988, 301.7608484320570028 ) ) ;
#45693 = CARTESIAN_POINT ( 'NONE',  ( 6.548821941055000373, 1516.688761843659904, 205.0844676760469838 ) ) ;
#45694 = CARTESIAN_POINT ( 'NONE',  ( -19.66678637224480397, 1519.551704408389924, 215.8936635741279986 ) ) ;
#45695 = B_SPLINE_SURFACE_WITH_KNOTS ( 'NONE', 5, 3, ( 
 ( #62915, #53946, #11369, #45540 ),
 ( #79680, #88629, #37657, #97026 ),
 ( #11908, #46083, #29801, #63989 ),
 ( #89704, #12985, #80215, #55033 ),
 ( #71862, #105980, #89160, #57236 ),
 ( #84052, #99743, #15717, #40398 ) ),
 .UNSPECIFIED., .F., .F., .F.,
 ( 6, 6 ),
 ( 4, 4 ),
 ( 0.000000000000000000, 52.98902693510000006 ),
 ( 37.69911184309999896, 40.20365518519999881 ),
 .UNSPECIFIED. ) ;
#45696 = CARTESIAN_POINT ( 'NONE',  ( -41.28233839276082762, 1435.098719027513653, 269.6338957342284175 ) ) ;
#45697 = CARTESIAN_POINT ( 'NONE',  ( -1.708092304294999808, 1516.523379810429788, 201.4131002843170108 ) ) ;
#45698 = CARTESIAN_POINT ( 'NONE',  ( -6.498943257060000533, 1410.073555944530199, 231.2704400879979971 ) ) ;
#45700 = EDGE_LOOP ( 'NONE', ( #92827, #42819, #52650, #72251 ) ) ;
#45699 = CARTESIAN_POINT ( 'NONE',  ( -12.18971938666500066, 1512.123542805230272, 194.3960765485670095 ) ) ;
#45701 = FACE_OUTER_BOUND ( 'NONE', #30553, .T. ) ;
#45702 = DIRECTION ( 'NONE',  ( 0.000000000000000000, 0.000000000000000000, -1.000000000000000000 ) ) ;
#45703 = CARTESIAN_POINT ( 'NONE',  ( -22.76979002380000239, 1383.850662563309925, 221.8906633995589743 ) ) ;
#45704 = CARTESIAN_POINT ( 'NONE',  ( 15.73091604048637926, 1506.446781332931778, 224.4927539354196711 ) ) ;
#45705 = CARTESIAN_POINT ( 'NONE',  ( 39.33429647749250080, 1428.581013311290235, 269.8320583910219739 ) ) ;
#45706 = CARTESIAN_POINT ( 'NONE',  ( 0.01327404799950150129, 1516.939877939420057, 212.5773418040870126 ) ) ;
#45707 = CARTESIAN_POINT ( 'NONE',  ( -67.88240010660000223, 1379.747289793479922, 278.3094642168589985 ) ) ;
#45708 = CARTESIAN_POINT ( 'NONE',  ( 0.02009193267265866820, 1507.207280861917752, 237.3586468649436938 ) ) ;
#45709 = CARTESIAN_POINT ( 'NONE',  ( -30.15968401513964281, 1524.412455883367329, 222.4100463060516972 ) ) ;
#45711 = CARTESIAN_POINT ( 'NONE',  ( 17.38482601099109814, 1410.884446382940041, 192.4603632472940262 ) ) ;
#45710 = CIRCLE ( 'NONE', #72476, 1.999999999999998446 ) ;
#45712 = CARTESIAN_POINT ( 'NONE',  ( -7.719640941135000212, 1516.939452820819952, 209.1319487995289705 ) ) ;
#45713 = ORIENTED_EDGE ( 'NONE', *, *, #102904, .F. ) ;
#45714 = DIRECTION ( 'NONE',  ( 0.000000000000000000, 1.000000000000000000, -1.836970198721029688E-16 ) ) ;
#45715 = CARTESIAN_POINT ( 'NONE',  ( -1.684665908019999936, 1420.451874816630152, 233.3235451955980011 ) ) ;
#45716 = CARTESIAN_POINT ( 'NONE',  ( -76.09441500830000393, 1384.885120960920176, 301.2261972959589684 ) ) ;
#45717 = ORIENTED_EDGE ( 'NONE', *, *, #101584, .F. ) ;
#45718 = CARTESIAN_POINT ( 'NONE',  ( -29.06065178196929821, 1385.237911838130003, 227.0774918126679722 ) ) ;
#45719 = CARTESIAN_POINT ( 'NONE',  ( -2.669930443950000232, 1429.978190405989835, 201.1023880675990085 ) ) ;
#45720 = CARTESIAN_POINT ( 'NONE',  ( 18.79378390429650025, 1478.713334920350007, 228.4735663057359716 ) ) ;
#45721 = CIRCLE ( 'NONE', #52907, 2.500000000000002220 ) ;
#45722 = CARTESIAN_POINT ( 'NONE',  ( -24.23891439175908147, 1437.877539721478342, 210.9599772510106277 ) ) ;
#45723 = CARTESIAN_POINT ( 'NONE',  ( 11.79002570591860000, 1447.121451514569799, 187.8029540059399949 ) ) ;
#45724 = CARTESIAN_POINT ( 'NONE',  ( -0.09448057143150000170, 1408.916359721629988, 231.7835052710979937 ) ) ;
#45725 = CARTESIAN_POINT ( 'NONE',  ( 0.02235964058503960017, 1420.444490115599820, 182.6732928536509917 ) ) ;
#45726 = B_SPLINE_CURVE_WITH_KNOTS ( 'NONE', 5,
 ( #7128, #25003, #48598, #66515, #75458, #92229, #75983, #40177, #31769 ),
 .UNSPECIFIED., .F., .F.,
 ( 6, 3, 6 ),
 ( 0.000000000000000000, 0.5050532947756587454, 1.000000000000000000 ),
 .UNSPECIFIED. ) ;
#45728 = CARTESIAN_POINT ( 'NONE',  ( 23.28627655106232197, 1507.873435797507682, 223.2320360419293479 ) ) ;
#45727 = CARTESIAN_POINT ( 'NONE',  ( 5.781490544344999982, 1516.807958722750072, 215.6734893570070142 ) ) ;
#45729 = CARTESIAN_POINT ( 'NONE',  ( 19.48412260369999771, 1509.357564207130281, 187.7562371571980009 ) ) ;
#45730 = DIRECTION ( 'NONE',  ( 1.755985294532464991E-16, -1.000000000000000000, 1.338183447452830017E-16 ) ) ;
#45731 = ORIENTED_EDGE ( 'NONE', *, *, #6974, .F. ) ;
#45732 = CARTESIAN_POINT ( 'NONE',  ( -12.92134813639500024, 1416.521607925280023, 196.5106865475920301 ) ) ;
#45733 = CARTESIAN_POINT ( 'NONE',  ( -0.7461436398870000541, 1508.913060260629891, 180.6894241092979883 ) ) ;
#45734 = ORIENTED_EDGE ( 'NONE', *, *, #10291, .F. ) ;
#45735 = CARTESIAN_POINT ( 'NONE',  ( -14.84895963876500780, 1511.957228877180114, 221.1990661657671637 ) ) ;
#45736 = CARTESIAN_POINT ( 'NONE',  ( 18.16442922799999948, 1430.105938726390150, 210.9087875679190063 ) ) ;
#45737 = CARTESIAN_POINT ( 'NONE',  ( 7.447811282559439583, 1511.198033794599951, 202.8566241436609801 ) ) ;
#45738 = CARTESIAN_POINT ( 'NONE',  ( 3.187857858790000165, 1443.094984070389955, 217.4314004907489846 ) ) ;
#45739 = CARTESIAN_POINT ( 'NONE',  ( 15.82264516024399903, 1421.172194390546792, 227.5204971587648970 ) ) ;
#45740 = CARTESIAN_POINT ( 'NONE',  ( 21.71798588809999941, 1410.865989080929921, 202.0964915433179954 ) ) ;
#45741 = LINE ( 'NONE', #86059, #48568 ) ;
#45742 = CARTESIAN_POINT ( 'NONE',  ( -18.86348425649999783, 1425.765603139730047, 225.9037505451979939 ) ) ;
#45743 = CARTESIAN_POINT ( 'NONE',  ( -16.03439795359999920, 1435.876017354450141, 148.8030225068980030 ) ) ;
#45744 = CARTESIAN_POINT ( 'NONE',  ( 17.84338787571921969, 1523.382868172864164, 180.3600277896298110 ) ) ;
#45745 = CARTESIAN_POINT ( 'NONE',  ( 16.20713703829999730, 1428.791430359930018, 190.9630754147979701 ) ) ;
#45746 = B_SPLINE_CURVE_WITH_KNOTS ( 'NONE', 5,
 ( #101248, #85019, #60403, #68813, #51434, #43045, #102376, #85564, #32961, #92316, #7767, #15587, #102914, #8313, #67702 ),
 .UNSPECIFIED., .F., .F.,
 ( 6, 3, 3, 3, 6 ),
 ( 0.000000000000000000, 0.2965494146486967186, 0.6162090003293669849, 0.8933765034092037149, 1.000000000000000000 ),
 .UNSPECIFIED. ) ;
#45748 = CARTESIAN_POINT ( 'NONE',  ( 4.329415431088969868, 1515.066066275059939, 207.4128929697799890 ) ) ;
#45747 = CARTESIAN_POINT ( 'NONE',  ( 0.5818187789159990908, 1408.933377948760153, 232.0310414966060080 ) ) ;
#45749 = DIRECTION ( 'NONE',  ( 0.000000000000000000, 0.000000000000000000, 1.000000000000000000 ) ) ;
#45750 = ORIENTED_EDGE ( 'NONE', *, *, #26231, .F. ) ;
#45751 = CARTESIAN_POINT ( 'NONE',  ( 12.32716646574370145, 1492.190914138330072, 209.5898718627249764 ) ) ;
#45752 = CARTESIAN_POINT ( 'NONE',  ( -10.78302954206379560, 1424.941192272636954, 142.1511525142338712 ) ) ;
#45753 = CARTESIAN_POINT ( 'NONE',  ( -24.01458399190000392, 1437.348856588880153, 212.3223689552080202 ) ) ;
#45754 = CARTESIAN_POINT ( 'NONE',  ( -4.927726023229999974, 1485.007261019890166, 198.2757096449989831 ) ) ;
#45755 = CARTESIAN_POINT ( 'NONE',  ( -18.52542037779999973, 1508.846193921429858, 229.9902974711980050 ) ) ;
#45756 = CARTESIAN_POINT ( 'NONE',  ( -3.062931151456462775, 1525.320827368860137, 241.4069010772119555 ) ) ;
#45757 = CARTESIAN_POINT ( 'NONE',  ( 12.10369631294569004, 1435.500269353037993, 151.1372464589562412 ) ) ;
#45758 = FACE_OUTER_BOUND ( 'NONE', #84597, .T. ) ;
#45759 = CARTESIAN_POINT ( 'NONE',  ( -33.36586802512182715, 1518.913060387330006, 201.9069332299493169 ) ) ;
#45760 = CARTESIAN_POINT ( 'NONE',  ( -5.169211785684260541, 1487.151124505699954, 220.0115435702170146 ) ) ;
#45761 = CARTESIAN_POINT ( 'NONE',  ( 8.129467950829999623, 1461.711574958590063, 228.8738014342989970 ) ) ;
#45763 = ADVANCED_FACE ( 'NONE', ( #12971 ), #16097, .F. ) ;
#45762 = CARTESIAN_POINT ( 'NONE',  ( -83.03943510906880476, 1383.774858932900088, 305.4843309025330313 ) ) ;
#45764 = AXIS2_PLACEMENT_3D ( 'NONE', #36139, #104436, #53507 ) ;
#45765 = CARTESIAN_POINT ( 'NONE',  ( -108.6615217476129942, 1383.758151187970270, 311.0749416052580045 ) ) ;
#45766 = CARTESIAN_POINT ( 'NONE',  ( -15.58634593545749780, 1506.535970897286916, 224.7451074557852735 ) ) ;
#45767 = CARTESIAN_POINT ( 'NONE',  ( 4.085147076609999317, 1428.826406437490050, 216.3215770461389980 ) ) ;
#45769 = ORIENTED_EDGE ( 'NONE', *, *, #45332, .F. ) ;
#45768 = CARTESIAN_POINT ( 'NONE',  ( -18.80814933326179883, 1444.056498683949940, 209.9870952034320055 ) ) ;
#45770 = CARTESIAN_POINT ( 'NONE',  ( -62.73150586050000044, 1380.013960346400154, 278.0159453995589729 ) ) ;
#45771 = CARTESIAN_POINT ( 'NONE',  ( 19.89197732033110100, 1508.728142334059839, 229.5184948967959997 ) ) ;
#45772 = EDGE_CURVE ( 'NONE', #50084, #82691, #13888, .T. ) ;
#45773 = EDGE_LOOP ( 'NONE', ( #18809, #18476, #93726, #60878 ) ) ;
#45774 = VERTEX_POINT ( 'NONE', #28424 ) ;
#45775 = CARTESIAN_POINT ( 'NONE',  ( -17.66551557795533611, 1521.951704408389787, 200.3426142980791269 ) ) ;
#45776 = CARTESIAN_POINT ( 'NONE',  ( -109.1650303699999967, 1384.945461312639964, 297.1327159909589568 ) ) ;
#45777 = CARTESIAN_POINT ( 'NONE',  ( 13.10420440301432876, 1443.028011217175617, 169.4053780122457340 ) ) ;
#45779 = CARTESIAN_POINT ( 'NONE',  ( -41.56052291839999668, 1443.484420489879994, 261.5689799724980276 ) ) ;
#45778 = CARTESIAN_POINT ( 'NONE',  ( 18.42977693619575064, 1413.445009768722457, 269.3801010515786629 ) ) ;
#45780 = DIRECTION ( 'NONE',  ( -0.9455185755993177343, 0.000000000000000000, 0.3255681544571540909 ) ) ;
#45781 = CARTESIAN_POINT ( 'NONE',  ( -11.57384147910000038, 1433.753257872449922, 151.2114678470979925 ) ) ;
#45782 = CARTESIAN_POINT ( 'NONE',  ( 28.77729888390000212, 1509.917985808229787, 206.0039979917680171 ) ) ;
#45783 = CARTESIAN_POINT ( 'NONE',  ( 11.65156729925299928, 1426.753153792180001, 138.0613224902349714 ) ) ;
#45784 = CARTESIAN_POINT ( 'NONE',  ( 6.512000794579999585, 1410.074001341329904, 186.9789373606980121 ) ) ;
#45785 = CARTESIAN_POINT ( 'NONE',  ( 17.07488731192357179, 1517.151704408390060, 205.4036014788801481 ) ) ;
#45786 = CARTESIAN_POINT ( 'NONE',  ( 1.700207153268540106, 1515.066230056300128, 213.4512571039940099 ) ) ;
#45787 = CARTESIAN_POINT ( 'NONE',  ( -11.78824854703250047, 1522.051704408389924, 206.8304425649369875 ) ) ;
#45788 = CARTESIAN_POINT ( 'NONE',  ( -9.818988496689140533, 1479.475980022059730, 215.4970472198330071 ) ) ;
#45789 = CARTESIAN_POINT ( 'NONE',  ( -9.129512800839998832, 1452.594250776829995, 151.6824240526980248 ) ) ;
#45791 = ORIENTED_EDGE ( 'NONE', *, *, #43929, .T. ) ;
#45790 = DIRECTION ( 'NONE',  ( -0.9824080081115912355, 0.000000000000000000, -0.1867471702549089174 ) ) ;
#45792 = ORIENTED_EDGE ( 'NONE', *, *, #17243, .F. ) ;
#45793 = CARTESIAN_POINT ( 'NONE',  ( -2.487923763832169843, 1508.731372606449895, 213.6767948502499905 ) ) ;
#45794 = VECTOR ( 'NONE', #34994, 1000.000000000000000 ) ;
#45795 = CARTESIAN_POINT ( 'NONE',  ( -5.549738551720860613, 1491.048330316449892, 185.8720954308039950 ) ) ;
#45796 = CARTESIAN_POINT ( 'NONE',  ( -10.92641736379999884, 1472.943607924629760, 270.2707055147980100 ) ) ;
#45797 = CARTESIAN_POINT ( 'NONE',  ( -1.491506560153233352, 1511.187213306747708, 175.5704429466618421 ) ) ;
#45798 = CARTESIAN_POINT ( 'NONE',  ( 9.470907091730000005, 1435.946707556030105, 153.1784963645979758 ) ) ;
#45799 = CARTESIAN_POINT ( 'NONE',  ( 13.72624666550403560, 1517.051704408389924, 222.4326881308259090 ) ) ;
#45800 = CARTESIAN_POINT ( 'NONE',  ( 4.328818125147670060, 1515.088876468540093, 210.3869497035339862 ) ) ;
#45801 = CARTESIAN_POINT ( 'NONE',  ( -13.95241924839999825, 1421.181435538830101, 227.8193205229979981 ) ) ;
#45802 = AXIS2_PLACEMENT_3D ( 'NONE', #75036, #8347, #25694 ) ;
#45803 = CARTESIAN_POINT ( 'NONE',  ( -6.609057684309999736, 1459.054199521789997, 216.6505361422790088 ) ) ;
#45804 = CARTESIAN_POINT ( 'NONE',  ( 7.859621272268051406, 1360.752827304597304, 210.6218459617030021 ) ) ;
#45805 = CARTESIAN_POINT ( 'NONE',  ( -43.84971736824440569, 1430.786840038769924, 268.8176679617099580 ) ) ;
#45806 = ORIENTED_EDGE ( 'NONE', *, *, #70687, .F. ) ;
#45807 = CARTESIAN_POINT ( 'NONE',  ( 25.70088977221606541, 1435.395012714986251, 135.4164360916261955 ) ) ;
#45808 = ORIENTED_EDGE ( 'NONE', *, *, #98959, .F. ) ;
#45809 = CARTESIAN_POINT ( 'NONE',  ( -7.323390445344999833, 1516.613712827999962, 210.2512321725070024 ) ) ;
#45810 = CYLINDRICAL_SURFACE ( 'NONE', #71662, 2.000000000000003109 ) ;
#45811 = DIRECTION ( 'NONE',  ( -0.7071067811865475727, -1.473812113707079158E-16, -0.7071067811865475727 ) ) ;
#45812 = CARTESIAN_POINT ( 'NONE',  ( -15.47784148859999931, 1410.406428057529865, 191.0438890190980032 ) ) ;
#45813 = CARTESIAN_POINT ( 'NONE',  ( 1.039074886133859899, 1495.944500751950045, 221.4190036890230147 ) ) ;
#45814 = VERTEX_POINT ( 'NONE', #80487 ) ;
#45815 = CARTESIAN_POINT ( 'NONE',  ( 4.253676957470000630, 1505.389161788490128, 221.1607250897990014 ) ) ;
#45816 =( BOUNDED_CURVE ( )  B_SPLINE_CURVE ( 3, ( #61844, #19797, #3588, #3040 ),
 .UNSPECIFIED., .F., .F. ) 
 B_SPLINE_CURVE_WITH_KNOTS ( ( 4, 4 ),
 ( 5.499719231357318883, 7.069826863760232172 ),
 .UNSPECIFIED. ) 
 CURVE ( )  GEOMETRIC_REPRESENTATION_ITEM ( )  RATIONAL_B_SPLINE_CURVE ( ( 1.000000000000000000, 0.8049001529976759217, 0.8049001529976759217, 1.000000000000000000 ) ) 
 REPRESENTATION_ITEM ( '' )  );
#45817 = CARTESIAN_POINT ( 'NONE',  ( 5.003848121975000396, 1517.005755693489846, 201.7875176594370146 ) ) ;
#45818 = CARTESIAN_POINT ( 'NONE',  ( 9.315703281059999341, 1470.272773095790171, 213.0620134152990204 ) ) ;
#45819 = CARTESIAN_POINT ( 'NONE',  ( -9.170040964561099628, 1440.195484865749904, 206.3355864816410019 ) ) ;
#45820 = ORIENTED_EDGE ( 'NONE', *, *, #102366, .T. ) ;
#45821 = CARTESIAN_POINT ( 'NONE',  ( -18.49698681803500122, 1413.444200939100028, 269.3800619411300090 ) ) ;
#45822 = CARTESIAN_POINT ( 'NONE',  ( -0.007128875282218469743, 1517.006509894990131, 208.3750284165899984 ) ) ;
#45823 = CARTESIAN_POINT ( 'NONE',  ( 3.677837710089999800E-15, 1426.566393376330097, 144.1938086916980239 ) ) ;
#45824 = CARTESIAN_POINT ( 'NONE',  ( 9.045129543558639185, 1434.758633656339953, 206.7452360523249979 ) ) ;
#45826 = ORIENTED_EDGE ( 'NONE', *, *, #57862, .T. ) ;
#45825 = CARTESIAN_POINT ( 'NONE',  ( -8.696701630030000629, 1367.135748871429996, 207.6218459616989946 ) ) ;
#45827 = ORIENTED_EDGE ( 'NONE', *, *, #73887, .T. ) ;
#45828 = CARTESIAN_POINT ( 'NONE',  ( 44.73266700618014369, 1447.687831433334622, 269.0000809591583106 ) ) ;
#45829 = CARTESIAN_POINT ( 'NONE',  ( 11.24295886237570130, 1471.530148615479902, 211.1614490031909952 ) ) ;
#45830 = CARTESIAN_POINT ( 'NONE',  ( 0.000000000000000000, 1511.187213306747708, 239.2297105040643714 ) ) ;
#45831 = CARTESIAN_POINT ( 'NONE',  ( -0.02513066005776489961, 1409.073703610690018, 185.8050026937470136 ) ) ;
#45832 = CARTESIAN_POINT ( 'NONE',  ( -18.43873448085470201, 1415.658863689850023, 207.5693132298119679 ) ) ;
#45833 = CARTESIAN_POINT ( 'NONE',  ( 7.717505752974999744, 1516.857914730730045, 216.8393517232070167 ) ) ;
#45834 = CARTESIAN_POINT ( 'NONE',  ( -13.90031192530000048, 1420.171540284829916, 222.0121128021980041 ) ) ;
#45835 = CARTESIAN_POINT ( 'NONE',  ( 12.60360202350000058, 1416.535385209630022, 223.3155814965980142 ) ) ;
#45836 = B_SPLINE_CURVE_WITH_KNOTS ( 'NONE', 5,
 ( #50956, #92939, #86196, #103545, #25166, #110293 ),
 .UNSPECIFIED., .F., .F.,
 ( 6, 6 ),
 ( -20.28790020619999979, -6.591324572240001345 ),
 .UNSPECIFIED. ) ;
#45837 = CARTESIAN_POINT ( 'NONE',  ( 8.987603741960001003, 1445.737909925099984, 185.1272997528979829 ) ) ;
#45838 = CARTESIAN_POINT ( 'NONE',  ( -0.01323705180209850014, 1516.939658295650133, 206.6356258303270010 ) ) ;
#45839 = ORIENTED_EDGE ( 'NONE', *, *, #30760, .F. ) ;
#45840 = CARTESIAN_POINT ( 'NONE',  ( -0.2232815667140019833, 1437.935022234890084, 227.7359842298990031 ) ) ;
#45841 = CARTESIAN_POINT ( 'NONE',  ( 1.493635725151659877, 1469.335982536970050, 182.7613696330639925 ) ) ;
#45842 = ORIENTED_EDGE ( 'NONE', *, *, #92607, .T. ) ;
#45843 = CARTESIAN_POINT ( 'NONE',  ( 3.238472285647973514, 1457.571195284309624, 228.6299524684958442 ) ) ;
#45844 = CARTESIAN_POINT ( 'NONE',  ( 24.50642912900270076, 1451.900605154380173, 137.2752955659460099 ) ) ;
#45845 = CARTESIAN_POINT ( 'NONE',  ( 16.18746221460043344, 1409.478339023977696, 224.9965714503316576 ) ) ;
#45846 = CARTESIAN_POINT ( 'NONE',  ( -33.87858360229999732, 1390.927706345010165, 218.8447143792689928 ) ) ;
#45847 = CARTESIAN_POINT ( 'NONE',  ( -9.775687243024277606, 1386.869824447039491, 218.1688999378142455 ) ) ;
#45848 = CARTESIAN_POINT ( 'NONE',  ( 21.99779377019999771, 1409.845345889329792, 206.2854409714980193 ) ) ;
#45849 = B_SPLINE_CURVE_WITH_KNOTS ( 'NONE', 3,
 ( #105397, #104290, #28690, #81273, #46060, #72360, #29777, #89683, #96445, #53925, #11345, #89139, #97004, #2963, #95888, #63425, #19148, #97543, #55012, #79108, #88060, #20267, #21351, #70729 ),
 .UNSPECIFIED., .F., .F.,
 ( 4, 2, 2, 2, 2, 2, 2, 2, 2, 2, 2, 4 ),
 ( -1.636478521365379857, -1.584985545560960052, -1.533441748506799929, -1.430342195185549947, -1.224163068651749953, -0.8182278975005480293, -0.4129906964137790570, -0.2064832563783289832, -0.1032404805529840708, -0.05160657342599406228, -0.02578454166961874350, 0.000000000000000000 ),
 .UNSPECIFIED. ) ;
#45850 = CARTESIAN_POINT ( 'NONE',  ( 32.02808312589922224, 1522.382868172863937, 219.9649204700462235 ) ) ;
#45851 = CARTESIAN_POINT ( 'NONE',  ( 17.60614391659999711, 1410.891372730630110, 225.2143943941980240 ) ) ;
#45852 = CARTESIAN_POINT ( 'NONE',  ( 10.50688481900000149, 1490.055410347190218, 204.4952978197489983 ) ) ;
#45853 = CARTESIAN_POINT ( 'NONE',  ( 0.8425900835067681172, 1451.065773967280165, 182.3319842116689813 ) ) ;
#45854 = CARTESIAN_POINT ( 'NONE',  ( 2.500000000000000000, 1439.522697744529978, 164.2180412838509938 ) ) ;
#45855 = CARTESIAN_POINT ( 'NONE',  ( -2.870951705914999597, 1517.111322026010157, 215.6844817927369888 ) ) ;
#45856 = CARTESIAN_POINT ( 'NONE',  ( 25.86984728598680050, 1447.207353507300013, 138.1976246213770310 ) ) ;
#45857 = VERTEX_POINT ( 'NONE', #39006 ) ;
#45858 = FACE_OUTER_BOUND ( 'NONE', #92519, .T. ) ;
#45859 = DIRECTION ( 'NONE',  ( -0.03489949676615768798, 0.9993908270168727626, 1.192931611642853769E-09 ) ) ;
#45860 = CARTESIAN_POINT ( 'NONE',  ( -0.3785191915233269699, 1409.088790390760096, 232.4100744083189909 ) ) ;
#45861 = AXIS2_PLACEMENT_3D ( 'NONE', #105803, #35269, #37480 ) ;
#45862 = FACE_OUTER_BOUND ( 'NONE', #84244, .T. ) ;
#45863 = CARTESIAN_POINT ( 'NONE',  ( -35.95901143404110201, 1450.034299295669825, 136.2432003471689939 ) ) ;
#45864 = CARTESIAN_POINT ( 'NONE',  ( 0.04210049761976375482, 1506.527232284500997, 231.1830146150431062 ) ) ;
#45865 = CARTESIAN_POINT ( 'NONE',  ( 1.509903313490000218E-14, 1461.407663418029870, 243.9198229339980060 ) ) ;
#45866 = CARTESIAN_POINT ( 'NONE',  ( 29.93311702910001415, 1467.353193293025925, 266.6089909078979190 ) ) ;
#45867 = CARTESIAN_POINT ( 'NONE',  ( 11.42063316640000004, 1433.075813662200062, 151.3550505031980151 ) ) ;
#45868 = CARTESIAN_POINT ( 'NONE',  ( -2.664535259099999805E-15, 1424.786834349990158, 209.1218459616989946 ) ) ;
#45869 = CARTESIAN_POINT ( 'NONE',  ( -17.57263815903020188, 1409.691670451539949, 195.6049335520870045 ) ) ;
#45870 = CARTESIAN_POINT ( 'NONE',  ( -22.21499610869999941, 1508.010819105329801, 225.8229464100980124 ) ) ;
#45871 = CARTESIAN_POINT ( 'NONE',  ( 10.93422485186690096, 1501.146248672419915, 205.7757054978180236 ) ) ;
#45872 = ORIENTED_EDGE ( 'NONE', *, *, #42783, .F. ) ;
#45873 = DIRECTION ( 'NONE',  ( 1.000000000000000000, 0.000000000000000000, 0.000000000000000000 ) ) ;
#45874 = CARTESIAN_POINT ( 'NONE',  ( 10.30255471828350089, 1462.241748833459951, 211.4138787017499794 ) ) ;
#45875 = CARTESIAN_POINT ( 'NONE',  ( -19.19677231483893109, 1485.580715045685565, 189.7096105684387339 ) ) ;
#45876 = CARTESIAN_POINT ( 'NONE',  ( -2.131986625842082095, 1526.000688113726937, 240.6925538243687015 ) ) ;
#45877 = CARTESIAN_POINT ( 'NONE',  ( 2.899728573290000444, 1474.727573286329971, 234.5030603628979975 ) ) ;
#45878 = CARTESIAN_POINT ( 'NONE',  ( 24.38832783640000201, 1430.357083400130023, 211.7627176485680138 ) ) ;
#45879 = CARTESIAN_POINT ( 'NONE',  ( -16.50400130224726780, 1525.907212628473644, 236.2546788475583242 ) ) ;
#45880 = CARTESIAN_POINT ( 'NONE',  ( -12.71706127659999908, 1509.357149952429836, 235.0231910820979806 ) ) ;
#45881 = CARTESIAN_POINT ( 'NONE',  ( -21.58355234741789985, 1383.851891895520112, 221.4751650834180055 ) ) ;
#45882 = CARTESIAN_POINT ( 'NONE',  ( -3.747768927200330058, 1508.879014986009906, 204.8753727076559983 ) ) ;
#45883 = CARTESIAN_POINT ( 'NONE',  ( 10.90933839120000037, 1409.294022878630130, 220.2163247819979972 ) ) ;
#45884 = CARTESIAN_POINT ( 'NONE',  ( 3.555115653736739510E-15, 1384.926148861439970, 209.1218459572589836 ) ) ;
#45885 = DIRECTION ( 'NONE',  ( -0.8771707857591169999, 0.03063147879954419839, 0.4792005061738630056 ) ) ;
#45887 = ORIENTED_EDGE ( 'NONE', *, *, #63092, .F. ) ;
#45886 = CARTESIAN_POINT ( 'NONE',  ( -10.73220944925208187, 1434.662271276825777, 151.9792366751727002 ) ) ;
#45888 = CARTESIAN_POINT ( 'NONE',  ( -1.210172143909999942, 1452.161324106529946, 183.6548506043980069 ) ) ;
#45889 = CARTESIAN_POINT ( 'NONE',  ( -10.21949078822098933, 1389.864309992940434, 202.1513456453452022 ) ) ;
#45890 = CARTESIAN_POINT ( 'NONE',  ( -3.018074008395929653, 1440.716223013230092, 157.2134785397810219 ) ) ;
#45891 = EDGE_CURVE ( 'NONE', #39734, #82569, #10397, .T. ) ;
#45893 = EDGE_LOOP ( 'NONE', ( #92882, #87724, #67823, #71810 ) ) ;
#45892 = CARTESIAN_POINT ( 'NONE',  ( -31.32941610406987820, 1525.856065479234758, 217.0550767640555136 ) ) ;
#45894 = CARTESIAN_POINT ( 'NONE',  ( 20.10526951509790194, 1430.877901956239839, 215.1856887477609916 ) ) ;
#45895 = ORIENTED_EDGE ( 'NONE', *, *, #101536, .T. ) ;
#45896 = CARTESIAN_POINT ( 'NONE',  ( -8.873922351719999213, 1388.797700485470159, 217.8009811287190018 ) ) ;
#45897 = CARTESIAN_POINT ( 'NONE',  ( 2.802893083669999896, 1485.536432262990047, 201.6817273870490226 ) ) ;
#45898 = CARTESIAN_POINT ( 'NONE',  ( -2.975637186240103205, 1509.038728186502112, 238.5532284157007155 ) ) ;
#45899 = CARTESIAN_POINT ( 'NONE',  ( 23.06762021731623591, 1409.889826804416771, 208.2909805245021175 ) ) ;
#45900 = CARTESIAN_POINT ( 'NONE',  ( -2.787468846669999945, 1432.903039033290042, 217.8476003497590057 ) ) ;
#45901 = CARTESIAN_POINT ( 'NONE',  ( 2.470168521978402421, 1523.382868172864164, 242.8787258963054398 ) ) ;
#45902 = CARTESIAN_POINT ( 'NONE',  ( 14.65346504764830193, 1409.424770662520132, 206.2342854941859969 ) ) ;
#45903 = CARTESIAN_POINT ( 'NONE',  ( 18.12392718799999969, 1425.124928798529936, 224.9480847838979969 ) ) ;
#45904 = CARTESIAN_POINT ( 'NONE',  ( -97.29371455280750070, 1385.213827748320227, 295.6673445477299538 ) ) ;
#45905 = DIRECTION ( 'NONE',  ( -0.009162664301380763279, -0.1630249973094845817, -0.9865793915520144619 ) ) ;
#45906 = CARTESIAN_POINT ( 'NONE',  ( -10.78871504700000017, 1416.913060387330006, 209.1218460627730167 ) ) ;
#45907 = CARTESIAN_POINT ( 'NONE',  ( 11.46755315091940020, 1491.645850675550037, 209.2229514265190176 ) ) ;
#45908 = ORIENTED_EDGE ( 'NONE', *, *, #10728, .T. ) ;
#45909 = ORIENTED_EDGE ( 'NONE', *, *, #27940, .F. ) ;
#45910 = CARTESIAN_POINT ( 'NONE',  ( -11.61894909938840037, 1415.258594621340080, 195.3027647187179809 ) ) ;
#45911 = CARTESIAN_POINT ( 'NONE',  ( 1.395568240770729940, 1496.886843748869978, 196.8164150919409963 ) ) ;
#45912 = CARTESIAN_POINT ( 'NONE',  ( 19.01867779685918336, 1468.113705757313028, 269.3842191184903072 ) ) ;
#45913 = CARTESIAN_POINT ( 'NONE',  ( 12.16878324720730120, 1427.280607052069854, 207.7518075308990149 ) ) ;
#45914 = CARTESIAN_POINT ( 'NONE',  ( -28.13497786889999830, 1508.084884472430076, 209.9324264222260013 ) ) ;
#45915 = CARTESIAN_POINT ( 'NONE',  ( 1.275935406860000176, 1416.411557770830086, 232.9857732278980222 ) ) ;
#45916 = CARTESIAN_POINT ( 'NONE',  ( -1.440135191710000040, 1453.598500553229997, 183.7985014944979980 ) ) ;
#45917 = CARTESIAN_POINT ( 'NONE',  ( -10.75519305779300616, 1363.664311205124022, 207.6218459616987673 ) ) ;
#45918 = CARTESIAN_POINT ( 'NONE',  ( 9.577041028380113730, 1507.356930867539177, 234.6859123068956876 ) ) ;
#45919 = EDGE_CURVE ( 'NONE', #15049, #91119, #72643, .T. ) ;
#45920 = B_SPLINE_CURVE_WITH_KNOTS ( 'NONE', 3,
 ( #69434, #77809, #84543, #68883, #102984, #26283, #60472, #86200, #9491, #1119 ),
 .UNSPECIFIED., .F., .F.,
 ( 4, 2, 2, 2, 4 ),
 ( 0.000000000000000000, 0.2500000000000000000, 0.5000000000000000000, 0.7500000000000000000, 1.000000000000000000 ),
 .UNSPECIFIED. ) ;
#45921 = CARTESIAN_POINT ( 'NONE',  ( 5.771149074885000729, 1516.616791731099966, 206.6334853027970269 ) ) ;
#45922 = DIRECTION ( 'NONE',  ( 0.000000000000000000, 0.000000000000000000, -1.000000000000000000 ) ) ;
#45923 = CARTESIAN_POINT ( 'NONE',  ( -8.296072169000000329, 1384.982551824029997, 218.7029005622489990 ) ) ;
#45924 = DIRECTION ( 'NONE',  ( 1.835183309750130004E-16, 1.000000000000000000, 1.599799320660000123E-19 ) ) ;
#45925 = CARTESIAN_POINT ( 'NONE',  ( 0.01496364964870140063, 1498.468111206090043, 197.7767147553989844 ) ) ;
#45926 = CARTESIAN_POINT ( 'NONE',  ( 2.798741260039999901, 1509.010794585729855, 238.1786444273980123 ) ) ;
#45927 = CARTESIAN_POINT ( 'NONE',  ( -104.8261132509999953, 1380.717247260959994, 300.0167969450589567 ) ) ;
#45928 = ORIENTED_EDGE ( 'NONE', *, *, #35168, .T. ) ;
#45929 = CARTESIAN_POINT ( 'NONE',  ( 28.68962088199999982, 1414.662824323530231, 264.4914085171980105 ) ) ;
#45930 = CARTESIAN_POINT ( 'NONE',  ( -26.16501621719999804, 1469.244469854430008, 206.7451401483880034 ) ) ;
#45932 = CARTESIAN_POINT ( 'NONE',  ( -33.91369120210140409, 1435.681798817159915, 134.0999999980979851 ) ) ;
#45931 = CARTESIAN_POINT ( 'NONE',  ( -3.544220692770000181, 1502.026769662330025, 181.1943011134980281 ) ) ;
#45933 = CARTESIAN_POINT ( 'NONE',  ( 1.625726771580663810, 1508.862184707432107, 180.0252976343047919 ) ) ;
#45934 = CARTESIAN_POINT ( 'NONE',  ( -14.70061896160000003, 1417.388462482530031, 244.5173668987980307 ) ) ;
#45935 = CARTESIAN_POINT ( 'NONE',  ( 2.423876137830000221, 1485.612096921090142, 220.0019078347989989 ) ) ;
#45936 = CARTESIAN_POINT ( 'NONE',  ( 1.363639811660000145, 1415.765555525229956, 232.8698637559979829 ) ) ;
#45937 = CARTESIAN_POINT ( 'NONE',  ( -23.56625796634288861, 1410.013281407407703, 208.7413938499740027 ) ) ;
#45938 = EDGE_LOOP ( 'NONE', ( #59200, #18074, #96046, #97514 ) ) ;
#45939 = CARTESIAN_POINT ( 'NONE',  ( -0.01233358747499999943, 1396.097901035330096, 197.1956428485979700 ) ) ;
#45940 = CARTESIAN_POINT ( 'NONE',  ( 14.78981622368054971, 1514.562529184305731, 225.3765129853291000 ) ) ;
#45941 = CARTESIAN_POINT ( 'NONE',  ( 11.79165948289999832, 1509.456730002229961, 236.8935920530979899 ) ) ;
#45942 = ORIENTED_EDGE ( 'NONE', *, *, #23098, .T. ) ;
#45943 = ORIENTED_EDGE ( 'NONE', *, *, #49612, .T. ) ;
#45944 = CARTESIAN_POINT ( 'NONE',  ( 9.359234811488938988, 1452.034566024799915, 210.3500916188470171 ) ) ;
#45945 = CARTESIAN_POINT ( 'NONE',  ( 5.046789308220000159, 1422.880134120949833, 194.5523403762989858 ) ) ;
#45946 = EDGE_LOOP ( 'NONE', ( #59303, #31869, #71599, #70118, #105213 ) ) ;
#45947 = CARTESIAN_POINT ( 'NONE',  ( -3.954134211063599746, 1507.541399951509902, 221.3757475976190108 ) ) ;
#45948 = CARTESIAN_POINT ( 'NONE',  ( -9.311098898702477200, 1418.495954698334117, 196.8548415329698003 ) ) ;
#45949 = CARTESIAN_POINT ( 'NONE',  ( 0.1923534468539999931, 1452.340213589330006, 183.2784190956980126 ) ) ;
#45950 = CARTESIAN_POINT ( 'NONE',  ( -2.509810337609999831, 1489.062117308030111, 236.1277042400979838 ) ) ;
#45951 = CARTESIAN_POINT ( 'NONE',  ( 16.85976061912576185, 1525.821544997590536, 236.1944305375347142 ) ) ;
#45952 = ORIENTED_EDGE ( 'NONE', *, *, #24333, .F. ) ;
#45953 = EDGE_CURVE ( 'NONE', #34173, #60549, #27287, .T. ) ;
#45954 = DIRECTION ( 'NONE',  ( 0.9064253123279890634, 0.3026617302209020366, -0.2945997797534770091 ) ) ;
#45955 = EDGE_CURVE ( 'NONE', #93518, #69912, #38916, .T. ) ;
#45956 = CARTESIAN_POINT ( 'NONE',  ( -13.15726444150010011, 1415.434635989089884, 221.3440418462499792 ) ) ;
#45957 = CARTESIAN_POINT ( 'NONE',  ( -108.9757583731840072, 1384.900984196950048, 297.1264776970670027 ) ) ;
#45958 = ORIENTED_EDGE ( 'NONE', *, *, #81537, .F. ) ;
#45959 = CARTESIAN_POINT ( 'NONE',  ( -6.559168674874999105, 1516.960844870249957, 204.1192525727769862 ) ) ;
#45960 = VERTEX_POINT ( 'NONE', #54206 ) ;
#45962 = EDGE_CURVE ( 'NONE', #19757, #98647, #62025, .T. ) ;
#45961 = CARTESIAN_POINT ( 'NONE',  ( 11.85443421315619972, 1431.523992928169946, 149.9226482103390197 ) ) ;
#45963 = CARTESIAN_POINT ( 'NONE',  ( 4.487249753905000027, 1509.038615934169911, 212.6094383991670043 ) ) ;
#45964 = ORIENTED_EDGE ( 'NONE', *, *, #103472, .T. ) ;
#45965 = ORIENTED_EDGE ( 'NONE', *, *, #62581, .F. ) ;
#45966 = CARTESIAN_POINT ( 'NONE',  ( -11.01596213409299985, 1481.419441981669934, 209.0719341547870158 ) ) ;
#45967 = EDGE_CURVE ( 'NONE', #84504, #102807, #14904, .T. ) ;
#45968 = CARTESIAN_POINT ( 'NONE',  ( -3.763579503338020160, 1508.126400519680146, 220.7366911303400059 ) ) ;
#45969 = CARTESIAN_POINT ( 'NONE',  ( 6.500069621292889899, 1497.924601430119992, 198.3228313574259971 ) ) ;
#45970 = AXIS2_PLACEMENT_3D ( 'NONE', #72169, #64865, #71634 ) ;
#45971 = ADVANCED_FACE ( 'NONE', ( #33359 ), #75133, .T. ) ;
#45972 = CARTESIAN_POINT ( 'NONE',  ( -4.157642293380810372, 1469.875985805179880, 218.3513889513289996 ) ) ;
#45973 = DIRECTION ( 'NONE',  ( 1.755985294532464991E-16, -1.000000000000000000, 1.338183447452830017E-16 ) ) ;
#45974 = CARTESIAN_POINT ( 'NONE',  ( 0.4896011454402059981, 1407.928426433459890, 270.2927087822229737 ) ) ;
#45975 = CARTESIAN_POINT ( 'NONE',  ( 9.176034321767531310, 1450.127176980830200, 208.3686583938580270 ) ) ;
#45976 = CARTESIAN_POINT ( 'NONE',  ( -12.55806607928250074, 1501.992048856159954, 211.3070401664170106 ) ) ;
#45977 = CARTESIAN_POINT ( 'NONE',  ( 11.59635154200000251, 1493.084219504590010, 213.4865999382489861 ) ) ;
#45978 = DIRECTION ( 'NONE',  ( 0.9858563016923833633, 0.000000000000000000, 0.1675928173085483863 ) ) ;
#45979 = CARTESIAN_POINT ( 'NONE',  ( 3.552713678799999608E-15, 1507.551704408389924, 209.1218459616989946 ) ) ;
#45980 = ADVANCED_FACE ( 'NONE', ( #58043 ), #109098, .T. ) ;
#45982 = CARTESIAN_POINT ( 'NONE',  ( 16.15031516230000008, 1471.311257370829935, 195.1295159150980112 ) ) ;
#45981 = CARTESIAN_POINT ( 'NONE',  ( -16.38073507929999906, 1503.849976525089915, 209.2714441331769990 ) ) ;
#45983 = CARTESIAN_POINT ( 'NONE',  ( -36.56818187795897757, 1379.727990715524356, 223.6839165922986297 ) ) ;
#45984 = CARTESIAN_POINT ( 'NONE',  ( 17.90387844572719800, 1420.535267245019895, 225.0886834623109962 ) ) ;
#45985 = CARTESIAN_POINT ( 'NONE',  ( -6.396410548735000035, 1511.623805160490065, 201.6463516768869795 ) ) ;
#45986 = VERTEX_POINT ( 'NONE', #18757 ) ;
#45987 = CARTESIAN_POINT ( 'NONE',  ( 23.03655028440000052, 1423.631548418229841, 255.3819207742980097 ) ) ;
#45988 = DIRECTION ( 'NONE',  ( -0.6736849260863841948, 0.000000000000000000, 0.7390186874254148774 ) ) ;
#45989 = VECTOR ( 'NONE', #55515, 1000.000000000000000 ) ;
#45990 = CARTESIAN_POINT ( 'NONE',  ( -63.63727237520100743, 1385.049170780109989, 286.7708433928359568 ) ) ;
#45991 = DIRECTION ( 'NONE',  ( -1.000000000000000000, 0.000000000000000000, 0.000000000000000000 ) ) ;
#45992 = CARTESIAN_POINT ( 'NONE',  ( 4.212150227310000439, 1506.735180723689837, 220.0177425982989803 ) ) ;
#45993 = CARTESIAN_POINT ( 'NONE',  ( -15.15570824359999946, 1415.677402261749876, 210.8787115431290147 ) ) ;
#45994 = EDGE_CURVE ( 'NONE', #92059, #82777, #72999, .T. ) ;
#45996 = ORIENTED_EDGE ( 'NONE', *, *, #33188, .T. ) ;
#45995 = CARTESIAN_POINT ( 'NONE',  ( -16.50063655363959825, 1419.653847773739926, 209.2961467218439964 ) ) ;
#45997 = LINE ( 'NONE', #61168, #44189 ) ;
#45998 = CARTESIAN_POINT ( 'NONE',  ( -24.02756305619999821, 1444.331317782170117, 212.2090029378380223 ) ) ;
#45999 = DIRECTION ( 'NONE',  ( 0.000000000000000000, 0.000000000000000000, -1.000000000000000000 ) ) ;
#46000 = DIRECTION ( 'NONE',  ( -0.8642610224696035681, -0.000000000000000000, -0.5030436214085171054 ) ) ;
#46001 = CARTESIAN_POINT ( 'NONE',  ( 14.28353071843499933, 1513.113451381389950, 224.7690913644670161 ) ) ;
#46002 = CARTESIAN_POINT ( 'NONE',  ( -12.01638188689999964, 1440.881463209799904, 187.8051711800980001 ) ) ;
#46003 = EDGE_CURVE ( 'NONE', #328, #86968, #14949, .T. ) ;
#46004 = CARTESIAN_POINT ( 'NONE',  ( 12.99126122772529968, 1509.366722754649800, 181.4462959118600054 ) ) ;
#46005 = CARTESIAN_POINT ( 'NONE',  ( 2.922712066004659714, 1412.240002439039927, 231.7135113672919999 ) ) ;
#46006 = CARTESIAN_POINT ( 'NONE',  ( 17.16388877745050934, 1523.678648413191695, 179.6262614458745190 ) ) ;
#46007 = EDGE_CURVE ( 'NONE', #31217, #95667, #78128, .T. ) ;
#46008 = CARTESIAN_POINT ( 'NONE',  ( 15.07806947409999943, 1412.745289768429984, 227.5463952181980005 ) ) ;
#46009 = CYLINDRICAL_SURFACE ( 'NONE', #67634, 1.000000000000000888 ) ;
#46010 = CARTESIAN_POINT ( 'NONE',  ( -16.13112951687100249, 1459.078801168009932, 230.3616389713189960 ) ) ;
#46011 = CARTESIAN_POINT ( 'NONE',  ( -7.338753868364999988, 1517.184383877180153, 206.8309596656170015 ) ) ;
#46012 = CARTESIAN_POINT ( 'NONE',  ( 44.11426962409999675, 1429.859647049230034, 268.2740853901979676 ) ) ;
#46013 = CARTESIAN_POINT ( 'NONE',  ( -18.82531593190000052, 1410.932625384329867, 223.3083523618979882 ) ) ;
#46014 = AXIS2_PLACEMENT_3D ( 'NONE', #4779, #31086, #38925 ) ;
#46015 = CARTESIAN_POINT ( 'NONE',  ( 18.77495633519999885, 1435.298717977980004, 145.7151766910979802 ) ) ;
#46016 = EDGE_CURVE ( 'NONE', #103324, #11383, #3118, .T. ) ;
#46018 = B_SPLINE_CURVE_WITH_KNOTS ( 'NONE', 3,
 ( #31814, #23406, #57044, #63788, #49190, #21730 ),
 .UNSPECIFIED., .F., .F.,
 ( 4, 2, 4 ),
 ( 1.000070671099200032E-06, 0.09529849184413820284, 0.1904887692805259936 ),
 .UNSPECIFIED. ) ;
#46017 = CARTESIAN_POINT ( 'NONE',  ( 19.55758403639999798, 1488.589959684130008, 189.8994889324980022 ) ) ;
#46019 = CARTESIAN_POINT ( 'NONE',  ( 29.78200767887302547, 1510.000544160475329, 209.1355521330470140 ) ) ;
#46020 = CARTESIAN_POINT ( 'NONE',  ( -14.25010227119279982, 1379.583597535630133, 207.8942344209849864 ) ) ;
#46021 = CARTESIAN_POINT ( 'NONE',  ( -15.90377527599999929, 1418.369030882129891, 226.9588463030979710 ) ) ;
#46022 = CARTESIAN_POINT ( 'NONE',  ( 12.48513440536379981, 1427.066873444910016, 206.5219089466239950 ) ) ;
#46023 = DIRECTION ( 'NONE',  ( 0.9786619618251627406, 0.000000000000000000, -0.2054769195713317953 ) ) ;
#46024 = CARTESIAN_POINT ( 'NONE',  ( -12.07987659813839976, 1408.300217416430087, 215.9313631298179814 ) ) ;
#46025 = CARTESIAN_POINT ( 'NONE',  ( -16.32615623849999764, 1416.524502645009989, 209.0932030950310150 ) ) ;
#46026 = CARTESIAN_POINT ( 'NONE',  ( -16.37832153215809328, 1409.485005020973631, 193.4350318287646644 ) ) ;
#46027 = CARTESIAN_POINT ( 'NONE',  ( 0.000000000000000000, 1518.913060387330006, 209.1218459616979999 ) ) ;
#46028 = CARTESIAN_POINT ( 'NONE',  ( 12.06142474169999979, 1433.903238137760127, 146.5968191413979866 ) ) ;
#46029 = CARTESIAN_POINT ( 'NONE',  ( -30.78500370360000105, 1435.572563320330119, 135.1635738117979884 ) ) ;
#46030 = DIRECTION ( 'NONE',  ( -0.000000000000000000, -1.000000000000000000, -0.000000000000000000 ) ) ;
#46031 = ORIENTED_EDGE ( 'NONE', *, *, #29537, .F. ) ;
#46032 = CARTESIAN_POINT ( 'NONE',  ( 7.190299821260000002, 1478.329013068389941, 201.1569836108390064 ) ) ;
#46033 = CARTESIAN_POINT ( 'NONE',  ( -11.75869035857540013, 1522.051704408389924, 190.9442076533970010 ) ) ;
#46034 = FACE_OUTER_BOUND ( 'NONE', #66616, .T. ) ;
#46035 = CARTESIAN_POINT ( 'NONE',  ( -4.675540975309999681, 1462.620895424390028, 200.5633310686890241 ) ) ;
#46036 = CARTESIAN_POINT ( 'NONE',  ( -17.11714618744633754, 1443.086052842848630, 162.7561046190426737 ) ) ;
#46037 = VECTOR ( 'NONE', #48616, 1000.000000000000000 ) ;
#46038 = CARTESIAN_POINT ( 'NONE',  ( -44.82664241559999851, 1451.165400018629953, 266.7159563179980069 ) ) ;
#46039 = CARTESIAN_POINT ( 'NONE',  ( -11.72765336777909972, 1481.328017084940029, 210.7793835027030127 ) ) ;
#46040 = CARTESIAN_POINT ( 'NONE',  ( -17.30126322264801786, 1523.462669333490567, 237.3930845918954731 ) ) ;
#46041 = CARTESIAN_POINT ( 'NONE',  ( -24.90809350219999985, 1507.935970483929850, 220.3557327460979991 ) ) ;
#46042 = CARTESIAN_POINT ( 'NONE',  ( 7.559010162000579847, 1510.805212306241174, 203.6254155100018011 ) ) ;
#46043 = CARTESIAN_POINT ( 'NONE',  ( -43.65248483671320656, 1384.999294573369980, 216.7159599902390141 ) ) ;
#46044 = CARTESIAN_POINT ( 'NONE',  ( -5.329878543928120216, 1374.946430637010053, 214.8576637461130190 ) ) ;
#46045 = CARTESIAN_POINT ( 'NONE',  ( 21.32980800760000051, 1509.431603210329968, 227.7697269125980029 ) ) ;
#46046 = CARTESIAN_POINT ( 'NONE',  ( 15.05032900819999853, 1485.054733288129910, 223.8431641993980179 ) ) ;
#46047 = EDGE_CURVE ( 'NONE', #100464, #87329, #11496, .T. ) ;
#46048 = CARTESIAN_POINT ( 'NONE',  ( 2.500000000000000000, 1419.524771318244348, 137.0999999980979851 ) ) ;
#46050 = EDGE_LOOP ( 'NONE', ( #103566, #83937, #61525 ) ) ;
#46049 = CYLINDRICAL_SURFACE ( 'NONE', #9052, 0.9999999999999988898 ) ;
#46051 = CARTESIAN_POINT ( 'NONE',  ( -8.156249721700000066, 1384.928229602200190, 199.6467685838189823 ) ) ;
#46052 = CARTESIAN_POINT ( 'NONE',  ( -8.888245507000000669E-15, 1414.050155615230096, 164.5351017311979831 ) ) ;
#46053 = EDGE_CURVE ( 'NONE', #27764, #103213, #88327, .T. ) ;
#46054 = CARTESIAN_POINT ( 'NONE',  ( -10.10084594930000002, 1498.671139517090069, 214.6853310067990037 ) ) ;
#46055 = CARTESIAN_POINT ( 'NONE',  ( -12.78667948450000047, 1416.822690122329959, 195.3262913363980147 ) ) ;
#46056 = CARTESIAN_POINT ( 'NONE',  ( -2.140910185329999660, 1421.480997455049874, 193.7252687417990273 ) ) ;
#46057 = CARTESIAN_POINT ( 'NONE',  ( 23.47111472610000149, 1410.227925161630083, 211.2550682413580034 ) ) ;
#46058 = CARTESIAN_POINT ( 'NONE',  ( -106.5125067552479976, 1391.913060387289988, 305.2240569073479719 ) ) ;
#46059 = CARTESIAN_POINT ( 'NONE',  ( 18.68388892448549754, 1457.534866238390123, 220.6832095082359899 ) ) ;
#46060 = CARTESIAN_POINT ( 'NONE',  ( -5.383045099570169967, 1431.499107093909970, 154.5620711115419965 ) ) ;
#46062 = CARTESIAN_POINT ( 'NONE',  ( -12.00444414999999942, 1381.312822588570043, 202.5161199644090289 ) ) ;
#46061 = CARTESIAN_POINT ( 'NONE',  ( 3.281831451650000009, 1466.303209849290170, 198.5678428638989885 ) ) ;
#46063 = CARTESIAN_POINT ( 'NONE',  ( -5.263803380099999707, 1391.914765747090087, 203.7221189175089933 ) ) ;
#46064 = CARTESIAN_POINT ( 'NONE',  ( -123.7789942035696811, 1376.302340817388313, 298.5517755817839998 ) ) ;
#46065 = DIRECTION ( 'NONE',  ( 1.000000000000000000, 0.000000000000000000, 0.000000000000000000 ) ) ;
#46066 = CARTESIAN_POINT ( 'NONE',  ( 13.63294200170024162, 1492.115741768783209, 192.2627525536992152 ) ) ;
#46067 = CIRCLE ( 'NONE', #103241, 26.99999999999999645 ) ;
#46068 = CARTESIAN_POINT ( 'NONE',  ( -1.110282348042360034, 1420.248281415159909, 184.7133612920480061 ) ) ;
#46069 = ADVANCED_FACE ( 'NONE', ( #88202 ), #47296, .T. ) ;
#46070 = CARTESIAN_POINT ( 'NONE',  ( -2.296124889065000119, 1516.677239312369920, 204.5136991508470032 ) ) ;
#46071 = CARTESIAN_POINT ( 'NONE',  ( 13.38054884590909843, 1507.805480882780103, 233.0860310194200054 ) ) ;
#46072 = CARTESIAN_POINT ( 'NONE',  ( -17.39085484616060029, 1485.731293066659873, 188.3208887600499963 ) ) ;
#46073 = CARTESIAN_POINT ( 'NONE',  ( 11.80625193467720102, 1501.815294225020125, 212.7003682637139832 ) ) ;
#46074 = CARTESIAN_POINT ( 'NONE',  ( -11.98171406608951628, 1421.814709082018453, 210.6443979596248539 ) ) ;
#46077 = VERTEX_POINT ( 'NONE', #97692 ) ;
#46076 = CARTESIAN_POINT ( 'NONE',  ( -68.06332100059638890, 1379.746517069849915, 279.5343399889710554 ) ) ;
#46075 = AXIS2_PLACEMENT_3D ( 'NONE', #31825, #109643, #6626 ) ;
#46078 = ORIENTED_EDGE ( 'NONE', *, *, #60523, .F. ) ;
#46079 = CARTESIAN_POINT ( 'NONE',  ( 29.14447581790000186, 1509.936536293530253, 213.8494348557679814 ) ) ;
#46080 = ORIENTED_EDGE ( 'NONE', *, *, #74972, .T. ) ;
#46081 = CARTESIAN_POINT ( 'NONE',  ( -105.6951163859999951, 1378.913064648980026, 305.0952293404590137 ) ) ;
#46082 = CARTESIAN_POINT ( 'NONE',  ( 1.383993012819999979, 1414.983771848829747, 191.7538275864980051 ) ) ;
#46084 = CARTESIAN_POINT ( 'NONE',  ( 15.73440523137610292, 1409.488452722919874, 192.6548270638369900 ) ) ;
#46083 = CARTESIAN_POINT ( 'NONE',  ( 0.7772817352909999755, 1427.305457135430061, 123.0297916884979941 ) ) ;
#46085 = CARTESIAN_POINT ( 'NONE',  ( 11.97827956719999776, 1441.604408666619975, 150.7817505876979851 ) ) ;
#46086 = EDGE_CURVE ( 'NONE', #66505, #103394, #1455, .T. ) ;
#46087 = CARTESIAN_POINT ( 'NONE',  ( -25.75378511762339784, 1451.133596423730069, 136.7593279701780205 ) ) ;
#46088 = CARTESIAN_POINT ( 'NONE',  ( -105.7995319784910038, 1378.913060387259975, 304.3206059282480282 ) ) ;
#46089 = CARTESIAN_POINT ( 'NONE',  ( 13.87080890250000031, 1409.899448471030155, 227.8810934041980261 ) ) ;
#46090 = CARTESIAN_POINT ( 'NONE',  ( 12.51041186362150093, 1501.167594044880161, 211.3998864982009991 ) ) ;
#46091 =( NAMED_UNIT ( * ) SI_UNIT ( $, .STERADIAN. ) SOLID_ANGLE_UNIT ( ) );
#46092 = CARTESIAN_POINT ( 'NONE',  ( 7.337153768115000751, 1517.119374999550018, 212.3815752680669959 ) ) ;
#46093 = CARTESIAN_POINT ( 'NONE',  ( 40.98974505593590578, 1446.927689382389872, 134.0999999985409943 ) ) ;
#46094 = CARTESIAN_POINT ( 'NONE',  ( -20.44228942490000023, 1485.240733021890037, 206.1051096756690129 ) ) ;
#46095 = ORIENTED_EDGE ( 'NONE', *, *, #4288, .T. ) ;
#46096 = CARTESIAN_POINT ( 'NONE',  ( 20.81805214273520122, 1457.016357340710101, 206.8941968723059972 ) ) ;
#46097 = MANIFOLD_SOLID_BREP ( 'Stock-MAS-682-1', #34206 ) ;
#46098 = EDGE_CURVE ( 'NONE', #8434, #106669, #88753, .T. ) ;
#46099 = CARTESIAN_POINT ( 'NONE',  ( -16.89232299734799980, 1526.349689584397083, 234.8971085836487873 ) ) ;
#46100 = VERTEX_POINT ( 'NONE', #46218 ) ;
#46101 = VERTEX_POINT ( 'NONE', #79256 ) ;
#46102 = ORIENTED_EDGE ( 'NONE', *, *, #44668, .T. ) ;
#46103 = CARTESIAN_POINT ( 'NONE',  ( -7.750386781025000893, 1513.342361861140034, 216.5914658619369959 ) ) ;
#46104 = CARTESIAN_POINT ( 'NONE',  ( 4.492546581380000958, 1453.878649273890005, 217.3453973181289882 ) ) ;
#46105 = CARTESIAN_POINT ( 'NONE',  ( 15.60193763504558007, 1451.131520225134182, 149.3236191048951582 ) ) ;
#46106 = AXIS2_PLACEMENT_3D ( 'NONE', #74659, #6876, #75208 ) ;
#46107 = CARTESIAN_POINT ( 'NONE',  ( -8.581520137690000993, 1384.906045364150032, 218.6697283336690134 ) ) ;
#46108 = CARTESIAN_POINT ( 'NONE',  ( 9.751945027609998817, 1462.536696320589954, 208.9120314007480204 ) ) ;
#46109 = CARTESIAN_POINT ( 'NONE',  ( -12.64088754379999990, 1379.240986521519744, 208.6656973887710080 ) ) ;
#46110 = CARTESIAN_POINT ( 'NONE',  ( -66.32605177295688748, 1379.742644928997834, 275.0426332078492351 ) ) ;
#46111 = CARTESIAN_POINT ( 'NONE',  ( 4.226171528248299225, 1446.259724416819836, 166.0438435565190218 ) ) ;
#46112 = ADVANCED_FACE ( 'NONE', ( #79810 ), #69552, .T. ) ;
#46113 = CARTESIAN_POINT ( 'NONE',  ( -0.04583980512609999586, 1508.666040292029948, 238.1629808674979927 ) ) ;
#46114 = ORIENTED_EDGE ( 'NONE', *, *, #85304, .T. ) ;
#46115 = CARTESIAN_POINT ( 'NONE',  ( -3.269184946495000244, 1516.940296199220029, 206.8376465686969823 ) ) ;
#46116 = ORIENTED_EDGE ( 'NONE', *, *, #58207, .F. ) ;
#46117 = CARTESIAN_POINT ( 'NONE',  ( 30.00383565071140168, 1440.913060387330006, 252.1044819011040090 ) ) ;
#46118 = B_SPLINE_CURVE_WITH_KNOTS ( 'NONE', 5,
 ( #88377, #98964, #48030, #97860, #11667, #55897, #30104, #73796, #5467 ),
 .UNSPECIFIED., .F., .F.,
 ( 6, 3, 6 ),
 ( 0.000000000000000000, 0.5000000000000000000, 1.000000000000000000 ),
 .UNSPECIFIED. ) ;
#46119 = CARTESIAN_POINT ( 'NONE',  ( 11.39627603927229949, 1478.751622603650048, 206.3037616009159763 ) ) ;
#46120 = EDGE_CURVE ( 'NONE', #36440, #58638, #19244, .T. ) ;
#46121 = VERTEX_POINT ( 'NONE', #81979 ) ;
#46122 = CARTESIAN_POINT ( 'NONE',  ( -7.507422039880669473, 1508.880866118479844, 202.9817282009999815 ) ) ;
#46123 = CARTESIAN_POINT ( 'NONE',  ( -14.49476690930000089, 1409.419228801430108, 191.6021942292979929 ) ) ;
#46124 = CARTESIAN_POINT ( 'NONE',  ( -18.00826777305211124, 1508.456934164587210, 211.8767047476162020 ) ) ;
#46126 = CARTESIAN_POINT ( 'NONE',  ( 14.89373265416590009, 1512.150422497879845, 196.7424079551790044 ) ) ;
#46125 = CARTESIAN_POINT ( 'NONE',  ( 21.13734888319999783, 1496.938803861589804, 209.1218459616989946 ) ) ;
#46127 = CARTESIAN_POINT ( 'NONE',  ( -9.390527344411388810, 1437.694362696060125, 212.1689238372079842 ) ) ;
#46128 = CARTESIAN_POINT ( 'NONE',  ( -5.949235733474299792, 1511.655824793919919, 200.8322428604340075 ) ) ;
#46129 = CARTESIAN_POINT ( 'NONE',  ( -11.87742750661531410, 1433.145441672523930, 147.6581217067710554 ) ) ;
#46130 = CARTESIAN_POINT ( 'NONE',  ( -11.94102939159999899, 1433.615517387009959, 149.9804957299980117 ) ) ;
#46131 = CARTESIAN_POINT ( 'NONE',  ( -7.482302563030000186, 1508.669737789789906, 219.1818476679989942 ) ) ;
#46132 = ADVANCED_FACE ( 'NONE', ( #56803 ), #93004, .T. ) ;
#46134 = CARTESIAN_POINT ( 'NONE',  ( -3.161014919395765510, 1370.090064437274350, 207.9054318704831985 ) ) ;
#46133 = DIRECTION ( 'NONE',  ( 0.01398399556878729237, -0.01017778278299899530, 0.9998504191155564991 ) ) ;
#46135 = VECTOR ( 'NONE', #24, 1000.000000000000000 ) ;
#46136 = B_SPLINE_CURVE_WITH_KNOTS ( 'NONE', 5,
 ( #11236, #25791, #52135, #9553, #35315, #30948, #7401, #82465, #100358 ),
 .UNSPECIFIED., .F., .F.,
 ( 6, 3, 6 ),
 ( 0.000000000000000000, 0.5198849050576186404, 1.000000000000000000 ),
 .UNSPECIFIED. ) ;
#46137 = CARTESIAN_POINT ( 'NONE',  ( 5.780232077335000440, 1516.760434454289907, 216.4486414936069991 ) ) ;
#46138 = EDGE_CURVE ( 'NONE', #71548, #46325, #35338, .T. ) ;
#46139 = CARTESIAN_POINT ( 'NONE',  ( -2.143765237719136518, 1525.848196786131211, 241.3832888336301323 ) ) ;
#46140 = EDGE_CURVE ( 'NONE', #89941, #22899, #109961, .T. ) ;
#46141 = CARTESIAN_POINT ( 'NONE',  ( 5.784678349096259886, 1511.501844456730169, 217.8912146184260052 ) ) ;
#46142 = CARTESIAN_POINT ( 'NONE',  ( 2.686321661465695065, 1516.547182400040128, 216.8312149107646576 ) ) ;
#46143 = CARTESIAN_POINT ( 'NONE',  ( 3.268235720634999897, 1516.890356958860139, 211.9874346545169885 ) ) ;
#46144 = CARTESIAN_POINT ( 'NONE',  ( -19.92213876099999936, 1452.807100929029957, 208.8541967413179918 ) ) ;
#46145 = CARTESIAN_POINT ( 'NONE',  ( -3.002568591853699953, 1483.560948544299890, 198.8865183318360152 ) ) ;
#46147 = VERTEX_POINT ( 'NONE', #94243 ) ;
#46146 = CARTESIAN_POINT ( 'NONE',  ( -106.4193208100000021, 1384.931129459059775, 311.3263713972589812 ) ) ;
#46148 = DIRECTION ( 'NONE',  ( -1.000000000000000000, 0.000000000000000000, 0.000000000000000000 ) ) ;
#46149 = CARTESIAN_POINT ( 'NONE',  ( 30.53571888369999954, 1442.873932100699903, 240.1260121790979838 ) ) ;
#46150 = DIRECTION ( 'NONE',  ( -0.6736849260863841948, 0.000000000000000000, 0.7390186874254148774 ) ) ;
#46151 = CARTESIAN_POINT ( 'NONE',  ( -14.01525947340000045, 1415.677402202029953, 204.0303135798690164 ) ) ;
#46152 = CARTESIAN_POINT ( 'NONE',  ( -0.2745515581962330032, 1507.636705584799984, 237.3923196597329763 ) ) ;
#46153 = CARTESIAN_POINT ( 'NONE',  ( -21.94178583340000088, 1452.077510002930239, 222.2803297732980070 ) ) ;
#46155 = CARTESIAN_POINT ( 'NONE',  ( 5.360347202541429823, 1422.243392962449889, 144.1217039821420087 ) ) ;
#46154 = CARTESIAN_POINT ( 'NONE',  ( -23.00040066099999692, 1457.437332268930049, 219.0071613830780279 ) ) ;
#46156 = CARTESIAN_POINT ( 'NONE',  ( 0.04749300429670000323, 1488.809466528630082, 187.8102763656980017 ) ) ;
#46157 = CARTESIAN_POINT ( 'NONE',  ( -106.3587827582539944, 1381.411344002460055, 309.3065060124769730 ) ) ;
#46158 = ORIENTED_EDGE ( 'NONE', *, *, #91968, .T. ) ;
#46159 = CARTESIAN_POINT ( 'NONE',  ( -4.041472511874999896, 1516.858649670339901, 205.0922732913970208 ) ) ;
#46160 = CARTESIAN_POINT ( 'NONE',  ( 1.779019444429999819, 1405.741471815129898, 267.8527215162980042 ) ) ;
#46161 = ADVANCED_FACE ( 'NONE', ( #17518 ), #42068, .T. ) ;
#46162 = CARTESIAN_POINT ( 'NONE',  ( 1.114108910750000181, 1515.531799303389789, 213.2143613245789879 ) ) ;
#46163 = CIRCLE ( 'NONE', #83594, 4.941741911590025182 ) ;
#46164 = AXIS2_PLACEMENT_3D ( 'NONE', #64811, #28982, #22190 ) ;
#46165 = CARTESIAN_POINT ( 'NONE',  ( 12.89647794391319913, 1471.158836576110161, 270.0761327948309827 ) ) ;
#46166 = CARTESIAN_POINT ( 'NONE',  ( -15.36549427709999982, 1420.352425059129928, 229.0210324418980008 ) ) ;
#46167 =( BOUNDED_CURVE ( )  B_SPLINE_CURVE ( 3, ( #80131, #53871, #96948, #88545 ),
 .UNSPECIFIED., .F., .T. ) 
 B_SPLINE_CURVE_WITH_KNOTS ( ( 4, 4 ),
 ( 1.037086443313566031, 2.104505668239319949 ),
 .UNSPECIFIED. ) 
 CURVE ( )  GEOMETRIC_REPRESENTATION_ITEM ( )  RATIONAL_B_SPLINE_CURVE ( ( 1.000000000000000000, 0.9072838702658839738, 0.9072838702658839738, 1.000000000000000000 ) ) 
 REPRESENTATION_ITEM ( '' )  );
#46168 = CARTESIAN_POINT ( 'NONE',  ( 2.330134122034449806, 1515.551704408389924, 205.2922258479440245 ) ) ;
#46169 = CARTESIAN_POINT ( 'NONE',  ( -44.56994949339100742, 1440.913060401099983, 264.9967186962099959 ) ) ;
#46170 = CARTESIAN_POINT ( 'NONE',  ( 1.590343439599928743, 1450.573397075630282, 154.2772178510776655 ) ) ;
#46171 = CARTESIAN_POINT ( 'NONE',  ( 8.648691725468450997, 1514.216922324319739, 214.7715657207340030 ) ) ;
#46172 = CARTESIAN_POINT ( 'NONE',  ( 0.5703798115540580360, 1450.893142285409795, 154.7888392056570126 ) ) ;
#46173 = CARTESIAN_POINT ( 'NONE',  ( 3.775315583779999873, 1507.374707175490130, 220.2027399556990019 ) ) ;
#46174 = CARTESIAN_POINT ( 'NONE',  ( 19.30499357109350811, 1478.515812373770359, 190.2772978286499495 ) ) ;
#46175 = ORIENTED_EDGE ( 'NONE', *, *, #40661, .F. ) ;
#46176 = CARTESIAN_POINT ( 'NONE',  ( -13.21926163189999848, 1421.359897795430015, 248.0989693021979861 ) ) ;
#46177 = CARTESIAN_POINT ( 'NONE',  ( 5.487466536400559924, 1465.925728487379956, 200.7492532196600052 ) ) ;
#46178 = CARTESIAN_POINT ( 'NONE',  ( -0.3342637058910000181, 1475.047619362329897, 269.6500372387980065 ) ) ;
#46180 = AXIS2_PLACEMENT_3D ( 'NONE', #10759, #62857, #26999 ) ;
#46179 = CARTESIAN_POINT ( 'NONE',  ( -16.68599179859999992, 1461.161699058329987, 228.2799821568980008 ) ) ;
#46181 = CARTESIAN_POINT ( 'NONE',  ( -28.91076495679999780, 1509.890507479829921, 211.0912775665780146 ) ) ;
#46182 = CARTESIAN_POINT ( 'NONE',  ( -3.650443696216681744, 1448.291914533057479, 184.9508012256059999 ) ) ;
#46183 = CARTESIAN_POINT ( 'NONE',  ( -39.05830609401130005, 1384.791778035780226, 240.5085568879630102 ) ) ;
#46184 = CARTESIAN_POINT ( 'NONE',  ( -17.62728127150000290, 1415.048591094029916, 207.6446436201280221 ) ) ;
#46185 = CARTESIAN_POINT ( 'NONE',  ( 11.87450673426269887, 1432.968194686480047, 149.9806125890570172 ) ) ;
#46186 = CARTESIAN_POINT ( 'NONE',  ( 26.79956694294169850, 1435.440314151020175, 135.4706125346669978 ) ) ;
#46187 = CARTESIAN_POINT ( 'NONE',  ( -9.209528894577250213, 1396.234664223010213, 215.2427597039980185 ) ) ;
#46188 = CARTESIAN_POINT ( 'NONE',  ( -15.49830443269999947, 1421.268164864530036, 227.1260603972979766 ) ) ;
#46189 = CARTESIAN_POINT ( 'NONE',  ( 19.54803553591734300, 1455.513809965727887, 225.8158593003944645 ) ) ;
#46190 = ORIENTED_EDGE ( 'NONE', *, *, #65200, .T. ) ;
#46191 = CARTESIAN_POINT ( 'NONE',  ( -21.92423686380000092, 1509.678671609130106, 190.3411753256980035 ) ) ;
#46192 = CARTESIAN_POINT ( 'NONE',  ( 1.674597368589999968, 1409.138563866230015, 231.5566276255979687 ) ) ;
#46193 = CARTESIAN_POINT ( 'NONE',  ( -3.175620192230000249, 1509.758513049789826, 217.6845658033289794 ) ) ;
#46195 = CARTESIAN_POINT ( 'NONE',  ( -13.50445036796499920, 1512.655881406850085, 193.7448231092670028 ) ) ;
#46194 = CARTESIAN_POINT ( 'NONE',  ( 11.56890495900000104, 1426.389997043230096, 132.2071877881980129 ) ) ;
#46196 = CARTESIAN_POINT ( 'NONE',  ( 11.65615920360559343, 1428.981702016564896, 138.1374390033663815 ) ) ;
#46197 = CARTESIAN_POINT ( 'NONE',  ( -11.23388613411650638, 1442.762691980111640, 151.7784653951601399 ) ) ;
#46198 = AXIS2_PLACEMENT_3D ( 'NONE', #28414, #20000, #54192 ) ;
#46199 = CARTESIAN_POINT ( 'NONE',  ( 3.260357128764999946, 1517.133889586189980, 201.3971135232069969 ) ) ;
#46200 = CARTESIAN_POINT ( 'NONE',  ( 7.663837900699999928, 1425.530251840890060, 211.9032649451089867 ) ) ;
#46201 = DIRECTION ( 'NONE',  ( 0.000000000000000000, 0.000000000000000000, -1.000000000000000000 ) ) ;
#46202 = CARTESIAN_POINT ( 'NONE',  ( 4.112297488690000336, 1508.008646858429984, 181.4894093006979858 ) ) ;
#46203 = CARTESIAN_POINT ( 'NONE',  ( 7.772759690054999560, 1512.089957059379913, 206.2799139137070199 ) ) ;
#46204 = CARTESIAN_POINT ( 'NONE',  ( -82.97477735809999899, 1376.309726841469910, 300.0739800579590337 ) ) ;
#46205 = CARTESIAN_POINT ( 'NONE',  ( 6.844085095878397418, 1365.985930475517080, 209.6218459617148824 ) ) ;
#46207 = ORIENTED_EDGE ( 'NONE', *, *, #73521, .F. ) ;
#46206 = CARTESIAN_POINT ( 'NONE',  ( 8.784742016200000947, 1452.237884818490102, 212.1741301903489898 ) ) ;
#46208 = EDGE_LOOP ( 'NONE', ( #97596, #78436, #12172, #27423 ) ) ;
#46209 = DIRECTION ( 'NONE',  ( 0.6742693640212139572, 4.521919481779819710E-17, 0.7384854939282339270 ) ) ;
#46210 = B_SPLINE_CURVE_WITH_KNOTS ( 'NONE', 3,
 ( #56983, #94850, #91114, #100606, #67040, #23889, #109578, #18126, #7656, #14939, #31206, #58082, #66501, #74885, #33393, #86446, #48584, #49134, #92215, #73786, #6562, #24441 ),
 .UNSPECIFIED., .F., .F.,
 ( 4, 3, 3, 3, 3, 3, 3, 4 ),
 ( -1.499425824813870101, -1.379341959591650069, -1.182344938071870022, -0.9769786663024579987, -0.7652101314604189408, -0.5410848898833939824, -0.3077391086603749049, -0.06613165699310008527 ),
 .UNSPECIFIED. ) ;
#46211 = CARTESIAN_POINT ( 'NONE',  ( 1.428000371958690007, 1474.800808632939834, 235.3830380111929799 ) ) ;
#46212 = CARTESIAN_POINT ( 'NONE',  ( 4.255689356150000435, 1519.913060387329779, 231.5674970370980077 ) ) ;
#46213 = CARTESIAN_POINT ( 'NONE',  ( -7.559010200714999961, 1510.805212328559946, 214.6182764915270127 ) ) ;
#46215 = CARTESIAN_POINT ( 'NONE',  ( -1.356962606528219872, 1410.665719724639985, 185.5898146020100228 ) ) ;
#46214 = CARTESIAN_POINT ( 'NONE',  ( -8.579897891159999901, 1384.651925423579996, 218.6623841843989737 ) ) ;
#46216 = EDGE_CURVE ( 'NONE', #45625, #22768, #35001, .T. ) ;
#46217 = CARTESIAN_POINT ( 'NONE',  ( 2.342170655370000354, 1410.304730194330205, 185.5336642671979916 ) ) ;
#46218 = CARTESIAN_POINT ( 'NONE',  ( 3.487592428935230249, 1508.551704408389924, 214.1089243929580164 ) ) ;
#46219 = CARTESIAN_POINT ( 'NONE',  ( -38.96469809825319430, 1449.667656893509957, 135.7280615607639902 ) ) ;
#46220 = FILL_AREA_STYLE ('',( #12592 ) ) ;
#46221 = CARTESIAN_POINT ( 'NONE',  ( -2.500000000000000000, 1448.200164017079942, 169.1288108960040120 ) ) ;
#46222 = CARTESIAN_POINT ( 'NONE',  ( 0.1681681984989999989, 1416.866694505930127, 168.0175527136979667 ) ) ;
#46223 = CARTESIAN_POINT ( 'NONE',  ( -9.184850993605149917E-16, 1374.913060387289988, 209.1218459616989946 ) ) ;
#46224 = CARTESIAN_POINT ( 'NONE',  ( -5.362054705371839702, 1406.004091175200074, 268.4716808012279898 ) ) ;
#46225 = B_SPLINE_CURVE_WITH_KNOTS ( 'NONE', 5,
 ( #37743, #2517, #71391, #95990, #70283, #106592 ),
 .UNSPECIFIED., .F., .F.,
 ( 6, 6 ),
 ( 0.000000000000000000, 1.000000000000000000 ),
 .UNSPECIFIED. ) ;
#46226 = CARTESIAN_POINT ( 'NONE',  ( 40.27001047769999786, 1443.957955290329892, 137.1320999901979860 ) ) ;
#46227 = ORIENTED_EDGE ( 'NONE', *, *, #64587, .F. ) ;
#46228 = CARTESIAN_POINT ( 'NONE',  ( -16.56816485275624373, 1526.186458717540290, 182.6341057012185445 ) ) ;
#46229 = CARTESIAN_POINT ( 'NONE',  ( 21.46350454714117717, 1524.972383263452457, 234.5041546974912023 ) ) ;
#46230 = ORIENTED_EDGE ( 'NONE', *, *, #80522, .T. ) ;
#46231 = AXIS2_PLACEMENT_3D ( 'NONE', #50811, #24482, #51355 ) ;
#46232 = EDGE_LOOP ( 'NONE', ( #40551, #80044 ) ) ;
#46233 = CARTESIAN_POINT ( 'NONE',  ( -3.954567845990000219, 1455.724191770290190, 200.5335190476789933 ) ) ;
#46234 = CARTESIAN_POINT ( 'NONE',  ( 8.251048879689999893, 1367.474174444410210, 207.6218459616989946 ) ) ;
#46235 = VECTOR ( 'NONE', #88974, 1000.000000000000114 ) ;
#46236 = CARTESIAN_POINT ( 'NONE',  ( 3.262264650305000124, 1516.633288330999903, 215.6694029015669969 ) ) ;
#46237 = CARTESIAN_POINT ( 'NONE',  ( 3.481979419164999978, 1511.353635254350138, 216.8568855192669957 ) ) ;
#46238 = AXIS2_PLACEMENT_3D ( 'NONE', #44773, #62701, #78923 ) ;
#46239 = B_SPLINE_CURVE_WITH_KNOTS ( 'NONE', 3,
 ( #13869, #73819, #107394, #83301, #100103, #65980, #57022, #21713, #58117, #6043 ),
 .UNSPECIFIED., .F., .F.,
 ( 4, 3, 3, 4 ),
 ( 9.225465320329998775, 9.476690767968960927, 9.821219881794329254, 10.07010780362520030 ),
 .UNSPECIFIED. ) ;
#46240 = ORIENTED_EDGE ( 'NONE', *, *, #13923, .F. ) ;
#46241 = CARTESIAN_POINT ( 'NONE',  ( 2.500000000000000000, 1448.386321835900162, 162.4776903873720073 ) ) ;
#46242 = CARTESIAN_POINT ( 'NONE',  ( -87.79856897099999458, 1379.577971547980042, 299.2711673883590038 ) ) ;
#46243 = AXIS2_PLACEMENT_3D ( 'NONE', #32613, #30951, #57294 ) ;
#46244 = AXIS2_PLACEMENT_3D ( 'NONE', #80059, #106365, #12848 ) ;
#46245 = CARTESIAN_POINT ( 'NONE',  ( 2.824000625309999624, 1415.931784855930118, 226.7557855299979792 ) ) ;
#46246 = CARTESIAN_POINT ( 'NONE',  ( 2.866857893004999713, 1516.951766529250108, 205.0784797119270024 ) ) ;
#46247 = CARTESIAN_POINT ( 'NONE',  ( -12.00397982357779902, 1489.758001204110087, 211.4229914170240079 ) ) ;
#46248 = ADVANCED_FACE ( 'NONE', ( #97030 ), #33551, .F. ) ;
#46249 = CARTESIAN_POINT ( 'NONE',  ( 11.85372022028200512, 1433.007143091356966, 150.3176643612456473 ) ) ;
#46250 = CARTESIAN_POINT ( 'NONE',  ( -11.43071925370000130, 1410.242129527830002, 228.7924613954980089 ) ) ;
#46251 = EDGE_CURVE ( 'NONE', #41641, #46650, #68556, .T. ) ;
#46253 = ORIENTED_EDGE ( 'NONE', *, *, #50873, .T. ) ;
#46252 = CARTESIAN_POINT ( 'NONE',  ( 2.472529913803022783, 1523.678648413191695, 175.3762130535718597 ) ) ;
#46254 = CARTESIAN_POINT ( 'NONE',  ( 27.01382310970000233, 1451.969724731730139, 134.9184576876980088 ) ) ;
#46255 = DIRECTION ( 'NONE',  ( -0.7063774289747313251, 0.04540766091858282338, 0.7063774289747313251 ) ) ;
#46256 = CARTESIAN_POINT ( 'NONE',  ( -5.958828918900000104, 1384.553407673830179, 218.5245230306490214 ) ) ;
#46257 = DIRECTION ( 'NONE',  ( 0.000000000000000000, 1.000000000000000000, 0.000000000000000000 ) ) ;
#46258 = EDGE_CURVE ( 'NONE', #87081, #57154, #51087, .T. ) ;
#46259 = AXIS2_PLACEMENT_3D ( 'NONE', #91053, #40658, #48528 ) ;
#46260 = CARTESIAN_POINT ( 'NONE',  ( 25.90444642119999941, 1413.781696259030014, 270.1671806362980419 ) ) ;
#46261 = CARTESIAN_POINT ( 'NONE',  ( -3.447264387095000160, 1516.858765657450249, 212.5828932618570093 ) ) ;
#46262 = CARTESIAN_POINT ( 'NONE',  ( -65.35196250319999933, 1379.741131604200064, 273.2162891523590247 ) ) ;
#46263 = ADVANCED_FACE ( 'NONE', ( #65632 ), #58143, .T. ) ;
#46264 = CARTESIAN_POINT ( 'NONE',  ( 23.37417682859999957, 1410.122926439930097, 208.1639534942089824 ) ) ;
#46265 = CARTESIAN_POINT ( 'NONE',  ( 0.01819570974567621957, 1507.514099832349757, 237.4105189671679739 ) ) ;
#46266 = CARTESIAN_POINT ( 'NONE',  ( 14.30096130324469961, 1427.140377532109824, 198.0371785924010055 ) ) ;
#46267 = CARTESIAN_POINT ( 'NONE',  ( -11.60004869885203682, 1422.222932908413441, 135.5999999980979851 ) ) ;
#46268 = CARTESIAN_POINT ( 'NONE',  ( -2.286472924554999953, 1516.883361325900069, 209.8798303522490016 ) ) ;
#46269 = ORIENTED_EDGE ( 'NONE', *, *, #50822, .F. ) ;
#46270 = CARTESIAN_POINT ( 'NONE',  ( 4.183002505363929480, 1421.631134843499922, 184.7734457259539909 ) ) ;
#46271 = B_SPLINE_CURVE_WITH_KNOTS ( 'NONE', 5,
 ( #51124, #84699, #59528, #26451, #43278, #8000 ),
 .UNSPECIFIED., .F., .F.,
 ( 6, 6 ),
 ( 0.000000000000000000, 1.000000000000000000 ),
 .UNSPECIFIED. ) ;
#46272 = LINE ( 'NONE', #108349, #28728 ) ;
#46273 = CARTESIAN_POINT ( 'NONE',  ( -5.513435801945663961, 1508.611350399025241, 201.8000010755221751 ) ) ;
#46274 = EDGE_LOOP ( 'NONE', ( #72396, #63262, #95818, #80372, #106116 ) ) ;
#46276 = B_SPLINE_CURVE_WITH_KNOTS ( 'NONE', 3,
 ( #16028, #50757, #17114, #23338, #57530, #84355, #91654, #41258, #75959, #14928 ),
 .UNSPECIFIED., .F., .F.,
 ( 4, 2, 2, 2, 4 ),
 ( 0.000000000000000000, 0.0007403986298595364567, 0.001480797259719072913, 0.002221195889578609153, 0.002961594519438145827 ),
 .UNSPECIFIED. ) ;
#46275 = CARTESIAN_POINT ( 'NONE',  ( -23.86417894507290072, 1385.260624856700133, 222.9263582714870040 ) ) ;
#46277 = CARTESIAN_POINT ( 'NONE',  ( -2.734206733259999744, 1429.237800606489827, 200.5523466973589848 ) ) ;
#46278 = CARTESIAN_POINT ( 'NONE',  ( 18.87980474539999776, 1507.654596655130035, 188.5454329983980131 ) ) ;
#46279 = MANIFOLD_SOLID_BREP ( 'Stock-MAS-682-1', #105696 ) ;
#46280 = FACE_OUTER_BOUND ( 'NONE', #39772, .T. ) ;
#46281 = DIRECTION ( 'NONE',  ( 0.000000000000000000, -0.9990482215818579093, -0.04361938736533144123 ) ) ;
#46282 = DIRECTION ( 'NONE',  ( 1.755985294532464991E-16, -1.000000000000000000, 1.338183447452830017E-16 ) ) ;
#46284 = CARTESIAN_POINT ( 'NONE',  ( -7.965810688893188996, 1384.899971919800009, 199.4892299149449855 ) ) ;
#46283 = CARTESIAN_POINT ( 'NONE',  ( 5.780861236055000241, 1516.783701990830195, 216.0610654530370027 ) ) ;
#46285 = CARTESIAN_POINT ( 'NONE',  ( 10.41177329615350011, 1460.024665156439823, 205.9063136364349873 ) ) ;
#46286 = FACE_OUTER_BOUND ( 'NONE', #83204, .T. ) ;
#46287 = ORIENTED_EDGE ( 'NONE', *, *, #46749, .F. ) ;
#46288 = CARTESIAN_POINT ( 'NONE',  ( 1.124894050234999998, 1517.194816588360027, 202.1703287997270309 ) ) ;
#46289 = ADVANCED_FACE ( 'NONE', ( #17937 ), #97289, .T. ) ;
#46290 = CARTESIAN_POINT ( 'NONE',  ( -18.91040668671855585, 1416.839570625527813, 208.2955991069221113 ) ) ;
#46291 = VERTEX_POINT ( 'NONE', #8861 ) ;
#46292 = DIRECTION ( 'NONE',  ( 0.000000000000000000, 1.000000000000000000, 0.000000000000000000 ) ) ;
#46293 = CARTESIAN_POINT ( 'NONE',  ( 10.81270716706183599, 1434.527702263565516, 151.9104491927415665 ) ) ;
#46294 = EDGE_CURVE ( 'NONE', #98127, #44371, #45746, .T. ) ;
#46295 = CARTESIAN_POINT ( 'NONE',  ( 8.795036018429138736, 1511.645100227929788, 202.9941036799409915 ) ) ;
#46296 = CARTESIAN_POINT ( 'NONE',  ( -0.2334700972460009849, 1444.212002848689963, 218.0769002143289867 ) ) ;
#46297 = CARTESIAN_POINT ( 'NONE',  ( -27.36410773769939908, 1509.677412868400097, 201.1425198521210120 ) ) ;
#46298 = CARTESIAN_POINT ( 'NONE',  ( -2.707337055090000000, 1447.195466704469936, 162.7581527779979922 ) ) ;
#46299 = CARTESIAN_POINT ( 'NONE',  ( -17.84295937140000277, 1424.580744259330004, 226.8532515114980299 ) ) ;
#46300 = CARTESIAN_POINT ( 'NONE',  ( -14.75639819380000084, 1435.138401597589791, 148.9684811175980030 ) ) ;
#46301 = CARTESIAN_POINT ( 'NONE',  ( -105.5067336309999888, 1391.271052109320181, 304.2081839319590131 ) ) ;
#46302 = DIRECTION ( 'NONE',  ( -1.000000000000000000, 0.000000000000000000, 0.000000000000000000 ) ) ;
#46304 = CARTESIAN_POINT ( 'NONE',  ( 29.25495648800000126, 1509.872423544630010, 209.6024569297780147 ) ) ;
#46303 = CARTESIAN_POINT ( 'NONE',  ( 0.7692391029780000222, 1415.628674266529742, 190.8565233057979924 ) ) ;
#46305 = CARTESIAN_POINT ( 'NONE',  ( 2.531940903048510086E-08, 1457.850589566970029, 229.0733431205499926 ) ) ;
#46306 = ORIENTED_EDGE ( 'NONE', *, *, #15063, .F. ) ;
#46307 = CARTESIAN_POINT ( 'NONE',  ( -11.48415382500000170, 1508.440752798089989, 218.1712173149890077 ) ) ;
#46308 = CARTESIAN_POINT ( 'NONE',  ( -45.63702719927069751, 1439.462929478074329, 268.9748534858272819 ) ) ;
#46309 = CARTESIAN_POINT ( 'NONE',  ( -24.11734304670000029, 1437.967394118240009, 211.4545401520780104 ) ) ;
#46310 = CARTESIAN_POINT ( 'NONE',  ( -2.001528378510000206, 1483.806447908390055, 198.6272630702989943 ) ) ;
#46311 = VECTOR ( 'NONE', #103761, 1000.000000000000000 ) ;
#46312 = CARTESIAN_POINT ( 'NONE',  ( -16.02483746670864662, 1417.968541902725747, 204.0964192873620959 ) ) ;
#46313 = CARTESIAN_POINT ( 'NONE',  ( -2.708816481115378760, 1524.478200376950781, 241.9482032910334510 ) ) ;
#46314 = CARTESIAN_POINT ( 'NONE',  ( 18.04400385319999955, 1497.713060387329961, 221.4191216194980143 ) ) ;
#46315 = CARTESIAN_POINT ( 'NONE',  ( 26.81574339440005872, 1435.910933784995905, 136.5210778358012078 ) ) ;
#46316 = CARTESIAN_POINT ( 'NONE',  ( 4.641807258861630814, 1493.238112264180018, 219.2220438651660004 ) ) ;
#46317 = VECTOR ( 'NONE', #47551, 1000.000000000000114 ) ;
#46318 = CARTESIAN_POINT ( 'NONE',  ( -4.969322309076429356, 1487.355502429559920, 219.6549086668990185 ) ) ;
#46319 = CARTESIAN_POINT ( 'NONE',  ( -18.29179384260000063, 1466.060301038189891, 217.7541513960790098 ) ) ;
#46320 = CARTESIAN_POINT ( 'NONE',  ( -76.80923957048339901, 1383.779367511659984, 301.3284849630780400 ) ) ;
#46321 = CIRCLE ( 'NONE', #73147, 2.000000000088558050 ) ;
#46322 = CARTESIAN_POINT ( 'NONE',  ( -109.7747990662900008, 1384.235278760439996, 311.3356848936479651 ) ) ;
#46323 = CARTESIAN_POINT ( 'NONE',  ( 0.3712394671979279970, 1517.036116044630262, 201.3996746346359714 ) ) ;
#46325 = VERTEX_POINT ( 'NONE', #94522 ) ;
#46324 = CARTESIAN_POINT ( 'NONE',  ( 20.58555848629999829, 1507.839439013330093, 189.9311647047979932 ) ) ;
#46326 = CARTESIAN_POINT ( 'NONE',  ( 13.89676589599709899, 1513.004579589660125, 224.4119314900950144 ) ) ;
#46327 = ORIENTED_EDGE ( 'NONE', *, *, #9754, .F. ) ;
#46328 = EDGE_LOOP ( 'NONE', ( #64837, #26181, #73882, #70595 ) ) ;
#46329 = CARTESIAN_POINT ( 'NONE',  ( 23.55087631299999984, 1411.110694763729953, 207.7642880164279973 ) ) ;
#46330 = DIRECTION ( 'NONE',  ( 0.9125304618753996566, 0.000000000000000000, 0.4090087482554252696 ) ) ;
#46331 = CARTESIAN_POINT ( 'NONE',  ( 12.68818856000646811, 1442.806559773770005, 169.4610080275735697 ) ) ;
#46333 = CARTESIAN_POINT ( 'NONE',  ( -14.70061896320000017, 1464.437658295030133, 244.5173668927980088 ) ) ;
#46332 = CARTESIAN_POINT ( 'NONE',  ( 38.46381803922925258, 1428.620948229150599, 269.5839343762438034 ) ) ;
#46334 = CARTESIAN_POINT ( 'NONE',  ( -19.92390948350000102, 1487.986067298129910, 190.3334121447979896 ) ) ;
#46335 = CARTESIAN_POINT ( 'NONE',  ( -11.73555011919999913, 1433.698852586370094, 150.9369036644980042 ) ) ;
#46336 = CARTESIAN_POINT ( 'NONE',  ( 11.48709584101343140, 1502.831951580399164, 210.2032813508793083 ) ) ;
#46337 = CARTESIAN_POINT ( 'NONE',  ( -19.35364397750000265, 1485.770172091730046, 189.8349640065979997 ) ) ;
#46338 = AXIS2_PLACEMENT_3D ( 'NONE', #40696, #49668, #39026 ) ;
#46339 = CARTESIAN_POINT ( 'NONE',  ( -5.723713397950000115, 1444.578274639889969, 217.6728780112489972 ) ) ;
#46340 = CARTESIAN_POINT ( 'NONE',  ( 4.435478739589999719, 1421.723673722030071, 185.0752384912979949 ) ) ;
#46341 = CARTESIAN_POINT ( 'NONE',  ( 1.379638663375890140, 1515.081065330719866, 213.4508686280049972 ) ) ;
#46342 = CARTESIAN_POINT ( 'NONE',  ( -68.77278092737650184, 1379.747928288920093, 280.3133413970129482 ) ) ;
#46343 = CARTESIAN_POINT ( 'NONE',  ( 13.15366522099999891, 1428.703228679929907, 223.0784815109979888 ) ) ;
#46344 = CARTESIAN_POINT ( 'NONE',  ( 3.355892881418364837, 1523.847233649538339, 242.0621658074067852 ) ) ;
#46346 = VERTEX_POINT ( 'NONE', #66607 ) ;
#46345 = CARTESIAN_POINT ( 'NONE',  ( 1.394896777640000085, 1465.720900818929977, 235.3343343731980042 ) ) ;
#46347 = VERTEX_POINT ( 'NONE', #67150 ) ;
#46348 = CARTESIAN_POINT ( 'NONE',  ( -11.86488112544160067, 1432.250788954399923, 149.9817061855939926 ) ) ;
#46349 = CARTESIAN_POINT ( 'NONE',  ( -22.15023429329999871, 1486.164746652490066, 217.3274157383089857 ) ) ;
#46350 = CARTESIAN_POINT ( 'NONE',  ( -24.79114683279999909, 1465.946749696029883, 269.6862801822979918 ) ) ;
#46351 = CARTESIAN_POINT ( 'NONE',  ( -12.18971938666500066, 1512.123542805230272, 194.3960765485670095 ) ) ;
#46352 = CARTESIAN_POINT ( 'NONE',  ( -106.7694122493245175, 1377.418846546389432, 315.3996670310588115 ) ) ;
#46353 = CARTESIAN_POINT ( 'NONE',  ( -22.53878221424140094, 1411.058442688259902, 212.0450776560099939 ) ) ;
#46354 = CARTESIAN_POINT ( 'NONE',  ( 0.3486255395347149788, 1450.932214069980091, 181.6278462867639973 ) ) ;
#46355 = CARTESIAN_POINT ( 'NONE',  ( -11.91935979259999989, 1420.493316629130049, 231.2800121289980098 ) ) ;
#46356 = CARTESIAN_POINT ( 'NONE',  ( -9.519812933809998157, 1460.017558320190119, 210.6311618102489831 ) ) ;
#46357 = CARTESIAN_POINT ( 'NONE',  ( 8.370313053925706015, 1361.245476951179626, 207.6218459616987673 ) ) ;
#46358 = CARTESIAN_POINT ( 'NONE',  ( -44.20424317085289800, 1432.326735547540011, 269.0150688337790257 ) ) ;
#46359 = ORIENTED_EDGE ( 'NONE', *, *, #86486, .F. ) ;
#46360 = CARTESIAN_POINT ( 'NONE',  ( -3.540123473188209857, 1498.107930687619955, 181.3611756044990102 ) ) ;
#46361 = EDGE_LOOP ( 'NONE', ( #87536, #54772, #51422, #11227 ) ) ;
#46362 = ORIENTED_EDGE ( 'NONE', *, *, #11938, .T. ) ;
#46363 = CARTESIAN_POINT ( 'NONE',  ( 5.014195101815000832, 1517.120861839400050, 210.8273123806970091 ) ) ;
#46364 = CARTESIAN_POINT ( 'NONE',  ( -7.454017790216410866, 1508.783371651619063, 203.6084103740970193 ) ) ;
#46365 = CARTESIAN_POINT ( 'NONE',  ( 12.90973010816660071, 1420.801971354559782, 222.8292615723929941 ) ) ;
#46366 = CARTESIAN_POINT ( 'NONE',  ( -14.44835241010000004, 1410.403412957530008, 190.4623667091979939 ) ) ;
#46367 = AXIS2_PLACEMENT_3D ( 'NONE', #30499, #64688, #21524 ) ;
#46368 = CARTESIAN_POINT ( 'NONE',  ( 1.210523399180029935, 1495.904440378810023, 221.4016620453209896 ) ) ;
#46369 = B_SPLINE_SURFACE_WITH_KNOTS ( 'NONE', 5, 5, ( 
 ( #72057, #87167, #61440, #46843, #97764, #10455 ),
 ( #80428, #96114, #46300, #19952, #71517, #18835 ),
 ( #2085, #54695, #21036, #88821, #53031, #55239 ),
 ( #106173, #11567, #63113, #44629, #45743, #36765 ),
 ( #37321, #3742, #27815, #27258, #19388, #28362 ),
 ( #12107, #79327, #28922, #2638, #29453, #63649 ),
 ( #70958, #97213, #20485, #78770, #35653, #105073 ),
 ( #62561, #80972, #96680, #89372, #69843, #36214 ),
 ( #70399, #104517, #54145, #61996, #53591, #87737 ),
 ( #45186, #79880, #3194, #74248, #83179, #92125 ),
 ( #6469, #48492, #4802, #107824, #55797, #5923 ),
 ( #39523, #4276, #56329, #40619, #65292, #5363 ) ),
 .UNSPECIFIED., .F., .F., .F.,
 ( 6, 3, 3, 6 ),
 ( 6, 6 ),
 ( 17.17643422080000093, 21.54070554389999970, 30.24627863650000137, 40.14628357800000202 ),
 ( 0.000000000000000000, 1.622089487970000077 ),
 .UNSPECIFIED. ) ;
#46370 = VERTEX_POINT ( 'NONE', #17796 ) ;
#46371 = CARTESIAN_POINT ( 'NONE',  ( 4.664268937930000192, 1505.247554523090002, 221.0077437511990013 ) ) ;
#46372 = CARTESIAN_POINT ( 'NONE',  ( -2.485846037024999955, 1516.545806094630279, 201.8003900583769905 ) ) ;
#46373 = AXIS2_PLACEMENT_3D ( 'NONE', #58299, #68369, #60514 ) ;
#46374 = MECHANICAL_DESIGN_GEOMETRIC_PRESENTATION_REPRESENTATION (  '', ( #60686 ), #17688 ) ;
#46375 = EDGE_CURVE ( 'NONE', #49270, #55773, #83685, .T. ) ;
#46376 = CARTESIAN_POINT ( 'NONE',  ( 4.972072924729999954, 1472.535148281390093, 218.0116174414390002 ) ) ;
#46377 = CARTESIAN_POINT ( 'NONE',  ( -9.463103648650079691, 1439.631690924059740, 207.7258123655099951 ) ) ;
#46378 = ORIENTED_EDGE ( 'NONE', *, *, #84235, .T. ) ;
#46379 = CARTESIAN_POINT ( 'NONE',  ( -27.08078463060560281, 1414.294447406490008, 269.9731611881400113 ) ) ;
#46380 = CARTESIAN_POINT ( 'NONE',  ( 2.840828255611359765, 1417.479495435399940, 232.6340383620710099 ) ) ;
#46381 = CARTESIAN_POINT ( 'NONE',  ( 8.280067823819621253, 1436.009449604699967, 206.8167673534310325 ) ) ;
#46383 = ORIENTED_EDGE ( 'NONE', *, *, #59611, .F. ) ;
#46382 = CARTESIAN_POINT ( 'NONE',  ( -7.996809115789493383, 1365.202203848373529, 208.3718459617061285 ) ) ;
#46384 = ORIENTED_EDGE ( 'NONE', *, *, #85910, .T. ) ;
#46385 = CARTESIAN_POINT ( 'NONE',  ( 44.72498031872709134, 1447.716264930823172, 269.0002976672203090 ) ) ;
#46386 = CARTESIAN_POINT ( 'NONE',  ( 1.311009928872819863, 1467.109053032259908, 220.1154688705190097 ) ) ;
#46387 = CARTESIAN_POINT ( 'NONE',  ( -13.58978489722930050, 1436.182389225290081, 150.4598382135330041 ) ) ;
#46388 = CARTESIAN_POINT ( 'NONE',  ( -0.3901548594470000131, 1486.096337175529925, 181.7750788774980037 ) ) ;
#46389 = TOROIDAL_SURFACE ( 'NONE', #12381, 10.10241613150000006, 2.000000000000000000 ) ;
#46390 = CARTESIAN_POINT ( 'NONE',  ( -19.81028112772915861, 1506.776553272468618, 219.5992980689768217 ) ) ;
#46391 = CARTESIAN_POINT ( 'NONE',  ( 8.401749989260000717, 1454.595346029489974, 215.7321778818789824 ) ) ;
#46392 = EDGE_CURVE ( 'NONE', #94689, #90525, #48519, .T. ) ;
#46393 = AXIS2_PLACEMENT_3D ( 'NONE', #35541, #79775, #108257 ) ;
#46394 = CARTESIAN_POINT ( 'NONE',  ( 5.317239278416240111, 1475.759745378969910, 269.0458115274469719 ) ) ;
#46395 = CARTESIAN_POINT ( 'NONE',  ( 11.54717405569999933, 1415.048591087029763, 222.4184568667979818 ) ) ;
#46396 = CARTESIAN_POINT ( 'NONE',  ( 3.880449101349999985, 1446.827807606209944, 183.7827426791980088 ) ) ;
#46397 = CARTESIAN_POINT ( 'NONE',  ( 7.321455873725000174, 1516.545806094630279, 206.6359999332069890 ) ) ;
#46398 = EDGE_LOOP ( 'NONE', ( #6166, #12054, #94353, #33812 ) ) ;
#46399 = CARTESIAN_POINT ( 'NONE',  ( -8.316672828268760753, 1425.055149638239982, 204.9623390585310005 ) ) ;
#46400 = CARTESIAN_POINT ( 'NONE',  ( -21.96271729628280411, 1452.898244988618899, 220.9930576170047232 ) ) ;
#46401 = ORIENTED_EDGE ( 'NONE', *, *, #24991, .F. ) ;
#46402 = CARTESIAN_POINT ( 'NONE',  ( 12.43875923093532343, 1454.082076206495913, 225.3359954487575010 ) ) ;
#46404 = EDGE_CURVE ( 'NONE', #86968, #98016, #99746, .T. ) ;
#46403 = CARTESIAN_POINT ( 'NONE',  ( -2.823654301615894369, 1367.710812309479252, 209.6453303274731468 ) ) ;
#46405 = CARTESIAN_POINT ( 'NONE',  ( -14.22126295610000213, 1417.509116686749849, 204.1625520109990077 ) ) ;
#46406 = CARTESIAN_POINT ( 'NONE',  ( 18.87295847649999914, 1409.572118621430036, 197.2370177091979997 ) ) ;
#46407 = CARTESIAN_POINT ( 'NONE',  ( 20.87866911129999892, 1445.052233488290085, 177.0630364655980031 ) ) ;
#46408 = CARTESIAN_POINT ( 'NONE',  ( -23.91862134480000179, 1435.332757494850057, 136.7253933288979795 ) ) ;
#46409 = CARTESIAN_POINT ( 'NONE',  ( 32.23107245337714488, 1523.542365884048195, 201.4053004075441038 ) ) ;
#46410 = CARTESIAN_POINT ( 'NONE',  ( -1.289560617741849935, 1504.157614064680047, 209.3656258553460248 ) ) ;
#46411 = AXIS2_PLACEMENT_3D ( 'NONE', #1481, #55207, #37288 ) ;
#46412 = CARTESIAN_POINT ( 'NONE',  ( 2.500000000000000000, 1439.624612761979961, 169.0979957011440149 ) ) ;
#46413 = CARTESIAN_POINT ( 'NONE',  ( 2.294209629405000062, 1516.603620185149794, 214.8927295341169952 ) ) ;
#46414 = CARTESIAN_POINT ( 'NONE',  ( -32.86802468386279941, 1523.481610426287716, 217.2040256693919957 ) ) ;
#46415 = VERTEX_POINT ( 'NONE', #41385 ) ;
#46416 = CARTESIAN_POINT ( 'NONE',  ( -17.33425267040000151, 1417.532075291570209, 206.8248474228290092 ) ) ;
#46417 = CARTESIAN_POINT ( 'NONE',  ( 20.98221433428943428, 1524.841055067849538, 237.1519650095368092 ) ) ;
#46418 = CARTESIAN_POINT ( 'NONE',  ( -1273.316865285699805, 2833.596074015789782, 9977.675558182170789 ) ) ;
#46419 = CARTESIAN_POINT ( 'NONE',  ( -37.35391162073399585, 1449.318672761829930, 136.3174603101959974 ) ) ;
#46420 = ADVANCED_FACE ( 'NONE', ( #49790 ), #23992, .F. ) ;
#46421 = CARTESIAN_POINT ( 'NONE',  ( 10.91790884276356266, 1424.877151459083962, 138.2600712752583547 ) ) ;
#46422 = DIRECTION ( 'NONE',  ( -1.000000000000000000, -5.823966869780190178E-19, 4.137698748469999823E-18 ) ) ;
#46423 = CARTESIAN_POINT ( 'NONE',  ( -2.500000000000000000, 1426.216228438830058, 155.9944625376979843 ) ) ;
#46424 = CARTESIAN_POINT ( 'NONE',  ( 11.87499166480000135, 1433.007134997589901, 150.0931860300979963 ) ) ;
#46425 = CARTESIAN_POINT ( 'NONE',  ( -44.92381709066269480, 1440.913053709800124, 269.6913904019010033 ) ) ;
#46426 = CARTESIAN_POINT ( 'NONE',  ( -10.07183425689889944, 1461.550206846259925, 210.3700608705820230 ) ) ;
#46427 = CARTESIAN_POINT ( 'NONE',  ( -110.0664121069999908, 1385.015438621219801, 296.9524368094589590 ) ) ;
#46428 = CARTESIAN_POINT ( 'NONE',  ( -2.038646110889678287, 1525.960063244516959, 241.1857569150893994 ) ) ;
#46429 = ORIENTED_EDGE ( 'NONE', *, *, #61773, .T. ) ;
#46430 = B_SPLINE_CURVE_WITH_KNOTS ( 'NONE', 5,
 ( #5399, #101501, #69061, #73732, #107855, #65332 ),
 .UNSPECIFIED., .F., .F.,
 ( 6, 6 ),
 ( -13.21653623010000089, -9.791999830326519216 ),
 .UNSPECIFIED. ) ;
#46431 = CARTESIAN_POINT ( 'NONE',  ( 11.23388613411650105, 1443.913060387330006, 150.9272215568489912 ) ) ;
#46432 = CARTESIAN_POINT ( 'NONE',  ( -2.695946298204319636, 1485.848501370371878, 182.4462471310350793 ) ) ;
#46433 = CARTESIAN_POINT ( 'NONE',  ( -1.282176200179999892, 1442.957053292389901, 200.3169478525390161 ) ) ;
#46434 = CARTESIAN_POINT ( 'NONE',  ( 2.116402719909999952, 1507.098271169029886, 236.1684022847979918 ) ) ;
#46435 = AXIS2_PLACEMENT_3D ( 'NONE', #35507, #69700, #103819 ) ;
#46436 = CARTESIAN_POINT ( 'NONE',  ( -16.56816485275871287, 1526.186458717539836, 235.6095862221776258 ) ) ;
#46437 = CARTESIAN_POINT ( 'NONE',  ( -10.18845689910000019, 1507.986917720829979, 234.4944681294980171 ) ) ;
#46438 = CARTESIAN_POINT ( 'NONE',  ( -24.95503619787630356, 1383.848126923009886, 223.4623740270739916 ) ) ;
#46439 = CARTESIAN_POINT ( 'NONE',  ( 19.44117294853580091, 1456.941945407359981, 224.4539793896520052 ) ) ;
#46440 = CARTESIAN_POINT ( 'NONE',  ( 2.499944775320749990, 1419.515170344529906, 137.7430823675560134 ) ) ;
#46441 = CARTESIAN_POINT ( 'NONE',  ( 3.829620113550000315, 1515.551704408389924, 206.7917118356089929 ) ) ;
#46442 = CARTESIAN_POINT ( 'NONE',  ( 1.742626253590000118, 1466.605724893630168, 234.7106070462979801 ) ) ;
#46444 = VERTEX_POINT ( 'NONE', #100712 ) ;
#46443 = CYLINDRICAL_SURFACE ( 'NONE', #101508, 2.000000000000003109 ) ;
#46445 = CARTESIAN_POINT ( 'NONE',  ( -1.141221057759999935, 1450.801352449960177, 182.0259209118979982 ) ) ;
#46446 = CIRCLE ( 'NONE', #26754, 1.999999999999999556 ) ;
#46447 = CARTESIAN_POINT ( 'NONE',  ( -46.07807520840000137, 1384.601971911739838, 219.0368719419589922 ) ) ;
#46448 = CARTESIAN_POINT ( 'NONE',  ( -3.640869362099999673, 1474.974412159089979, 198.7036061503989970 ) ) ;
#46450 = ORIENTED_EDGE ( 'NONE', *, *, #50827, .F. ) ;
#46449 = CARTESIAN_POINT ( 'NONE',  ( 1.547463896846929865, 1414.913060387349788, 192.3096116128920130 ) ) ;
#46451 = CARTESIAN_POINT ( 'NONE',  ( -11.77904337550669922, 1483.168283496399908, 228.2502193403299771 ) ) ;
#46452 = EDGE_LOOP ( 'NONE', ( #11245, #30734, #49723 ) ) ;
#46453 = CARTESIAN_POINT ( 'NONE',  ( -13.29669657483730205, 1389.765376659109961, 214.2158769609019942 ) ) ;
#46454 = CARTESIAN_POINT ( 'NONE',  ( 12.81436426557939967, 1447.032452139500037, 186.0874941928050248 ) ) ;
#46455 = CARTESIAN_POINT ( 'NONE',  ( 13.80546151116429954, 1434.979654507460054, 148.5370226032280243 ) ) ;
#46456 = VECTOR ( 'NONE', #65046, 1000.000000000000000 ) ;
#46457 = DIRECTION ( 'NONE',  ( 0.02616798426500960631, 0.9993150019883682011, 0.02616798426500960631 ) ) ;
#46458 = CARTESIAN_POINT ( 'NONE',  ( -3.100192419969999946, 1431.506313241990028, 216.9304414810590060 ) ) ;
#46459 = CARTESIAN_POINT ( 'NONE',  ( 7.703785732380000084, 1490.746146274789908, 209.8379679705590206 ) ) ;
#46460 = CARTESIAN_POINT ( 'NONE',  ( 10.25464339219990073, 1409.271160421150171, 220.0084936090869974 ) ) ;
#46461 = CARTESIAN_POINT ( 'NONE',  ( -33.91369110979979951, 1435.681798629080049, 135.0664268289980043 ) ) ;
#46462 = CARTESIAN_POINT ( 'NONE',  ( -95.64499328508460962, 1385.209349391769820, 295.1734178191939577 ) ) ;
#46463 = DIRECTION ( 'NONE',  ( -0.9861488070177710785, 0.1648740218884660325, -0.01808555566601800085 ) ) ;
#46464 = CARTESIAN_POINT ( 'NONE',  ( -68.53407989799998745, 1379.748277114789971, 279.6522222015589705 ) ) ;
#46465 = CIRCLE ( 'NONE', #96488, 2.000000000000000000 ) ;
#46466 = CARTESIAN_POINT ( 'NONE',  ( 10.96071825005859957, 1490.321551646910166, 209.5423776189929868 ) ) ;
#46467 = ORIENTED_EDGE ( 'NONE', *, *, #46140, .T. ) ;
#46468 = EDGE_LOOP ( 'NONE', ( #2690, #97705, #20712, #34999, #16869, #34809, #74736, #97807 ) ) ;
#46469 =( BOUNDED_CURVE ( )  B_SPLINE_CURVE ( 3, ( #2398, #12407, #46591, #79641 ),
 .UNSPECIFIED., .F., .F. ) 
 B_SPLINE_CURVE_WITH_KNOTS ( ( 4, 4 ),
 ( 1.070796326794966058, 1.570796326794965614 ),
 .UNSPECIFIED. ) 
 CURVE ( )  GEOMETRIC_REPRESENTATION_ITEM ( )  RATIONAL_B_SPLINE_CURVE ( ( 1.000000000000000000, 0.9792749478070965630, 0.9792749478070965630, 1.000000000000000000 ) ) 
 REPRESENTATION_ITEM ( '' )  );
#46470 = CARTESIAN_POINT ( 'NONE',  ( -13.84742034927290000, 1420.584111001069914, 215.1188189259799799 ) ) ;
#46471 = CARTESIAN_POINT ( 'NONE',  ( -11.74953517305270090, 1415.393085341020196, 195.1736183478689668 ) ) ;
#46472 = CARTESIAN_POINT ( 'NONE',  ( 0.6919511451386070044, 1496.727473275949933, 196.7667901871089953 ) ) ;
#46473 = CARTESIAN_POINT ( 'NONE',  ( 16.29513934676993969, 1469.031411797243663, 269.3703662538208050 ) ) ;
#46474 = CARTESIAN_POINT ( 'NONE',  ( -20.22039848381579574, 1495.569241252630036, 190.7459851463269729 ) ) ;
#46475 = CARTESIAN_POINT ( 'NONE',  ( 4.487326635059999624, 1396.069761286429866, 219.5977994197980081 ) ) ;
#46476 = CARTESIAN_POINT ( 'NONE',  ( 32.36539537780658549, 1523.843271061948144, 202.1341907014572428 ) ) ;
#46477 = CARTESIAN_POINT ( 'NONE',  ( -12.53380499174499896, 1445.052233488290085, 169.4755105688890069 ) ) ;
#46478 = CARTESIAN_POINT ( 'NONE',  ( -9.978586514373580130, 1364.539968386208102, 210.6218459616991936 ) ) ;
#46479 = CARTESIAN_POINT ( 'NONE',  ( -20.11865724026149849, 1457.295805411310084, 208.8536593322139936 ) ) ;
#46480 = DIRECTION ( 'NONE',  ( -1.000000000000000000, 0.000000000000000000, 0.000000000000000000 ) ) ;
#46481 = CARTESIAN_POINT ( 'NONE',  ( 1.700259675955000160, 1516.898441858519845, 207.4036424686470070 ) ) ;
#46482 = AXIS2_PLACEMENT_3D ( 'NONE', #34307, #58423, #76876 ) ;
#46483 = CARTESIAN_POINT ( 'NONE',  ( -13.76849749719999849, 1435.338886191890197, 149.7896896373979985 ) ) ;
#46484 = CARTESIAN_POINT ( 'NONE',  ( -8.580821470709999232, 1384.944142111179872, 218.6694750710489927 ) ) ;
#46485 = B_SPLINE_SURFACE_WITH_KNOTS ( 'NONE', 5, 5, ( 
 ( #40558, #23194, #99342, #31600, #47313, #6412 ),
 ( #108316, #82574, #48433, #5304, #5866, #73634 ),
 ( #106653, #38890, #14799, #12607, #55186, #29944 ),
 ( #65231, #74732, #90957, #48985, #65779, #64136 ),
 ( #90395, #30501, #22617, #56821, #31049, #73072 ),
 ( #72524, #40007, #83118, #108866, #74185, #38345 ),
 ( #46787, #64690, #107213, #14244, #99896, #98257 ),
 ( #98808, #107765, #57393, #80917, #4215, #63592 ),
 ( #97709, #39462, #21526, #55738, #89860, #13129 ) ),
 .UNSPECIFIED., .F., .F., .F.,
 ( 6, 3, 6 ),
 ( 6, 6 ),
 ( 135.0843208316090056, 135.9934071210000184, 136.9024933901449970 ),
 ( 0.000000000000000000, 2.000049861391349992 ),
 .UNSPECIFIED. ) ;
#46486 = DIRECTION ( 'NONE',  ( 0.000000000000000000, 0.000000000000000000, 1.000000000000000000 ) ) ;
#46487 = DIRECTION ( 'NONE',  ( 0.000000000000000000, 1.000000000000000000, 0.000000000000000000 ) ) ;
#46488 = CARTESIAN_POINT ( 'NONE',  ( 41.02301855367610273, 1444.170996474450021, 136.8522558531069819 ) ) ;
#46489 = VERTEX_POINT ( 'NONE', #24547 ) ;
#46490 = CARTESIAN_POINT ( 'NONE',  ( 20.03573725999999766, 1421.675448603130008, 240.3194873134980014 ) ) ;
#46491 = CARTESIAN_POINT ( 'NONE',  ( -26.66951752270000142, 1488.685949851729902, 205.2938759693780071 ) ) ;
#46493 = CARTESIAN_POINT ( 'NONE',  ( 3.390830802950000193E-14, 1412.903649629229903, 264.4545146410980010 ) ) ;
#46492 = CARTESIAN_POINT ( 'NONE',  ( -0.5406448194880001390, 1507.263894173830067, 180.8238120802979836 ) ) ;
#46494 = DIRECTION ( 'NONE',  ( 0.000000000000000000, -0.02617694830808806397, -0.9996573249755517088 ) ) ;
#46495 = TOROIDAL_SURFACE ( 'NONE', #96600, 20.98341875039999849, 2.000000000000000000 ) ;
#46496 = CARTESIAN_POINT ( 'NONE',  ( -32.03901054129999437, 1430.123112395929866, 250.0966427571979978 ) ) ;
#46497 = CARTESIAN_POINT ( 'NONE',  ( 19.64611444698550002, 1509.628769227909970, 231.3538552484560000 ) ) ;
#46498 = CARTESIAN_POINT ( 'NONE',  ( 0.9264612404903812548, 1415.565606034773054, 233.1932629902654810 ) ) ;
#46499 = CARTESIAN_POINT ( 'NONE',  ( 1.674813627306420027, 1416.913057013589878, 192.1894777045280023 ) ) ;
#46500 = ORIENTED_EDGE ( 'NONE', *, *, #60946, .T. ) ;
#46501 = CARTESIAN_POINT ( 'NONE',  ( -11.22085815268440001, 1416.913060341719984, 220.6193217018360144 ) ) ;
#46502 = CARTESIAN_POINT ( 'NONE',  ( 11.88248411615536071, 1513.001574290550934, 225.6614044502198340 ) ) ;
#46503 = CARTESIAN_POINT ( 'NONE',  ( 11.68641999220000116, 1509.361170997829959, 236.6365785814979859 ) ) ;
#46504 = VERTEX_POINT ( 'NONE', #59309 ) ;
#46505 = ORIENTED_EDGE ( 'NONE', *, *, #110315, .F. ) ;
#46506 = CARTESIAN_POINT ( 'NONE',  ( 2.890489020090289962, 1507.108937781499890, 235.9439513786750240 ) ) ;
#46507 = CARTESIAN_POINT ( 'NONE',  ( -24.07937766809569879, 1410.986708645050157, 208.6133125710570084 ) ) ;
#46508 = ORIENTED_EDGE ( 'NONE', *, *, #19256, .T. ) ;
#46509 = CARTESIAN_POINT ( 'NONE',  ( 0.08494797014840001215, 1421.818460406029999, 227.4435403455979952 ) ) ;
#46510 = CARTESIAN_POINT ( 'NONE',  ( -7.198880892473511928, 1419.144553764449938, 195.5038830598559798 ) ) ;
#46511 = CARTESIAN_POINT ( 'NONE',  ( -14.76404367679999829, 1479.765582119930059, 230.2923287122980014 ) ) ;
#46512 = CARTESIAN_POINT ( 'NONE',  ( 16.77192111138402453, 1526.333389947941896, 234.9129815758702762 ) ) ;
#46513 = ORIENTED_EDGE ( 'NONE', *, *, #60243, .T. ) ;
#46514 = CARTESIAN_POINT ( 'NONE',  ( 11.73704819359999973, 1426.695975325029849, 144.1715469084980157 ) ) ;
#46515 = CARTESIAN_POINT ( 'NONE',  ( -12.93742170084479959, 1415.431750870119913, 221.3405841367710138 ) ) ;
#46516 = CARTESIAN_POINT ( 'NONE',  ( -109.0700388966839967, 1384.901248464930177, 297.1296046054879980 ) ) ;
#46517 = ORIENTED_EDGE ( 'NONE', *, *, #45206, .T. ) ;
#46518 = CARTESIAN_POINT ( 'NONE',  ( -1.711311266675000109, 1516.591755933730155, 203.3510257909670145 ) ) ;
#46519 = ORIENTED_EDGE ( 'NONE', *, *, #10545, .F. ) ;
#46520 = CARTESIAN_POINT ( 'NONE',  ( 11.86211521484639952, 1432.057615692780018, 149.9751993002209929 ) ) ;
#46521 = CIRCLE ( 'NONE', #28595, 2.000000000000003109 ) ;
#46522 = CARTESIAN_POINT ( 'NONE',  ( 2.789312393583509131, 1478.277622718212115, 199.0202689340788140 ) ) ;
#46523 = VERTEX_POINT ( 'NONE', #34076 ) ;
#46524 = ORIENTED_EDGE ( 'NONE', *, *, #43271, .T. ) ;
#46525 = CARTESIAN_POINT ( 'NONE',  ( -10.68970859486899805, 1481.192556119350229, 208.4617474437989983 ) ) ;
#46526 = CARTESIAN_POINT ( 'NONE',  ( 3.045280019940000305, 1464.258769156330118, 233.3054829794980094 ) ) ;
#46527 = CARTESIAN_POINT ( 'NONE',  ( 6.042363554874039977, 1498.446830258970067, 198.9500472058119840 ) ) ;
#46528 = CARTESIAN_POINT ( 'NONE',  ( -5.667442515161419614, 1470.223707235179972, 217.5701957336380019 ) ) ;
#46529 = CARTESIAN_POINT ( 'NONE',  ( 17.79764678428299973, 1452.291552866509846, 145.5855917355939937 ) ) ;
#46530 = AXIS2_PLACEMENT_3D ( 'NONE', #88358, #79957, #30083 ) ;
#46531 = CARTESIAN_POINT ( 'NONE',  ( 9.197260543180000525, 1420.703589484819986, 196.7538032495989739 ) ) ;
#46532 = CARTESIAN_POINT ( 'NONE',  ( -204.2714532754874881, 1526.382868172863937, 194.5341519463070767 ) ) ;
#46533 = CARTESIAN_POINT ( 'NONE',  ( -5.938382366523570433, 1494.685032631710101, 198.3270043733569992 ) ) ;
#46534 = CARTESIAN_POINT ( 'NONE',  ( -11.87490713740000103, 1433.006767100669776, 150.3951466367980174 ) ) ;
#46535 = CARTESIAN_POINT ( 'NONE',  ( 0.03661006106857637304, 1409.805696954575524, 233.1128360409267657 ) ) ;
#46537 = CARTESIAN_POINT ( 'NONE',  ( -105.5460946514699998, 1391.484849259569955, 304.2071873224919614 ) ) ;
#46536 = CARTESIAN_POINT ( 'NONE',  ( -13.53999783040000082, 1502.986154819089961, 208.9317388931999915 ) ) ;
#46538 = DIRECTION ( 'NONE',  ( 0.9858563016923833633, 0.000000000000000000, 0.1675928173085483863 ) ) ;
#46539 = CARTESIAN_POINT ( 'NONE',  ( -25.51896244293709870, 1509.784549317990013, 223.0112913589669859 ) ) ;
#46540 = CARTESIAN_POINT ( 'NONE',  ( -6.044020076205000258, 1511.752511073100095, 200.8248430530570090 ) ) ;
#46541 = ORIENTED_EDGE ( 'NONE', *, *, #85145, .F. ) ;
#46542 = CARTESIAN_POINT ( 'NONE',  ( 12.15345577959999979, 1413.272114225030009, 265.6112252686980355 ) ) ;
#46543 = CIRCLE ( 'NONE', #66212, 0.9999999999999947820 ) ;
#46544 = CARTESIAN_POINT ( 'NONE',  ( 19.05930086383896693, 1522.051704408389924, 195.1946787710221827 ) ) ;
#46545 = CARTESIAN_POINT ( 'NONE',  ( -88.01291097481920644, 1384.974171169579904, 308.0014400498420173 ) ) ;
#46546 = CARTESIAN_POINT ( 'NONE',  ( 4.337831292979999809, 1507.165484465889904, 219.9878051107990302 ) ) ;
#46547 = CARTESIAN_POINT ( 'NONE',  ( -11.71397119449999913, 1489.483175832489906, 212.5377882278690151 ) ) ;
#46549 = ORIENTED_EDGE ( 'NONE', *, *, #25465, .T. ) ;
#46548 = CARTESIAN_POINT ( 'NONE',  ( 3.535327672168380175, 1487.160996015089950, 197.6951163816430039 ) ) ;
#46550 = CARTESIAN_POINT ( 'NONE',  ( 4.506137960680000276, 1429.623679839590068, 216.5655692257590204 ) ) ;
#46551 = CARTESIAN_POINT ( 'NONE',  ( -2.878008746956259856, 1440.267634386450027, 157.3979731866919849 ) ) ;
#46552 = CARTESIAN_POINT ( 'NONE',  ( -15.94166470599999919, 1416.020783510179854, 209.6543286340279906 ) ) ;
#46553 = CARTESIAN_POINT ( 'NONE',  ( -2.076036472240859965, 1429.421786079320100, 199.9751262666950140 ) ) ;
#46554 = CARTESIAN_POINT ( 'NONE',  ( 12.80694033583499980, 1512.080583811389943, 224.7218690204669826 ) ) ;
#46555 = CARTESIAN_POINT ( 'NONE',  ( 4.473673856261621395, 1370.472484186452448, 209.0519328995294472 ) ) ;
#46556 = CARTESIAN_POINT ( 'NONE',  ( 17.14290233499820104, 1509.642557952590096, 233.9671050410080113 ) ) ;
#46557 = CARTESIAN_POINT ( 'NONE',  ( 8.508615264710758908, 1460.260753410110055, 204.1139426562619690 ) ) ;
#46558 = DIRECTION ( 'NONE',  ( 0.8090169943747140824, -7.703825410061002683E-33, 0.5877852522927943246 ) ) ;
#46559 = CARTESIAN_POINT ( 'NONE',  ( 16.60571044980000366, 1417.431011486929947, 226.8588397439980042 ) ) ;
#46560 = ADVANCED_FACE ( 'NONE', ( #59850 ), #105329, .F. ) ;
#46561 = CARTESIAN_POINT ( 'NONE',  ( -3.657996696819999727, 1474.872005729190050, 218.7367884669989735 ) ) ;
#46562 = CYLINDRICAL_SURFACE ( 'NONE', #76407, 2.000000000000003553 ) ;
#46563 = VECTOR ( 'NONE', #27261, 1000.000000000000000 ) ;
#46564 = CARTESIAN_POINT ( 'NONE',  ( -1.718203501584999904, 1516.898441858519845, 207.4215862561470090 ) ) ;
#46565 = CARTESIAN_POINT ( 'NONE',  ( 46.05259010380000007, 1440.913083222670139, 266.6770556958979910 ) ) ;
#46566 = CARTESIAN_POINT ( 'NONE',  ( -17.35552329220000090, 1409.519128615229874, 223.9298083007980154 ) ) ;
#46567 = CARTESIAN_POINT ( 'NONE',  ( 20.76392971010000110, 1435.368631235799967, 143.5555241923979963 ) ) ;
#46568 = CARTESIAN_POINT ( 'NONE',  ( 21.62573963749999706, 1508.012258617029829, 191.4661207822979918 ) ) ;
#46569 = CARTESIAN_POINT ( 'NONE',  ( -17.00059099016130304, 1410.433725695080057, 191.9734673053639824 ) ) ;
#46570 = CARTESIAN_POINT ( 'NONE',  ( -3.721063415729999695E-09, 1475.837061091930082, 266.9611530633980010 ) ) ;
#46571 = DIRECTION ( 'NONE',  ( -0.000000000000000000, -1.000000000000000000, -0.000000000000000000 ) ) ;
#46572 = CARTESIAN_POINT ( 'NONE',  ( 0.8350686643532178044, 1524.382868172863937, 177.3106345060153046 ) ) ;
#46573 = CARTESIAN_POINT ( 'NONE',  ( 0.2173304821316540125, 1453.251628194559999, 183.2425976906270080 ) ) ;
#46574 = CARTESIAN_POINT ( 'NONE',  ( -12.83650301490549950, 1408.840943845570109, 203.6725700213090136 ) ) ;
#46575 = CARTESIAN_POINT ( 'NONE',  ( -15.56083348049999948, 1415.425433635630043, 200.9032378748180179 ) ) ;
#46576 = AXIS2_PLACEMENT_3D ( 'NONE', #80694, #28078, #10742 ) ;
#46577 = CARTESIAN_POINT ( 'NONE',  ( 17.06401309437439906, 1526.329757971584968, 181.0652997614131721 ) ) ;
#46578 = CARTESIAN_POINT ( 'NONE',  ( -7.749623004274919680, 1383.351629194430188, 218.8775256501539843 ) ) ;
#46579 = CARTESIAN_POINT ( 'NONE',  ( 3.222662844351010136, 1456.191203615270069, 219.2431310769710251 ) ) ;
#46580 = CARTESIAN_POINT ( 'NONE',  ( -37.28324836091690742, 1436.551445511060138, 134.0999999968369991 ) ) ;
#46581 = FACE_OUTER_BOUND ( 'NONE', #53820, .T. ) ;
#46582 = EDGE_LOOP ( 'NONE', ( #14081, #96613, #79821, #64917, #67580, #15208, #48265, #79563 ) ) ;
#46583 = CARTESIAN_POINT ( 'NONE',  ( 18.86688640473580847, 1511.187213306747708, 180.7825021045438518 ) ) ;
#46584 = CARTESIAN_POINT ( 'NONE',  ( -1.893628906283649993, 1408.979187365889857, 223.9928269826189933 ) ) ;
#46585 = CARTESIAN_POINT ( 'NONE',  ( -32.02808312589908013, 1512.187213306747481, 221.9649204700466782 ) ) ;
#46586 = CARTESIAN_POINT ( 'NONE',  ( -5.534100668969379910, 1464.371862158079921, 199.5915835189479992 ) ) ;
#46587 = CARTESIAN_POINT ( 'NONE',  ( 15.16119009004890117, 1509.174112450859866, 232.9869830570750082 ) ) ;
#46588 = CARTESIAN_POINT ( 'NONE',  ( -30.19712123989999952, 1467.538238601129933, 267.1520868254980314 ) ) ;
#46589 = CARTESIAN_POINT ( 'NONE',  ( -11.84446372125409930, 1481.644281931980004, 209.8205016465489621 ) ) ;
#46590 = CARTESIAN_POINT ( 'NONE',  ( 18.90776566690000138, 1416.839648768830102, 210.0259813939200058 ) ) ;
#46591 = CARTESIAN_POINT ( 'NONE',  ( 1.347412987175395260, 1395.960113085665625, 217.1218459616980283 ) ) ;
#46592 = CARTESIAN_POINT ( 'NONE',  ( -100.5338213842030086, 1384.599842449589914, 310.8803881067170209 ) ) ;
#46593 = CARTESIAN_POINT ( 'NONE',  ( -42.80917332632159855, 1384.997012664380009, 215.7662912984700085 ) ) ;
#46594 = CARTESIAN_POINT ( 'NONE',  ( -12.05523474180890098, 1491.092627158069945, 206.8423379236589881 ) ) ;
#46595 = CARTESIAN_POINT ( 'NONE',  ( -4.788487179430729768, 1508.551704408389924, 205.6544253393599888 ) ) ;
#46596 = LINE ( 'NONE', #72348, #55686 ) ;
#46597 = CARTESIAN_POINT ( 'NONE',  ( 17.60627569411529691, 1410.895669416499913, 224.1775087544040161 ) ) ;
#46599 = ORIENTED_EDGE ( 'NONE', *, *, #68110, .F. ) ;
#46598 = CARTESIAN_POINT ( 'NONE',  ( 0.4877217612525719947, 1418.262951728039980, 184.7316173986440333 ) ) ;
#46600 = CARTESIAN_POINT ( 'NONE',  ( -109.4843783879999961, 1384.890515631779863, 311.2841057952589949 ) ) ;
#46601 = EDGE_CURVE ( 'NONE', #108746, #60035, #61826, .T. ) ;
#46602 = DIRECTION ( 'NONE',  ( -9.500914144214121536E-47, 1.000000000000000000, -1.836970198721029688E-16 ) ) ;
#46603 = EDGE_CURVE ( 'NONE', #86231, #87558, #27330, .T. ) ;
#46604 = EDGE_CURVE ( 'NONE', #36273, #59045, #85431, .T. ) ;
#46605 = CARTESIAN_POINT ( 'NONE',  ( 23.97466837309999832, 1430.490890388329944, 207.3419347240379977 ) ) ;
#46606 = CARTESIAN_POINT ( 'NONE',  ( -12.61566532500000015, 1416.819756528530206, 194.9201883977979719 ) ) ;
#46607 = CIRCLE ( 'NONE', #75209, 2.000000000000001776 ) ;
#46608 = CARTESIAN_POINT ( 'NONE',  ( 0.2270307469910020082, 1422.992384322039925, 192.4621272340990004 ) ) ;
#46609 = ADVANCED_FACE ( 'NONE', ( #90959 ), #37187, .T. ) ;
#46610 = CARTESIAN_POINT ( 'NONE',  ( 23.85787685490000243, 1410.668016354230076, 210.4985967482580236 ) ) ;
#46611 = B_SPLINE_SURFACE_WITH_KNOTS ( 'NONE', 5, 5, ( 
 ( #64887, #81101, #65991, #107957, #100113, #23396 ),
 ( #64330, #14984, #84948, #67089, #34561, #59238 ),
 ( #101191, #24489, #50287, #101748, #25036, #9366 ),
 ( #67636, #60331, #109621, #43530, #68201, #68744 ),
 ( #440, #58675, #50817, #986, #77673, #84416 ),
 ( #102847, #42976, #15531, #26140, #92810, #76562 ) ),
 .UNSPECIFIED., .F., .F., .F.,
 ( 6, 6 ),
 ( 6, 6 ),
 ( 0.8543875779139999960, 1.193533517340000127 ),
 ( 0.000000000000000000, 2.000000000000000000 ),
 .UNSPECIFIED. ) ;
#46612 = CARTESIAN_POINT ( 'NONE',  ( 3.914929521479999952, 1435.141524774260006, 184.8876600372980192 ) ) ;
#46613 = ADVANCED_FACE ( 'NONE', ( #82000 ), #41145, .F. ) ;
#46614 = CARTESIAN_POINT ( 'NONE',  ( -16.51469981520000019, 1466.007824952989949, 220.7976724296989914 ) ) ;
#46615 = FACE_OUTER_BOUND ( 'NONE', #10053, .T. ) ;
#46617 = CARTESIAN_POINT ( 'NONE',  ( 20.55201027734717201, 1526.382868172863937, 181.8366482295329263 ) ) ;
#46616 = CARTESIAN_POINT ( 'NONE',  ( -19.66678637224480397, 1522.051704408389924, 215.8936635741279986 ) ) ;
#46618 = CARTESIAN_POINT ( 'NONE',  ( -7.228663065755881689, 1512.913060387330006, 183.1074954935087646 ) ) ;
#46619 = DIRECTION ( 'NONE',  ( 0.000000000000000000, 1.000000000000000000, 0.000000000000000000 ) ) ;
#46620 = CARTESIAN_POINT ( 'NONE',  ( 17.07488731192356823, 1522.051704408389924, 205.4036014788801481 ) ) ;
#46621 = DIRECTION ( 'NONE',  ( 0.000000000000000000, 1.000000000000000000, 0.000000000000000000 ) ) ;
#46622 = CARTESIAN_POINT ( 'NONE',  ( 9.943976501839999926, 1365.461622992590037, 210.6218459616991936 ) ) ;
#46623 = CARTESIAN_POINT ( 'NONE',  ( -1.714334285315000095, 1516.699825673279975, 205.0952314524469955 ) ) ;
#46624 = CARTESIAN_POINT ( 'NONE',  ( -17.48302101486839888, 1486.143752436420073, 188.0522656724239994 ) ) ;
#46625 = CARTESIAN_POINT ( 'NONE',  ( -11.39483696856016692, 1422.053277916610568, 210.6383599177140695 ) ) ;
#46627 = VERTEX_POINT ( 'NONE', #75829 ) ;
#46626 = CARTESIAN_POINT ( 'NONE',  ( -68.18010506664271020, 1379.746744738860116, 279.6916017517709747 ) ) ;
#46628 = ORIENTED_EDGE ( 'NONE', *, *, #15063, .T. ) ;
#46629 = CARTESIAN_POINT ( 'NONE',  ( 28.75306184379999763, 1509.589359938030157, 209.8852704373689733 ) ) ;
#46630 = VERTEX_POINT ( 'NONE', #101545 ) ;
#46631 = CARTESIAN_POINT ( 'NONE',  ( -105.7844069010000112, 1378.913060387289988, 304.5472711634590155 ) ) ;
#46632 = CARTESIAN_POINT ( 'NONE',  ( -109.8260976820000110, 1384.930814608760102, 311.3808200542590043 ) ) ;
#46634 = CARTESIAN_POINT ( 'NONE',  ( 1.279965696769999939, 1508.893017011729853, 179.9879573282979948 ) ) ;
#46633 = CARTESIAN_POINT ( 'NONE',  ( 15.74014332448429876, 1412.735343691740127, 191.4587741565329964 ) ) ;
#46635 = CARTESIAN_POINT ( 'NONE',  ( 12.00000000000000000, 1443.913060387330006, 150.5878346084980137 ) ) ;
#46636 = EDGE_CURVE ( 'NONE', #22353, #93538, #43152, .T. ) ;
#46637 = CARTESIAN_POINT ( 'NONE',  ( -24.35936372944500050, 1451.998951890219814, 137.0312813218010035 ) ) ;
#46638 = CARTESIAN_POINT ( 'NONE',  ( 12.13968626136060891, 1436.959392319449307, 151.4453562942360350 ) ) ;
#46639 = CARTESIAN_POINT ( 'NONE',  ( 13.94099194679999876, 1410.772699170629949, 228.0747510220979848 ) ) ;
#46640 = CARTESIAN_POINT ( 'NONE',  ( 7.396059631071099538, 1483.223942348629862, 217.9804716342530071 ) ) ;
#46641 = SURFACE_STYLE_USAGE ( .BOTH. , #10819 ) ;
#46642 = EDGE_CURVE ( 'NONE', #93372, #86029, #246, .T. ) ;
#46643 = CARTESIAN_POINT ( 'NONE',  ( 41.56910739862709647, 1442.487573087749979, 134.0999999980959956 ) ) ;
#46644 = CIRCLE ( 'NONE', #71926, 1.999236069818542960 ) ;
#46645 = CARTESIAN_POINT ( 'NONE',  ( 12.24108702360000045, 1428.408480395390143, 194.9166229853989876 ) ) ;
#46646 = ORIENTED_EDGE ( 'NONE', *, *, #68566, .T. ) ;
#46647 = CARTESIAN_POINT ( 'NONE',  ( 14.57896927624650019, 1436.094750401150122, 149.8401917988270213 ) ) ;
#46648 = CARTESIAN_POINT ( 'NONE',  ( -17.19011713638783334, 1410.879030080967823, 226.0567197966691992 ) ) ;
#46649 = VERTEX_POINT ( 'NONE', #102112 ) ;
#46650 = VERTEX_POINT ( 'NONE', #25946 ) ;
#46651 = EDGE_CURVE ( 'NONE', #97278, #46489, #1714, .T. ) ;
#46652 = ORIENTED_EDGE ( 'NONE', *, *, #24671, .T. ) ;
#46653 = CARTESIAN_POINT ( 'NONE',  ( -5.763076042985000313, 1514.407352313670117, 216.7876711347169874 ) ) ;
#46654 = CARTESIAN_POINT ( 'NONE',  ( 16.66011979181740443, 1513.969110093212976, 195.1663535919080914 ) ) ;
#46655 = AXIS2_PLACEMENT_3D ( 'NONE', #18450, #69466, #36930 ) ;
#46656 = CARTESIAN_POINT ( 'NONE',  ( 6.009315719639841014, 1451.457099272296318, 153.4908535104837313 ) ) ;
#46657 = CARTESIAN_POINT ( 'NONE',  ( -7.545178787140000232, 1384.911017756160163, 219.0875996242590134 ) ) ;
#46658 = CARTESIAN_POINT ( 'NONE',  ( -15.81087456010765102, 1450.970563601593767, 221.9774777022516332 ) ) ;
#46659 = CARTESIAN_POINT ( 'NONE',  ( -62.44511414011146400, 1379.732285075670234, 266.8351904209325198 ) ) ;
#46660 = CARTESIAN_POINT ( 'NONE',  ( -0.1571152812289989820, 1465.182248420690030, 198.5055488938989754 ) ) ;
#46661 = CARTESIAN_POINT ( 'NONE',  ( -1.320018102479999955, 1507.624001479029857, 232.0809353007979894 ) ) ;
#46662 = CARTESIAN_POINT ( 'NONE',  ( 9.790177624210000928, 1414.971287085330005, 195.6150972186979971 ) ) ;
#46663 = CARTESIAN_POINT ( 'NONE',  ( -64.86421170961099847, 1384.704012963549985, 254.7553430863480060 ) ) ;
#46664 = ORIENTED_EDGE ( 'NONE', *, *, #41222, .F. ) ;
#46665 = CARTESIAN_POINT ( 'NONE',  ( -4.045182518055000287, 1517.057265928030120, 207.4180663268770104 ) ) ;
#46666 = VERTEX_POINT ( 'NONE', #63470 ) ;
#46667 = CARTESIAN_POINT ( 'NONE',  ( 27.31982573739979969, 1440.913060387330006, 245.8751062284599982 ) ) ;
#46668 = CONICAL_SURFACE ( 'NONE', #78767, 1.000000000000009104, 0.7853981633970000820 ) ;
#46669 = CARTESIAN_POINT ( 'NONE',  ( -17.21313104309999886, 1509.582386186229769, 184.6661624875980010 ) ) ;
#46670 = ORIENTED_EDGE ( 'NONE', *, *, #108261, .F. ) ;
#46671 = CARTESIAN_POINT ( 'NONE',  ( -33.93390012576846715, 1451.576011116597783, 135.5842836269593192 ) ) ;
#46672 = CARTESIAN_POINT ( 'NONE',  ( -15.66085203299999762, 1409.459949385129903, 192.2846886866980185 ) ) ;
#46673 = CARTESIAN_POINT ( 'NONE',  ( -19.09790268268400126, 1508.458003811930212, 210.0050661408479868 ) ) ;
#46675 = CARTESIAN_POINT ( 'NONE',  ( -0.4558760921085245887, 1414.913060387330006, 225.2405208435152701 ) ) ;
#46674 = CARTESIAN_POINT ( 'NONE',  ( -24.67090459839999994, 1441.025736683209971, 210.6889990472880072 ) ) ;
#46676 = CARTESIAN_POINT ( 'NONE',  ( -9.215400547745700166, 1437.452820398420045, 212.6238575580420047 ) ) ;
#46677 = CARTESIAN_POINT ( 'NONE',  ( -5.619918030323759695, 1511.009256124219974, 201.4419183480959816 ) ) ;
#46678 = CARTESIAN_POINT ( 'NONE',  ( 1.770390159249999984, 1406.013915744430051, 266.9599398126979963 ) ) ;
#46679 = DIRECTION ( 'NONE',  ( -1.755985294532469921E-16, 1.000000000000000000, -1.338183447452831989E-16 ) ) ;
#46680 = LINE ( 'NONE', #20334, #110751 ) ;
#46682 = CARTESIAN_POINT ( 'NONE',  ( -11.60004869885203682, 1425.894669240205303, 137.5118602016662237 ) ) ;
#46681 = CARTESIAN_POINT ( 'NONE',  ( 2.887394341690000310, 1464.524587323030119, 235.8761363967979889 ) ) ;
#46683 = CARTESIAN_POINT ( 'NONE',  ( 2.486474742745000022, 1516.560253536979872, 216.0557253731069807 ) ) ;
#46684 = CARTESIAN_POINT ( 'NONE',  ( -3.865992865399999978, 1463.465618750590011, 228.4375626785990221 ) ) ;
#46685 = PRODUCT_RELATED_PRODUCT_CATEGORY ( 'part', '', ( #104493 ) ) ;
#46686 = CARTESIAN_POINT ( 'NONE',  ( -0.04370337965792400053, 1508.780601165080043, 179.8640435178710106 ) ) ;
#46687 = CARTESIAN_POINT ( 'NONE',  ( 19.42500282749999840, 1440.913060387330006, 212.4633492400480179 ) ) ;
#46688 = CARTESIAN_POINT ( 'NONE',  ( -4.609064341505000328, 1516.723920667490120, 211.9995909164769898 ) ) ;
#46689 = CARTESIAN_POINT ( 'NONE',  ( -19.82086717690000199, 1452.811554597929899, 208.9556627768919839 ) ) ;
#46690 = CARTESIAN_POINT ( 'NONE',  ( -4.044582423638403590, 1419.921508911728779, 137.0999999980979851 ) ) ;
#46692 = EDGE_LOOP ( 'NONE', ( #59214, #79818, #35014, #88851, #37493 ) ) ;
#46691 = CARTESIAN_POINT ( 'NONE',  ( -109.9987473089999952, 1389.430187130500144, 300.0861861933589694 ) ) ;
#46693 = CARTESIAN_POINT ( 'NONE',  ( -1.159637561150000051, 1415.063410489829948, 226.6648382762980134 ) ) ;
#46694 = CARTESIAN_POINT ( 'NONE',  ( 19.57999186420000015, 1459.737765858830016, 238.2202666691980255 ) ) ;
#46695 = CARTESIAN_POINT ( 'NONE',  ( -11.86606752090000150, 1432.333718217379783, 149.9825819519979859 ) ) ;
#46696 = CARTESIAN_POINT ( 'NONE',  ( -15.01736473799999949, 1415.953171031319926, 205.5614245712289971 ) ) ;
#46697 = DIRECTION ( 'NONE',  ( 0.000000000000000000, 0.000000000000000000, 1.000000000000000000 ) ) ;
#46698 = CARTESIAN_POINT ( 'NONE',  ( 16.69297358002692278, 1526.382868172864164, 183.6963177704308521 ) ) ;
#46699 = EDGE_CURVE ( 'NONE', #38044, #9577, #4097, .T. ) ;
#46701 = DIRECTION ( 'NONE',  ( 0.5877852522924568168, 0.000000000000000000, -0.8090169943749592196 ) ) ;
#46700 = CARTESIAN_POINT ( 'NONE',  ( -19.92408690999999976, 1457.445828243930009, 225.3974416310980189 ) ) ;
#46702 = CARTESIAN_POINT ( 'NONE',  ( 19.41157449629999832, 1457.417846740989944, 209.1218459616989946 ) ) ;
#46703 = CARTESIAN_POINT ( 'NONE',  ( -104.5730503306040049, 1380.111946902090040, 306.5319961363489369 ) ) ;
#46704 = ORIENTED_EDGE ( 'NONE', *, *, #16149, .T. ) ;
#46705 = CARTESIAN_POINT ( 'NONE',  ( 1.703779605225000049, 1517.057265928030120, 205.0766634521770015 ) ) ;
#46706 = CARTESIAN_POINT ( 'NONE',  ( 0.8854628104720000392, 1405.995467260429905, 266.9608410729979937 ) ) ;
#46707 = EDGE_CURVE ( 'NONE', #92866, #41219, #108581, .T. ) ;
#46708 = AXIS2_PLACEMENT_3D ( 'NONE', #100571, #31715, #109542 ) ;
#46709 = CARTESIAN_POINT ( 'NONE',  ( -1.842962231260000028, 1515.492058413689847, 213.2603893528589936 ) ) ;
#46710 = CARTESIAN_POINT ( 'NONE',  ( 39.82896661013450057, 1456.864206082610053, 270.1537018815570264 ) ) ;
#46711 = CARTESIAN_POINT ( 'NONE',  ( -2.735359696209999747, 1470.857183403589943, 189.2159460739989925 ) ) ;
#46712 = DIRECTION ( 'NONE',  ( 0.000000000000000000, 1.000000000000000000, 0.000000000000000000 ) ) ;
#46713 = AXIS2_PLACEMENT_3D ( 'NONE', #95953, #88671, #63491 ) ;
#46714 = CARTESIAN_POINT ( 'NONE',  ( -10.33299300126450149, 1447.717326489380184, 209.8084994042759774 ) ) ;
#46715 = EDGE_CURVE ( 'NONE', #56418, #23046, #79703, .T. ) ;
#46716 = CARTESIAN_POINT ( 'NONE',  ( -4.468118146560000170, 1458.475370017489922, 218.8772509106790096 ) ) ;
#46717 = CARTESIAN_POINT ( 'NONE',  ( -1.557202951210026276, 1451.015816330957477, 183.5890866117867688 ) ) ;
#46718 = CARTESIAN_POINT ( 'NONE',  ( 1.967245043674230365, 1450.337415823809806, 154.7913109945830286 ) ) ;
#46719 = CARTESIAN_POINT ( 'NONE',  ( -14.40791762929059949, 1416.384967875099846, 221.3406101171449905 ) ) ;
#46720 = DIRECTION ( 'NONE',  ( -1.000000000000000000, 0.000000000000000000, 0.000000000000000000 ) ) ;
#46721 = ORIENTED_EDGE ( 'NONE', *, *, #89828, .T. ) ;
#46722 = CARTESIAN_POINT ( 'NONE',  ( -26.42714720800000094, 1437.883259617029807, 243.9198229606980135 ) ) ;
#46723 = CARTESIAN_POINT ( 'NONE',  ( 5.586270675034979760, 1465.491174728670103, 200.8384121407760006 ) ) ;
#46724 = TOROIDAL_SURFACE ( 'NONE', #44968, 9.522913805089999073, 1.000000000000000000 ) ;
#46725 = CARTESIAN_POINT ( 'NONE',  ( -0.3399431336819999649, 1476.108518450929978, 267.8539949209979909 ) ) ;
#46726 = CARTESIAN_POINT ( 'NONE',  ( 20.49831092009999978, 1496.178973653789853, 204.1013708937389879 ) ) ;
#46727 = CARTESIAN_POINT ( 'NONE',  ( -18.34590456075780196, 1416.851343895820037, 208.8605686865189739 ) ) ;
#46728 = CARTESIAN_POINT ( 'NONE',  ( -3.207697512962450315, 1448.279240478991369, 184.6677887077926528 ) ) ;
#46729 = CARTESIAN_POINT ( 'NONE',  ( -40.37520412227119948, 1384.785868538820068, 242.7915335778529879 ) ) ;
#46730 = CARTESIAN_POINT ( 'NONE',  ( 1.174755966547918140, 1431.055736453459531, 217.8297097953777666 ) ) ;
#46731 = CARTESIAN_POINT ( 'NONE',  ( -10.83907793900000094, 1482.736899269390051, 205.3800505913289953 ) ) ;
#46732 = CARTESIAN_POINT ( 'NONE',  ( 8.302022980286720255, 1511.419866572826550, 204.7917934253724184 ) ) ;
#46733 = ADVANCED_FACE ( 'NONE', ( #87548 ), #24133, .F. ) ;
#46734 = CARTESIAN_POINT ( 'NONE',  ( -11.07153876272299975, 1396.299687040369918, 208.9417196923349991 ) ) ;
#46735 = EDGE_CURVE ( 'NONE', #22237, #96609, #72509, .T. ) ;
#46736 = VECTOR ( 'NONE', #83722, 1000.000000000000000 ) ;
#46738 = B_SPLINE_CURVE_WITH_KNOTS ( 'NONE', 3,
 ( #30185, #64377, #110771, #93960 ),
 .UNSPECIFIED., .F., .F.,
 ( 4, 4 ),
 ( 0.000000000000000000, 1.000000000000000000 ),
 .UNSPECIFIED. ) ;
#46737 = CARTESIAN_POINT ( 'NONE',  ( -15.82161016549999921, 1420.644138379529750, 227.0290855803980037 ) ) ;
#46739 = CARTESIAN_POINT ( 'NONE',  ( 19.26863053809116622, 1456.090792970590655, 225.0961701050973431 ) ) ;
#46740 = VERTEX_POINT ( 'NONE', #48856 ) ;
#46741 = FACE_OUTER_BOUND ( 'NONE', #69469, .T. ) ;
#46742 = CARTESIAN_POINT ( 'NONE',  ( 2.760778241670000188, 1409.009468887930097, 230.1977506513979961 ) ) ;
#46743 = CARTESIAN_POINT ( 'NONE',  ( -17.41081140942853622, 1485.005952666161875, 188.5080410486085896 ) ) ;
#46744 = CIRCLE ( 'NONE', #75352, 7.799999999999999822 ) ;
#46746 = FACE_OUTER_BOUND ( 'NONE', #29895, .T. ) ;
#46745 = CARTESIAN_POINT ( 'NONE',  ( 11.48672039610000084, 1426.428532722830141, 126.2854488628979936 ) ) ;
#46747 = FACE_OUTER_BOUND ( 'NONE', #20835, .T. ) ;
#46748 = CARTESIAN_POINT ( 'NONE',  ( -11.23388613411650105, 1443.913060387330006, 151.7784653951599978 ) ) ;
#46749 = EDGE_CURVE ( 'NONE', #43965, #61502, #32433, .T. ) ;
#46750 = CARTESIAN_POINT ( 'NONE',  ( 5.003848121975000396, 1517.005755693489846, 201.7875176594370146 ) ) ;
#46751 = CARTESIAN_POINT ( 'NONE',  ( 8.377020731070000892, 1427.910351821989934, 212.6460221678989910 ) ) ;
#46752 = CARTESIAN_POINT ( 'NONE',  ( 20.56230369369999877, 1477.111288992490017, 217.7195332328089989 ) ) ;
#46753 = CARTESIAN_POINT ( 'NONE',  ( 4.486266698770000616, 1509.079604303730093, 179.9451462963979793 ) ) ;
#46754 = CARTESIAN_POINT ( 'NONE',  ( 7.615555629554999761, 1511.534866634170157, 206.2833989651869899 ) ) ;
#46755 = CARTESIAN_POINT ( 'NONE',  ( -60.58607047561810077, 1378.469422833939916, 271.2016459589009969 ) ) ;
#46756 = CIRCLE ( 'NONE', #64657, 1.999999999999997780 ) ;
#46757 = CARTESIAN_POINT ( 'NONE',  ( 8.251048879710380035, 1367.474174444426126, 210.6218459616987957 ) ) ;
#46758 = EDGE_CURVE ( 'NONE', #73741, #104178, #37798, .T. ) ;
#46760 = EDGE_LOOP ( 'NONE', ( #63366, #37454, #58206, #84205 ) ) ;
#46759 = CARTESIAN_POINT ( 'NONE',  ( -21.77664080601369889, 1379.664485263579991, 213.4127619154490105 ) ) ;
#46761 = ORIENTED_EDGE ( 'NONE', *, *, #70127, .F. ) ;
#46762 = CARTESIAN_POINT ( 'NONE',  ( -5.639077333919999546, 1396.170382963030079, 198.9228296477979825 ) ) ;
#46763 = CARTESIAN_POINT ( 'NONE',  ( 1.156245593104790137, 1474.789461591380132, 235.6542973942920014 ) ) ;
#46764 = CARTESIAN_POINT ( 'NONE',  ( -4.440892098499999806E-15, 1519.913060387329779, 231.7062449670980300 ) ) ;
#46765 = CARTESIAN_POINT ( 'NONE',  ( -8.213194891504999262, 1511.437978678640093, 213.1815177657570075 ) ) ;
#46767 = CARTESIAN_POINT ( 'NONE',  ( -1.361090702285459919, 1413.800366288759960, 185.4570810730789958 ) ) ;
#46766 = CARTESIAN_POINT ( 'NONE',  ( -8.591590428069999064, 1384.539102583910108, 218.6519172601589958 ) ) ;
#46768 = CARTESIAN_POINT ( 'NONE',  ( 14.72486392259999910, 1429.763008465929943, 190.7271437690980065 ) ) ;
#46769 = CARTESIAN_POINT ( 'NONE',  ( -2.170363546252639608, 1464.474365425050109, 199.1286919944959948 ) ) ;
#46770 = CARTESIAN_POINT ( 'NONE',  ( -36.84775941671910005, 1449.744939508739890, 136.2617221972240031 ) ) ;
#46771 = CARTESIAN_POINT ( 'NONE',  ( 39.80563939443820232, 1439.297435335050068, 136.4608509805550227 ) ) ;
#46772 = CARTESIAN_POINT ( 'NONE',  ( 4.090111291624164203, 1370.944973062717054, 208.3718459617010978 ) ) ;
#46773 = FACE_OUTER_BOUND ( 'NONE', #93818, .T. ) ;
#46774 = CARTESIAN_POINT ( 'NONE',  ( 11.55327403699999955, 1430.567211606730098, 150.9659738814980017 ) ) ;
#46775 = CARTESIAN_POINT ( 'NONE',  ( -15.24750712096500038, 1514.857962383129916, 223.5728236591669997 ) ) ;
#46776 = ORIENTED_EDGE ( 'NONE', *, *, #80306, .F. ) ;
#46777 = CARTESIAN_POINT ( 'NONE',  ( -12.53380499169999851, 1442.773887286369927, 169.4755105685979970 ) ) ;
#46778 = CARTESIAN_POINT ( 'NONE',  ( 21.15380500792148766, 1525.425686270224105, 234.2557952880171683 ) ) ;
#46779 = ORIENTED_EDGE ( 'NONE', *, *, #73249, .T. ) ;
#46780 = EDGE_CURVE ( 'NONE', #10547, #31839, #107198, .T. ) ;
#46781 = ORIENTED_EDGE ( 'NONE', *, *, #23951, .F. ) ;
#46782 = CARTESIAN_POINT ( 'NONE',  ( -19.57912521677359763, 1488.016130565860067, 228.2702076737010088 ) ) ;
#46783 = DIRECTION ( 'NONE',  ( 0.000000000000000000, 0.000000000000000000, 1.000000000000000000 ) ) ;
#46784 = CARTESIAN_POINT ( 'NONE',  ( -17.36305420999961058, 1410.600123101027066, 225.7636173774992017 ) ) ;
#46785 = ADVANCED_FACE ( 'NONE', ( #107635 ), #28155, .F. ) ;
#46786 = CARTESIAN_POINT ( 'NONE',  ( -7.326795561505000443, 1516.760434454289907, 214.9020780475669881 ) ) ;
#46787 = CARTESIAN_POINT ( 'NONE',  ( -12.31367108914779962, 1378.373004075840072, 209.7324437289769890 ) ) ;
#46788 =( GEOMETRIC_REPRESENTATION_CONTEXT ( 3 ) GLOBAL_UNCERTAINTY_ASSIGNED_CONTEXT ( ( #9894 ) ) GLOBAL_UNIT_ASSIGNED_CONTEXT ( ( #22054, #6938, #7494 ) ) REPRESENTATION_CONTEXT ( 'NONE', 'WORKASPACE' ) );
#46789 = ORIENTED_EDGE ( 'NONE', *, *, #45256, .F. ) ;
#46790 = CARTESIAN_POINT ( 'NONE',  ( -8.956458691531819838, 1509.358275544009985, 180.2336362669479968 ) ) ;
#46791 = CARTESIAN_POINT ( 'NONE',  ( -46.19755678469999793, 1379.154583033749986, 231.0255711761590192 ) ) ;
#46792 = VECTOR ( 'NONE', #91116, 1000.000000000000000 ) ;
#46793 = CARTESIAN_POINT ( 'NONE',  ( 18.88659680459999990, 1416.522662136229883, 210.6651046700080201 ) ) ;
#46794 = CARTESIAN_POINT ( 'NONE',  ( -1.133517003235000153, 1516.713079096360161, 204.5117660986770147 ) ) ;
#46795 = CARTESIAN_POINT ( 'NONE',  ( 10.69530615799999929, 1492.057806673789855, 212.3894089256490076 ) ) ;
#46796 = CARTESIAN_POINT ( 'NONE',  ( -41.79940509948184513, 1437.492528948050449, 269.6436970879940418 ) ) ;
#46797 = CARTESIAN_POINT ( 'NONE',  ( -2.573074615509999941, 1409.002914132830028, 231.1540680731980046 ) ) ;
#46799 = ORIENTED_EDGE ( 'NONE', *, *, #77567, .T. ) ;
#46798 = DIRECTION ( 'NONE',  ( 0.4857255149070415778, -0.7475168846447919346, -0.4530885469080344619 ) ) ;
#46800 = CARTESIAN_POINT ( 'NONE',  ( -2.344512155952720001, 1516.526058380829909, 201.4130301786289863 ) ) ;
#46801 = CARTESIAN_POINT ( 'NONE',  ( 28.30919303740000004, 1508.136605797730226, 209.0041157894929995 ) ) ;
#46802 = CARTESIAN_POINT ( 'NONE',  ( -8.753528060440000758, 1383.864184473070054, 218.4105340633189769 ) ) ;
#46803 = CARTESIAN_POINT ( 'NONE',  ( 15.66042904549793136, 1506.491018775014027, 224.6173112146069002 ) ) ;
#46804 = VECTOR ( 'NONE', #68908, 1000.000000000000000 ) ;
#46805 = CARTESIAN_POINT ( 'NONE',  ( 28.35905216135870077, 1416.639651061350150, 270.3509323902579808 ) ) ;
#46806 = CARTESIAN_POINT ( 'NONE',  ( -4.028630622785000170, 1516.812923327049930, 212.5819478221170016 ) ) ;
#46807 = CARTESIAN_POINT ( 'NONE',  ( -68.17091063920000238, 1379.746761204979975, 278.7818561045589831 ) ) ;
#46808 = CARTESIAN_POINT ( 'NONE',  ( 22.68006499860000247, 1409.705091528429875, 208.7629400170540066 ) ) ;
#46809 = CARTESIAN_POINT ( 'NONE',  ( 0.008918347722598321536, 1508.393983269119872, 237.8902324756037672 ) ) ;
#46810 = CARTESIAN_POINT ( 'NONE',  ( 16.53404221824990117, 1428.071160471989970, 201.6834493251120080 ) ) ;
#46811 = CARTESIAN_POINT ( 'NONE',  ( -7.709431855391500221, 1516.549587951120202, 211.8473045898290081 ) ) ;
#46812 = CARTESIAN_POINT ( 'NONE',  ( 1.133653140995000141, 1516.978425811520083, 209.8592968530090275 ) ) ;
#46813 = CARTESIAN_POINT ( 'NONE',  ( 4.363122683464830232, 1421.971318488559973, 183.8271341761570170 ) ) ;
#46814 = CARTESIAN_POINT ( 'NONE',  ( -0.4152942141409999843, 1420.456388890930157, 233.6206558093980163 ) ) ;
#46815 =( BOUNDED_CURVE ( )  B_SPLINE_CURVE ( 3, ( #14223, #107743, #91500, #81415 ),
 .UNSPECIFIED., .F., .F. ) 
 B_SPLINE_CURVE_WITH_KNOTS ( ( 4, 4 ),
 ( 4.673418987722709694, 4.822346547659980054 ),
 .UNSPECIFIED. ) 
 CURVE ( )  GEOMETRIC_REPRESENTATION_ITEM ( )  RATIONAL_B_SPLINE_CURVE ( ( 1.000000000000000000, 0.9981525690389736472, 0.9981525690389736472, 1.000000000000000000 ) ) 
 REPRESENTATION_ITEM ( '' )  );
#46816 = CARTESIAN_POINT ( 'NONE',  ( -73.55519582189999994, 1385.011955127469946, 298.9534985252589649 ) ) ;
#46817 = ORIENTED_EDGE ( 'NONE', *, *, #87858, .F. ) ;
#46819 = VECTOR ( 'NONE', #90022, 1000.000000000000114 ) ;
#46818 = CARTESIAN_POINT ( 'NONE',  ( -27.83627237203649685, 1385.243440311610129, 225.9367174611259941 ) ) ;
#46820 = CARTESIAN_POINT ( 'NONE',  ( -15.01814846036320006, 1514.214451730469818, 194.3960741685959874 ) ) ;
#46821 = CARTESIAN_POINT ( 'NONE',  ( -20.79161711910150245, 1507.840252237830100, 228.0156062829520067 ) ) ;
#46822 = CARTESIAN_POINT ( 'NONE',  ( -106.4049156021218465, 1391.248059910561551, 307.7491788416908776 ) ) ;
#46823 = CARTESIAN_POINT ( 'NONE',  ( 10.75070237740000145, 1423.976811909279832, 204.9811967931990182 ) ) ;
#46824 = CARTESIAN_POINT ( 'NONE',  ( 0.5096330788092879871, 1452.969753185240052, 183.2932557940929996 ) ) ;
#46825 = EDGE_CURVE ( 'NONE', #52145, #96903, #8461, .T. ) ;
#46827 = CARTESIAN_POINT ( 'NONE',  ( -4.212124233566025389, 1455.571073703328693, 200.6608987289929757 ) ) ;
#46826 = CARTESIAN_POINT ( 'NONE',  ( -0.7396922758749979732, 1517.135701590510052, 216.4591432822169850 ) ) ;
#46828 = CARTESIAN_POINT ( 'NONE',  ( 18.87155961639999902, 1509.015964899329902, 188.0102586092980061 ) ) ;
#46829 = CARTESIAN_POINT ( 'NONE',  ( 10.06738412557950113, 1469.597899895000182, 209.1389479632179871 ) ) ;
#46830 = ORIENTED_EDGE ( 'NONE', *, *, #88448, .F. ) ;
#46831 = CARTESIAN_POINT ( 'NONE',  ( 0.7396922377450010355, 1517.135701590510052, 201.7845486201169933 ) ) ;
#46832 = CARTESIAN_POINT ( 'NONE',  ( 28.77213281030099878, 1509.917805400869838, 206.8662417278609951 ) ) ;
#46833 = EDGE_LOOP ( 'NONE', ( #67045, #93247, #17235, #93060, #48103 ) ) ;
#46834 = AXIS2_PLACEMENT_3D ( 'NONE', #74092, #6854, #109882 ) ;
#46835 = CARTESIAN_POINT ( 'NONE',  ( 11.60004869884797429, 1426.654319849603780, 134.6710116165313877 ) ) ;
#46836 = DIRECTION ( 'NONE',  ( -0.03084237732693835901, -0.9990097606182641865, -0.03206627434332531140 ) ) ;
#46837 = CARTESIAN_POINT ( 'NONE',  ( 7.930811094041184006, 1423.727541757261861, 195.8483739583643342 ) ) ;
#46838 = CARTESIAN_POINT ( 'NONE',  ( 1.657211920199999966, 1442.925229136189955, 217.9916902927889737 ) ) ;
#46839 = CARTESIAN_POINT ( 'NONE',  ( -26.48205241774240193, 1508.638501742070048, 201.4894952595709867 ) ) ;
#46840 = EDGE_CURVE ( 'NONE', #75732, #51540, #17478, .T. ) ;
#46841 = CARTESIAN_POINT ( 'NONE',  ( -4.239021722809999559, 1446.365493693999952, 162.7142554342980247 ) ) ;
#46842 = CARTESIAN_POINT ( 'NONE',  ( -19.00435212720000422, 1425.942472208630079, 225.6636987373979935 ) ) ;
#46843 = CARTESIAN_POINT ( 'NONE',  ( -14.43917572210000166, 1435.432076402839812, 149.5787593319979862 ) ) ;
#46844 = CARTESIAN_POINT ( 'NONE',  ( -2.569508516276699961, 1464.905644613789718, 198.4146467863039902 ) ) ;
#46845 = CARTESIAN_POINT ( 'NONE',  ( 16.45201478129999728, 1509.487577403229807, 185.2161393109980168 ) ) ;
#46847 = CARTESIAN_POINT ( 'NONE',  ( -18.16584306366592116, 1435.617507662623666, 214.1170364969505044 ) ) ;
#46846 = CARTESIAN_POINT ( 'NONE',  ( -106.7279299509999930, 1391.913060387289988, 302.2165404876590173 ) ) ;
#46848 = FACE_OUTER_BOUND ( 'NONE', #70009, .T. ) ;
#46849 = ORIENTED_EDGE ( 'NONE', *, *, #93911, .T. ) ;
#46851 = EDGE_CURVE ( 'NONE', #107006, #76166, #20327, .T. ) ;
#46850 = CARTESIAN_POINT ( 'NONE',  ( -2.496058351850642065, 1410.375802693013156, 186.5499807929696772 ) ) ;
#46852 = CARTESIAN_POINT ( 'NONE',  ( -9.386420905929998781, 1508.551704408389924, 218.5291032798490107 ) ) ;
#46853 = CARTESIAN_POINT ( 'NONE',  ( -19.68364361505096483, 1521.951704408389787, 221.2357901429078879 ) ) ;
#46854 = CARTESIAN_POINT ( 'NONE',  ( 11.41287573240554032, 1427.618782186570115, 209.6357587079445182 ) ) ;
#46855 = CARTESIAN_POINT ( 'NONE',  ( -1.906495983305939756E-08, 1508.551704408389924, 214.1089243866270238 ) ) ;
#46856 = CARTESIAN_POINT ( 'NONE',  ( -18.56679401179999900, 1509.561427120029975, 231.0972437537980113 ) ) ;
#46857 = CARTESIAN_POINT ( 'NONE',  ( -3.017180836140621825, 1525.408327360769817, 241.3338531177342929 ) ) ;
#46858 = CARTESIAN_POINT ( 'NONE',  ( -13.24295770958712737, 1443.166206736402501, 186.8421231537473943 ) ) ;
#46859 = CARTESIAN_POINT ( 'NONE',  ( -17.11711237129999930, 1414.913528139930122, 207.5661155201680117 ) ) ;
#46860 = CARTESIAN_POINT ( 'NONE',  ( 3.902834784268570001, 1495.323243761410140, 220.8767705547660114 ) ) ;
#46861 = CARTESIAN_POINT ( 'NONE',  ( -2.775543834090889561, 1468.867531313959944, 187.4507025151330026 ) ) ;
#46862 = CARTESIAN_POINT ( 'NONE',  ( -15.36839037194300062, 1415.677402202079975, 209.1379692602760088 ) ) ;
#46863 = CARTESIAN_POINT ( 'NONE',  ( -109.4664803445590024, 1384.534987613060139, 311.2654761184969630 ) ) ;
#46864 = CARTESIAN_POINT ( 'NONE',  ( -0.3328841718826340279, 1516.837731796779963, 201.4048689279690052 ) ) ;
#46866 = ORIENTED_EDGE ( 'NONE', *, *, #97442, .F. ) ;
#46865 = CARTESIAN_POINT ( 'NONE',  ( 20.15452338710000291, 1507.845775801930131, 189.3412755345979690 ) ) ;
#46867 = CARTESIAN_POINT ( 'NONE',  ( 33.93019615848946557, 1524.726013923371283, 197.6607374645996344 ) ) ;
#46868 = EDGE_CURVE ( 'NONE', #71088, #64216, #7046, .T. ) ;
#46869 = CARTESIAN_POINT ( 'NONE',  ( 13.18795884192349988, 1512.495155157800127, 224.3903603686180190 ) ) ;
#46870 = ORIENTED_EDGE ( 'NONE', *, *, #62690, .T. ) ;
#46871 = ORIENTED_EDGE ( 'NONE', *, *, #52584, .F. ) ;
#46872 = CARTESIAN_POINT ( 'NONE',  ( 25.69821269425319699, 1461.615829411680124, 207.7065348595210139 ) ) ;
#46873 = CARTESIAN_POINT ( 'NONE',  ( 13.63495199149999948, 1509.148422029330050, 233.7524325507980052 ) ) ;
#46874 = CARTESIAN_POINT ( 'NONE',  ( 7.561666052370960678, 1423.087019363542595, 213.9609131946497200 ) ) ;
#46876 = CARTESIAN_POINT ( 'NONE',  ( -31.95512683489999617, 1440.913060389640123, 244.1805851169980031 ) ) ;
#46875 = CARTESIAN_POINT ( 'NONE',  ( 27.62485365530106307, 1417.942135513340645, 269.4472113980168047 ) ) ;
#46877 = EDGE_CURVE ( 'NONE', #32551, #9968, #92635, .T. ) ;
#46878 = CARTESIAN_POINT ( 'NONE',  ( -19.88572119940000249, 1484.728770958729910, 191.0592868864980005 ) ) ;
#46879 = CARTESIAN_POINT ( 'NONE',  ( -11.74481771089999960, 1433.726929579510170, 150.9290601731980246 ) ) ;
#46880 = ADVANCED_FACE ( 'NONE', ( #41119 ), #78478, .F. ) ;
#46881 = CIRCLE ( 'NONE', #89773, 3.000000000000002665 ) ;
#46882 = FACE_OUTER_BOUND ( 'NONE', #40092, .T. ) ;
#46883 = CARTESIAN_POINT ( 'NONE',  ( 11.61068082338428376, 1426.780165915954285, 135.1396153442166508 ) ) ;
#46884 = CARTESIAN_POINT ( 'NONE',  ( 8.237294568284330154, 1465.649939967559931, 214.5915065964550195 ) ) ;
#46885 = CARTESIAN_POINT ( 'NONE',  ( -2.038847259693655545, 1522.861859112239244, 244.9330574173661432 ) ) ;
#46886 = CARTESIAN_POINT ( 'NONE',  ( -0.7087989430410059910, 1515.130721759790049, 213.4495683292759907 ) ) ;
#46887 = CARTESIAN_POINT ( 'NONE',  ( -12.89608512423069975, 1434.724840024559853, 149.2206170422699927 ) ) ;
#46888 = CARTESIAN_POINT ( 'NONE',  ( -3.795278851281820298, 1476.619100922419875, 219.9733720370720107 ) ) ;
#46889 = CARTESIAN_POINT ( 'NONE',  ( 1.670893000356252323, 1361.439592909522844, 207.6218459616988241 ) ) ;
#46890 = EDGE_CURVE ( 'NONE', #66323, #101705, #49736, .T. ) ;
#46891 = CARTESIAN_POINT ( 'NONE',  ( 34.68852446352035201, 1522.861859112239472, 199.9946320047950508 ) ) ;
#46893 = ORIENTED_EDGE ( 'NONE', *, *, #107727, .T. ) ;
#46892 = CARTESIAN_POINT ( 'NONE',  ( 1.181658762251719971E-08, 1409.019473503670042, 260.8196857114169802 ) ) ;
#46894 = ORIENTED_EDGE ( 'NONE', *, *, #104242, .T. ) ;
#46895 = CARTESIAN_POINT ( 'NONE',  ( -11.86550914360719844, 1432.294685167699981, 149.9822461645989904 ) ) ;
#46896 = CARTESIAN_POINT ( 'NONE',  ( -5.731845798429999306, 1492.036577540089866, 185.8612320274989997 ) ) ;
#46897 = CARTESIAN_POINT ( 'NONE',  ( -14.88997911370000082, 1470.145154249029702, 270.0818331703979425 ) ) ;
#46898 = CARTESIAN_POINT ( 'NONE',  ( -23.78956544001448137, 1436.033567404351288, 211.5876866959136180 ) ) ;
#46899 = CARTESIAN_POINT ( 'NONE',  ( -126.2838827870999836, 1371.894749952190068, 304.2218459572590064 ) ) ;
#46900 = CARTESIAN_POINT ( 'NONE',  ( -14.12009054920000040, 1452.401137584329945, 223.0071355110979994 ) ) ;
#46901 = B_SPLINE_CURVE_WITH_KNOTS ( 'NONE', 5,
 ( #63610, #106134, #96637, #89329, #88786, #27767 ),
 .UNSPECIFIED., .F., .F.,
 ( 6, 6 ),
 ( 0.000000000000000000, 1.000000000000000000 ),
 .UNSPECIFIED. ) ;
#46902 = CARTESIAN_POINT ( 'NONE',  ( 0.2108446687585300017, 1451.971434986430040, 183.0264145658140080 ) ) ;
#46903 = CARTESIAN_POINT ( 'NONE',  ( -13.34103997769999950, 1419.849113831329760, 228.0065750030979927 ) ) ;
#46904 = CARTESIAN_POINT ( 'NONE',  ( 0.000000000000000000, 1526.382868172863937, 209.1218459616979999 ) ) ;
#46905 = DIRECTION ( 'NONE',  ( 0.9993902469228587160, -0.03489947646764298556, -0.001077449651559719661 ) ) ;
#46906 = CARTESIAN_POINT ( 'NONE',  ( 8.151756514128491560, 1360.143105037590431, 208.3718459617010978 ) ) ;
#46907 = CARTESIAN_POINT ( 'NONE',  ( -45.49343607084999519, 1434.389643311759983, 267.6171445062669250 ) ) ;
#46908 = ORIENTED_EDGE ( 'NONE', *, *, #63971, .F. ) ;
#46909 = CARTESIAN_POINT ( 'NONE',  ( -3.549085716194020357, 1506.761702413250077, 180.9924597521999772 ) ) ;
#46910 = EDGE_CURVE ( 'NONE', #44860, #41956, #67646, .T. ) ;
#46911 = ORIENTED_EDGE ( 'NONE', *, *, #72735, .F. ) ;
#46912 = VERTEX_POINT ( 'NONE', #94268 ) ;
#46913 = CARTESIAN_POINT ( 'NONE',  ( 3.463767257884999839, 1517.014196759610059, 210.8246003415769962 ) ) ;
#46914 = CARTESIAN_POINT ( 'NONE',  ( 33.08096890875820151, 1445.052233488291222, 154.3416101011785031 ) ) ;
#46915 = ADVANCED_FACE ( 'NONE', ( #9184 ), #17545, .T. ) ;
#46916 = PLANE ( 'NONE',  #60542 ) ;
#46917 = CARTESIAN_POINT ( 'NONE',  ( -17.06344815410000137, 1425.426455383629900, 191.2828403587980119 ) ) ;
#46918 = AXIS2_PLACEMENT_3D ( 'NONE', #59892, #58778, #69406 ) ;
#46919 = CARTESIAN_POINT ( 'NONE',  ( -2.382487917691452406, 1449.571493106297112, 183.0105235244745074 ) ) ;
#46920 = VERTEX_POINT ( 'NONE', #34924 ) ;
#46921 = ADVANCED_FACE ( 'NONE', ( #101552 ), #67453, .T. ) ;
#46922 = CARTESIAN_POINT ( 'NONE',  ( -5.005071046424999892, 1516.710692850270107, 201.7963041449669959 ) ) ;
#46923 = CARTESIAN_POINT ( 'NONE',  ( 7.885640402109999059, 1473.211498812089985, 217.4524272520789907 ) ) ;
#46924 = B_SPLINE_CURVE_WITH_KNOTS ( 'NONE', 3,
 ( #1228, #77921, #94715, #35364, #77377, #26971 ),
 .UNSPECIFIED., .F., .F.,
 ( 4, 2, 4 ),
 ( 3.469446951953614189E-17, 0.001087661325621730500, 0.002175322651243426306 ),
 .UNSPECIFIED. ) ;
#46925 = CARTESIAN_POINT ( 'NONE',  ( -20.72234375626489822, 1384.535007408160027, 201.8751713657979963 ) ) ;
#46926 = ORIENTED_EDGE ( 'NONE', *, *, #108297, .T. ) ;
#46927 = CARTESIAN_POINT ( 'NONE',  ( -8.364488026064709203, 1410.621949147049918, 269.8709166813640650 ) ) ;
#46928 = CARTESIAN_POINT ( 'NONE',  ( -30.78500370360000105, 1435.572563320330119, 135.1635738117979884 ) ) ;
#46929 = CARTESIAN_POINT ( 'NONE',  ( 0.01233320375960000014, 1396.097901045329991, 197.1956428527979881 ) ) ;
#46931 = ORIENTED_EDGE ( 'NONE', *, *, #88751, .T. ) ;
#46930 = CARTESIAN_POINT ( 'NONE',  ( -10.02185219039999886, 1364.916310432309956, 207.6218459616989946 ) ) ;
#46932 = EDGE_LOOP ( 'NONE', ( #17656, #26218, #27949, #19006, #84082 ) ) ;
#46933 = CARTESIAN_POINT ( 'NONE',  ( 42.49826213307465395, 1453.378461683928663, 269.0622770231100844 ) ) ;
#46934 = CARTESIAN_POINT ( 'NONE',  ( 11.15425147308119946, 1471.646069826549819, 211.6152046850310171 ) ) ;
#46935 = CARTESIAN_POINT ( 'NONE',  ( -2.500000000000000000, 1419.383167280829866, 144.0983880305979881 ) ) ;
#46936 = CARTESIAN_POINT ( 'NONE',  ( -0.03529809467915469984, 1410.073064431770035, 185.0480559684600053 ) ) ;
#46937 = CARTESIAN_POINT ( 'NONE',  ( 2.881325373965000214, 1517.003078582959688, 210.2407492406470055 ) ) ;
#46938 = CARTESIAN_POINT ( 'NONE',  ( -18.57053249869930056, 1415.834070658489964, 207.5706722826859902 ) ) ;
#46939 = CARTESIAN_POINT ( 'NONE',  ( -33.13357216314875586, 1523.313115944345327, 217.3564597502661115 ) ) ;
#46940 = FACE_OUTER_BOUND ( 'NONE', #92415, .T. ) ;
#46941 = CARTESIAN_POINT ( 'NONE',  ( 12.44601730950000018, 1416.547221147930031, 223.4678929843980200 ) ) ;
#46942 = CARTESIAN_POINT ( 'NONE',  ( 7.558229865324999963, 1510.775363762149937, 205.2680898081869998 ) ) ;
#46943 = CARTESIAN_POINT ( 'NONE',  ( -6.950833568235000648, 1517.156142772249950, 206.6378959915070084 ) ) ;
#46944 = ORIENTED_EDGE ( 'NONE', *, *, #15820, .F. ) ;
#46945 = CARTESIAN_POINT ( 'NONE',  ( -42.60628463920510001, 1443.705283414160021, 135.0584851923260032 ) ) ;
#46946 = CARTESIAN_POINT ( 'NONE',  ( 0.08509230700728949437, 1516.966051576903965, 201.6138908561003973 ) ) ;
#46947 = ORIENTED_EDGE ( 'NONE', *, *, #26073, .T. ) ;
#46948 = CARTESIAN_POINT ( 'NONE',  ( 5.997518064628799550, 1456.982253578982636, 228.0100344516387736 ) ) ;
#46949 = CARTESIAN_POINT ( 'NONE',  ( 24.60314935906709621, 1451.898314952959936, 137.0370639567690034 ) ) ;
#46950 = CARTESIAN_POINT ( 'NONE',  ( -4.130945703660738211, 1439.900949266221915, 185.4738977992453215 ) ) ;
#46951 = CARTESIAN_POINT ( 'NONE',  ( -11.61983319979999862, 1416.674354222800048, 204.7879751430089925 ) ) ;
#46952 = CARTESIAN_POINT ( 'NONE',  ( 21.82631551119999713, 1410.169362862829985, 203.3225918027780210 ) ) ;
#46953 = CARTESIAN_POINT ( 'NONE',  ( -2.500000000000000000, 1448.210448412289907, 170.5244215879980061 ) ) ;
#46954 = CARTESIAN_POINT ( 'NONE',  ( 17.28479430970000053, 1410.440253690029976, 225.9720111249980050 ) ) ;
#46955 = CYLINDRICAL_SURFACE ( 'NONE', #85076, 1.000000000000000888 ) ;
#46956 = FACE_OUTER_BOUND ( 'NONE', #57904, .T. ) ;
#46957 = CARTESIAN_POINT ( 'NONE',  ( 21.42399653786173630, 1453.892630570952861, 221.3230395484720532 ) ) ;
#46958 = DIRECTION ( 'NONE',  ( -1.755985294532469921E-16, 1.000000000000000000, -1.338183447452831989E-16 ) ) ;
#46959 = CARTESIAN_POINT ( 'NONE',  ( 7.720650135305000994, 1516.977993847330026, 214.9014730243169993 ) ) ;
#46960 = ORIENTED_EDGE ( 'NONE', *, *, #54478, .F. ) ;
#46961 = CARTESIAN_POINT ( 'NONE',  ( 7.709377398217750255, 1516.547505386119838, 206.4302690467380046 ) ) ;
#46962 = CARTESIAN_POINT ( 'NONE',  ( -10.97762738589999998, 1473.214251705830065, 270.1116084939980055 ) ) ;
#46963 = CARTESIAN_POINT ( 'NONE',  ( -2.500000000000000000, 1448.235640331100058, 183.7014620552980091 ) ) ;
#46964 = CARTESIAN_POINT ( 'NONE',  ( 2.320368942857389871E-14, 1422.005500615010078, 112.3240825799360039 ) ) ;
#46965 = CARTESIAN_POINT ( 'NONE',  ( -40.26206638547280647, 1444.220281762339937, 137.0954650734020106 ) ) ;
#46966 = CARTESIAN_POINT ( 'NONE',  ( 11.60004869885212919, 1425.574822748529868, 138.2968742054259508 ) ) ;
#46967 = CARTESIAN_POINT ( 'NONE',  ( -20.55201027734757702, 1526.382868172863937, 181.8366482295332105 ) ) ;
#46968 = CARTESIAN_POINT ( 'NONE',  ( -1.912619103278670130, 1484.245594002130019, 182.9331903370400028 ) ) ;
#46969 = CARTESIAN_POINT ( 'NONE',  ( 11.13831797289999948, 1433.014992880049931, 151.6441518879979924 ) ) ;
#46970 = CARTESIAN_POINT ( 'NONE',  ( -44.68916218182129541, 1444.637905724729990, 269.6957224876979922 ) ) ;
#46971 = CARTESIAN_POINT ( 'NONE',  ( 27.93016292933110023, 1440.913060387420046, 230.8733152401279938 ) ) ;
#46972 = CARTESIAN_POINT ( 'NONE',  ( -20.00075399880000049, 1508.017360025530024, 229.1239405492979984 ) ) ;
#46973 = CARTESIAN_POINT ( 'NONE',  ( -31.29224244793355680, 1525.661276915132476, 201.9587770753091718 ) ) ;
#46974 = ORIENTED_EDGE ( 'NONE', *, *, #24147, .T. ) ;
#46975 = CARTESIAN_POINT ( 'NONE',  ( 11.23388613411650638, 1445.063428794548372, 207.0699376370758955 ) ) ;
#46976 = DIRECTION ( 'NONE',  ( -1.836970198721029688E-16, -1.000000000000000000, 0.000000000000000000 ) ) ;
#46977 = CARTESIAN_POINT ( 'NONE',  ( -0.8732732019916324973, 1409.114783162738604, 186.1304715542366353 ) ) ;
#46978 = CARTESIAN_POINT ( 'NONE',  ( 12.30852457429709901, 1501.337141734960142, 211.6826237522950009 ) ) ;
#46979 = B_SPLINE_CURVE_WITH_KNOTS ( 'NONE', 3,
 ( #105142, #37386, #96187, #37945, #19463, #96751, #29527, #87807, #106241, #54216, #71587, #97827, #21105, #12733, #1589, #69915, #39590, #13257, #98384, #56952, #91081, #5432, #4347, #72653, #22202, #73194, #31725, #58055, #89983, #4874, #91638, #73761, #5983, #21655 ),
 .UNSPECIFIED., .F., .F.,
 ( 4, 3, 3, 3, 3, 3, 3, 3, 3, 3, 3, 4 ),
 ( -2.000000000000000000, -1.894376539578449981, -1.708008357126509891, -1.519432768888129948, -1.329646548225599911, -1.138371395304140110, -0.9466417899035080019, -0.7549279318903319158, -0.5636971425523138457, -0.3741224486121028647, -0.1861321647941660551, 0.000000000000000000 ),
 .UNSPECIFIED. ) ;
#46980 = CARTESIAN_POINT ( 'NONE',  ( -10.46900974659999939, 1491.361946609490133, 212.5217932129490066 ) ) ;
#46981 = CARTESIAN_POINT ( 'NONE',  ( -16.27856158940000242, 1509.481520284230101, 232.7807208966979999 ) ) ;
#46982 = CARTESIAN_POINT ( 'NONE',  ( -43.29541590384620520, 1383.822952073729994, 247.8268964491909685 ) ) ;
#46983 = CARTESIAN_POINT ( 'NONE',  ( -4.058118992948309689, 1508.551704408389924, 204.4428593323469840 ) ) ;
#46984 = CARTESIAN_POINT ( 'NONE',  ( 6.688848995729999913, 1408.965348139829985, 221.4809136123979840 ) ) ;
#46985 = DIRECTION ( 'NONE',  ( -1.989694733329999956E-13, -6.948167114159990914E-15, 1.000000000000000000 ) ) ;
#46986 = CARTESIAN_POINT ( 'NONE',  ( 2.872763937410000246, 1464.652692451630173, 236.7382212475980054 ) ) ;
#46988 = EDGE_LOOP ( 'NONE', ( #21756, #48740, #71742, #89720, #20423 ) ) ;
#46987 = DIRECTION ( 'NONE',  ( -0.6736849260863839728, 0.000000000000000000, 0.7390186874254150995 ) ) ;
#46989 = CARTESIAN_POINT ( 'NONE',  ( -0.8784639586519999988, 1452.142747003829982, 183.3918967091979937 ) ) ;
#46990 = CARTESIAN_POINT ( 'NONE',  ( -26.04564454490000003, 1383.846902489159902, 224.1106665064590118 ) ) ;
#46991 = EDGE_CURVE ( 'NONE', #53764, #78921, #9610, .T. ) ;
#46992 = CARTESIAN_POINT ( 'NONE',  ( -3.349195415509999663, 1474.892783691989962, 198.1874921133990028 ) ) ;
#46994 = ORIENTED_EDGE ( 'NONE', *, *, #66712, .T. ) ;
#46993 = CARTESIAN_POINT ( 'NONE',  ( -16.38929703815969674, 1414.913060387399810, 208.0943756141269887 ) ) ;
#46995 = CARTESIAN_POINT ( 'NONE',  ( 18.68388055094409950, 1457.534813197310086, 220.6832175138739842 ) ) ;
#46996 = ORIENTED_EDGE ( 'NONE', *, *, #4863, .T. ) ;
#46997 = CARTESIAN_POINT ( 'NONE',  ( -8.317554072875960713, 1387.933845735730074, 218.3619299428229965 ) ) ;
#46998 = LINE ( 'NONE', #106870, #46235 ) ;
#46999 = LINE ( 'NONE', #82782, #20803 ) ;
#47000 = CARTESIAN_POINT ( 'NONE',  ( 11.22296312822500752, 1503.420383748715722, 211.9371915619264541 ) ) ;
#47001 = CARTESIAN_POINT ( 'NONE',  ( -15.33708062616911327, 1509.448643044570190, 233.9107056133578340 ) ) ;
#47002 = CARTESIAN_POINT ( 'NONE',  ( 2.621078202464464546, 1523.542365884047967, 242.1599611597542037 ) ) ;
#47003 = CARTESIAN_POINT ( 'NONE',  ( 11.05349294225439927, 1409.299056866449973, 199.0526579458750120 ) ) ;
#47004 = CYLINDRICAL_SURFACE ( 'NONE', #77711, 0.5000000000000379696 ) ;
#47005 = CARTESIAN_POINT ( 'NONE',  ( -95.05608304844369627, 1385.207712179709915, 294.9719338976229892 ) ) ;
#47006 = CARTESIAN_POINT ( 'NONE',  ( -18.67323663170000003, 1463.212872143629966, 190.4754105328979961 ) ) ;
#47007 = DIRECTION ( 'NONE',  ( -0.000000000000000000, -1.000000000000000000, -0.000000000000000000 ) ) ;
#47008 = CARTESIAN_POINT ( 'NONE',  ( -17.14944456869280032, 1460.835971333450061, 230.2708732161399894 ) ) ;
#47009 = EDGE_CURVE ( 'NONE', #23879, #47496, #1539, .T. ) ;
#47010 = ORIENTED_EDGE ( 'NONE', *, *, #9351, .T. ) ;
#47011 = ORIENTED_EDGE ( 'NONE', *, *, #104411, .T. ) ;
#47012 = DIRECTION ( 'NONE',  ( 0.9455185755993178454, 0.000000000000000000, -0.3255681544571537578 ) ) ;
#47013 = CARTESIAN_POINT ( 'NONE',  ( -12.24150297201249948, 1416.512142030569976, 194.6918193283640051 ) ) ;
#47014 = B_SPLINE_CURVE_WITH_KNOTS ( 'NONE', 5,
 ( #108135, #102888, #99722, #57219, #8285, #48813 ),
 .UNSPECIFIED., .F., .F.,
 ( 6, 6 ),
 ( 0.000000000000000000, 1.000000000000000000 ),
 .UNSPECIFIED. ) ;
#47015 = CARTESIAN_POINT ( 'NONE',  ( -12.06918120999999999, 1434.098677319379931, 150.5974712778979949 ) ) ;
#47016 = CARTESIAN_POINT ( 'NONE',  ( -7.982875717626110139E-10, 1468.280901364470083, 249.1209479164010077 ) ) ;
#47017 = CARTESIAN_POINT ( 'NONE',  ( -20.55923624469150113, 1506.544472774470023, 190.4275880989339953 ) ) ;
#47018 = FACE_OUTER_BOUND ( 'NONE', #88433, .T. ) ;
#47019 = CARTESIAN_POINT ( 'NONE',  ( -109.9058460539999942, 1384.928481735109926, 311.4185263572589975 ) ) ;
#47020 = CARTESIAN_POINT ( 'NONE',  ( -19.27069311609591651, 1486.269147065019297, 189.5747608116244578 ) ) ;
#47021 = CARTESIAN_POINT ( 'NONE',  ( -11.83375927753976065, 1364.194490855938511, 208.3718459617010978 ) ) ;
#47022 = FACE_OUTER_BOUND ( 'NONE', #74160, .T. ) ;
#47023 = B_SPLINE_CURVE_WITH_KNOTS ( 'NONE', 3,
 ( #110799, #35756, #43610, #25674, #93992, #43059, #60422, #59324, #94539, #18927, #110242, #42491, #34090, #52569, #51449, #86703, #102391, #25119, #93435, #52012, #9996, #86154, #16704, #85582, #44167, #50905, #520, #34645, #77760, #69384, #85036, #101826, #69940, #78304, #59866, #8877, #68829, #102930, #103494, #27346 ),
 .UNSPECIFIED., .F., .F.,
 ( 4, 3, 3, 3, 3, 3, 3, 3, 3, 3, 3, 3, 3, 4 ),
 ( -167.7881597174699948, -162.0210453901829908, -153.2885860985529973, -144.2037312555439996, -134.8360698329800016, -124.8049311414389990, -114.1011191363109987, -102.2819146078059873, -87.23193074669060820, -72.32291041643570395, -60.59518579591799892, -49.91975445303839365, -39.91025693460328228, -30.37891568121239061 ),
 .UNSPECIFIED. ) ;
#47024 = CARTESIAN_POINT ( 'NONE',  ( 2.596261494520225366, 1525.907212628473644, 240.7735774411713123 ) ) ;
#47025 = CARTESIAN_POINT ( 'NONE',  ( -4.625790014595000166, 1517.104192383289956, 208.0004623403669939 ) ) ;
#47026 = CARTESIAN_POINT ( 'NONE',  ( 2.522951803030079727E-08, 1397.914279477030050, 222.1218461579910297 ) ) ;
#47027 = CARTESIAN_POINT ( 'NONE',  ( -13.10408799755770026, 1435.790188770230088, 150.6193508587029726 ) ) ;
#47028 = CARTESIAN_POINT ( 'NONE',  ( -7.543627442569999175, 1385.104043808209781, 219.0827038849589883 ) ) ;
#47029 = ADVANCED_FACE ( 'NONE', ( #38231 ), #70470, .F. ) ;
#47030 = CARTESIAN_POINT ( 'NONE',  ( 0.9042083405910000815, 1416.833018152729892, 190.2143527203979829 ) ) ;
#47031 = CARTESIAN_POINT ( 'NONE',  ( 20.13590845398709916, 1492.832540254449896, 227.2160562042610081 ) ) ;
#47032 = DIRECTION ( 'NONE',  ( -0.8023110876747339137, -0.5969061220947440294, 0.000000000000000000 ) ) ;
#47033 = EDGE_LOOP ( 'NONE', ( #2593, #87249 ) ) ;
#47034 = CARTESIAN_POINT ( 'NONE',  ( 31.20802388339999922, 1430.369980854530013, 248.1710554639980160 ) ) ;
#47035 = CARTESIAN_POINT ( 'NONE',  ( -2.521622038060000293, 1415.707855076169835, 204.8799433334789910 ) ) ;
#47037 = CARTESIAN_POINT ( 'NONE',  ( 17.33645362950000290, 1414.996442546130083, 210.3925741896480304 ) ) ;
#47036 = CARTESIAN_POINT ( 'NONE',  ( -10.36174392853389925, 1425.413733281229952, 93.54415789945380766 ) ) ;
#47038 = EDGE_CURVE ( 'NONE', #68340, #5427, #16339, .T. ) ;
#47039 = CARTESIAN_POINT ( 'NONE',  ( -40.61001291052744477, 1425.241084799366718, 269.7704882069099313 ) ) ;
#47040 = CARTESIAN_POINT ( 'NONE',  ( -24.78057548010000133, 1437.622990999089780, 216.3901361313880329 ) ) ;
#47041 = CARTESIAN_POINT ( 'NONE',  ( 20.08696296560329841, 1509.650477513600208, 231.0046925456110216 ) ) ;
#47042 = CARTESIAN_POINT ( 'NONE',  ( -5.030623778630000764, 1391.799617351889992, 214.4844137014689807 ) ) ;
#47043 = CARTESIAN_POINT ( 'NONE',  ( 27.03406173819999836, 1451.512718515130018, 136.1495732049980063 ) ) ;
#47044 = ORIENTED_EDGE ( 'NONE', *, *, #99580, .F. ) ;
#47045 = CARTESIAN_POINT ( 'NONE',  ( -32.78250617288034618, 1512.187213306747481, 218.3079823578271430 ) ) ;
#47046 = CARTESIAN_POINT ( 'NONE',  ( 13.41829267866989106, 1513.652806704122668, 225.8959966016125236 ) ) ;
#47047 = CARTESIAN_POINT ( 'NONE',  ( 8.835340541969999961, 1509.234990883429873, 237.6028457034980192 ) ) ;
#47048 = ORIENTED_EDGE ( 'NONE', *, *, #45020, .T. ) ;
#47049 = ORIENTED_EDGE ( 'NONE', *, *, #109695, .F. ) ;
#47050 = CARTESIAN_POINT ( 'NONE',  ( -10.10004869884733125, 1422.222932908416851, 137.0999999980979851 ) ) ;
#47051 = CARTESIAN_POINT ( 'NONE',  ( -24.06078745206859892, 1410.858125197970139, 208.6187097067000025 ) ) ;
#47052 = ORIENTED_EDGE ( 'NONE', *, *, #107484, .T. ) ;
#47053 = CARTESIAN_POINT ( 'NONE',  ( -4.626185416090139668, 1439.746126037229942, 205.5536779009150052 ) ) ;
#47054 = DIRECTION ( 'NONE',  ( 0.000000000000000000, 0.000000000000000000, 1.000000000000000000 ) ) ;
#47055 = CARTESIAN_POINT ( 'NONE',  ( -13.30975985100000081, 1479.764766878030059, 231.2919490532979978 ) ) ;
#47056 = CARTESIAN_POINT ( 'NONE',  ( -0.2549717317763739999, 1442.897952001810154, 200.2186391711400120 ) ) ;
#47057 = ORIENTED_EDGE ( 'NONE', *, *, #31202, .T. ) ;
#47058 = DIRECTION ( 'NONE',  ( -0.08338001035890203749, 1.207410962451694502E-12, -0.9965178241619914168 ) ) ;
#47059 = CARTESIAN_POINT ( 'NONE',  ( -3.487586626270560153, 1508.731366866819826, 204.5668911269270041 ) ) ;
#47060 = CARTESIAN_POINT ( 'NONE',  ( 14.07846764309999976, 1463.781906650229985, 224.7807885173980367 ) ) ;
#47061 = CARTESIAN_POINT ( 'NONE',  ( -3.458526536014999930, 1516.742629295279812, 204.1242721449069961 ) ) ;
#47062 = VERTEX_POINT ( 'NONE', #89741 ) ;
#47063 = CARTESIAN_POINT ( 'NONE',  ( -4.500000000000000000, 1426.966631815929986, 170.4008037693979816 ) ) ;
#47064 = CARTESIAN_POINT ( 'NONE',  ( 12.58023385476424494, 1442.780465393927670, 186.4880924237379247 ) ) ;
#47065 = ORIENTED_EDGE ( 'NONE', *, *, #10083, .F. ) ;
#47066 = ORIENTED_EDGE ( 'NONE', *, *, #49612, .F. ) ;
#47067 = CARTESIAN_POINT ( 'NONE',  ( 2.372478608334043670, 1522.644714754858114, 174.8996806668799024 ) ) ;
#47068 = CARTESIAN_POINT ( 'NONE',  ( -29.33475263078172546, 1526.373507135058617, 217.1429229503218039 ) ) ;
#47069 = CARTESIAN_POINT ( 'NONE',  ( 12.76760079159999961, 1508.356069781229962, 233.5455612081979950 ) ) ;
#47070 = CARTESIAN_POINT ( 'NONE',  ( -9.891642072088888682, 1470.030674514850034, 213.7492784014550011 ) ) ;
#47071 = CARTESIAN_POINT ( 'NONE',  ( 13.23745870105759970, 1452.450798143380098, 148.9949343981280094 ) ) ;
#47072 = CARTESIAN_POINT ( 'NONE',  ( 9.223040078240002160, 1420.831005969599801, 196.7861790798990000 ) ) ;
#47073 = CARTESIAN_POINT ( 'NONE',  ( -2.229670771031690091, 1476.033530122819911, 220.3577958911180019 ) ) ;
#47074 = CARTESIAN_POINT ( 'NONE',  ( -3.263114576272079827E-31, 1414.677402202029953, 209.1218459616989946 ) ) ;
#47075 = CARTESIAN_POINT ( 'NONE',  ( -11.58636794539999926, 1433.009610086610110, 151.1946776885979773 ) ) ;
#47076 = CARTESIAN_POINT ( 'NONE',  ( 0.03406326677807396813, 1410.027273331433889, 233.1845275417764469 ) ) ;
#47078 = CARTESIAN_POINT ( 'NONE',  ( -106.3976924294359918, 1390.939209247700092, 307.7528211820909974 ) ) ;
#47077 = CARTESIAN_POINT ( 'NONE',  ( -16.80801311784789931, 1415.384652614329980, 191.6111484580369790 ) ) ;
#47079 = CARTESIAN_POINT ( 'NONE',  ( 11.23478826778469930, 1422.543918281529841, 207.0476803316210237 ) ) ;
#47080 = B_SPLINE_CURVE_WITH_KNOTS ( 'NONE', 5,
 ( #84916, #93869, #65955, #48597, #82731, #100080 ),
 .UNSPECIFIED., .F., .F.,
 ( 6, 6 ),
 ( -15.04427212800000113, -3.432284964179999065 ),
 .UNSPECIFIED. ) ;
#47081 = CARTESIAN_POINT ( 'NONE',  ( -9.788108383745552032, 1440.056842154589958, 207.0031482218739995 ) ) ;
#47082 = CARTESIAN_POINT ( 'NONE',  ( -6.775684858734999594, 1512.341575225259930, 201.7407336143970156 ) ) ;
#47083 = ORIENTED_EDGE ( 'NONE', *, *, #84419, .F. ) ;
#47084 = CARTESIAN_POINT ( 'NONE',  ( 12.22219588455229911, 1415.434635989089884, 222.2791104031980183 ) ) ;
#47085 = CYLINDRICAL_SURFACE ( 'NONE', #90962, 2.000000000000000000 ) ;
#47086 = CARTESIAN_POINT ( 'NONE',  ( -79.14188242860410583, 1384.996239183999933, 303.2876060637049704 ) ) ;
#47087 = CARTESIAN_POINT ( 'NONE',  ( -9.699806184529998987, 1388.369311790329903, 201.2298857673789882 ) ) ;
#47088 = CARTESIAN_POINT ( 'NONE',  ( 10.47511427260239891, 1482.040461736080033, 210.7458695605469927 ) ) ;
#47090 = ORIENTED_EDGE ( 'NONE', *, *, #63226, .T. ) ;
#47089 = CARTESIAN_POINT ( 'NONE',  ( -10.28857233090000101, 1463.185141274090256, 204.9217573806190273 ) ) ;
#47091 = CARTESIAN_POINT ( 'NONE',  ( -16.70830179842720042, 1417.149226859160080, 207.3570905742490140 ) ) ;
#47092 = CARTESIAN_POINT ( 'NONE',  ( -2.596326248400549819, 1439.736080710940087, 157.6563194317720047 ) ) ;
#47093 = CARTESIAN_POINT ( 'NONE',  ( -8.102530104066362426, 1477.152887553389974, 215.6207631052049294 ) ) ;
#47094 = CARTESIAN_POINT ( 'NONE',  ( 9.682511080499990541, 1436.279831232390052, 210.8541354582289955 ) ) ;
#47095 = CARTESIAN_POINT ( 'NONE',  ( 12.53415176833500055, 1512.123798513659949, 225.3767377372669785 ) ) ;
#47096 = CARTESIAN_POINT ( 'NONE',  ( 13.00574619272959964, 1416.230844595159851, 196.4148928853770144 ) ) ;
#47097 = CARTESIAN_POINT ( 'NONE',  ( 3.313918604249419975, 1458.909887735149823, 200.0205288476430212 ) ) ;
#47098 = FACE_OUTER_BOUND ( 'NONE', #5185, .T. ) ;
#47099 = CARTESIAN_POINT ( 'NONE',  ( 14.73464909550000002, 1422.105278128630061, 228.1938737527979697 ) ) ;
#47100 = B_SPLINE_CURVE_WITH_KNOTS ( 'NONE', 5,
 ( #101161, #50784, #99510, #49148, #67602, #40727, #92777, #16052, #58098, #91678, #15500, #74900 ),
 .UNSPECIFIED., .F., .F.,
 ( 6, 3, 3, 6 ),
 ( 13.03551675900000006, 13.93909308159999938, 15.74624572679999979, 17.56231401080000154 ),
 .UNSPECIFIED. ) ;
#47101 = CARTESIAN_POINT ( 'NONE',  ( -21.71247731329013675, 1523.982201850120191, 234.6948375436862193 ) ) ;
#47102 = CARTESIAN_POINT ( 'NONE',  ( -3.269984819434999856, 1516.999105586269934, 207.4194399470370058 ) ) ;
#47103 = CARTESIAN_POINT ( 'NONE',  ( 45.11781237659999277, 1434.982694580879979, 266.2041965131979850 ) ) ;
#47104 = CARTESIAN_POINT ( 'NONE',  ( -17.46956007389999854, 1409.523110867929972, 223.7310521786980075 ) ) ;
#47105 = CARTESIAN_POINT ( 'NONE',  ( 16.25264133110000131, 1436.302628333469784, 148.7774457700980122 ) ) ;
#47106 = CARTESIAN_POINT ( 'NONE',  ( -0.9041356904339998835, 1416.839648772129976, 228.0296119443979990 ) ) ;
#47107 = CARTESIAN_POINT ( 'NONE',  ( 29.53677856842397631, 1509.959383199721287, 207.3087542667464618 ) ) ;
#47108 = CARTESIAN_POINT ( 'NONE',  ( -1.770636241409999867, 1475.812198116930176, 266.9599394754979471 ) ) ;
#47109 = CARTESIAN_POINT ( 'NONE',  ( -14.30580887908100074, 1416.879264667930101, 203.2316167391460056 ) ) ;
#47110 =( BOUNDED_CURVE ( )  B_SPLINE_CURVE ( 3, ( #51505, #19403, #68333, #102440 ),
 .UNSPECIFIED., .F., .F. ) 
 B_SPLINE_CURVE_WITH_KNOTS ( ( 4, 4 ),
 ( 0.9971162661778150138, 2.144476395621194964 ),
 .UNSPECIFIED. ) 
 CURVE ( )  GEOMETRIC_REPRESENTATION_ITEM ( )  RATIONAL_B_SPLINE_CURVE ( ( 1.000000000000000000, 0.8932729319369855370, 0.8932729319369855370, 1.000000000000000000 ) ) 
 REPRESENTATION_ITEM ( '' )  );
#47111 = CARTESIAN_POINT ( 'NONE',  ( -40.33412369041069923, 1439.452808492470012, 136.1315416014939785 ) ) ;
#47112 = DIRECTION ( 'NONE',  ( -1.000000000000000000, 0.000000000000000000, 0.000000000000000000 ) ) ;
#47113 = CARTESIAN_POINT ( 'NONE',  ( -8.786848204050000888, 1409.039826487530036, 220.7305139779979868 ) ) ;
#47114 = CARTESIAN_POINT ( 'NONE',  ( -15.87297696440000117, 1415.931391677429929, 200.7186373451680197 ) ) ;
#47115 = CARTESIAN_POINT ( 'NONE',  ( 18.02257621027576562, 1526.382868172863937, 182.8951942368371988 ) ) ;
#47116 = CARTESIAN_POINT ( 'NONE',  ( 0.6485169668797152731, 1484.502209508327951, 198.4327370695805257 ) ) ;
#47117 = CARTESIAN_POINT ( 'NONE',  ( 12.06124454959999959, 1433.903398563020119, 147.6243995897980028 ) ) ;
#47118 = DIRECTION ( 'NONE',  ( 0.1402804634180439824, 0.9901118076173108795, -3.469446951951086598E-18 ) ) ;
#47119 = CARTESIAN_POINT ( 'NONE',  ( 4.219438956540000341, 1441.595895961080259, 182.7715286933980110 ) ) ;
#47120 = EDGE_LOOP ( 'NONE', ( #2018, #66005, #73862, #87689 ) ) ;
#47121 = DIRECTION ( 'NONE',  ( 0.9510565162951478690, 0.000000000000000000, -0.3090169943749654369 ) ) ;
#47122 = CARTESIAN_POINT ( 'NONE',  ( 26.96383586069999794, 1437.662818847919880, 136.8825122631980094 ) ) ;
#47123 = CARTESIAN_POINT ( 'NONE',  ( -12.25106032620000107, 1490.322274117190091, 209.3376309630089622 ) ) ;
#47124 = CARTESIAN_POINT ( 'NONE',  ( -8.992287217462708426, 1437.995524108949894, 210.4996962295319918 ) ) ;
#47125 = CARTESIAN_POINT ( 'NONE',  ( -14.67313656458610005, 1477.920145184079956, 193.6164693688140233 ) ) ;
#47126 = CARTESIAN_POINT ( 'NONE',  ( -45.85459127630000609, 1440.913039247130200, 268.7562765203980462 ) ) ;
#47127 = CARTESIAN_POINT ( 'NONE',  ( 9.345710454894810226, 1422.635914553260136, 212.8840094578699791 ) ) ;
#47128 = LINE ( 'NONE', #21332, #32474 ) ;
#47129 = CARTESIAN_POINT ( 'NONE',  ( -85.23413153088101524, 1384.628137661299888, 306.7983909476229769 ) ) ;
#47130 = B_SPLINE_SURFACE_WITH_KNOTS ( 'NONE', 3, 5, ( 
 ( #88890, #54217, #87808, #11633, #71023, #79395 ),
 ( #106242, #21107, #10527, #97828, #105710, #88342 ),
 ( #72654, #2159, #71589, #62633, #106781, #54760 ),
 ( #3818, #2709, #28992, #87238, #36276, #55308 ) ),
 .UNSPECIFIED., .F., .F., .F.,
 ( 4, 4 ),
 ( 6, 6 ),
 ( 0.000000000000000000, 0.07116409211490000442 ),
 ( 0.000000000000000000, 2.000000000000000000 ),
 .UNSPECIFIED. ) ;
#47131 = CARTESIAN_POINT ( 'NONE',  ( -32.91460356916239505, 1384.974432874500053, 207.2804400437590004 ) ) ;
#47132 = CARTESIAN_POINT ( 'NONE',  ( -16.68062049856698081, 1526.382868172863937, 236.8314524626096897 ) ) ;
#47133 = CARTESIAN_POINT ( 'NONE',  ( -26.80425739744236679, 1436.404103241545272, 136.7059128651563924 ) ) ;
#47134 = CARTESIAN_POINT ( 'NONE',  ( -27.79584127320000420, 1451.487053449729956, 136.1260449201980123 ) ) ;
#47135 = CARTESIAN_POINT ( 'NONE',  ( -3.347801439372898979, 1523.456924617338245, 176.1543725842045376 ) ) ;
#47136 = ADVANCED_FACE ( 'NONE', ( #48868 ), #7176, .F. ) ;
#47138 = ORIENTED_EDGE ( 'NONE', *, *, #102233, .T. ) ;
#47137 = CARTESIAN_POINT ( 'NONE',  ( -0.3888774176050009967, 1508.936806585589920, 218.1328934611190107 ) ) ;
#47139 = CARTESIAN_POINT ( 'NONE',  ( -31.43069643840468075, 1526.748660780343698, 216.5579808171739842 ) ) ;
#47140 = CARTESIAN_POINT ( 'NONE',  ( -24.00439558080000069, 1410.673376339430206, 208.3492520220979998 ) ) ;
#47141 = CARTESIAN_POINT ( 'NONE',  ( -7.465188678339999662, 1497.180420109090164, 217.7707592773190015 ) ) ;
#47142 = CARTESIAN_POINT ( 'NONE',  ( -12.07588402680000073, 1415.579607678529783, 195.0757015091980122 ) ) ;
#47143 = CARTESIAN_POINT ( 'NONE',  ( 1.833868989029999952, 1422.484255930740119, 193.6377413423990106 ) ) ;
#47144 = EDGE_CURVE ( 'NONE', #71879, #14033, #28474, .T. ) ;
#47145 = CARTESIAN_POINT ( 'NONE',  ( 22.76066440079999609, 1410.202971864430083, 213.5588159894880107 ) ) ;
#47146 = DIRECTION ( 'NONE',  ( 0.7384854939282339270, 1.641580738839949676E-15, -0.6742693640212139572 ) ) ;
#47147 = CARTESIAN_POINT ( 'NONE',  ( -16.61337859989249921, 1463.629512765479831, 220.4655032150840270 ) ) ;
#47148 = CARTESIAN_POINT ( 'NONE',  ( -3.666694481987490040, 1509.114858341099989, 179.5219341129400163 ) ) ;
#47150 = CARTESIAN_POINT ( 'NONE',  ( -14.05078142410000019, 1379.708754511839743, 206.9026084073089748 ) ) ;
#47149 = CARTESIAN_POINT ( 'NONE',  ( 19.75084982879439721, 1455.504334177440114, 226.5702129464319796 ) ) ;
#47151 = CARTESIAN_POINT ( 'NONE',  ( 25.74606117743979894, 1449.914928376210128, 209.5154968510050253 ) ) ;
#47152 = CYLINDRICAL_SURFACE ( 'NONE', #98472, 0.9999999999999950040 ) ;
#47153 = DIRECTION ( 'NONE',  ( -1.000000000000000000, 0.000000000000000000, 0.000000000000000000 ) ) ;
#47154 = CARTESIAN_POINT ( 'NONE',  ( -0.6609304440939999248, 1417.306157093830052, 234.7827881003979940 ) ) ;
#47155 = CARTESIAN_POINT ( 'NONE',  ( 9.704582620010000937, 1366.001145740639913, 210.6218459616991936 ) ) ;
#47156 = CARTESIAN_POINT ( 'NONE',  ( -5.785582951674999919, 1516.981965530290154, 205.0894480302270040 ) ) ;
#47157 = CARTESIAN_POINT ( 'NONE',  ( -11.30203360114940025, 1485.177505568769902, 185.2631062660830139 ) ) ;
#47158 = ORIENTED_EDGE ( 'NONE', *, *, #26171, .F. ) ;
#47159 = CARTESIAN_POINT ( 'NONE',  ( 11.20410962351969886, 1503.462441903569925, 212.0609900696560146 ) ) ;
#47160 = CARTESIAN_POINT ( 'NONE',  ( 17.40764059099999628, 1414.996444526030018, 210.6782161193179945 ) ) ;
#47162 = ORIENTED_EDGE ( 'NONE', *, *, #42579, .F. ) ;
#47161 = CARTESIAN_POINT ( 'NONE',  ( -68.39393351552520528, 1379.747380541330131, 279.9548358144079998 ) ) ;
#47163 = ORIENTED_EDGE ( 'NONE', *, *, #49019, .F. ) ;
#47164 = CARTESIAN_POINT ( 'NONE',  ( 29.25495334450000229, 1509.872415968330188, 209.6024640478379979 ) ) ;
#47165 = ORIENTED_EDGE ( 'NONE', *, *, #64430, .F. ) ;
#47166 = CARTESIAN_POINT ( 'NONE',  ( 6.811012380346902262, 1507.262579170454046, 182.5160571386342951 ) ) ;
#47167 = CARTESIAN_POINT ( 'NONE',  ( 11.35976097320000022, 1500.240390108989914, 205.8138550405789999 ) ) ;
#47169 = DIRECTION ( 'NONE',  ( -0.6736849260863841948, 0.000000000000000000, 0.7390186874254148774 ) ) ;
#47168 = CARTESIAN_POINT ( 'NONE',  ( 15.90371042334150253, 1418.365809420349933, 191.2849450763380048 ) ) ;
#47170 = CARTESIAN_POINT ( 'NONE',  ( 2.493697040924999886, 1516.977201124959947, 210.2401991861970032 ) ) ;
#47171 = CARTESIAN_POINT ( 'NONE',  ( -24.63384085366289966, 1451.895538293800200, 136.9985731684789982 ) ) ;
#47172 = CARTESIAN_POINT ( 'NONE',  ( -106.5595845979900105, 1378.913060387289988, 306.5187700427659934 ) ) ;
#47173 = CARTESIAN_POINT ( 'NONE',  ( 13.25587788500000030, 1409.542715034829826, 227.8021890157979783 ) ) ;
#47174 = CARTESIAN_POINT ( 'NONE',  ( 9.690694291389919002, 1481.940033707770226, 215.3400710034819951 ) ) ;
#47175 = SHAPE_DEFINITION_REPRESENTATION ( #57247, #22211 ) ;
#47176 = CARTESIAN_POINT ( 'NONE',  ( 41.65974987187789935, 1443.430997017130267, 134.0999999981650035 ) ) ;
#47177 = CARTESIAN_POINT ( 'NONE',  ( -18.70459388414779767, 1509.566239243649989, 231.7064163625079800 ) ) ;
#47178 = CARTESIAN_POINT ( 'NONE',  ( -14.38097578403179888, 1422.143783148600050, 196.2925640312170117 ) ) ;
#47179 = CARTESIAN_POINT ( 'NONE',  ( -10.25368860849440011, 1391.913060387289988, 204.2726074216130030 ) ) ;
#47180 = ORIENTED_EDGE ( 'NONE', *, *, #101841, .F. ) ;
#47181 = ORIENTED_EDGE ( 'NONE', *, *, #40526, .T. ) ;
#47182 = ORIENTED_EDGE ( 'NONE', *, *, #107298, .F. ) ;
#47183 = AXIS2_PLACEMENT_3D ( 'NONE', #10823, #105989, #44995 ) ;
#47184 = CARTESIAN_POINT ( 'NONE',  ( -6.910053069894999567, 1514.330398624150121, 217.1607477560669679 ) ) ;
#47185 = CARTESIAN_POINT ( 'NONE',  ( 16.78435730151638694, 1513.560745841035896, 195.8810728685500635 ) ) ;
#47186 = CARTESIAN_POINT ( 'NONE',  ( -14.11750138697139789, 1379.894919723800058, 211.2943169131719969 ) ) ;
#47187 = CARTESIAN_POINT ( 'NONE',  ( -16.88275388290000123, 1507.705444072489854, 209.4032267757409898 ) ) ;
#47188 = B_SPLINE_CURVE_WITH_KNOTS ( 'NONE', 5,
 ( #16115, #467, #7733, #51395, #34591, #9394 ),
 .UNSPECIFIED., .F., .F.,
 ( 6, 6 ),
 ( -20.59614117366909980, -15.24393013793890006 ),
 .UNSPECIFIED. ) ;
#47189 = CIRCLE ( 'NONE', #27511, 2.000000000000011102 ) ;
#47190 = CARTESIAN_POINT ( 'NONE',  ( -16.83328027291899076, 1449.459041290944015, 219.8226804865572603 ) ) ;
#47191 = CARTESIAN_POINT ( 'NONE',  ( -68.61568296326619532, 1379.747656804948974, 279.7483219046964678 ) ) ;
#47192 = CARTESIAN_POINT ( 'NONE',  ( 0.9125060962980010570, 1465.149707686289730, 198.8904297983990261 ) ) ;
#47193 = CARTESIAN_POINT ( 'NONE',  ( 28.27265630610000002, 1508.146186351229971, 209.2480474313609875 ) ) ;
#47194 = CARTESIAN_POINT ( 'NONE',  ( 5.414687584439999313, 1414.913060387329779, 193.6792642988980049 ) ) ;
#47195 = CARTESIAN_POINT ( 'NONE',  ( -55.20091899711550099, 1384.645211897679928, 234.2512433511650158 ) ) ;
#47196 = ORIENTED_EDGE ( 'NONE', *, *, #44079, .T. ) ;
#47197 = CARTESIAN_POINT ( 'NONE',  ( 4.608146781254999880, 1516.677239312369920, 206.8257210811669893 ) ) ;
#47198 = ORIENTED_EDGE ( 'NONE', *, *, #90389, .T. ) ;
#47199 = DIRECTION ( 'NONE',  ( 1.171491307323471973E-14, 1.000000000000000000, -1.371895365494980038E-14 ) ) ;
#47200 = CARTESIAN_POINT ( 'NONE',  ( 19.06412006440000084, 1467.189854735629979, 227.5855243549980287 ) ) ;
#47201 = ORIENTED_EDGE ( 'NONE', *, *, #38752, .F. ) ;
#47202 = CARTESIAN_POINT ( 'NONE',  ( -0.1489371451341119923, 1450.907859387619965, 181.8882210233129797 ) ) ;
#47203 = CARTESIAN_POINT ( 'NONE',  ( -7.500000000000000000, 1391.913060387289988, 209.1218459616989946 ) ) ;
#47204 = CARTESIAN_POINT ( 'NONE',  ( -17.85077614882369090, 1508.456763636446112, 212.1147255241837115 ) ) ;
#47205 = CARTESIAN_POINT ( 'NONE',  ( 8.206329918199999796, 1502.256773578390039, 208.4091422247220180 ) ) ;
#47206 = CARTESIAN_POINT ( 'NONE',  ( -8.906178969139920909, 1437.089246318600090, 213.2884079821210150 ) ) ;
#47207 = AXIS2_PLACEMENT_3D ( 'NONE', #32304, #66487, #74330 ) ;
#47208 = CARTESIAN_POINT ( 'NONE',  ( -5.689538399873499408, 1510.689985724140115, 201.5635966250480067 ) ) ;
#47209 = CARTESIAN_POINT ( 'NONE',  ( 41.16455037149999896, 1425.337515733230020, 266.3184770345980041 ) ) ;
#47210 = CARTESIAN_POINT ( 'NONE',  ( -5.726916886920052185, 1510.539524115660697, 201.5773753062340461 ) ) ;
#47211 = CARTESIAN_POINT ( 'NONE',  ( -22.01290455779466271, 1522.906363951597314, 182.8785777331678446 ) ) ;
#47213 = CARTESIAN_POINT ( 'NONE',  ( -11.60004869885203682, 1422.586144007987514, 135.6000000023773282 ) ) ;
#47212 = CARTESIAN_POINT ( 'NONE',  ( 2.805385066259999949, 1465.548011742730296, 234.3643945938979982 ) ) ;
#47214 = CARTESIAN_POINT ( 'NONE',  ( -2.870951705914999597, 1517.111322026010157, 215.6844817927369888 ) ) ;
#47215 = DIRECTION ( 'NONE',  ( -0.000000000000000000, -1.000000000000000000, -0.000000000000000000 ) ) ;
#47216 = CARTESIAN_POINT ( 'NONE',  ( -0.1497422254867110114, 1507.486086595969937, 180.8511887974889873 ) ) ;
#47217 = CARTESIAN_POINT ( 'NONE',  ( 2.491619553449157642, 1516.536652113955824, 216.8309391655190836 ) ) ;
#47218 = CARTESIAN_POINT ( 'NONE',  ( 2.298048923505000118, 1516.764084769670262, 212.5672535042169784 ) ) ;
#47219 = EDGE_CURVE ( 'NONE', #33927, #82900, #64142, .T. ) ;
#47220 = CARTESIAN_POINT ( 'NONE',  ( -19.67719249089999778, 1452.817890304729872, 209.2087704682629976 ) ) ;
#47221 = CARTESIAN_POINT ( 'NONE',  ( -5.102340803919999779, 1483.010473641589897, 199.7820758705289848 ) ) ;
#47223 = ORIENTED_EDGE ( 'NONE', *, *, #96690, .F. ) ;
#47222 = DIRECTION ( 'NONE',  ( -6.123233995736769734E-17, -1.000000000000000000, -1.124819836996399911E-32 ) ) ;
#47224 = CARTESIAN_POINT ( 'NONE',  ( -20.06869840700000296, 1507.849569109330105, 229.0200580499979992 ) ) ;
#47225 = CARTESIAN_POINT ( 'NONE',  ( 1.343386335820000024E-08, 1460.517119006129860, 217.3476459701080046 ) ) ;
#47226 = CARTESIAN_POINT ( 'NONE',  ( -11.29459831670000014, 1431.803823149859909, 151.5027742212979831 ) ) ;
#47227 = CARTESIAN_POINT ( 'NONE',  ( -1.637258856660000150, 1483.893433971690001, 198.5669146070989939 ) ) ;
#47228 = EDGE_CURVE ( 'NONE', #19916, #94671, #81794, .T. ) ;
#47229 = CARTESIAN_POINT ( 'NONE',  ( 5.106122016996108570, 1414.913060387329779, 193.4216302945174562 ) ) ;
#47230 = CARTESIAN_POINT ( 'NONE',  ( 8.247379814629999473, 1421.181889050119935, 196.1087402428989890 ) ) ;
#47231 = CARTESIAN_POINT ( 'NONE',  ( -8.809238219330000064, 1438.685537000089880, 208.2566061143539855 ) ) ;
#47233 = CARTESIAN_POINT ( 'NONE',  ( 5.368321057878550739, 1426.798736626489926, 152.9345200458829765 ) ) ;
#47232 = CARTESIAN_POINT ( 'NONE',  ( -18.65643340519999782, 1444.808185763539996, 226.4043360155980054 ) ) ;
#47234 = CARTESIAN_POINT ( 'NONE',  ( -0.2223819995240000069, 1416.825245919230156, 191.0547458884979903 ) ) ;
#47235 = ORIENTED_EDGE ( 'NONE', *, *, #85004, .T. ) ;
#47236 = CARTESIAN_POINT ( 'NONE',  ( 4.609996581545000360, 1516.769879638719885, 205.6626893540170329 ) ) ;
#47237 = CARTESIAN_POINT ( 'NONE',  ( 0.5588755390740001161, 1405.778268568529938, 268.4836505046980051 ) ) ;
#47238 = FACE_OUTER_BOUND ( 'NONE', #59554, .T. ) ;
#47239 = CARTESIAN_POINT ( 'NONE',  ( 24.17267386829139753, 1436.406449779874038, 213.4172145310692201 ) ) ;
#47240 = CARTESIAN_POINT ( 'NONE',  ( -25.74086641750000126, 1452.014152722630115, 135.1060044590980169 ) ) ;
#47241 = CARTESIAN_POINT ( 'NONE',  ( 11.60004869885203682, 1424.621838078508063, 136.2521644537905559 ) ) ;
#47242 = CARTESIAN_POINT ( 'NONE',  ( 4.219439031349260461, 1446.230224802979819, 182.3842141579679890 ) ) ;
#47243 = B_SPLINE_CURVE_WITH_KNOTS ( 'NONE', 3,
 ( #84922, #66520, #6028, #102281, #8215, #92782 ),
 .UNSPECIFIED., .F., .F.,
 ( 4, 2, 4 ),
 ( 0.000000000000000000, 0.5000000000000000000, 1.000000000000000000 ),
 .UNSPECIFIED. ) ;
#47244 = CARTESIAN_POINT ( 'NONE',  ( -2.500290412864679901, 1448.931711032029853, 154.7923269189249993 ) ) ;
#47245 = DIRECTION ( 'NONE',  ( -0.000000000000000000, -1.000000000000000000, -0.000000000000000000 ) ) ;
#47246 = CARTESIAN_POINT ( 'NONE',  ( -19.83769288353390436, 1485.661834359392060, 190.4830555484894887 ) ) ;
#47247 = CARTESIAN_POINT ( 'NONE',  ( -13.49369408200810128, 1415.034069327400175, 220.4142464946930033 ) ) ;
#47248 = CARTESIAN_POINT ( 'NONE',  ( -3.984081798389999651, 1515.551704150889918, 210.9648099238589793 ) ) ;
#47249 =( BOUNDED_CURVE ( )  B_SPLINE_CURVE ( 3, ( #66473, #41786, #93287, #92736 ),
 .UNSPECIFIED., .F., .T. ) 
 B_SPLINE_CURVE_WITH_KNOTS ( ( 4, 4 ),
 ( 0.000000000000000000, 0.7048113239776826466 ),
 .UNSPECIFIED. ) 
 CURVE ( )  GEOMETRIC_REPRESENTATION_ITEM ( )  RATIONAL_B_SPLINE_CURVE ( ( 1.000000000000000000, 0.9590300661663233583, 0.9590300661663233583, 1.000000000000000000 ) ) 
 REPRESENTATION_ITEM ( '' )  );
#47250 = CARTESIAN_POINT ( 'NONE',  ( -14.73695825179999908, 1419.186926028530252, 255.3819207742980097 ) ) ;
#47251 = CIRCLE ( 'NONE', #108055, 11.26398391340000060 ) ;
#47252 = CARTESIAN_POINT ( 'NONE',  ( 11.02688339341326440, 1425.203200046631764, 139.1360293941474993 ) ) ;
#47253 = CARTESIAN_POINT ( 'NONE',  ( 4.221259200859999616, 1441.605854689579928, 166.9080625328979863 ) ) ;
#47254 = CARTESIAN_POINT ( 'NONE',  ( -0.5546426699349999989, 1475.558885421630066, 269.2946135826979912 ) ) ;
#47255 = CARTESIAN_POINT ( 'NONE',  ( 21.38516915557965703, 1501.977400791986611, 180.3939891059721106 ) ) ;
#47256 = CARTESIAN_POINT ( 'NONE',  ( 9.296941329909470753, 1453.078838434450063, 212.1081459014599773 ) ) ;
#47257 = CARTESIAN_POINT ( 'NONE',  ( 30.90487439922560498, 1525.907212628473644, 216.4335774778780035 ) ) ;
#47258 = CARTESIAN_POINT ( 'NONE',  ( -39.59684760391189684, 1384.789378137079893, 241.4292011553590100 ) ) ;
#47259 = VECTOR ( 'NONE', #21193, 1000.000000000000000 ) ;
#47260 = LINE ( 'NONE', #81383, #103936 ) ;
#47261 = B_SPLINE_SURFACE_WITH_KNOTS ( 'NONE', 5, 3, ( 
 ( #49049, #83186, #51233, #6475 ),
 ( #40625, #74796, #32229, #66409 ),
 ( #23806, #79214, #34432, #43945 ),
 ( #87611, #306, #851, #52365 ),
 ( #19262, #1391, #68605, #53465 ),
 ( #34978, #60201, #78088, #85937 ) ),
 .UNSPECIFIED., .F., .F., .F.,
 ( 6, 6 ),
 ( 4, 4 ),
 ( 0.000000000000000000, 11.48858425020000062 ),
 ( 37.69911184309999896, 40.20365518519999881 ),
 .UNSPECIFIED. ) ;
#47262 = CARTESIAN_POINT ( 'NONE',  ( 12.24165105991550107, 1491.712733692510028, 207.8385283740699947 ) ) ;
#47263 = CARTESIAN_POINT ( 'NONE',  ( 32.00465973459103708, 1524.843178112495480, 216.1170700846211901 ) ) ;
#47264 = CARTESIAN_POINT ( 'NONE',  ( 7.976333483275767300, 1511.738168994444095, 205.8271000182464832 ) ) ;
#47265 = CARTESIAN_POINT ( 'NONE',  ( -10.41617235030460087, 1396.276801140979842, 212.8667543991859930 ) ) ;
#47266 = CARTESIAN_POINT ( 'NONE',  ( -14.46798390520000055, 1422.172973043230058, 228.7514975090980158 ) ) ;
#47267 = CARTESIAN_POINT ( 'NONE',  ( 19.28094568327996683, 1456.010430125557605, 225.1773291266683827 ) ) ;
#47268 = EDGE_LOOP ( 'NONE', ( #63588, #64151, #60264, #97121, #94131 ) ) ;
#47269 = EDGE_CURVE ( 'NONE', #71507, #44004, #85504, .T. ) ;
#47270 = CARTESIAN_POINT ( 'NONE',  ( -13.86092847646930082, 1410.765486861110048, 227.1170286572800023 ) ) ;
#47271 = CARTESIAN_POINT ( 'NONE',  ( -13.58498611669640077, 1508.504310626469987, 210.0344663469770126 ) ) ;
#47272 = FACE_OUTER_BOUND ( 'NONE', #56509, .T. ) ;
#47274 = CARTESIAN_POINT ( 'NONE',  ( -10.96015512746500065, 1512.830284628050094, 193.2119433744669834 ) ) ;
#47273 = CARTESIAN_POINT ( 'NONE',  ( 10.44233456949999983, 1425.120996158829939, 121.0077805707980048 ) ) ;
#47275 = CARTESIAN_POINT ( 'NONE',  ( 11.71230443242549057, 1428.980197708463947, 142.1750151601943912 ) ) ;
#47276 = CARTESIAN_POINT ( 'NONE',  ( -5.101062890589999732, 1453.677351314490124, 200.8020249629389866 ) ) ;
#47277 = CARTESIAN_POINT ( 'NONE',  ( -7.718134667564999774, 1516.881930554049859, 201.7919159189069944 ) ) ;
#47278 = CARTESIAN_POINT ( 'NONE',  ( 7.360599658199999062, 1427.547306193929899, 213.0878178632989943 ) ) ;
#47279 = CARTESIAN_POINT ( 'NONE',  ( -11.81707110430000007, 1430.266231075130008, 147.2485970657980090 ) ) ;
#47280 = CARTESIAN_POINT ( 'NONE',  ( 7.193668918159999315, 1509.090620986230078, 181.2520380256979990 ) ) ;
#47281 = CARTESIAN_POINT ( 'NONE',  ( -21.33070998724348755, 1509.431296620148714, 190.3921826398929795 ) ) ;
#47282 = CARTESIAN_POINT ( 'NONE',  ( -52.72375982305769782, 1377.543534630760178, 254.3719140001319943 ) ) ;
#47283 = CARTESIAN_POINT ( 'NONE',  ( 8.501157997614470219, 1365.972601565777268, 207.6218459616988241 ) ) ;
#47285 = VERTEX_POINT ( 'NONE', #45963 ) ;
#47284 = CARTESIAN_POINT ( 'NONE',  ( 16.06273934902591094, 1410.858425379293749, 191.5167191839988163 ) ) ;
#47286 = VERTEX_POINT ( 'NONE', #103652 ) ;
#47287 = CARTESIAN_POINT ( 'NONE',  ( -12.03082380390000061, 1397.656013067930189, 203.3051016873779986 ) ) ;
#47288 = CARTESIAN_POINT ( 'NONE',  ( 2.918579238077160021, 1409.742862551950111, 231.4428086086070095 ) ) ;
#47289 = CARTESIAN_POINT ( 'NONE',  ( 10.13545654959800046, 1453.511789294690061, 212.2748785446170245 ) ) ;
#47290 = CARTESIAN_POINT ( 'NONE',  ( -12.79393335520562225, 1444.983108077871066, 169.4500695159219106 ) ) ;
#47291 = CARTESIAN_POINT ( 'NONE',  ( -23.61227025210000008, 1435.322036687620084, 137.2858276859979867 ) ) ;
#47292 = CARTESIAN_POINT ( 'NONE',  ( -7.589847775084999526, 1511.982868782460173, 211.5342623288869959 ) ) ;
#47294 = CARTESIAN_POINT ( 'NONE',  ( -21.50985349126370139, 1505.528545743399945, 209.4501121847560228 ) ) ;
#47293 = CARTESIAN_POINT ( 'NONE',  ( -8.022767810259999521, 1384.891328718040086, 218.7875262017990110 ) ) ;
#47295 = CARTESIAN_POINT ( 'NONE',  ( -30.61443310237140381, 1523.382868172863937, 196.4193608261162467 ) ) ;
#47296 = PLANE ( 'NONE',  #110469 ) ;
#47297 = CARTESIAN_POINT ( 'NONE',  ( -41.27932424117140187, 1445.656587030789979, 136.3077099605269780 ) ) ;
#47298 = CARTESIAN_POINT ( 'NONE',  ( 10.17615046018800129, 1396.268419396740001, 204.7703056290459926 ) ) ;
#47299 = FACE_OUTER_BOUND ( 'NONE', #57601, .T. ) ;
#47300 = CARTESIAN_POINT ( 'NONE',  ( 11.65217179949999959, 1425.851026166929842, 145.3825519544979841 ) ) ;
#47301 = CARTESIAN_POINT ( 'NONE',  ( 41.65883123370000618, 1443.939564121179956, 136.1335272508979983 ) ) ;
#47302 = EDGE_LOOP ( 'NONE', ( #32160, #27178, #39754, #4721 ) ) ;
#47303 = CARTESIAN_POINT ( 'NONE',  ( 4.091329073579999864, 1425.301743040829933, 185.3866542801980017 ) ) ;
#47304 = CARTESIAN_POINT ( 'NONE',  ( 12.45988844690000086, 1442.668228039740143, 187.1806564808980227 ) ) ;
#47305 = ORIENTED_EDGE ( 'NONE', *, *, #34725, .F. ) ;
#47306 = ORIENTED_EDGE ( 'NONE', *, *, #23299, .F. ) ;
#47307 = EDGE_CURVE ( 'NONE', #56739, #14033, #1494, .T. ) ;
#47308 = CARTESIAN_POINT ( 'NONE',  ( -17.46087120122630054, 1458.256338415900018, 228.1902854820540085 ) ) ;
#47309 = CARTESIAN_POINT ( 'NONE',  ( -14.35945310470000180, 1461.065408120830170, 229.7470706200979862 ) ) ;
#47310 = CARTESIAN_POINT ( 'NONE',  ( -17.03290348309940683, 1409.881251522323964, 225.5427118406987006 ) ) ;
#47311 = CARTESIAN_POINT ( 'NONE',  ( 12.61812115829999925, 1416.825245919230156, 196.1892291636980019 ) ) ;
#47312 = CARTESIAN_POINT ( 'NONE',  ( 2.875850094215000041, 1516.647618671360078, 214.8936433964170192 ) ) ;
#47313 = CARTESIAN_POINT ( 'NONE',  ( -13.88306073332670110, 1379.761802596040070, 208.2296390988570067 ) ) ;
#47314 = ORIENTED_EDGE ( 'NONE', *, *, #85613, .F. ) ;
#47315 = CARTESIAN_POINT ( 'NONE',  ( -18.30672310084519694, 1508.551704408389924, 210.5933980790459827 ) ) ;
#47316 = CARTESIAN_POINT ( 'NONE',  ( 0.05162197306659999790, 1509.009019568429949, 179.2212271949979936 ) ) ;
#47317 = CARTESIAN_POINT ( 'NONE',  ( -58.56722971349999796, 1374.895658628189949, 258.8926058799589782 ) ) ;
#47318 = DIRECTION ( 'NONE',  ( -0.7044160264027579110, -0.08715574274767008689, -0.7044160264027579110 ) ) ;
#47319 = CARTESIAN_POINT ( 'NONE',  ( -3.459156616214999591, 1516.769879638719885, 204.5118493505569859 ) ) ;
#47320 = ORIENTED_EDGE ( 'NONE', *, *, #10614, .F. ) ;
#47321 = CARTESIAN_POINT ( 'NONE',  ( -19.97699668690000152, 1508.102459366529956, 229.1407657077979820 ) ) ;
#47322 = CARTESIAN_POINT ( 'NONE',  ( -21.90170135886932457, 1414.871184935607744, 269.4017551159469690 ) ) ;
#47323 = CARTESIAN_POINT ( 'NONE',  ( -0.4274081085919999579, 1409.096031296729961, 232.6209005452979852 ) ) ;
#47325 = EDGE_LOOP ( 'NONE', ( #14659, #34118, #51111, #60767 ) ) ;
#47324 = DIRECTION ( 'NONE',  ( -1.000000000000000000, 0.000000000000000000, 0.000000000000000000 ) ) ;
#47326 = CARTESIAN_POINT ( 'NONE',  ( 2.500000000000000000, 1424.377232884329942, 154.7346221771979913 ) ) ;
#47327 = CARTESIAN_POINT ( 'NONE',  ( -31.04776337085569793, 1440.913060388089889, 241.5191150371310016 ) ) ;
#47328 = CIRCLE ( 'NONE', #16908, 2.000000000000003553 ) ;
#47329 = CARTESIAN_POINT ( 'NONE',  ( -38.49145949329999894, 1384.794605546870116, 239.3122526757589981 ) ) ;
#47330 = CARTESIAN_POINT ( 'NONE',  ( -0.1879632238746349882, 1466.387553677260030, 235.6886251357990147 ) ) ;
#47331 = CARTESIAN_POINT ( 'NONE',  ( 27.66281618764540084, 1417.733632362909930, 269.4444038297550037 ) ) ;
#47332 = AXIS2_PLACEMENT_3D ( 'NONE', #4001, #2363, #96950 ) ;
#47333 = CARTESIAN_POINT ( 'NONE',  ( 7.723480079395000253, 1517.086065052259983, 213.1573821953169841 ) ) ;
#47334 = CARTESIAN_POINT ( 'NONE',  ( -65.09292129899999679, 1379.738243665130085, 272.5656652546590522 ) ) ;
#47335 = CARTESIAN_POINT ( 'NONE',  ( 23.08676684170000115, 1409.825010724229969, 208.4789857369090100 ) ) ;
#47336 = CARTESIAN_POINT ( 'NONE',  ( 0.02089856015480650100, 1507.111761549349922, 237.3522809668369860 ) ) ;
#47337 = CARTESIAN_POINT ( 'NONE',  ( 6.900299337267749245, 1425.082553785249956, 192.4924159130339945 ) ) ;
#47339 = ADVANCED_FACE ( 'NONE', ( #37550 ), #70636, .T. ) ;
#47338 = CARTESIAN_POINT ( 'NONE',  ( -7.719696504299309758, 1516.941612417570013, 209.0971862408350148 ) ) ;
#47340 = CARTESIAN_POINT ( 'NONE',  ( -4.608021707265000266, 1516.660388280709867, 210.8351633799069873 ) ) ;
#47341 = EDGE_CURVE ( 'NONE', #90450, #61502, #6828, .T. ) ;
#47342 = CARTESIAN_POINT ( 'NONE',  ( 4.401092417150000102, 1420.174153566729956, 185.7217845719979721 ) ) ;
#47343 = CARTESIAN_POINT ( 'NONE',  ( 2.759768239755020058, 1516.551696783219995, 216.8313331240459831 ) ) ;
#47344 = EDGE_CURVE ( 'NONE', #78256, #100339, #105201, .T. ) ;
#47345 = EDGE_LOOP ( 'NONE', ( #25121, #99579, #103285, #60785 ) ) ;
#47346 = CARTESIAN_POINT ( 'NONE',  ( -24.11259409631230000, 1385.259584648939835, 223.0827457712539967 ) ) ;
#47347 = CARTESIAN_POINT ( 'NONE',  ( 18.90720652019999903, 1416.826388498430106, 210.0261622758970077 ) ) ;
#47348 = EDGE_CURVE ( 'NONE', #67457, #26746, #89746, .T. ) ;
#47349 = CARTESIAN_POINT ( 'NONE',  ( 0.2257619562299999771, 1417.282465340730141, 234.8473851690980041 ) ) ;
#47350 = EDGE_CURVE ( 'NONE', #27144, #10158, #3315, .T. ) ;
#47351 = B_SPLINE_SURFACE_WITH_KNOTS ( 'NONE', 5, 5, ( 
 ( #26467, #67406, #17495, #92566, #58997, #101504 ),
 ( #85834, #66853, #43297, #34877, #60662, #18064 ),
 ( #100962, #44967, #29243, #52806, #11895, #71848 ),
 ( #28137, #63433, #95345, #43842, #103743, #95895 ),
 ( #70188, #18607, #53932, #46068, #97550, #77988 ),
 ( #104297, #52258, #71291, #79666, #2970, #37088 ) ),
 .UNSPECIFIED., .F., .F., .F.,
 ( 6, 6 ),
 ( 6, 6 ),
 ( 3.274326487366419958, 6.007249690403580367 ),
 ( -2.359960357783379966E-05, 2.000000000000000000 ),
 .UNSPECIFIED. ) ;
#47352 = FACE_OUTER_BOUND ( 'NONE', #17164, .T. ) ;
#47353 = LINE ( 'NONE', #96658, #16875 ) ;
#47354 = CARTESIAN_POINT ( 'NONE',  ( 11.15518508559999944, 1425.266589066719916, 204.1085830429390171 ) ) ;
#47355 = CARTESIAN_POINT ( 'NONE',  ( 0.6019981773732412389, 1498.612803264159538, 197.8140259511527006 ) ) ;
#47356 = EDGE_CURVE ( 'NONE', #13762, #49801, #21153, .T. ) ;
#47358 = CARTESIAN_POINT ( 'NONE',  ( 18.16418870590809931, 1416.835419214280137, 209.1673351295509917 ) ) ;
#47357 = CARTESIAN_POINT ( 'NONE',  ( -1.124894088365000044, 1517.194816588360027, 216.0733631026070043 ) ) ;
#47359 = CARTESIAN_POINT ( 'NONE',  ( -25.59985477246175378, 1450.799230641226586, 137.0693086342491256 ) ) ;
#47360 = CARTESIAN_POINT ( 'NONE',  ( 11.21992499831749868, 1470.403109959280073, 207.2954163329770267 ) ) ;
#47361 = ORIENTED_EDGE ( 'NONE', *, *, #27023, .F. ) ;
#47362 = CARTESIAN_POINT ( 'NONE',  ( -5.004442077115000664, 1516.690345681169902, 201.4087281291169802 ) ) ;
#47363 = DIRECTION ( 'NONE',  ( 0.3282391760791589785, -0.000000000000000000, 0.9445946449598763284 ) ) ;
#47364 = ORIENTED_EDGE ( 'NONE', *, *, #89465, .F. ) ;
#47365 = CARTESIAN_POINT ( 'NONE',  ( -15.18044686046500935, 1511.791180387469922, 220.8782529452671497 ) ) ;
#47366 = AXIS2_PLACEMENT_3D ( 'NONE', #5984, #88473, #107885 ) ;
#47367 = CARTESIAN_POINT ( 'NONE',  ( 20.63648295220000151, 1455.268815933329961, 222.7070109917980290 ) ) ;
#47368 = CARTESIAN_POINT ( 'NONE',  ( 10.95486373408519931, 1461.099043641600019, 209.0941366827430272 ) ) ;
#47369 = CARTESIAN_POINT ( 'NONE',  ( -119.4674887953348872, 1384.913060387289988, 299.8135573092559412 ) ) ;
#47370 = EDGE_CURVE ( 'NONE', #47286, #21147, #76658, .T. ) ;
#47371 = CARTESIAN_POINT ( 'NONE',  ( 2.032300221149999864, 1441.827160225690022, 218.8459470114090379 ) ) ;
#47372 = CARTESIAN_POINT ( 'NONE',  ( -28.01951961465029939, 1509.887603853479959, 200.8921116242010214 ) ) ;
#47373 = CARTESIAN_POINT ( 'NONE',  ( 4.967684365510000255, 1469.890599266690060, 189.7939106698990201 ) ) ;
#47374 = CARTESIAN_POINT ( 'NONE',  ( -19.28416521189999955, 1426.095206623730064, 225.9565170197979853 ) ) ;
#47375 = CARTESIAN_POINT ( 'NONE',  ( -29.59241942509761003, 1466.933728989316251, 269.3641340189501534 ) ) ;
#47376 = CARTESIAN_POINT ( 'NONE',  ( -104.3158487040000040, 1389.466353268959892, 300.6607691406589993 ) ) ;
#47377 = FACE_OUTER_BOUND ( 'NONE', #7043, .T. ) ;
#47379 = CARTESIAN_POINT ( 'NONE',  ( 28.27265630610000002, 1508.146186351229971, 209.2480474313609875 ) ) ;
#47378 = CARTESIAN_POINT ( 'NONE',  ( -105.9112875430000145, 1391.839465932129997, 303.4711480509590160 ) ) ;
#47380 = EDGE_CURVE ( 'NONE', #79801, #77058, #19332, .T. ) ;
#47381 = AXIS2_PLACEMENT_3D ( 'NONE', #241, #7505, #75824 ) ;
#47382 = CARTESIAN_POINT ( 'NONE',  ( -10.16240527536719895, 1472.558926193989919, 209.8189312950259762 ) ) ;
#47384 = VERTEX_POINT ( 'NONE', #25131 ) ;
#47383 = B_SPLINE_CURVE_WITH_KNOTS ( 'NONE', 3,
 ( #54325, #35849, #36934, #105819, #21203, #106349, #36389, #29635, #20666, #45911, #20131, #12278, #53783, #46472, #87920, #105252, #2815, #63822, #70034, #88455, #27431, #70578, #63282, #3369, #61614, #97935, #80603, #80047, #88990, #27990, #10082, #11742, #54867, #29097, #97396, #62744, #3919 ),
 .UNSPECIFIED., .F., .F.,
 ( 4, 3, 3, 3, 3, 3, 3, 3, 3, 3, 3, 3, 4 ),
 ( -13.59025040360000069, -13.39461751845870019, -12.66963757110119992, -11.90222376896450029, -11.09384317622529892, -10.22895211640910063, -9.214965427742340509, -8.224269270894209782, -7.395227323644159689, -6.444494315334388546, -5.598046305014300117, -4.859242130686430627, -4.164915011539999767 ),
 .UNSPECIFIED. ) ;
#47385 = DIRECTION ( 'NONE',  ( -0.0001837273416260859385, 0.9990401814439695549, 0.04380276366468503074 ) ) ;
#47386 = CARTESIAN_POINT ( 'NONE',  ( -13.11794498660000130, 1508.551704418990084, 216.7314840583389923 ) ) ;
#47387 = CARTESIAN_POINT ( 'NONE',  ( -7.878537825433329367, 1517.151704408390060, 218.1850669711710111 ) ) ;
#47388 = ADVANCED_FACE ( 'NONE', ( #42500 ), #65892, .T. ) ;
#47389 = CARTESIAN_POINT ( 'NONE',  ( 11.25715570474750038, 1470.474397315270153, 207.5113747759559999 ) ) ;
#47390 = CARTESIAN_POINT ( 'NONE',  ( -13.22806383169999833, 1431.113060387329824, 222.3499097936980036 ) ) ;
#47391 = CARTESIAN_POINT ( 'NONE',  ( -10.46250751532009993, 1491.356802638789986, 212.5409670664860187 ) ) ;
#47392 = CARTESIAN_POINT ( 'NONE',  ( -2.596261494520262225, 1525.907212628473644, 240.7735774411712271 ) ) ;
#47393 = CARTESIAN_POINT ( 'NONE',  ( -12.65578976995832861, 1442.797870648871594, 186.1192285427375737 ) ) ;
#47394 = B_SPLINE_SURFACE_WITH_KNOTS ( 'NONE', 4, 5, ( 
 ( #82763, #22269, #75489, #109622, #107958, #90603 ),
 ( #64888, #74389, #32894, #16083, #48067, #92811 ),
 ( #30702, #31252, #65435, #31804, #23397, #57586 ),
 ( #91711, #86617, #93903, #34562, #42977, #76563 ),
 ( #9911, #69295, #33439, #43531, #35664, #42410 ) ),
 .UNSPECIFIED., .F., .F., .F.,
 ( 5, 5 ),
 ( 6, 6 ),
 ( 0.000000000000000000, 4.166045933440000404 ),
 ( 0.000000000000000000, 0.5000005421829999408 ),
 .UNSPECIFIED. ) ;
#47395 = CARTESIAN_POINT ( 'NONE',  ( -16.81223226430000039, 1414.913060387329779, 207.5743821216680089 ) ) ;
#47396 = DIRECTION ( 'NONE',  ( 1.000000000000000000, 0.000000000000000000, 0.000000000000000000 ) ) ;
#47397 = ADVANCED_FACE ( 'NONE', ( #84503 ), #41413, .F. ) ;
#47398 = CARTESIAN_POINT ( 'NONE',  ( -7.798516306275617538, 1417.059749218360821, 231.0301366618491272 ) ) ;
#47399 = CARTESIAN_POINT ( 'NONE',  ( -5.623474965688048840E-07, 1451.660737107639989, 154.0815186765750013 ) ) ;
#47400 = CARTESIAN_POINT ( 'NONE',  ( 18.59804234570002279, 1425.273062378426175, 226.9839929844980304 ) ) ;
#47401 = CARTESIAN_POINT ( 'NONE',  ( 7.393822440330000134, 1429.049734447289893, 215.1950306291689969 ) ) ;
#47403 = EDGE_LOOP ( 'NONE', ( #53557, #104542, #54089, #48427, #16334 ) ) ;
#47402 = CARTESIAN_POINT ( 'NONE',  ( 17.01540922059999872, 1497.106364323189837, 222.9636020297990058 ) ) ;
#47404 = CARTESIAN_POINT ( 'NONE',  ( -113.4000000000000057, 1382.004344128540197, 297.9600760927590386 ) ) ;
#47405 = CARTESIAN_POINT ( 'NONE',  ( -16.65010197087777399, 1526.345556099435726, 234.9005341682540973 ) ) ;
#47406 = EDGE_LOOP ( 'NONE', ( #44293, #75179, #96745, #58092, #78475 ) ) ;
#47407 = EDGE_LOOP ( 'NONE', ( #2775, #27127, #15231, #34080, #93689 ) ) ;
#47408 = CARTESIAN_POINT ( 'NONE',  ( 16.88248175295160181, 1414.913057834419988, 210.3124741370610025 ) ) ;
#47409 = CARTESIAN_POINT ( 'NONE',  ( 13.94913730080000036, 1509.400263820630016, 234.9268341509979905 ) ) ;
#47410 = CARTESIAN_POINT ( 'NONE',  ( -8.393274306154939524, 1382.788095255750022, 199.9340640290776321 ) ) ;
#47412 = CARTESIAN_POINT ( 'NONE',  ( -21.00608537319999769, 1461.014378767029939, 244.4374624616980043 ) ) ;
#47411 = CARTESIAN_POINT ( 'NONE',  ( 34.75159598319835652, 1423.783191157365536, 269.5281025998144742 ) ) ;
#47413 = AXIS2_PLACEMENT_3D ( 'NONE', #39739, #108595, #82291 ) ;
#47414 = CARTESIAN_POINT ( 'NONE',  ( -20.40938849349999984, 1503.704554046830026, 189.8792483973980154 ) ) ;
#47415 = CARTESIAN_POINT ( 'NONE',  ( -11.89389463660000068, 1433.576802385009842, 150.4827622296980110 ) ) ;
#47416 = DIRECTION ( 'NONE',  ( -5.980589973904019347E-17, 1.000000000000000000, -1.736889445713099699E-16 ) ) ;
#47417 = CARTESIAN_POINT ( 'NONE',  ( 11.68805093410779961, 1426.728226893330202, 140.6662312984289827 ) ) ;
#47418 = CARTESIAN_POINT ( 'NONE',  ( 27.51968813986070117, 1491.156149288490042, 209.4200479053579897 ) ) ;
#47419 = CARTESIAN_POINT ( 'NONE',  ( -1.356522590142140050, 1410.335674017130032, 185.6037846924129724 ) ) ;
#47420 = CARTESIAN_POINT ( 'NONE',  ( -0.04897144331352380753, 1515.158513834189989, 213.4488405682529617 ) ) ;
#47421 = CARTESIAN_POINT ( 'NONE',  ( -19.01706420256807917, 1526.382868172863937, 185.3900685784704478 ) ) ;
#47422 = CARTESIAN_POINT ( 'NONE',  ( -5.368410399077579775, 1477.261207538329927, 219.3405594986899985 ) ) ;
#47423 = CARTESIAN_POINT ( 'NONE',  ( -4.512821541280432669, 1361.898012553873741, 207.6218459616988241 ) ) ;
#47424 = CARTESIAN_POINT ( 'NONE',  ( 31.47409394596293453, 1526.278758871496848, 199.6577681796570118 ) ) ;
#47425 = EDGE_CURVE ( 'NONE', #77064, #99465, #10477, .T. ) ;
#47427 = EDGE_LOOP ( 'NONE', ( #13844, #107478, #102362, #22652 ) ) ;
#47426 = CARTESIAN_POINT ( 'NONE',  ( 5.857070821897849958E-09, 1409.867647545549971, 258.8986024302779470 ) ) ;
#47428 = ORIENTED_EDGE ( 'NONE', *, *, #11795, .F. ) ;
#47429 = CARTESIAN_POINT ( 'NONE',  ( -11.74583512589999934, 1503.658496363889981, 208.1214728489190122 ) ) ;
#47430 = CARTESIAN_POINT ( 'NONE',  ( -18.85104330493919633, 1504.529957806199945, 222.4016543459620152 ) ) ;
#47431 = CARTESIAN_POINT ( 'NONE',  ( -25.02521468490000345, 1466.386952600029872, 270.1035466365980255 ) ) ;
#47432 = CARTESIAN_POINT ( 'NONE',  ( -1.547118986179999878, 1416.568813549730066, 228.0093688194979791 ) ) ;
#47433 = DIRECTION ( 'NONE',  ( 0.000000000000000000, 0.000000000000000000, -1.000000000000000000 ) ) ;
#47434 = CARTESIAN_POINT ( 'NONE',  ( 35.18816452081259882, 1451.157525408279980, 135.9224998729500271 ) ) ;
#47435 = CARTESIAN_POINT ( 'NONE',  ( 4.326992699981060397, 1515.158586643130093, 209.1431034449670108 ) ) ;
#47436 = CARTESIAN_POINT ( 'NONE',  ( 4.908653116315950804, 1484.161144941180055, 219.8999275612819986 ) ) ;
#47437 = CARTESIAN_POINT ( 'NONE',  ( 21.92444878912329997, 1509.678679009930192, 227.6602567754504491 ) ) ;
#47438 = CARTESIAN_POINT ( 'NONE',  ( -6.120030076239999950, 1458.493692400089913, 216.6798046192089942 ) ) ;
#47439 = CARTESIAN_POINT ( 'NONE',  ( 10.40445411670284415, 1362.691325679774536, 210.6218459617030021 ) ) ;
#47440 = CARTESIAN_POINT ( 'NONE',  ( -33.19754209624489505, 1417.174461616820054, 269.2945989659730230 ) ) ;
#47441 = ORIENTED_EDGE ( 'NONE', *, *, #85145, .T. ) ;
#47442 = DIRECTION ( 'NONE',  ( 1.000000000000000000, 0.000000000000000000, 0.000000000000000000 ) ) ;
#47443 = EDGE_LOOP ( 'NONE', ( #53269, #11021, #70234, #36505 ) ) ;
#47444 = VERTEX_POINT ( 'NONE', #8887 ) ;
#47445 = CARTESIAN_POINT ( 'NONE',  ( -1.700259714084999763, 1516.898441858519845, 210.8400494336869997 ) ) ;
#47446 = EDGE_CURVE ( 'NONE', #90113, #7633, #7793, .T. ) ;
#47447 = CARTESIAN_POINT ( 'NONE',  ( 17.22592475669603473, 1444.324653571829685, 162.9227486557985003 ) ) ;
#47449 = CARTESIAN_POINT ( 'NONE',  ( -17.63102292954804895, 1419.721208921065681, 206.9322081005539360 ) ) ;
#47448 = CARTESIAN_POINT ( 'NONE',  ( -2.283570671295000132, 1516.909589401870107, 212.0033943946770023 ) ) ;
#47450 = CARTESIAN_POINT ( 'NONE',  ( -17.78468008800000177, 1440.443143732879889, 191.0126434879979911 ) ) ;
#47451 = CARTESIAN_POINT ( 'NONE',  ( -18.63578313170000200, 1416.568813547830132, 208.5538819738139864 ) ) ;
#47452 = VERTEX_POINT ( 'NONE', #34101 ) ;
#47453 = CARTESIAN_POINT ( 'NONE',  ( -26.64894350899999864, 1436.272083837089895, 136.6568872077980075 ) ) ;
#47454 = CIRCLE ( 'NONE', #27774, 1.000000000000000888 ) ;
#47455 =( BOUNDED_SURFACE ( )  B_SPLINE_SURFACE ( 3, 2, ( 
 ( #9662, #84709, #43833 ),
 ( #50581, #41624, #59536 ),
 ( #18055, #77979, #76326 ),
 ( #61223, #68498, #103158 ),
 ( #109931, #85259, #60654 ),
 ( #93648, #77437, #102597 ),
 ( #25898, #110476, #43289 ),
 ( #8009, #196, #34869 ),
 ( #7462, #84161, #60096 ),
 ( #94212, #33208, #16931 ),
 ( #42728, #34320, #75778 ),
 ( #1287, #67398, #76887 ),
 ( #17487, #736, #101496 ),
 ( #69057, #51685, #26459 ) ),
 .UNSPECIFIED., .F., .F., .F. ) 
 B_SPLINE_SURFACE_WITH_KNOTS ( ( 4, 2, 2, 2, 2, 2, 4 ),
 ( 3, 3 ),
 ( 7.665309359472516348E-17, 0.0009443072508236404188, 0.001416460876235422356, 0.001888614501647204293, 0.002360768127058986230, 0.002832921752470767950, 0.003777229003294331824 ),
 ( 0.000000000000000000, 1.000000000000000000 ),
 .UNSPECIFIED. ) 
 GEOMETRIC_REPRESENTATION_ITEM ( )  RATIONAL_B_SPLINE_SURFACE ( (
 ( 1.000000000000000000, 0.9376006582765954445, 1.000000000000000000),
 ( 1.000000000000000000, 0.9283977714737452480, 1.000000000000000000),
 ( 1.000000000000000000, 0.9189750060478982796, 1.000000000000000000),
 ( 1.000000000000000000, 0.9042792056127966216, 1.000000000000000000),
 ( 1.000000000000000000, 0.8992469033839340931, 1.000000000000000000),
 ( 1.000000000000000000, 0.8891280264686174384, 1.000000000000000000),
 ( 1.000000000000000000, 0.8840337471669303948, 1.000000000000000000),
 ( 1.000000000000000000, 0.8736395124169680226, 1.000000000000000000),
 ( 1.000000000000000000, 0.8683406746541313392, 1.000000000000000000),
 ( 1.000000000000000000, 0.8573361860719177496, 1.000000000000000000),
 ( 1.000000000000000000, 0.8516508399498529114, 1.000000000000000000),
 ( 1.000000000000000000, 0.8340914917061317269, 1.000000000000000000),
 ( 1.000000000000000000, 0.8215597275865531568, 1.000000000000000000),
 ( 1.000000000000000000, 0.8070209408750207425, 1.000000000000000000) ) ) 
 REPRESENTATION_ITEM ( '' )  SURFACE ( )  );
#47456 = CARTESIAN_POINT ( 'NONE',  ( -4.616861546545000472, 1516.666407245520077, 201.4093549791169835 ) ) ;
#47457 = EDGE_CURVE ( 'NONE', #63901, #54088, #75580, .T. ) ;
#47458 = FACE_OUTER_BOUND ( 'NONE', #97187, .T. ) ;
#47460 = CIRCLE ( 'NONE', #13451, 1.999999999999999556 ) ;
#47459 = CARTESIAN_POINT ( 'NONE',  ( -26.52518363774159837, 1384.548060173010072, 203.9081812816960166 ) ) ;
#47461 = CARTESIAN_POINT ( 'NONE',  ( -44.43458752740489359, 1435.686101446479825, 270.0922352104699939 ) ) ;
#47462 = CARTESIAN_POINT ( 'NONE',  ( 2.936137002789280359, 1417.857599898479975, 233.6311759696189938 ) ) ;
#47463 = CARTESIAN_POINT ( 'NONE',  ( -2.349329596450000057, 1396.056272350230074, 197.6305884707980169 ) ) ;
#47464 = ADVANCED_FACE ( 'NONE', ( #68293 ), #77228, .F. ) ;
#47466 = EDGE_LOOP ( 'NONE', ( #97162, #99898, #28353, #67451 ) ) ;
#47465 = CARTESIAN_POINT ( 'NONE',  ( -8.543947113920394187, 1365.600700106919930, 210.6218459617142003 ) ) ;
#47467 = ORIENTED_EDGE ( 'NONE', *, *, #55611, .F. ) ;
#47468 = CARTESIAN_POINT ( 'NONE',  ( 44.72902951799282079, 1447.701297687701526, 269.0001835098157699 ) ) ;
#47469 = CARTESIAN_POINT ( 'NONE',  ( 2.740633910414560059, 1466.650861077639775, 219.8322804162909847 ) ) ;
#47470 = CARTESIAN_POINT ( 'NONE',  ( 3.005276066430000448, 1369.205039411269809, 207.6218459616989946 ) ) ;
#47471 = CARTESIAN_POINT ( 'NONE',  ( -2.793439694759999981, 1486.025328433629966, 182.0741016712979956 ) ) ;
#47472 = CARTESIAN_POINT ( 'NONE',  ( 1.718203463455000080, 1516.898441858519845, 210.8221056461869978 ) ) ;
#47473 = CARTESIAN_POINT ( 'NONE',  ( -68.77805555110001023, 1379.747954593040049, 280.2446631412590250 ) ) ;
#47474 = CARTESIAN_POINT ( 'NONE',  ( -33.28034951413919629, 1522.862737210649811, 217.4407153818824554 ) ) ;
#47475 = CARTESIAN_POINT ( 'NONE',  ( 6.666983987850649385, 1439.588742573630043, 215.5177180616709904 ) ) ;
#47476 = CARTESIAN_POINT ( 'NONE',  ( 11.68483146220000002, 1415.296882296330068, 223.0065844743980108 ) ) ;
#47477 = ADVANCED_FACE ( 'NONE', ( #101275 ), #25049, .T. ) ;
#47478 = CARTESIAN_POINT ( 'NONE',  ( 7.848179674985000354, 1511.193640125469983, 204.5989548728170178 ) ) ;
#47479 = CARTESIAN_POINT ( 'NONE',  ( -4.043990345725000601, 1516.983612918759945, 206.6425990843970055 ) ) ;
#47480 = ORIENTED_EDGE ( 'NONE', *, *, #40496, .T. ) ;
#47481 = CARTESIAN_POINT ( 'NONE',  ( -33.91369111065759512, 1451.728768197430099, 135.0584859664319879 ) ) ;
#47482 = CARTESIAN_POINT ( 'NONE',  ( -1.949295105551302365, 1516.541277319989604, 201.8775772585021286 ) ) ;
#47483 = ORIENTED_EDGE ( 'NONE', *, *, #63813, .T. ) ;
#47484 = CARTESIAN_POINT ( 'NONE',  ( 5.136464557128770814, 1457.210140256051773, 228.2402603896014739 ) ) ;
#47485 = ADVANCED_FACE ( 'NONE', ( #58763 ), #104406, .F. ) ;
#47486 = CARTESIAN_POINT ( 'NONE',  ( -18.89924245745137554, 1416.831922880734282, 207.5749492336007904 ) ) ;
#47487 = CARTESIAN_POINT ( 'NONE',  ( 13.50890991390000018, 1415.048591094029916, 197.7020156336979824 ) ) ;
#47488 = CARTESIAN_POINT ( 'NONE',  ( -9.094202543475169875, 1384.745265098430082, 199.9473045631640105 ) ) ;
#47489 = CARTESIAN_POINT ( 'NONE',  ( 22.30118273070000257, 1410.611534642730248, 204.7343940648379714 ) ) ;
#47490 = CARTESIAN_POINT ( 'NONE',  ( 16.84507916019999740, 1409.666197915029898, 225.6438639091979894 ) ) ;
#47491 = CARTESIAN_POINT ( 'NONE',  ( 10.68762204729999965, 1490.102721893990065, 205.8926831195890088 ) ) ;
#47492 = CARTESIAN_POINT ( 'NONE',  ( -5.923682464646780943, 1517.051704408389924, 223.8623791742500089 ) ) ;
#47493 = CARTESIAN_POINT ( 'NONE',  ( 24.58641666395997305, 1443.335256792440759, 213.0934990515747529 ) ) ;
#47494 = EDGE_CURVE ( 'NONE', #49356, #76758, #30822, .T. ) ;
#47495 = CARTESIAN_POINT ( 'NONE',  ( -5.001338666445000136, 1516.911981270829983, 214.9058546054269812 ) ) ;
#47496 = VERTEX_POINT ( 'NONE', #24858 ) ;
#47497 = CARTESIAN_POINT ( 'NONE',  ( 7.708939270935911026, 1516.530773980259937, 207.1624426174489884 ) ) ;
#47498 = DIRECTION ( 'NONE',  ( 0.9999999993216598382, 3.683192149143328935E-05, 3.002444966984699305E-07 ) ) ;
#47499 = CARTESIAN_POINT ( 'NONE',  ( 3.071538966616300659, 1375.413060387289988, 210.7998353468136941 ) ) ;
#47500 = ADVANCED_FACE ( 'NONE', ( #811 ), #12356, .T. ) ;
#47501 = CARTESIAN_POINT ( 'NONE',  ( -31.92108011125358047, 1512.187213306747481, 197.2845127572065849 ) ) ;
#47502 = AXIS2_PLACEMENT_3D ( 'NONE', #42865, #26594, #8684 ) ;
#47503 = CARTESIAN_POINT ( 'NONE',  ( -37.74895065031819996, 1449.030701455520102, 136.3532337052970149 ) ) ;
#47504 = CARTESIAN_POINT ( 'NONE',  ( 20.71343476517513338, 1501.977400791986611, 179.9059455038194528 ) ) ;
#47505 = DIRECTION ( 'NONE',  ( 1.000000000000000000, 0.000000000000000000, 0.000000000000000000 ) ) ;
#47506 = CARTESIAN_POINT ( 'NONE',  ( 18.00600711065910531, 1424.203672432876601, 225.4083150014673436 ) ) ;
#47507 = CARTESIAN_POINT ( 'NONE',  ( -0.6415093019302169353, 1455.478019572560015, 198.6153582363290013 ) ) ;
#47508 = LINE ( 'NONE', #81632, #86282 ) ;
#47509 = B_SPLINE_SURFACE_WITH_KNOTS ( 'NONE', 5, 5, ( 
 ( #9782, #87043, #34981, #70843, #26574, #79767 ),
 ( #43948, #88164, #56066, #27693, #62432, #103846 ),
 ( #94895, #52367, #64488, #27146, #21867, #19829 ),
 ( #3074, #79215, #2523, #43400, #87612, #18715 ),
 ( #98603, #11452, #44503, #38696, #90193, #77551 ),
 ( #86487, #61331, #78650, #1965, #36102, #104398 ),
 ( #61879, #66688, #56620, #6199, #67237, #109771 ),
 ( #33049, #24085, #109233, #81795, #100795, #48226 ),
 ( #90755, #7308, #73972, #41474, #82908, #75083 ) ),
 .UNSPECIFIED., .F., .F., .F.,
 ( 6, 3, 6 ),
 ( 6, 6 ),
 ( 4.119224442280000176, 8.124444112980000909, 13.43342673250000097 ),
 ( 0.000000000000000000, 2.000000000000000000 ),
 .UNSPECIFIED. ) ;
#47510 = CARTESIAN_POINT ( 'NONE',  ( 29.68293233167989698, 1440.913060386479856, 237.3170996871120053 ) ) ;
#47511 = CARTESIAN_POINT ( 'NONE',  ( -11.14782975800259912, 1470.277812220770102, 211.4323380035779962 ) ) ;
#47512 = CARTESIAN_POINT ( 'NONE',  ( 8.761752346032359640, 1498.445853823050129, 199.9005563031199983 ) ) ;
#47513 = ORIENTED_EDGE ( 'NONE', *, *, #41570, .F. ) ;
#47514 = VERTEX_POINT ( 'NONE', #4122 ) ;
#47515 = EDGE_CURVE ( 'NONE', #29266, #40040, #72430, .T. ) ;
#47516 = CARTESIAN_POINT ( 'NONE',  ( -7.012921474261649024, 1508.551704408390151, 202.7299072940186875 ) ) ;
#47517 = CARTESIAN_POINT ( 'NONE',  ( -1.725662463192670248, 1484.236887848700007, 182.7463278875050037 ) ) ;
#47518 = CARTESIAN_POINT ( 'NONE',  ( -1.326067526109999895, 1442.466427602190151, 200.3461943362390230 ) ) ;
#47519 = CARTESIAN_POINT ( 'NONE',  ( -5.036242141850692633, 1491.189339853503043, 188.8516911269720993 ) ) ;
#47520 = EDGE_CURVE ( 'NONE', #37990, #73491, #37708, .T. ) ;
#47521 = DIRECTION ( 'NONE',  ( -0.6736849260863841948, 0.000000000000000000, 0.7390186874254148774 ) ) ;
#47522 = CARTESIAN_POINT ( 'NONE',  ( 1.840021611441419846, 1508.551704408389924, 219.7092512643660029 ) ) ;
#47523 = CARTESIAN_POINT ( 'NONE',  ( -50.96332219156189325, 1383.810333793590189, 263.3241036801269956 ) ) ;
#47524 = CIRCLE ( 'NONE', #63469, 11.71219856409999949 ) ;
#47525 = CARTESIAN_POINT ( 'NONE',  ( -3.780286426965000057, 1510.542924508009946, 201.5697040178069983 ) ) ;
#47526 = CARTESIAN_POINT ( 'NONE',  ( -14.73399051909999891, 1489.466620109829819, 192.5160264904980068 ) ) ;
#47527 = CARTESIAN_POINT ( 'NONE',  ( -12.62836648000669904, 1502.649130299180115, 209.0071212651150176 ) ) ;
#47528 = CARTESIAN_POINT ( 'NONE',  ( 1.613885712409999895, 1466.648931211529771, 234.8412340160980136 ) ) ;
#47530 = ORIENTED_EDGE ( 'NONE', *, *, #104492, .T. ) ;
#47529 = CARTESIAN_POINT ( 'NONE',  ( -41.66090858750000336, 1443.836096447190130, 135.6920785174980040 ) ) ;
#47531 = CARTESIAN_POINT ( 'NONE',  ( -0.7408122144259999819, 1450.887191310580192, 181.3422759365979857 ) ) ;
#47532 = CARTESIAN_POINT ( 'NONE',  ( -13.47003478659999942, 1382.321222797600058, 218.2872753327090152 ) ) ;
#47533 = CARTESIAN_POINT ( 'NONE',  ( 4.449471081249349425, 1508.551704408389924, 205.0837167827569942 ) ) ;
#47535 = ORIENTED_EDGE ( 'NONE', *, *, #63062, .F. ) ;
#47534 = CARTESIAN_POINT ( 'NONE',  ( -17.97699752310530030, 1415.938742849230039, 208.9722450247610084 ) ) ;
#47536 = CARTESIAN_POINT ( 'NONE',  ( 8.129483923442441196, 1461.711659188759995, 228.8737998629739820 ) ) ;
#47537 = ORIENTED_EDGE ( 'NONE', *, *, #32258, .T. ) ;
#47538 = VECTOR ( 'NONE', #71496, 1000.000000000000000 ) ;
#47539 = B_SPLINE_CURVE_WITH_KNOTS ( 'NONE', 3,
 ( #102053, #15821, #75773, #24778, #41619, #16925, #84156, #73158, #33748, #84703, #38981, #30030, #49478, #23697, #8003, #109384, #93643, #50025, #64784, #58425, #93108, #41055, #75234, #51127, #58977, #100948, #15286, #50576, #33203, #7456, #109923, #6900, #32661, #16378, #66838, #25336, #42168, #64224, #67393, #98347, #21620, #101491, #55825, #83602, #76321, #24243, #110471, #72612, #47410, #85251, #57882, #8551, #106743, #98894, #89945, #13220 ),
 .UNSPECIFIED., .F., .F.,
 ( 4, 2, 2, 2, 2, 2, 2, 2, 2, 1, 1, 2, 2, 2, 1, 1, 1, 2, 2, 2, 2, 1, 1, 2, 2, 2, 2, 1, 1, 1, 2, 2, 4 ),
 ( 0.000000000000000000, 0.1250000000005362932, 0.1875000000008112955, 0.2187500000009487966, 0.2500000000010862977, 0.3125000000013673507, 0.3437500000014971357, 0.3750000000016269763, 0.4375000000018683943, 0.4687500000019733659, 0.4843750000020397573, 0.4921875000020562441, 0.5000000000020726754, 0.5625000000021440627, 0.5937500000021798119, 0.6093750000022118973, 0.6171875000022302160, 0.6210937500022218893, 0.6250000000022134516, 0.6875000000020528024, 0.7187500000019703128, 0.7343750000019292345, 0.7421875000019292345, 0.7460937500019085844, 0.7500000000018879343, 0.8125000000017519319, 0.8437500000016620039, 0.8593750000016184831, 0.8671875000016213697, 0.8710937500016240342, 0.8730468750016000534, 0.8750000000015760726, 1.000000000000000000 ),
 .UNSPECIFIED. ) ;
#47540 = CARTESIAN_POINT ( 'NONE',  ( -11.49982667903889855, 1391.068238042669918, 213.8785252920860103 ) ) ;
#47541 = CARTESIAN_POINT ( 'NONE',  ( 36.22314289287339761, 1437.522903125109906, 136.5404214408590065 ) ) ;
#47542 = CARTESIAN_POINT ( 'NONE',  ( -8.751716459555160199, 1384.978504587089901, 220.6816886054729991 ) ) ;
#47543 = CARTESIAN_POINT ( 'NONE',  ( -11.60004869885203327, 1426.721831802138922, 134.4552142047555208 ) ) ;
#47544 = CARTESIAN_POINT ( 'NONE',  ( 1.191524307911311586, 1526.382868172863937, 179.0083900503167911 ) ) ;
#47545 = CARTESIAN_POINT ( 'NONE',  ( -10.07264118456989976, 1472.874378509069857, 207.3195388941770148 ) ) ;
#47546 = PLANE ( 'NONE',  #79012 ) ;
#47547 = CARTESIAN_POINT ( 'NONE',  ( 18.02089981653400130, 1424.325684919356036, 225.2034556834539956 ) ) ;
#47548 = CARTESIAN_POINT ( 'NONE',  ( 7.724188899110816742, 1461.608062285011329, 227.4089472320192442 ) ) ;
#47549 = CARTESIAN_POINT ( 'NONE',  ( -19.91421809350000061, 1485.651811164430228, 190.8591891487979808 ) ) ;
#47550 = CARTESIAN_POINT ( 'NONE',  ( 11.30129387169999866, 1432.307760315640053, 151.5220333367980174 ) ) ;
#47551 = DIRECTION ( 'NONE',  ( -0.0006352486380477548626, 0.9989931984823255950, -0.04485739454338198706 ) ) ;
#47552 = VERTEX_POINT ( 'NONE', #53424 ) ;
#47553 = ORIENTED_EDGE ( 'NONE', *, *, #74117, .T. ) ;
#47554 = CARTESIAN_POINT ( 'NONE',  ( -6.769661310147350619, 1509.032013615249980, 216.3879269483049939 ) ) ;
#47555 = CARTESIAN_POINT ( 'NONE',  ( -20.02799630220000182, 1485.574563381989947, 204.1280247810589970 ) ) ;
#47556 = CARTESIAN_POINT ( 'NONE',  ( -11.69984112520000075, 1435.115366081830189, 151.3290766764980049 ) ) ;
#47557 = CARTESIAN_POINT ( 'NONE',  ( -4.253586639292240192E-10, 1469.109899135820115, 251.5649450797509701 ) ) ;
#47558 = CARTESIAN_POINT ( 'NONE',  ( -20.50883971185030319, 1504.912087959059818, 190.4750152204429980 ) ) ;
#47559 = CARTESIAN_POINT ( 'NONE',  ( -15.08663666819999882, 1420.078856858149948, 212.5885907255689915 ) ) ;
#47560 = CARTESIAN_POINT ( 'NONE',  ( -109.3311711570000000, 1386.522315934440030, 311.1006615362589969 ) ) ;
#47561 = CARTESIAN_POINT ( 'NONE',  ( -0.9030881519919999878, 1483.390131495029891, 182.0736268275980194 ) ) ;
#47562 = CARTESIAN_POINT ( 'NONE',  ( -9.351945459727259546, 1366.519103298152004, 210.6218459616991936 ) ) ;
#47563 = DIRECTION ( 'NONE',  ( 8.727810504445229884E-47, -1.000000000000000000, 1.836970198721029688E-16 ) ) ;
#47564 = DIRECTION ( 'NONE',  ( 0.000000000000000000, 0.000000000000000000, 1.000000000000000000 ) ) ;
#47565 = CARTESIAN_POINT ( 'NONE',  ( -4.626591905484999323, 1517.096587378560116, 207.4170511287669854 ) ) ;
#47566 = CARTESIAN_POINT ( 'NONE',  ( -15.15764896601350031, 1414.025930248449868, 226.8247619795940011 ) ) ;
#47567 = CARTESIAN_POINT ( 'NONE',  ( 0.02955819112566610354, 1517.151704408390060, 193.2356110507530218 ) ) ;
#47568 = CARTESIAN_POINT ( 'NONE',  ( -14.03821757262499936, 1435.593435673239810, 149.8875993374950042 ) ) ;
#47569 = CARTESIAN_POINT ( 'NONE',  ( -8.021685169730000453, 1385.080864991280123, 218.7833935487189763 ) ) ;
#47570 = CARTESIAN_POINT ( 'NONE',  ( 6.639707775743658225, 1425.354353559006995, 226.3614492073465954 ) ) ;
#47571 = CARTESIAN_POINT ( 'NONE',  ( 7.312941311139250722, 1425.031074977940079, 212.6307961945279885 ) ) ;
#47572 = EDGE_LOOP ( 'NONE', ( #109287, #87019, #85028, #36189 ) ) ;
#47573 = CARTESIAN_POINT ( 'NONE',  ( 10.53938673299999884, 1414.594228655729921, 248.5638781382980085 ) ) ;
#47574 = CARTESIAN_POINT ( 'NONE',  ( -28.18850436489999822, 1508.134789598230100, 208.4601711067210204 ) ) ;
#47577 = CARTESIAN_POINT ( 'NONE',  ( -17.72824029589999739, 1410.893857127930232, 194.8229014749980195 ) ) ;
#47576 = VECTOR ( 'NONE', #96596, 999.9999999999998863 ) ;
#47575 = CARTESIAN_POINT ( 'NONE',  ( -2.540026744920000024, 1494.212893936630053, 181.3995399813979930 ) ) ;
#47578 = CARTESIAN_POINT ( 'NONE',  ( -6.865865202968861603, 1408.020609328411410, 270.1276013130552656 ) ) ;
#47579 = CARTESIAN_POINT ( 'NONE',  ( -25.95018329139999835, 1431.999486641019985, 231.7147496198979866 ) ) ;
#47580 = CARTESIAN_POINT ( 'NONE',  ( -29.24989835495881252, 1509.943647848841238, 204.9747545366232657 ) ) ;
#47581 = CARTESIAN_POINT ( 'NONE',  ( -11.21839826972749954, 1452.521305287280029, 150.0610815246930088 ) ) ;
#47582 = CARTESIAN_POINT ( 'NONE',  ( 27.85271936110000013, 1451.938833075630100, 135.3270518959979825 ) ) ;
#47583 = EDGE_LOOP ( 'NONE', ( #77455, #30697, #10364, #65454 ) ) ;
#47584 = CARTESIAN_POINT ( 'NONE',  ( -5.360341398479370412, 1422.242775764549833, 144.1555102201419913 ) ) ;
#47585 = CARTESIAN_POINT ( 'NONE',  ( 14.79465543570480079, 1514.566425925628209, 225.3731531939783679 ) ) ;
#47586 = B_SPLINE_CURVE_WITH_KNOTS ( 'NONE', 5,
 ( #2229, #44211, #71090, #94583, #20090, #1663, #52613, #36345, #104654, #95155, #35242, #27951 ),
 .UNSPECIFIED., .F., .F.,
 ( 6, 3, 3, 6 ),
 ( 0.000000000000000000, 0.3723444189143530481, 0.7907814729714509605, 1.000000000000000000 ),
 .UNSPECIFIED. ) ;
#47587 = CARTESIAN_POINT ( 'NONE',  ( -3.958338145845619049, 1515.551704408390151, 206.7917118413306241 ) ) ;
#47588 = ORIENTED_EDGE ( 'NONE', *, *, #28178, .F. ) ;
#47589 = ORIENTED_EDGE ( 'NONE', *, *, #102366, .F. ) ;
#47590 = FACE_OUTER_BOUND ( 'NONE', #54910, .T. ) ;
#47591 = CARTESIAN_POINT ( 'NONE',  ( -22.81607804052979915, 1409.709800168469883, 208.9487546288140152 ) ) ;
#47592 = ORIENTED_EDGE ( 'NONE', *, *, #3551, .T. ) ;
#47593 = CARTESIAN_POINT ( 'NONE',  ( 0.0002122017571388959824, 1432.353341358199941, 123.3907408769529894 ) ) ;
#47594 = CARTESIAN_POINT ( 'NONE',  ( -4.329448776040000446, 1515.064792882589927, 211.4519800877889963 ) ) ;
#47595 = CARTESIAN_POINT ( 'NONE',  ( -1.122745254329999831, 1479.775692482730165, 236.0081096927980013 ) ) ;
#47597 = CONICAL_SURFACE ( 'NONE', #1172, 18.60900368820000850, 0.6981317007980000211 ) ;
#47596 = CARTESIAN_POINT ( 'NONE',  ( -2.109056957580000002, 1421.166295015029846, 183.8085771866980167 ) ) ;
#47598 = ORIENTED_EDGE ( 'NONE', *, *, #62445, .F. ) ;
#47599 = CARTESIAN_POINT ( 'NONE',  ( 46.15241727715709885, 1441.855333579869921, 268.2045457479380275 ) ) ;
#47600 = CARTESIAN_POINT ( 'NONE',  ( -3.487587141067280072, 1509.038630944639863, 204.6345965622120104 ) ) ;
#47601 = FACE_OUTER_BOUND ( 'NONE', #77897, .T. ) ;
#47602 = CARTESIAN_POINT ( 'NONE',  ( -4.039897316195000698, 1516.787536375099990, 204.1233307748069876 ) ) ;
#47603 = ORIENTED_EDGE ( 'NONE', *, *, #33184, .F. ) ;
#47604 = CARTESIAN_POINT ( 'NONE',  ( -3.077634474923088170, 1432.970815717276764, 217.4382276955035991 ) ) ;
#47605 = ADVANCED_FACE ( 'NONE', ( #53995 ), #20886, .F. ) ;
#47606 = CARTESIAN_POINT ( 'NONE',  ( 13.12808455398275953, 1443.048474982209200, 187.4204472368715244 ) ) ;
#47607 = ORIENTED_EDGE ( 'NONE', *, *, #85697, .T. ) ;
#47608 = VERTEX_POINT ( 'NONE', #106025 ) ;
#47609 = CARTESIAN_POINT ( 'NONE',  ( 0.4260839224734093711, 1523.429859730329781, 173.4147438076381604 ) ) ;
#47610 = EDGE_CURVE ( 'NONE', #56666, #80182, #109769, .T. ) ;
#47611 = CARTESIAN_POINT ( 'NONE',  ( -2.181792844398890097, 1508.008799467449990, 220.9520129855879986 ) ) ;
#47612 = CARTESIAN_POINT ( 'NONE',  ( 13.31241404839999909, 1509.377940129630133, 234.8971984757980067 ) ) ;
#47613 = CARTESIAN_POINT ( 'NONE',  ( -14.42425707855669970, 1513.497693042470019, 193.9846077359950129 ) ) ;
#47614 = CARTESIAN_POINT ( 'NONE',  ( 23.84533589473599946, 1452.080362908450070, 136.9869410992479857 ) ) ;
#47615 = CARTESIAN_POINT ( 'NONE',  ( 11.77327517880000052, 1420.353493371139848, 199.1939701564990060 ) ) ;
#47616 = CARTESIAN_POINT ( 'NONE',  ( -3.523962699983150149, 1476.511731499819916, 220.0526012347959863 ) ) ;
#47617 = CARTESIAN_POINT ( 'NONE',  ( -108.3228733452354504, 1380.963783207329016, 298.1737543167551507 ) ) ;
#47618 = CARTESIAN_POINT ( 'NONE',  ( -10.97428490540760038, 1432.631986041290247, 151.7699425487470251 ) ) ;
#47619 = CARTESIAN_POINT ( 'NONE',  ( 0.03374749302241145110, 1409.321302690946368, 232.7832470492207051 ) ) ;
#47621 = CARTESIAN_POINT ( 'NONE',  ( -105.4624875116129914, 1391.255303400100047, 304.2078100440970161 ) ) ;
#47620 = CARTESIAN_POINT ( 'NONE',  ( -16.78589851036889868, 1414.704930897790064, 191.6301813728830155 ) ) ;
#47622 = CARTESIAN_POINT ( 'NONE',  ( 10.66776494291289978, 1424.286286161430098, 206.6302605353940010 ) ) ;
#47623 = CARTESIAN_POINT ( 'NONE',  ( -24.46809548295560077, 1509.129436896289917, 222.5284892987700118 ) ) ;
#47624 = CARTESIAN_POINT ( 'NONE',  ( 4.866999017969999564, 1428.784516533529995, 149.2390836726979728 ) ) ;
#47625 = ORIENTED_EDGE ( 'NONE', *, *, #58460, .T. ) ;
#47626 = CARTESIAN_POINT ( 'NONE',  ( 19.80583403109999807, 1436.359101875030092, 219.6133833564979909 ) ) ;
#47627 = DIRECTION ( 'NONE',  ( 1.755985294532469921E-16, -1.000000000000000000, 1.338183447452831989E-16 ) ) ;
#47628 = CARTESIAN_POINT ( 'NONE',  ( -93.64869092343039370, 1384.961098842790079, 309.7453634167209771 ) ) ;
#47629 = EDGE_CURVE ( 'NONE', #24499, #4978, #108382, .T. ) ;
#47630 = CARTESIAN_POINT ( 'NONE',  ( -9.963621752110000784, 1388.075463991820016, 201.3019539889990028 ) ) ;
#47631 = CARTESIAN_POINT ( 'NONE',  ( 9.591773081235949405, 1427.106394943569967, 210.3977398271019865 ) ) ;
#47633 = ORIENTED_EDGE ( 'NONE', *, *, #918, .T. ) ;
#47632 = CARTESIAN_POINT ( 'NONE',  ( -16.52130536630199842, 1419.782083806110222, 209.2901812870670142 ) ) ;
#47634 = CARTESIAN_POINT ( 'NONE',  ( 4.760952894889999065, 1429.902475422190037, 216.8416751273590251 ) ) ;
#47635 = B_SPLINE_CURVE_WITH_KNOTS ( 'NONE', 3,
 ( #12910, #97481, #96943, #20749 ),
 .UNSPECIFIED., .F., .F.,
 ( 4, 4 ),
 ( -105.4335682549999973, -86.05908296062720808 ),
 .UNSPECIFIED. ) ;
#47636 = CARTESIAN_POINT ( 'NONE',  ( 4.425709718559999041E-15, 1434.541746329560056, 150.4759714514979976 ) ) ;
#47637 = CARTESIAN_POINT ( 'NONE',  ( -16.98382738839999817, 1417.304179998030122, 207.5927328966690197 ) ) ;
#47638 = DIRECTION ( 'NONE',  ( -1.755985294532469921E-16, 1.000000000000000000, -1.338183447452831989E-16 ) ) ;
#47639 = CARTESIAN_POINT ( 'NONE',  ( 12.04783377103500008, 1512.799725290120023, 225.7711220359670108 ) ) ;
#47640 = LINE ( 'NONE', #74508, #58130 ) ;
#47641 = CARTESIAN_POINT ( 'NONE',  ( 30.79106905599203969, 1526.107880201381477, 217.1184136641281839 ) ) ;
#47642 = CARTESIAN_POINT ( 'NONE',  ( -110.0482597500069915, 1385.373319905469771, 296.9711118272649628 ) ) ;
#47643 = CARTESIAN_POINT ( 'NONE',  ( 16.84769428410000103, 1419.772082749829906, 226.8208912202979946 ) ) ;
#47644 = CARTESIAN_POINT ( 'NONE',  ( -32.52439779765793304, 1524.599984580802129, 201.1674557869507964 ) ) ;
#47645 = CARTESIAN_POINT ( 'NONE',  ( 2.871115274837119813, 1474.577308913379966, 220.1770025878000183 ) ) ;
#47646 = CARTESIAN_POINT ( 'NONE',  ( -19.26254113000000245, 1410.947276881129937, 222.4619606201979991 ) ) ;
#47647 = ADVANCED_FACE ( 'NONE', ( #10861 ), #55635, .T. ) ;
#47648 = CARTESIAN_POINT ( 'NONE',  ( -0.3327850108241715565, 1508.979300183436180, 238.8653632281604757 ) ) ;
#47649 = CARTESIAN_POINT ( 'NONE',  ( -0.9049687798709999953, 1422.347128627729944, 228.2716864167980191 ) ) ;
#47650 = VECTOR ( 'NONE', #84196, 1000.000000000000000 ) ;
#47651 = CARTESIAN_POINT ( 'NONE',  ( 0.4463512193210009693, 1458.283482050889916, 202.2977778409189966 ) ) ;
#47652 = DIRECTION ( 'NONE',  ( 0.000000000000000000, 1.000000000000000000, 0.000000000000000000 ) ) ;
#47653 = CARTESIAN_POINT ( 'NONE',  ( 0.7620301704480010319, 1515.588179473189939, 205.1071895219889996 ) ) ;
#47654 = CARTESIAN_POINT ( 'NONE',  ( 12.47025950862620114, 1427.078089640870076, 206.5892868991739988 ) ) ;
#47655 = CARTESIAN_POINT ( 'NONE',  ( -34.93120292363229851, 1435.717329652130047, 135.0377845007600115 ) ) ;
#47656 = EDGE_CURVE ( 'NONE', #83547, #97968, #31886, .T. ) ;
#47657 = CYLINDRICAL_SURFACE ( 'NONE', #92008, 1.999999999999999556 ) ;
#47658 = DIRECTION ( 'NONE',  ( 1.755985294532464991E-16, -1.000000000000000000, 1.338183447452830017E-16 ) ) ;
#47659 = CARTESIAN_POINT ( 'NONE',  ( -6.290310848379998987, 1409.132722882430016, 222.9509587267980066 ) ) ;
#47660 = DIRECTION ( 'NONE',  ( 0.02616798426500965835, 0.9993150019883683122, 0.02616798426500955774 ) ) ;
#47661 = CARTESIAN_POINT ( 'NONE',  ( 17.44374831407675686, 1524.130440953581001, 180.7216696960668116 ) ) ;
#47662 = CARTESIAN_POINT ( 'NONE',  ( -0.3238248822707833208, 1484.229047029399453, 198.4309250370245934 ) ) ;
#47663 = CARTESIAN_POINT ( 'NONE',  ( 12.40413062160000024, 1434.420063654429896, 149.0257888567980160 ) ) ;
#47664 = PLANE ( 'NONE',  #48325 ) ;
#47665 = CARTESIAN_POINT ( 'NONE',  ( 10.69787753770000016, 1442.513770420949868, 185.9957791832980263 ) ) ;
#47666 = ORIENTED_EDGE ( 'NONE', *, *, #87166, .T. ) ;
#47667 = CARTESIAN_POINT ( 'NONE',  ( -17.36692773919844512, 1525.425665131969481, 181.2365449020387871 ) ) ;
#47668 = CARTESIAN_POINT ( 'NONE',  ( 8.703395638689999103, 1478.819332251489868, 202.9087528450090190 ) ) ;
#47669 = CARTESIAN_POINT ( 'NONE',  ( -2.554115229335069959, 1409.002252056529869, 223.8943861301169989 ) ) ;
#47670 = CARTESIAN_POINT ( 'NONE',  ( -11.41602169729999972, 1491.175948940390072, 208.3010286188369946 ) ) ;
#47671 = CARTESIAN_POINT ( 'NONE',  ( -8.480431295684640602, 1436.263860089859918, 210.8443010970399882 ) ) ;
#47672 = CARTESIAN_POINT ( 'NONE',  ( 13.96283759872080132, 1508.693956055879880, 233.0808216126870036 ) ) ;
#47673 = CARTESIAN_POINT ( 'NONE',  ( 40.50375002456848250, 1425.156793582443925, 269.1155438645719187 ) ) ;
#47674 = CARTESIAN_POINT ( 'NONE',  ( 20.56164794690000264, 1453.151875979930082, 210.4536761478879896 ) ) ;
#47675 = CARTESIAN_POINT ( 'NONE',  ( -13.69967938769999982, 1380.327631092480033, 209.8719513141080029 ) ) ;
#47676 = CARTESIAN_POINT ( 'NONE',  ( -103.9238620277660061, 1384.593426725770087, 311.1343658853500642 ) ) ;
#47677 = CARTESIAN_POINT ( 'NONE',  ( -56.36773401075790701, 1385.044407682810061, 236.4819119073529805 ) ) ;
#47678 = CARTESIAN_POINT ( 'NONE',  ( -7.980167497413499511, 1424.314663469349398, 210.5240444418427899 ) ) ;
#47679 = CARTESIAN_POINT ( 'NONE',  ( -4.530454247226269437, 1508.551704408389924, 205.1921026621450324 ) ) ;
#47680 = CARTESIAN_POINT ( 'NONE',  ( -28.57599588808039925, 1509.162863321990017, 208.7718535704119915 ) ) ;
#47681 = AXIS2_PLACEMENT_3D ( 'NONE', #50468, #107601, #65064 ) ;
#47682 = CARTESIAN_POINT ( 'NONE',  ( 2.165176160181045528, 1526.186458717538926, 177.9542909903756254 ) ) ;
#47683 = CARTESIAN_POINT ( 'NONE',  ( -16.37947571190000318, 1409.734195298129862, 225.9725054800979933 ) ) ;
#47685 = ORIENTED_EDGE ( 'NONE', *, *, #102194, .F. ) ;
#47684 = CARTESIAN_POINT ( 'NONE',  ( 0.5111074947771929722, 1410.993655183119927, 185.0427835985659897 ) ) ;
#47686 = CARTESIAN_POINT ( 'NONE',  ( -11.82020261140000095, 1508.077988756929926, 183.1980805049979892 ) ) ;
#47687 = CARTESIAN_POINT ( 'NONE',  ( 9.858506243812300340, 1469.740707437229958, 211.1772101207760102 ) ) ;
#47688 = CARTESIAN_POINT ( 'NONE',  ( 12.44780704128189974, 1501.268281525590055, 211.7240718234590133 ) ) ;
#47689 = CARTESIAN_POINT ( 'NONE',  ( -109.1343026320000007, 1384.783638055820120, 311.2626717992590102 ) ) ;
#47690 = CARTESIAN_POINT ( 'NONE',  ( -11.36018332909999984, 1414.996444518330009, 195.9645814724980255 ) ) ;
#47691 = CARTESIAN_POINT ( 'NONE',  ( 0.001377745780720000032, 1465.018687260529987, 237.3906760667979938 ) ) ;
#47692 = CARTESIAN_POINT ( 'NONE',  ( 18.88261216240000095, 1409.572455740129953, 220.0130051960980211 ) ) ;
#47693 = CARTESIAN_POINT ( 'NONE',  ( 0.5697990016583959205, 1450.893162567740092, 181.2939912002310052 ) ) ;
#47694 = CARTESIAN_POINT ( 'NONE',  ( -13.10665367552279825, 1467.935415218449862, 191.9179395855259997 ) ) ;
#47695 = CARTESIAN_POINT ( 'NONE',  ( -18.11291060900000005, 1424.770096122030054, 227.5276574296979959 ) ) ;
#47697 = CARTESIAN_POINT ( 'NONE',  ( -13.83438311809999810, 1379.888128081619925, 206.0089139935990090 ) ) ;
#47696 = CARTESIAN_POINT ( 'NONE',  ( -3.029841966249135599, 1511.989348024461833, 201.2192106154559781 ) ) ;
#47698 = CARTESIAN_POINT ( 'NONE',  ( 26.62565391809450333, 1469.324738006449934, 208.6920304769689949 ) ) ;
#47699 = CARTESIAN_POINT ( 'NONE',  ( -102.6162175075999414, 1366.350733876289723, 293.4380634648590558 ) ) ;
#47700 = DIRECTION ( 'NONE',  ( -0.9786619618251657382, 0.000000000000000000, 0.2054769195713184449 ) ) ;
#47701 = CARTESIAN_POINT ( 'NONE',  ( -0.9237819473580000107, 1416.172288158230231, 233.4037497922979867 ) ) ;
#47702 = CARTESIAN_POINT ( 'NONE',  ( 9.231361398829999843, 1366.659448741839924, 210.6218459616991936 ) ) ;
#47703 = CARTESIAN_POINT ( 'NONE',  ( -3.461047329755000401, 1516.858765657450249, 205.6745815831370123 ) ) ;
#47704 = DIRECTION ( 'NONE',  ( -0.9272785430170710219, -0.03238144682225380100, -0.3729690946470439750 ) ) ;
#47705 = ORIENTED_EDGE ( 'NONE', *, *, #87675, .F. ) ;
#47706 = CARTESIAN_POINT ( 'NONE',  ( -3.500000000000000000, 1424.163060387329779, 172.2701767054979882 ) ) ;
#47707 = CARTESIAN_POINT ( 'NONE',  ( 14.00898853540000033, 1416.833018152729892, 196.3916011246980133 ) ) ;
#47709 = VERTEX_POINT ( 'NONE', #95958 ) ;
#47708 = CARTESIAN_POINT ( 'NONE',  ( -67.09039466822581232, 1379.744314274860017, 278.2050095193470156 ) ) ;
#47710 = ORIENTED_EDGE ( 'NONE', *, *, #66712, .F. ) ;
#47711 = CARTESIAN_POINT ( 'NONE',  ( 28.13477516149999857, 1508.112005763430034, 210.1092937961579992 ) ) ;
#47712 = ORIENTED_EDGE ( 'NONE', *, *, #67067, .T. ) ;
#47713 = CARTESIAN_POINT ( 'NONE',  ( 1.478581789801439950, 1485.417738077120021, 220.8958599741850151 ) ) ;
#47714 = CARTESIAN_POINT ( 'NONE',  ( -17.76091714769999896, 1410.905089322729964, 194.9382696558980115 ) ) ;
#47716 = CARTESIAN_POINT ( 'NONE',  ( 15.69540887480520119, 1410.567746757359828, 191.5434892055160105 ) ) ;
#47715 = CARTESIAN_POINT ( 'NONE',  ( -11.69554736699999786, 1426.722884897929816, 141.2004217243980122 ) ) ;
#47717 = CARTESIAN_POINT ( 'NONE',  ( 3.269984781304999810, 1516.999105586269934, 210.8242519552970009 ) ) ;
#47718 = CARTESIAN_POINT ( 'NONE',  ( -24.62049690961300286, 1452.037610211400079, 136.1636793085519912 ) ) ;
#47719 = CARTESIAN_POINT ( 'NONE',  ( -11.63666214179999869, 1425.864857562230100, 144.1663263557980201 ) ) ;
#47720 = CARTESIAN_POINT ( 'NONE',  ( 9.055707583609999389, 1409.396424226330055, 229.6055981440979963 ) ) ;
#47721 = CARTESIAN_POINT ( 'NONE',  ( 8.403712088333849195, 1482.711991784579823, 217.0153515255709920 ) ) ;
#47722 = DIRECTION ( 'NONE',  ( 1.000000000000000000, 0.000000000000000000, 0.000000000000000000 ) ) ;
#47723 = CARTESIAN_POINT ( 'NONE',  ( 41.61795676512019782, 1442.846609226920009, 134.0999999981039821 ) ) ;
#47724 = CARTESIAN_POINT ( 'NONE',  ( -39.87872480270220166, 1441.370340969270046, 136.8657547114230226 ) ) ;
#47725 = EDGE_LOOP ( 'NONE', ( #11628, #50219, #25052 ) ) ;
#47726 = CARTESIAN_POINT ( 'NONE',  ( 20.10528729609999843, 1430.878053336090034, 215.1856554784289983 ) ) ;
#47727 = CARTESIAN_POINT ( 'NONE',  ( -3.696289592874629548, 1429.417634134486434, 201.6803503126470218 ) ) ;
#47728 = EDGE_LOOP ( 'NONE', ( #374, #25362, #3016 ) ) ;
#47729 = VERTEX_POINT ( 'NONE', #12506 ) ;
#47730 = CARTESIAN_POINT ( 'NONE',  ( -7.248946814685000462, 1514.005261957190214, 217.0303516513569946 ) ) ;
#47731 = DIRECTION ( 'NONE',  ( 0.000000000000000000, 0.000000000000000000, -1.000000000000000000 ) ) ;
#47732 = CARTESIAN_POINT ( 'NONE',  ( 12.49505606288779980, 1500.014223150440102, 206.9771888552629662 ) ) ;
#47733 = CARTESIAN_POINT ( 'NONE',  ( -16.86744945587559741, 1508.551704408389924, 210.3912200788219877 ) ) ;
#47734 = CIRCLE ( 'NONE', #54861, 2.000051271460090430 ) ;
#47735 = CARTESIAN_POINT ( 'NONE',  ( -40.26396455803409680, 1444.186530478750001, 137.1012301494149881 ) ) ;
#47736 = CARTESIAN_POINT ( 'NONE',  ( -63.85514023855817811, 1379.736301226116211, 269.8882248764738847 ) ) ;
#47737 = DIRECTION ( 'NONE',  ( 0.6480245870892008542, 0.000000000000000000, -0.7616194158028475325 ) ) ;
#47738 = CARTESIAN_POINT ( 'NONE',  ( -1.517666159849999863, 1497.689500997429832, 231.6008634864979854 ) ) ;
#47739 = CARTESIAN_POINT ( 'NONE',  ( 11.22085809280000035, 1414.913060387329779, 197.6243702818979955 ) ) ;
#47740 = CARTESIAN_POINT ( 'NONE',  ( -73.46068911739270391, 1384.758501831970079, 272.7067926322189919 ) ) ;
#47741 = VERTEX_POINT ( 'NONE', #27653 ) ;
#47742 = CARTESIAN_POINT ( 'NONE',  ( 9.387051760214630391, 1462.123984385330004, 206.5521735341949920 ) ) ;
#47743 = CARTESIAN_POINT ( 'NONE',  ( 2.868112131164999745, 1516.855632454399938, 208.3641823986619954 ) ) ;
#47744 = ORIENTED_EDGE ( 'NONE', *, *, #87105, .T. ) ;
#47745 = CARTESIAN_POINT ( 'NONE',  ( 34.07917771385839956, 1440.913060387330006, 259.4382560880169422 ) ) ;
#47746 = CARTESIAN_POINT ( 'NONE',  ( 18.15454648420000083, 1457.025425127630115, 227.8110394751979868 ) ) ;
#47747 = ORIENTED_EDGE ( 'NONE', *, *, #56834, .F. ) ;
#47748 = CARTESIAN_POINT ( 'NONE',  ( -0.3067201157339999873, 1452.334527121330211, 183.2866423852979949 ) ) ;
#47749 = CARTESIAN_POINT ( 'NONE',  ( -16.22975407500000244, 1409.646465899229952, 192.1195335419979813 ) ) ;
#47750 = CARTESIAN_POINT ( 'NONE',  ( -22.98095477630000261, 1420.941325299229902, 212.0408358845679970 ) ) ;
#47751 = DIRECTION ( 'NONE',  ( 0.000000000000000000, 1.000000000000000000, -6.123233995736769734E-17 ) ) ;
#47752 = CARTESIAN_POINT ( 'NONE',  ( 22.17089962140870085, 1410.141205781899998, 206.2581381202189732 ) ) ;
#47753 = CARTESIAN_POINT ( 'NONE',  ( -5.762402200599920477, 1511.083508941950186, 201.4380933754170258 ) ) ;
#47754 = CARTESIAN_POINT ( 'NONE',  ( -2.858129514550000305, 1507.751283221830136, 180.8639750916980233 ) ) ;
#47755 = CARTESIAN_POINT ( 'NONE',  ( -5.750872970432570952, 1510.549724825256135, 201.5793989082007727 ) ) ;
#47756 = CYLINDRICAL_SURFACE ( 'NONE', #109008, 0.4999999999999449329 ) ;
#47758 = CARTESIAN_POINT ( 'NONE',  ( -23.32556912959070061, 1416.023918999339912, 210.9192148309080039 ) ) ;
#47757 = CARTESIAN_POINT ( 'NONE',  ( 14.88687292590000055, 1460.215022219430011, 231.2459449793980184 ) ) ;
#47759 = CIRCLE ( 'NONE', #40631, 2.458500000000000352 ) ;
#47760 = CARTESIAN_POINT ( 'NONE',  ( -1.709384611084999950, 1517.224900789629828, 216.4615953054470197 ) ) ;
#47761 = CARTESIAN_POINT ( 'NONE',  ( -33.28034951413922471, 1512.187213306747481, 217.4407153818824838 ) ) ;
#47762 = CARTESIAN_POINT ( 'NONE',  ( -0.1434969078204259840, 1507.634396196580155, 180.8101134974600086 ) ) ;
#47763 = EDGE_CURVE ( 'NONE', #59940, #5947, #93681, .T. ) ;
#47764 = CARTESIAN_POINT ( 'NONE',  ( 2.346054097678328176, 1516.530616268062886, 216.8307811113319303 ) ) ;
#47765 = CARTESIAN_POINT ( 'NONE',  ( -2.285487619494999567, 1517.001127920769704, 213.1661676502270097 ) ) ;
#47766 = CARTESIAN_POINT ( 'NONE',  ( 18.64460737039999927, 1509.564144423530252, 186.5337401517980140 ) ) ;
#47767 =( BOUNDED_CURVE ( )  B_SPLINE_CURVE ( 3, ( #54536, #52318, #44458, #78602 ),
 .UNSPECIFIED., .F., .F. ) 
 B_SPLINE_CURVE_WITH_KNOTS ( ( 4, 4 ),
 ( 2.436781329611989122, 3.141592653589793116 ),
 .UNSPECIFIED. ) 
 CURVE ( )  GEOMETRIC_REPRESENTATION_ITEM ( )  RATIONAL_B_SPLINE_CURVE ( ( 1.000000000000000000, 0.9590300661663093695, 0.9590300661663093695, 1.000000000000000000 ) ) 
 REPRESENTATION_ITEM ( '' )  );
#47768 = CARTESIAN_POINT ( 'NONE',  ( -3.837713176184200048, 1483.349439374189842, 199.1769404390510090 ) ) ;
#47770 = VERTEX_POINT ( 'NONE', #97616 ) ;
#47769 = CARTESIAN_POINT ( 'NONE',  ( -10.93667282414601694, 1508.551702216402191, 207.6442590326176401 ) ) ;
#47771 = CARTESIAN_POINT ( 'NONE',  ( 4.500000000000000000, 1448.210448412289907, 170.6974824052979898 ) ) ;
#47772 = CARTESIAN_POINT ( 'NONE',  ( 6.216948005759999719E-09, 1459.726867864730139, 213.1264974772779794 ) ) ;
#47773 = ADVANCED_FACE ( 'NONE', ( #107665 ), #23086, .F. ) ;
#47774 = CARTESIAN_POINT ( 'NONE',  ( -11.57120699989999757, 1431.932395937310048, 151.1858022038979925 ) ) ;
#47775 = CARTESIAN_POINT ( 'NONE',  ( 19.19771385826059884, 1456.936707467760243, 224.8620913037029823 ) ) ;
#47776 = CARTESIAN_POINT ( 'NONE',  ( -7.618671585723859607, 1439.752128060139967, 204.7697547506639921 ) ) ;
#47777 = CARTESIAN_POINT ( 'NONE',  ( 1.547463896846929865, 1414.913060387349788, 192.3096116128920130 ) ) ;
#47778 = CARTESIAN_POINT ( 'NONE',  ( 8.135441375949998388, 1421.256651981180084, 196.0379973919989709 ) ) ;
#47779 = CARTESIAN_POINT ( 'NONE',  ( 12.70914363729999863, 1445.041869922740034, 186.8564040585980024 ) ) ;
#47781 = CARTESIAN_POINT ( 'NONE',  ( -18.26050052379999755, 1504.444625823090064, 209.3988868026209786 ) ) ;
#47780 = CARTESIAN_POINT ( 'NONE',  ( -23.50891559320000113, 1470.079355157530017, 219.2631860520979785 ) ) ;
#47783 = CARTESIAN_POINT ( 'NONE',  ( -0.08461443291850000159, 1416.823634022829992, 191.0185729562979873 ) ) ;
#47782 = CIRCLE ( 'NONE', #26256, 2.000000000000003553 ) ;
#47784 = EDGE_LOOP ( 'NONE', ( #37925, #59686, #85798, #35595 ) ) ;
#47785 = CARTESIAN_POINT ( 'NONE',  ( 5.773668814845000163, 1516.734985836460055, 205.0832084693769843 ) ) ;
#47786 = CARTESIAN_POINT ( 'NONE',  ( 7.084494119980000448, 1406.178315946529892, 268.4624913171979870 ) ) ;
#47787 = CARTESIAN_POINT ( 'NONE',  ( 0.7050289746089989373, 1515.139588934790027, 213.4493361341789921 ) ) ;
#47788 = DIRECTION ( 'NONE',  ( 0.9417419115949053898, 0.3363363969979660806, 0.000000000000000000 ) ) ;
#47789 = CARTESIAN_POINT ( 'NONE',  ( 22.93959776030420272, 1432.116225619942270, 216.2250907020126363 ) ) ;
#47790 = B_SPLINE_CURVE_WITH_KNOTS ( 'NONE', 3,
 ( #31578, #4725, #38869, #30478, #68521, #50601, #76911, #43854, #85280, #8030, #60678, #8579, #34343, #59012, #43311, #94236, #69079, #7485, #9148 ),
 .UNSPECIFIED., .F., .F.,
 ( 4, 2, 2, 2, 1, 1, 1, 2, 2, 2, 4 ),
 ( 0.000000000000000000, 0.2500000000006191159, 0.3750000000009287016, 0.4375000000010938472, 0.4687500000012264634, 0.4843750000013014589, 0.4921875000013305468, 0.4960937500014176993, 0.5000000000015047963, 0.7500000000007523981, 1.000000000000000000 ),
 .UNSPECIFIED. ) ;
#47791 = CARTESIAN_POINT ( 'NONE',  ( -0.4918821362568480682, 1463.495325596601333, 199.3433850722970817 ) ) ;
#47792 = FACE_OUTER_BOUND ( 'NONE', #61467, .T. ) ;
#47793 = CARTESIAN_POINT ( 'NONE',  ( -6.570337678066239917, 1439.978317356713887, 203.3223113697309259 ) ) ;
#47794 = CARTESIAN_POINT ( 'NONE',  ( -2.323033500480000235, 1449.800808693189992, 155.6080925164979760 ) ) ;
#47795 = CARTESIAN_POINT ( 'NONE',  ( -12.53380136120000010, 1445.052233027470038, 185.6742673453979933 ) ) ;
#47796 = CARTESIAN_POINT ( 'NONE',  ( 2.500094834180730086, 1448.919094884260176, 155.0643240262459983 ) ) ;
#47797 = CARTESIAN_POINT ( 'NONE',  ( -2.367088349510000356, 1507.435255637589989, 221.3405631526989907 ) ) ;
#47798 = CARTESIAN_POINT ( 'NONE',  ( -10.26603356420000068, 1498.779766624589911, 214.4369877271390123 ) ) ;
#47799 = CARTESIAN_POINT ( 'NONE',  ( 5.329070518200000398E-15, 1416.825952160429779, 255.3819207742980097 ) ) ;
#47800 = TOROIDAL_SURFACE ( 'NONE', #55019, 2.000000000000000000, 1.000000000000000000 ) ;
#47801 = LINE ( 'NONE', #23683, #41246 ) ;
#47802 = CARTESIAN_POINT ( 'NONE',  ( 3.655447866509999866, 1441.516748634489886, 170.5484046385980150 ) ) ;
#47803 = CARTESIAN_POINT ( 'NONE',  ( -3.386669734929999898, 1474.956089833430042, 269.6463548828979810 ) ) ;
#47804 = CARTESIAN_POINT ( 'NONE',  ( 13.77266209894789917, 1517.051704408389924, 201.2043266506040027 ) ) ;
#47805 = CARTESIAN_POINT ( 'NONE',  ( -8.759952407214090186, 1423.587288072539877, 144.1551656127980152 ) ) ;
#47806 = CARTESIAN_POINT ( 'NONE',  ( 2.038646110889675178, 1525.960063244516959, 241.1857569150893994 ) ) ;
#47807 = CARTESIAN_POINT ( 'NONE',  ( -24.34705444099909855, 1384.848287400760228, 223.2598029039740197 ) ) ;
#47808 = CARTESIAN_POINT ( 'NONE',  ( -9.234134023826198856, 1461.205490114660051, 206.1827678865119822 ) ) ;
#47809 = AXIS2_PLACEMENT_3D ( 'NONE', #42436, #92286, #15009 ) ;
#47810 = CARTESIAN_POINT ( 'NONE',  ( -17.40764085468179800, 1414.996442620800053, 207.5654756526599840 ) ) ;
#47811 = CARTESIAN_POINT ( 'NONE',  ( 12.26176529699089990, 1491.759805890980033, 208.0003969321799957 ) ) ;
#47812 = DIRECTION ( 'NONE',  ( 0.000000000000000000, 0.000000000000000000, -1.000000000000000000 ) ) ;
#47813 = CARTESIAN_POINT ( 'NONE',  ( 8.384950263960369909, 1511.400233449589450, 204.5379475627291868 ) ) ;
#47814 = CARTESIAN_POINT ( 'NONE',  ( -22.40412009319999953, 1411.055624679330094, 203.1355812455580008 ) ) ;
#47815 = CARTESIAN_POINT ( 'NONE',  ( -15.49572516138399969, 1421.633966799186055, 227.2929845234520201 ) ) ;
#47816 = CARTESIAN_POINT ( 'NONE',  ( -45.08261358189999868, 1435.036897264239997, 268.9899376266980653 ) ) ;
#47817 = EDGE_LOOP ( 'NONE', ( #34766, #6119, #110183, #10953, #32440, #75869, #108722 ) ) ;
#47818 = CARTESIAN_POINT ( 'NONE',  ( 31.33756689035257992, 1523.580203803270933, 221.9021554055875356 ) ) ;
#47819 = CARTESIAN_POINT ( 'NONE',  ( 13.40958089240390017, 1414.996442620800053, 197.9133050684260127 ) ) ;
#47820 = CARTESIAN_POINT ( 'NONE',  ( 18.28862923867550094, 1430.119187293129926, 201.0315415175020064 ) ) ;
#47822 = CARTESIAN_POINT ( 'NONE',  ( -12.15948100306500024, 1512.592133792520144, 192.4950717916669873 ) ) ;
#47821 = CYLINDRICAL_SURFACE ( 'NONE', #8543, 1.000000000000000888 ) ;
#47823 = CARTESIAN_POINT ( 'NONE',  ( -16.09630756760823189, 1409.475146607743454, 225.1332669131820410 ) ) ;
#47824 = CARTESIAN_POINT ( 'NONE',  ( -7.099928628730000746, 1453.632733172990129, 202.8366510152990259 ) ) ;
#47825 = B_SPLINE_CURVE_WITH_KNOTS ( 'NONE', 3,
 ( #50113, #109461, #7540, #75854, #49013, #110004, #83149, #23224, #83691, #33281 ),
 .UNSPECIFIED., .F., .F.,
 ( 4, 2, 2, 2, 4 ),
 ( 0.000000000000000000, 0.2500000000000000000, 0.5000000000000000000, 0.7500000000000000000, 1.000000000000000000 ),
 .UNSPECIFIED. ) ;
#47826 = CARTESIAN_POINT ( 'NONE',  ( -7.718763544034999313, 1516.905946377369901, 202.1794916586869988 ) ) ;
#47827 = CARTESIAN_POINT ( 'NONE',  ( 7.531671725839999887, 1426.336758191899889, 212.2880588734690264 ) ) ;
#47829 = CARTESIAN_POINT ( 'NONE',  ( 24.04367183769999983, 1494.655699983489967, 207.1743773500889745 ) ) ;
#47828 = AXIS2_PLACEMENT_3D ( 'NONE', #38533, #98440, #80553 ) ;
#47830 = CARTESIAN_POINT ( 'NONE',  ( 15.29601658473500159, 1513.169116394660023, 194.9970914992669861 ) ) ;
#47831 = FACE_BOUND ( 'NONE', #27403, .T. ) ;
#47832 = CARTESIAN_POINT ( 'NONE',  ( -75.41334994439999662, 1376.365900248229991, 294.0916975056589990 ) ) ;
#47833 = CARTESIAN_POINT ( 'NONE',  ( 8.312847552073090895, 1366.156914216811174, 207.6218459616988241 ) ) ;
#47835 = ORIENTED_EDGE ( 'NONE', *, *, #39862, .F. ) ;
#47834 = CARTESIAN_POINT ( 'NONE',  ( -14.07256126937990004, 1379.709109777840013, 211.5290051616560163 ) ) ;
#47836 = ORIENTED_EDGE ( 'NONE', *, *, #101568, .T. ) ;
#47837 = CARTESIAN_POINT ( 'NONE',  ( -6.220302174429999553, 1397.477102020930033, 197.7753768578980100 ) ) ;
#47838 = CARTESIAN_POINT ( 'NONE',  ( -19.36881300869999833, 1410.511871308530090, 222.2034276849980188 ) ) ;
#47839 = CARTESIAN_POINT ( 'NONE',  ( -1.316362887759999989, 1415.041103189330215, 226.7113481479980237 ) ) ;
#47840 = CARTESIAN_POINT ( 'NONE',  ( -13.35314812681837360, 1444.506189530448182, 169.3733437756958438 ) ) ;
#47841 = CARTESIAN_POINT ( 'NONE',  ( -26.60753868740000172, 1509.169818042129918, 201.4350758664580212 ) ) ;
#47842 = CARTESIAN_POINT ( 'NONE',  ( 2.329906352153470195, 1515.372228416580128, 204.8601837675520017 ) ) ;
#47844 = CARTESIAN_POINT ( 'NONE',  ( 17.77226856539999744, 1416.272325472730017, 225.3684990499980074 ) ) ;
#47843 = CARTESIAN_POINT ( 'NONE',  ( -104.1991585039999961, 1389.999238680429926, 304.1793527667589956 ) ) ;
#47845 = CARTESIAN_POINT ( 'NONE',  ( -32.22536377336285085, 1523.621879633029039, 201.4085774011533090 ) ) ;
#47846 = CARTESIAN_POINT ( 'NONE',  ( -3.783954225830480134, 1462.812684261019967, 200.1151939703100027 ) ) ;
#47847 = CARTESIAN_POINT ( 'NONE',  ( -40.94281863450720493, 1445.635000978330027, 136.6596512823030025 ) ) ;
#47848 = CARTESIAN_POINT ( 'NONE',  ( 8.618023458351569133, 1396.214008466279893, 202.1935922150420026 ) ) ;
#47849 = CARTESIAN_POINT ( 'NONE',  ( 0.5679639878839999323, 1416.568813547830132, 190.4860628299979908 ) ) ;
#47850 = CARTESIAN_POINT ( 'NONE',  ( 11.84752247700000005, 1430.969153207809995, 150.2425949294979830 ) ) ;
#47851 = CARTESIAN_POINT ( 'NONE',  ( 8.788316489185000080, 1511.741868877540128, 202.8695794779170001 ) ) ;
#47852 = ORIENTED_EDGE ( 'NONE', *, *, #32415, .F. ) ;
#47853 = CARTESIAN_POINT ( 'NONE',  ( -16.77192111137889441, 1526.333389947941896, 183.3307103475322322 ) ) ;
#47854 = CARTESIAN_POINT ( 'NONE',  ( 2.373304165714522629, 1449.620559872589865, 182.2130135973664551 ) ) ;
#47855 = ORIENTED_EDGE ( 'NONE', *, *, #96727, .F. ) ;
#47856 = ORIENTED_EDGE ( 'NONE', *, *, #39576, .T. ) ;
#47857 = CARTESIAN_POINT ( 'NONE',  ( 11.86874272849999912, 1492.043035549590059, 209.5970695671510100 ) ) ;
#47858 = CARTESIAN_POINT ( 'NONE',  ( -14.60046712539999980, 1460.133194728129865, 230.9282956282980024 ) ) ;
#47859 = CIRCLE ( 'NONE', #89001, 0.4999999999999449329 ) ;
#47860 = CARTESIAN_POINT ( 'NONE',  ( -13.58416853039999950, 1434.822844256989811, 196.0567512594979860 ) ) ;
#47861 = DIRECTION ( 'NONE',  ( -1.755985294532469921E-16, 1.000000000000000000, -1.338183447452831989E-16 ) ) ;
#47862 = CARTESIAN_POINT ( 'NONE',  ( -5.778372601744999670, 1516.932669162149978, 216.0673360190369863 ) ) ;
#47863 = CARTESIAN_POINT ( 'NONE',  ( 3.331783404088237699, 1517.051704408389924, 197.4348858789911674 ) ) ;
#47864 = ORIENTED_EDGE ( 'NONE', *, *, #99437, .T. ) ;
#47865 = DIRECTION ( 'NONE',  ( -0.9995238204287079098, -0.03085664264949923227, 3.329727431759169316E-08 ) ) ;
#47866 = CARTESIAN_POINT ( 'NONE',  ( 0.05018163627710000435, 1508.979242228630028, 179.3226982217979923 ) ) ;
#47867 = CARTESIAN_POINT ( 'NONE',  ( -46.72344042710000878, 1377.583786706710043, 230.7048910953589882 ) ) ;
#47868 = CARTESIAN_POINT ( 'NONE',  ( 5.335637657409999512, 1416.823418193129783, 226.4969446031979885 ) ) ;
#47869 = CARTESIAN_POINT ( 'NONE',  ( -7.723480117524999855, 1517.086065052259983, 205.0863097070169943 ) ) ;
#47870 = ORIENTED_EDGE ( 'NONE', *, *, #70919, .T. ) ;
#47871 = CARTESIAN_POINT ( 'NONE',  ( 5.006259848694999626, 1516.939723362869927, 209.1089481433290018 ) ) ;
#47872 = CARTESIAN_POINT ( 'NONE',  ( -20.49660237009999975, 1509.524916194930029, 230.0429231069980176 ) ) ;
#47873 = CARTESIAN_POINT ( 'NONE',  ( -16.23190381645581937, 1412.775336537543126, 269.3700702654938937 ) ) ;
#47874 = CARTESIAN_POINT ( 'NONE',  ( 6.772137591825000413, 1511.702066573639968, 216.3336057811770274 ) ) ;
#47876 = ORIENTED_EDGE ( 'NONE', *, *, #93250, .T. ) ;
#47875 = CARTESIAN_POINT ( 'NONE',  ( 2.493590731671294414, 1524.152444737676660, 175.5218342203271504 ) ) ;
#47877 = CARTESIAN_POINT ( 'NONE',  ( 2.500000000000000000, 1428.988705744230174, 157.0781314899979861 ) ) ;
#47878 = CARTESIAN_POINT ( 'NONE',  ( -28.50339170433599989, 1440.913060387269979, 233.1297467994120041 ) ) ;
#47880 = CARTESIAN_POINT ( 'NONE',  ( -89.71137825399999599, 1383.770488589559818, 308.5740051020589476 ) ) ;
#47879 = CIRCLE ( 'NONE', #71164, 0.9999999999999976685 ) ;
#47881 = CARTESIAN_POINT ( 'NONE',  ( 21.04904418909999819, 1494.916427559390058, 209.1218459616989946 ) ) ;
#47882 = CARTESIAN_POINT ( 'NONE',  ( 5.349258415000000433, 1408.472118978329945, 270.3881948815980536 ) ) ;
#47883 = CARTESIAN_POINT ( 'NONE',  ( 1.715361092244999996, 1516.743010792419909, 212.5670474586069929 ) ) ;
#47884 = CARTESIAN_POINT ( 'NONE',  ( -47.55875411400000274, 1379.740588162619815, 235.3895649973590025 ) ) ;
#47885 = VECTOR ( 'NONE', #70181, 1000.000000000000000 ) ;
#47886 = CARTESIAN_POINT ( 'NONE',  ( 22.98387363149999985, 1409.741890572629927, 208.9143205900259943 ) ) ;
#47887 = CARTESIAN_POINT ( 'NONE',  ( 0.04641543544835657897, 1517.051704408389924, 187.8934844801420923 ) ) ;
#47888 = CARTESIAN_POINT ( 'NONE',  ( 11.99250861867660056, 1492.789266563229830, 212.0938347205880063 ) ) ;
#47889 = STYLED_ITEM ( 'NONE', ( #59438 ), #46279 ) ;
#47890 = CARTESIAN_POINT ( 'NONE',  ( -7.708862459925570398, 1516.527839230000154, 211.3267386195620077 ) ) ;
#47891 = CARTESIAN_POINT ( 'NONE',  ( -7.321169269124999879, 1516.531533746980131, 210.8305669548069829 ) ) ;
#47892 = CARTESIAN_POINT ( 'NONE',  ( 25.10807187043309341, 1509.789853576705582, 224.8278757916732218 ) ) ;
#47893 = FACE_OUTER_BOUND ( 'NONE', #35784, .T. ) ;
#47894 = CARTESIAN_POINT ( 'NONE',  ( -106.4193208199999958, 1384.816937872099970, 311.3271286962590239 ) ) ;
#47896 = VERTEX_POINT ( 'NONE', #6841 ) ;
#47895 = CARTESIAN_POINT ( 'NONE',  ( -31.92467753469999892, 1384.972130813700005, 206.3032401593790155 ) ) ;
#47897 = CARTESIAN_POINT ( 'NONE',  ( -54.15112835251079559, 1385.097464586390061, 270.1434570728429776 ) ) ;
#47898 = CARTESIAN_POINT ( 'NONE',  ( 30.61443310214306024, 1523.462669333491704, 196.4193608261350334 ) ) ;
#47899 = CARTESIAN_POINT ( 'NONE',  ( 0.3041635068690000665, 1415.771586802929960, 233.4346734808979988 ) ) ;
#47900 =( BOUNDED_CURVE ( )  B_SPLINE_CURVE ( 3, ( #100174, #23459, #56534, #13945 ),
 .UNSPECIFIED., .F., .T. ) 
 B_SPLINE_CURVE_WITH_KNOTS ( ( 4, 4 ),
 ( 5.864774099209800085, 6.175064727860119618 ),
 .UNSPECIFIED. ) 
 CURVE ( )  GEOMETRIC_REPRESENTATION_ITEM ( )  RATIONAL_B_SPLINE_CURVE ( ( 1.000000000000000000, 0.9919927244685476930, 0.9919927244685476930, 1.000000000000000000 ) ) 
 REPRESENTATION_ITEM ( '' )  );
#47901 = CARTESIAN_POINT ( 'NONE',  ( -21.22285432549390194, 1509.591297325790038, 229.2096536192680105 ) ) ;
#47902 = CARTESIAN_POINT ( 'NONE',  ( -107.0144515918482284, 1391.913060387290216, 307.4418155938021187 ) ) ;
#47903 = CARTESIAN_POINT ( 'NONE',  ( 10.95509605640000039, 1422.839500331020190, 206.5757350954289961 ) ) ;
#47904 = CARTESIAN_POINT ( 'NONE',  ( 0.7581006759604393963, 1498.651877382277689, 197.8214185162987917 ) ) ;
#47906 = CARTESIAN_POINT ( 'NONE',  ( -15.85591190879999779, 1415.880081504350073, 209.4912631162540038 ) ) ;
#47905 = CARTESIAN_POINT ( 'NONE',  ( -4.034908597844999889, 1517.068717944079935, 216.4577469658269990 ) ) ;
#47907 = CARTESIAN_POINT ( 'NONE',  ( -22.51990865419010035, 1410.619212616680215, 212.0399858957769936 ) ) ;
#47908 = CARTESIAN_POINT ( 'NONE',  ( 30.04822308544837384, 1524.382868172804365, 221.7633950662767290 ) ) ;
#47909 = AXIS2_PLACEMENT_3D ( 'NONE', #74269, #14322, #39544 ) ;
#47910 = VERTEX_POINT ( 'NONE', #91957 ) ;
#47911 = CARTESIAN_POINT ( 'NONE',  ( -6.942973667334999988, 1516.833844030519913, 201.7931697622170191 ) ) ;
#47912 = CARTESIAN_POINT ( 'NONE',  ( -19.00334344016446764, 1416.835288280170971, 207.9336683422605461 ) ) ;
#47913 = VERTEX_POINT ( 'NONE', #41001 ) ;
#47914 = CARTESIAN_POINT ( 'NONE',  ( 11.60004869884797252, 1426.686844628437029, 134.5519029425135216 ) ) ;
#47915 = CARTESIAN_POINT ( 'NONE',  ( 24.42191297719999810, 1445.300895561380003, 213.9593811286180198 ) ) ;
#47916 = CARTESIAN_POINT ( 'NONE',  ( 8.882670428210953872, 1437.098088324273021, 153.1961944285610855 ) ) ;
#47917 = CARTESIAN_POINT ( 'NONE',  ( 9.625916079488465726, 1425.428719264066558, 195.5010095755044119 ) ) ;
#47918 = CARTESIAN_POINT ( 'NONE',  ( 2.713660715419999647, 1441.511099666689915, 218.6663635638090000 ) ) ;
#47919 = CARTESIAN_POINT ( 'NONE',  ( 16.31056445758360951, 1421.543483176982136, 227.2422000032759115 ) ) ;
#47920 = CARTESIAN_POINT ( 'NONE',  ( -2.500000000200000017, 1447.619163115419724, 168.9991030154980081 ) ) ;
#47921 = CARTESIAN_POINT ( 'NONE',  ( -19.81973760889999880, 1426.576893715330016, 222.8594164923980259 ) ) ;
#47922 = CARTESIAN_POINT ( 'NONE',  ( -21.83293579365600934, 1470.997130817396737, 269.4963378681733843 ) ) ;
#47923 = CARTESIAN_POINT ( 'NONE',  ( -106.1649378089999942, 1391.047127029819876, 300.9392596058589788 ) ) ;
#47924 = CARTESIAN_POINT ( 'NONE',  ( 18.13816720160000173, 1445.350867493739770, 191.0157095493979966 ) ) ;
#47926 = CARTESIAN_POINT ( 'NONE',  ( -17.51694058469201920, 1434.100402768573076, 216.1837452212066637 ) ) ;
#47925 = CARTESIAN_POINT ( 'NONE',  ( -105.9134739529999933, 1391.838461175369957, 304.2044424958590412 ) ) ;
#47927 = CARTESIAN_POINT ( 'NONE',  ( -38.85577259545065942, 1452.541743301062752, 269.5906804772505438 ) ) ;
#47928 = ORIENTED_EDGE ( 'NONE', *, *, #38446, .F. ) ;
#47929 = DIRECTION ( 'NONE',  ( 0.000000000000000000, 6.123233995736769734E-17, 1.000000000000000000 ) ) ;
#47930 = CARTESIAN_POINT ( 'NONE',  ( -15.46794562779999893, 1508.541555192090073, 214.7748198980189898 ) ) ;
#47931 = CARTESIAN_POINT ( 'NONE',  ( 11.48266949309999951, 1442.832333866149838, 147.8781297902980043 ) ) ;
#47932 = EDGE_CURVE ( 'NONE', #97755, #74404, #12183, .T. ) ;
#47933 = VECTOR ( 'NONE', #21346, 1000.000000000000000 ) ;
#47934 = CARTESIAN_POINT ( 'NONE',  ( 31.34491535884036040, 1525.848196786131211, 201.1913537499540894 ) ) ;
#47935 = CARTESIAN_POINT ( 'NONE',  ( -15.96958168569999970, 1519.913060387329779, 225.0914276473980067 ) ) ;
#47936 = CARTESIAN_POINT ( 'NONE',  ( 1.465959060849369999, 1490.245831247160140, 181.8489739673789813 ) ) ;
#47937 = CARTESIAN_POINT ( 'NONE',  ( -3.527569048119670203, 1486.518325592330029, 181.8541486797999767 ) ) ;
#47938 = CARTESIAN_POINT ( 'NONE',  ( -13.32047630834354379, 1444.558074092078868, 186.7651240210572610 ) ) ;
#47939 = CARTESIAN_POINT ( 'NONE',  ( -9.139715296915689180, 1438.756510518619962, 209.0162231784520088 ) ) ;
#47940 = CARTESIAN_POINT ( 'NONE',  ( 0.000000000000000000, 1522.051704408389924, 209.1218459616979999 ) ) ;
#47941 = CARTESIAN_POINT ( 'NONE',  ( -7.965810688893188996, 1384.899971919800009, 199.4892299149449855 ) ) ;
#47942 = CARTESIAN_POINT ( 'NONE',  ( -14.87973836575140041, 1415.677402202029953, 206.9056846400189897 ) ) ;
#47943 = DIRECTION ( 'NONE',  ( -1.000000000000000000, 0.000000000000000000, 0.000000000000000000 ) ) ;
#47944 = CARTESIAN_POINT ( 'NONE',  ( 7.987221624930000985, 1428.707470559690137, 214.3354289489490156 ) ) ;
#47946 = ORIENTED_EDGE ( 'NONE', *, *, #107050, .F. ) ;
#47945 = CARTESIAN_POINT ( 'NONE',  ( 12.27023112330000032, 1416.839692136459917, 223.5796784318309847 ) ) ;
#47947 = CARTESIAN_POINT ( 'NONE',  ( -106.7189926970000187, 1380.782700635500078, 299.4006339732590050 ) ) ;
#47948 = CARTESIAN_POINT ( 'NONE',  ( 14.62991242738410058, 1513.722010161000071, 224.1519871687980014 ) ) ;
#47949 = ORIENTED_EDGE ( 'NONE', *, *, #76982, .T. ) ;
#47950 = ORIENTED_EDGE ( 'NONE', *, *, #60374, .F. ) ;
#47951 = CARTESIAN_POINT ( 'NONE',  ( -12.75386558790000002, 1502.395049388389907, 210.0740108765389778 ) ) ;
#47952 = CARTESIAN_POINT ( 'NONE',  ( -8.589426147275000645, 1436.798469860880004, 209.9038450004319998 ) ) ;
#47954 = CARTESIAN_POINT ( 'NONE',  ( -4.694071443940000421, 1465.143864313730091, 238.2947549836979988 ) ) ;
#47953 = CARTESIAN_POINT ( 'NONE',  ( 38.89347719239705725, 1429.350770580238759, 269.5911400078334736 ) ) ;
#47955 = CARTESIAN_POINT ( 'NONE',  ( -20.19216181010000000, 1506.518050785829928, 189.2324904367980309 ) ) ;
#47956 = VECTOR ( 'NONE', #37724, 999.9999999999998863 ) ;
#47957 = CARTESIAN_POINT ( 'NONE',  ( -11.12720837410000030, 1433.553190407860029, 151.6643070703979959 ) ) ;
#47958 = CARTESIAN_POINT ( 'NONE',  ( 19.64992912776053657, 1521.951704408389787, 207.6921549199338983 ) ) ;
#47959 = CARTESIAN_POINT ( 'NONE',  ( 11.72449310896590013, 1426.703930266699899, 143.2718442946500090 ) ) ;
#47960 = DIRECTION ( 'NONE',  ( 0.000000000000000000, 0.000000000000000000, 1.000000000000000000 ) ) ;
#47961 = CARTESIAN_POINT ( 'NONE',  ( 0.9669097429690169943, 1515.111355597249940, 213.4500754500990070 ) ) ;
#47962 = CARTESIAN_POINT ( 'NONE',  ( -19.97968237250000101, 1483.906011188890034, 214.0068283976289933 ) ) ;
#47963 = DIRECTION ( 'NONE',  ( -0.9993908263153354898, 0.03489949404026521790, 3.990594469010557284E-05 ) ) ;
#47964 = CIRCLE ( 'NONE', #110543, 2.000000000000001776 ) ;
#47965 = CARTESIAN_POINT ( 'NONE',  ( 5.264170345090959380, 1362.294551344075671, 210.6218459617142003 ) ) ;
#47966 = CARTESIAN_POINT ( 'NONE',  ( -22.52609270459879909, 1509.699688878229836, 190.3921826462719764 ) ) ;
#47968 = ORIENTED_EDGE ( 'NONE', *, *, #70625, .F. ) ;
#47967 = CARTESIAN_POINT ( 'NONE',  ( -6.143218938422219407E-10, 1412.721203181489955, 251.5507141014840045 ) ) ;
#47969 = VERTEX_POINT ( 'NONE', #90295 ) ;
#47970 = CARTESIAN_POINT ( 'NONE',  ( 21.62164173114529930, 1521.951704408389787, 208.0273405545509888 ) ) ;
#47971 = EDGE_CURVE ( 'NONE', #19696, #7591, #56933, .T. ) ;
#47972 = EDGE_CURVE ( 'NONE', #33967, #104880, #60534, .T. ) ;
#47973 = CARTESIAN_POINT ( 'NONE',  ( 13.58730094343779982, 1498.318843676340066, 227.8486215837370139 ) ) ;
#47974 = CARTESIAN_POINT ( 'NONE',  ( -13.45498908600000121, 1472.108093304129852, 270.3655312995979898 ) ) ;
#47975 = CARTESIAN_POINT ( 'NONE',  ( 13.43167025587599817, 1509.382104656720003, 235.1752264429409820 ) ) ;
#47976 = CARTESIAN_POINT ( 'NONE',  ( -124.5778210738000809, 1377.418846546389886, 301.3676796492106860 ) ) ;
#47977 = EDGE_CURVE ( 'NONE', #41836, #42097, #83548, .T. ) ;
#47978 = CARTESIAN_POINT ( 'NONE',  ( -13.83973980200000220, 1452.407470494729978, 223.0844041600979892 ) ) ;
#47980 = EDGE_CURVE ( 'NONE', #68835, #92411, #48315, .T. ) ;
#47979 = CARTESIAN_POINT ( 'NONE',  ( 0.2157562901360330077, 1451.841949984589974, 182.9506228356109716 ) ) ;
#47981 = CARTESIAN_POINT ( 'NONE',  ( -9.092273600540000444, 1384.801544621870107, 199.9443845869589893 ) ) ;
#47982 = EDGE_CURVE ( 'NONE', #59669, #88136, #74079, .T. ) ;
#47983 = CARTESIAN_POINT ( 'NONE',  ( 12.78776258895000062, 1416.851343899079893, 222.7045348340550106 ) ) ;
#47984 = CARTESIAN_POINT ( 'NONE',  ( -3.440623305239999929, 1458.093607836889760, 219.2469823057990084 ) ) ;
#47985 = CARTESIAN_POINT ( 'NONE',  ( 10.97628319970143274, 1365.429341111210306, 207.6218459616987673 ) ) ;
#47986 = CARTESIAN_POINT ( 'NONE',  ( -41.79789112272889895, 1426.458875065289931, 266.3000610535190162 ) ) ;
#47987 = ORIENTED_EDGE ( 'NONE', *, *, #55500, .T. ) ;
#47988 = CYLINDRICAL_SURFACE ( 'NONE', #48443, 4.000000000000003553 ) ;
#47989 = VERTEX_POINT ( 'NONE', #65676 ) ;
#47990 = ORIENTED_EDGE ( 'NONE', *, *, #41892, .T. ) ;
#47991 = CARTESIAN_POINT ( 'NONE',  ( -4.995623491025000362, 1516.636036526019780, 210.8344906863870278 ) ) ;
#47992 = CARTESIAN_POINT ( 'NONE',  ( 4.817341278711412933, 1423.525569767164825, 184.0959883682457132 ) ) ;
#47993 = AXIS2_PLACEMENT_3D ( 'NONE', #35437, #27588, #1865 ) ;
#47995 = DIRECTION ( 'NONE',  ( 0.9858563016923833633, 0.000000000000000000, 0.1675928173085483863 ) ) ;
#47994 = CARTESIAN_POINT ( 'NONE',  ( 7.335900995594999863, 1517.068717944079935, 213.1567545299469657 ) ) ;
#47996 = CARTESIAN_POINT ( 'NONE',  ( -7.781677482780000155, 1455.443741433530249, 185.5405848752979807 ) ) ;
#47997 = CARTESIAN_POINT ( 'NONE',  ( -15.76201573909119880, 1470.477545809950243, 228.9865716979510069 ) ) ;
#47998 = ORIENTED_EDGE ( 'NONE', *, *, #66484, .F. ) ;
#47999 = CARTESIAN_POINT ( 'NONE',  ( -26.64155692649999807, 1435.970859033209990, 136.4793274970979837 ) ) ;
#48000 = ADVANCED_FACE ( 'NONE', ( #99239 ), #81342, .F. ) ;
#48001 = B_SPLINE_CURVE_WITH_KNOTS ( 'NONE', 5,
 ( #62223, #53828, #70082, #44869, #45418, #71177, #104195, #53264, #85729 ),
 .UNSPECIFIED., .F., .F.,
 ( 6, 3, 6 ),
 ( 463.1457853109999974, 468.8934854820000169, 473.5625621899999942 ),
 .UNSPECIFIED. ) ;
#48002 = CARTESIAN_POINT ( 'NONE',  ( 6.553524377605000062, 1516.882690742909972, 202.1776141839370098 ) ) ;
#48003 = CARTESIAN_POINT ( 'NONE',  ( -37.55262740391170695, 1450.862648352295537, 134.7342543275423452 ) ) ;
#48004 = EDGE_CURVE ( 'NONE', #37474, #10931, #56159, .T. ) ;
#48005 = CARTESIAN_POINT ( 'NONE',  ( 1.092787220074867172, 1508.991959848587385, 238.7857758380762903 ) ) ;
#48006 = CARTESIAN_POINT ( 'NONE',  ( -27.13870397648479837, 1417.586336025329956, 269.4419590831910227 ) ) ;
#48007 = CARTESIAN_POINT ( 'NONE',  ( -6.682617376610000548, 1481.590913066989970, 205.7929905812889899 ) ) ;
#48008 = CARTESIAN_POINT ( 'NONE',  ( -3.817532458140000085, 1397.107874215530046, 196.7824443944979862 ) ) ;
#48010 = ORIENTED_EDGE ( 'NONE', *, *, #90466, .F. ) ;
#48009 = CARTESIAN_POINT ( 'NONE',  ( -9.977700672476359500, 1365.292605733893879, 210.6218459616987957 ) ) ;
#48011 = ORIENTED_EDGE ( 'NONE', *, *, #9035, .T. ) ;
#48013 = EDGE_CURVE ( 'NONE', #61056, #37055, #13565, .T. ) ;
#48012 = CARTESIAN_POINT ( 'NONE',  ( 0.2313785129550000041, 1452.338695476229759, 183.2832210453979940 ) ) ;
#48014 = DIRECTION ( 'NONE',  ( -0.8642610224695934651, -1.396226527196591439E-14, -0.5030436214085343138 ) ) ;
#48015 = CARTESIAN_POINT ( 'NONE',  ( 2.199364402880799929, 1426.043163797689886, 191.2103802779980128 ) ) ;
#48016 = CARTESIAN_POINT ( 'NONE',  ( -13.29541393167429852, 1436.106548041590031, 150.6070985400420170 ) ) ;
#48017 = CARTESIAN_POINT ( 'NONE',  ( -0.03628264342808269760, 1409.501674693219911, 185.3028950835800117 ) ) ;
#48018 = CARTESIAN_POINT ( 'NONE',  ( 4.625789976465000564, 1517.104192383289956, 210.2432295619669844 ) ) ;
#48019 = EDGE_CURVE ( 'NONE', #84553, #46912, #13080, .T. ) ;
#48020 = CARTESIAN_POINT ( 'NONE',  ( -68.75214133429999208, 1379.747884264789946, 280.1338633208590068 ) ) ;
#48021 = CARTESIAN_POINT ( 'NONE',  ( -23.42324794740000016, 1435.764285783320247, 213.6171179551379851 ) ) ;
#48022 = CARTESIAN_POINT ( 'NONE',  ( -13.89764403649999913, 1426.832043286230146, 222.2177421718979815 ) ) ;
#48023 = CARTESIAN_POINT ( 'NONE',  ( 12.26815783919999880, 1415.553739807329976, 222.8908496634980168 ) ) ;
#48024 = CARTESIAN_POINT ( 'NONE',  ( 7.559010162584999470, 1510.805212328559946, 203.6254154108069940 ) ) ;
#48025 = CARTESIAN_POINT ( 'NONE',  ( 1.118104729594999958, 1516.965971551240045, 206.8221779662269739 ) ) ;
#48026 = ORIENTED_EDGE ( 'NONE', *, *, #84024, .F. ) ;
#48027 = CARTESIAN_POINT ( 'NONE',  ( -40.71747596589660390, 1448.637563225599934, 134.7398509209010058 ) ) ;
#48028 = CARTESIAN_POINT ( 'NONE',  ( -23.94385147653602885, 1445.794803258163483, 213.0147832418295764 ) ) ;
#48029 = EDGE_LOOP ( 'NONE', ( #1442, #88354, #54381, #386, #32632, #70630 ) ) ;
#48030 = CARTESIAN_POINT ( 'NONE',  ( 17.96021206209637811, 1457.749394617433381, 229.4559061195007530 ) ) ;
#48031 = CARTESIAN_POINT ( 'NONE',  ( -28.59841874989484367, 1509.911739175358662, 211.5620547949469312 ) ) ;
#48032 = CARTESIAN_POINT ( 'NONE',  ( 13.20846943169999932, 1414.988017870030035, 197.7899243759980266 ) ) ;
#48033 = CARTESIAN_POINT ( 'NONE',  ( -2.480175256589999933, 1429.207669907389800, 200.0830570456390092 ) ) ;
#48034 = CARTESIAN_POINT ( 'NONE',  ( 19.90019938289999857, 1410.103226705929956, 197.6288084474979883 ) ) ;
#48035 = CARTESIAN_POINT ( 'NONE',  ( -7.982037141949999359, 1424.874072662569915, 210.5243721551090061 ) ) ;
#48036 = CARTESIAN_POINT ( 'NONE',  ( -14.06834915342731485, 1379.597580802498896, 211.7528822239692659 ) ) ;
#48037 = CARTESIAN_POINT ( 'NONE',  ( -0.04210048962123905114, 1506.527232291142582, 187.0606773027650434 ) ) ;
#48038 = CARTESIAN_POINT ( 'NONE',  ( 24.64629085034158607, 1442.486177488785188, 212.7671816332840251 ) ) ;
#48039 = CARTESIAN_POINT ( 'NONE',  ( -4.500000000000000000, 1439.615672362369878, 183.5288080717980108 ) ) ;
#48040 = AXIS2_PLACEMENT_3D ( 'NONE', #52276, #24810, #59014 ) ;
#48041 = CARTESIAN_POINT ( 'NONE',  ( -113.4000000000000057, 1391.913060387289988, 304.2218459572590064 ) ) ;
#48042 = CARTESIAN_POINT ( 'NONE',  ( 2.873329360754999673, 1516.572193931679976, 216.4439510378570048 ) ) ;
#48043 = ORIENTED_EDGE ( 'NONE', *, *, #88581, .F. ) ;
#48044 = CARTESIAN_POINT ( 'NONE',  ( 7.714747304227939750, 1516.752573823159992, 208.4886776470619907 ) ) ;
#48045 = CARTESIAN_POINT ( 'NONE',  ( -4.692099526989998992, 1474.463958302690116, 198.6947328130989945 ) ) ;
#48046 = CIRCLE ( 'NONE', #62389, 1.000000000000000888 ) ;
#48047 = CARTESIAN_POINT ( 'NONE',  ( -18.06717587838990013, 1416.826860677879949, 209.3441468771879954 ) ) ;
#48048 = AXIS2_PLACEMENT_3D ( 'NONE', #73811, #47498, #91688 ) ;
#48049 = CARTESIAN_POINT ( 'NONE',  ( 1.514738106409309948, 1507.606285602550088, 186.2052147526660235 ) ) ;
#48050 = CARTESIAN_POINT ( 'NONE',  ( 1.547463896846929865, 1414.913060387349788, 192.3096116128920130 ) ) ;
#48051 = CARTESIAN_POINT ( 'NONE',  ( 11.41850631254851578, 1425.727621129565023, 138.9282626850327631 ) ) ;
#48052 = DIRECTION ( 'NONE',  ( 4.137698748470009068E-18, 0.000000000000000000, 1.000000000000000000 ) ) ;
#48053 = B_SPLINE_CURVE_WITH_KNOTS ( 'NONE', 5,
 ( #39654, #62842, #96955, #20221, #54422, #11838 ),
 .UNSPECIFIED., .F., .F.,
 ( 6, 6 ),
 ( 0.9643540072699122723, 1.000000000000000000 ),
 .UNSPECIFIED. ) ;
#48054 = CARTESIAN_POINT ( 'NONE',  ( 17.95318235374812588, 1423.997979201475118, 225.6706602935287265 ) ) ;
#48055 = CARTESIAN_POINT ( 'NONE',  ( 1.722617949397659887, 1456.338984862310099, 198.6776180596440042 ) ) ;
#48056 = CARTESIAN_POINT ( 'NONE',  ( -112.5460140234005735, 1375.913060387289988, 303.7015499340457723 ) ) ;
#48057 = CARTESIAN_POINT ( 'NONE',  ( 30.96029428649589832, 1440.913060384339815, 241.2683408943260019 ) ) ;
#48058 = FACE_OUTER_BOUND ( 'NONE', #100170, .T. ) ;
#48059 = FACE_OUTER_BOUND ( 'NONE', #27489, .T. ) ;
#48060 = VERTEX_POINT ( 'NONE', #51076 ) ;
#48061 = ORIENTED_EDGE ( 'NONE', *, *, #91505, .T. ) ;
#48062 = CARTESIAN_POINT ( 'NONE',  ( 12.53380498098208840, 1442.773887284840384, 150.7612718761199062 ) ) ;
#48063 = B_SPLINE_CURVE_WITH_KNOTS ( 'NONE', 5,
 ( #76581, #41334, #75504, #74951, #109638, #25051, #91724, #33453, #8809 ),
 .UNSPECIFIED., .F., .F.,
 ( 6, 3, 6 ),
 ( -12.51705759590000078, -7.545169656169999683, -3.809711666909999295 ),
 .UNSPECIFIED. ) ;
#48064 = EDGE_CURVE ( 'NONE', #39470, #58564, #24283, .T. ) ;
#48065 = LINE ( 'NONE', #64885, #6774 ) ;
#48066 = CARTESIAN_POINT ( 'NONE',  ( -4.304668157050000055, 1442.652147467789973, 200.8964050455090273 ) ) ;
#48067 = CARTESIAN_POINT ( 'NONE',  ( 7.815357466500000072, 1423.735213141060058, 195.8220613176989957 ) ) ;
#48068 = VECTOR ( 'NONE', #94965, 1000.000000000000000 ) ;
#48069 = EDGE_CURVE ( 'NONE', #108182, #40151, #46924, .T. ) ;
#48070 = CYLINDRICAL_SURFACE ( 'NONE', #75052, 2.000000000000003109 ) ;
#48071 = DIRECTION ( 'NONE',  ( 0.8775825618903763115, 0.000000000000000000, -0.4794255386041963996 ) ) ;
#48072 = CARTESIAN_POINT ( 'NONE',  ( -5.519906363166400709, 1440.499855196290127, 154.7645174855159951 ) ) ;
#48073 = CARTESIAN_POINT ( 'NONE',  ( -36.57638826848899782, 1383.833252621880092, 236.1977204853059789 ) ) ;
#48074 =( BOUNDED_CURVE ( )  B_SPLINE_CURVE ( 3, ( #62049, #77720, #26755, #18888 ),
 .UNSPECIFIED., .F., .F. ) 
 B_SPLINE_CURVE_WITH_KNOTS ( ( 4, 4 ),
 ( 0.1582411938933160067, 0.2197467457803065072 ),
 .UNSPECIFIED. ) 
 CURVE ( )  GEOMETRIC_REPRESENTATION_ITEM ( )  RATIONAL_B_SPLINE_CURVE ( ( 1.000000000000000000, 0.9996847804345658783, 0.9996847804345658783, 1.000000000000000000 ) ) 
 REPRESENTATION_ITEM ( '' )  );
#48075 = CARTESIAN_POINT ( 'NONE',  ( -5.441672406744999968, 1511.126521646420088, 201.4186169135170132 ) ) ;
#48076 = CARTESIAN_POINT ( 'NONE',  ( -12.73048902499999890, 1416.839648768630013, 195.1127163454979723 ) ) ;
#48077 = CARTESIAN_POINT ( 'NONE',  ( 22.59589169820000265, 1507.700907224229923, 209.5602205471840023 ) ) ;
#48078 = DIRECTION ( 'NONE',  ( 0.000000000000000000, 1.000000000000000000, 0.000000000000000000 ) ) ;
#48080 = ORIENTED_EDGE ( 'NONE', *, *, #51552, .T. ) ;
#48079 = CARTESIAN_POINT ( 'NONE',  ( 3.196970390959999797, 1490.438169550290013, 188.4165637325990303 ) ) ;
#48081 = CARTESIAN_POINT ( 'NONE',  ( -1.034612360689999955, 1450.827783963229876, 181.5425543420979864 ) ) ;
#48082 = EDGE_CURVE ( 'NONE', #288, #1510, #71270, .T. ) ;
#48083 = CARTESIAN_POINT ( 'NONE',  ( -28.08746868569999933, 1382.324033938389903, 225.1301489039589967 ) ) ;
#48084 = CARTESIAN_POINT ( 'NONE',  ( 2.968682044221400140, 1508.551704408389924, 204.1814749987780147 ) ) ;
#48086 = EDGE_LOOP ( 'NONE', ( #26933, #35284, #75407, #72256 ) ) ;
#48085 = CARTESIAN_POINT ( 'NONE',  ( -31.12456774391166547, 1525.960063244516959, 217.0912716842400130 ) ) ;
#48087 = CARTESIAN_POINT ( 'NONE',  ( 22.24401761576379855, 1475.958701603000009, 209.7631723292300023 ) ) ;
#48088 = ORIENTED_EDGE ( 'NONE', *, *, #29505, .F. ) ;
#48089 = CARTESIAN_POINT ( 'NONE',  ( -10.43842217732019861, 1388.008184915300035, 217.2398969709649919 ) ) ;
#48090 = CARTESIAN_POINT ( 'NONE',  ( 35.25381697133219205, 1437.199467842329796, 136.5363498936850135 ) ) ;
#48091 = DIRECTION ( 'NONE',  ( 1.000000000000000000, 0.000000000000000000, 0.000000000000000000 ) ) ;
#48092 = FACE_OUTER_BOUND ( 'NONE', #20357, .T. ) ;
#48093 = CARTESIAN_POINT ( 'NONE',  ( -106.3207909569999998, 1379.688851738430003, 300.3888801278590108 ) ) ;
#48094 = CARTESIAN_POINT ( 'NONE',  ( 3.958338146192914131, 1515.551704408294881, 211.4519800820672799 ) ) ;
#48095 = CARTESIAN_POINT ( 'NONE',  ( 7.729166927079999638, 1490.261404644089907, 208.7262156379529756 ) ) ;
#48096 = CARTESIAN_POINT ( 'NONE',  ( 22.69876404240077505, 1501.977400791986611, 181.3483716558180276 ) ) ;
#48097 = CARTESIAN_POINT ( 'NONE',  ( 18.02334845919999751, 1424.404998451829897, 224.9094352651979989 ) ) ;
#48098 = CARTESIAN_POINT ( 'NONE',  ( -2.016889697369080192, 1485.643995215409859, 197.3940317714459809 ) ) ;
#48099 = CARTESIAN_POINT ( 'NONE',  ( -19.22223935719999943, 1463.238052774929884, 191.9037305475980304 ) ) ;
#48100 = CARTESIAN_POINT ( 'NONE',  ( 11.86538723930000039, 1432.286167281789858, 149.9824190668979895 ) ) ;
#48101 = AXIS2_PLACEMENT_3D ( 'NONE', #34933, #50644, #101563 ) ;
#48102 = CARTESIAN_POINT ( 'NONE',  ( -2.434305826324310029, 1449.542286390619893, 183.0300738527029978 ) ) ;
#48103 = ORIENTED_EDGE ( 'NONE', *, *, #32405, .T. ) ;
#48104 = ORIENTED_EDGE ( 'NONE', *, *, #82382, .T. ) ;
#48105 = EDGE_CURVE ( 'NONE', #73515, #106529, #81925, .T. ) ;
#48106 = CARTESIAN_POINT ( 'NONE',  ( 18.31941652029303214, 1522.051704408389924, 203.8280657238408651 ) ) ;
#48107 = CARTESIAN_POINT ( 'NONE',  ( 19.03068750294750089, 1456.518195700050001, 227.4971866881460016 ) ) ;
#48108 =( BOUNDED_CURVE ( )  B_SPLINE_CURVE ( 3, ( #82173, #106282, #5473, #107930 ),
 .UNSPECIFIED., .F., .F. ) 
 B_SPLINE_CURVE_WITH_KNOTS ( ( 4, 4 ),
 ( 1.282549416543149912, 2.438195290895380118 ),
 .UNSPECIFIED. ) 
 CURVE ( )  GEOMETRIC_REPRESENTATION_ITEM ( )  RATIONAL_B_SPLINE_CURVE ( ( 1.000000000000000000, 0.8917691661751018239, 0.8917691661751018239, 1.000000000000000000 ) ) 
 REPRESENTATION_ITEM ( '' )  );
#48109 = LINE ( 'NONE', #5548, #83984 ) ;
#48110 = AXIS2_PLACEMENT_3D ( 'NONE', #104697, #19013, #63285 ) ;
#48111 = CYLINDRICAL_SURFACE ( 'NONE', #55489, 33.13701971169416538 ) ;
#48112 = CARTESIAN_POINT ( 'NONE',  ( -20.24618143411970195, 1496.404372048379855, 190.7218018821779992 ) ) ;
#48113 = CARTESIAN_POINT ( 'NONE',  ( 13.43167025587599817, 1509.382104656720003, 235.1752264429409820 ) ) ;
#48114 = CARTESIAN_POINT ( 'NONE',  ( -108.6094801609999934, 1386.676297506519859, 310.8587284262589492 ) ) ;
#48115 = CARTESIAN_POINT ( 'NONE',  ( 0.1595984450810000177, 1486.508833535129952, 181.8147410097979844 ) ) ;
#48116 = CARTESIAN_POINT ( 'NONE',  ( -9.057796188674942073, 1360.633927564615988, 208.3718459617010978 ) ) ;
#48117 = CARTESIAN_POINT ( 'NONE',  ( -45.88369462358249251, 1440.913065976889811, 266.4123280151379731 ) ) ;
#48118 = CARTESIAN_POINT ( 'NONE',  ( 13.43419142301149982, 1508.291771318299880, 233.2426489798709781 ) ) ;
#48119 = CARTESIAN_POINT ( 'NONE',  ( -30.51231035492526900, 1524.382868172863937, 200.0858385050243555 ) ) ;
#48120 = EDGE_CURVE ( 'NONE', #9928, #29539, #33149, .T. ) ;
#48121 = CARTESIAN_POINT ( 'NONE',  ( 7.708745647785000266, 1516.523379810429788, 207.4137536659370085 ) ) ;
#48122 = CARTESIAN_POINT ( 'NONE',  ( -8.891021255688182023, 1447.878015951419911, 211.6948139168939917 ) ) ;
#48123 = CARTESIAN_POINT ( 'NONE',  ( 2.807051378689749743, 1408.949923395980022, 223.3166750014169963 ) ) ;
#48124 = CIRCLE ( 'NONE', #67790, 0.9999999999999981126 ) ;
#48125 = CARTESIAN_POINT ( 'NONE',  ( -13.44914210490000173, 1435.283433589039760, 149.9761265592980237 ) ) ;
#48126 = CARTESIAN_POINT ( 'NONE',  ( 29.67167576298692566, 1526.344110814223313, 201.2571182723716845 ) ) ;
#48127 = CARTESIAN_POINT ( 'NONE',  ( 4.329341231296368164, 1515.068899845852911, 206.1636068449589629 ) ) ;
#48128 = CARTESIAN_POINT ( 'NONE',  ( 6.826200034800000260, 1424.874072630889941, 213.4902541782590220 ) ) ;
#48129 = EDGE_CURVE ( 'NONE', #24247, #17035, #6868, .T. ) ;
#48130 = VERTEX_POINT ( 'NONE', #94154 ) ;
#48131 = AXIS2_PLACEMENT_3D ( 'NONE', #98899, #30602, #82099 ) ;
#48132 = CARTESIAN_POINT ( 'NONE',  ( -2.712032821819999946E-09, 1413.088571902330159, 250.5651368503980052 ) ) ;
#48133 = CARTESIAN_POINT ( 'NONE',  ( -28.27621775920000147, 1508.136061367030152, 209.0190599981050070 ) ) ;
#48135 = DIRECTION ( 'NONE',  ( -5.980589973904019347E-17, 1.000000000000000000, -1.736889445713099699E-16 ) ) ;
#48134 = CARTESIAN_POINT ( 'NONE',  ( -3.494005144269999974, 1464.122160809730076, 182.8043410306979979 ) ) ;
#48136 = CARTESIAN_POINT ( 'NONE',  ( -44.93136599389160324, 1440.913052653349951, 269.6838063022050278 ) ) ;
#48137 = CARTESIAN_POINT ( 'NONE',  ( -26.57890459689999929, 1439.181835129569890, 225.2395996781980045 ) ) ;
#48138 = CARTESIAN_POINT ( 'NONE',  ( -2.194060776939999791, 1486.670284103789982, 220.4458495409990064 ) ) ;
#48139 = CARTESIAN_POINT ( 'NONE',  ( -17.80061515946090012, 1452.291449208500126, 145.5827938162609883 ) ) ;
#48140 = CARTESIAN_POINT ( 'NONE',  ( -18.89905520810000183, 1416.828042640230024, 207.5748962046480131 ) ) ;
#48141 = ORIENTED_EDGE ( 'NONE', *, *, #108376, .F. ) ;
#48142 = CARTESIAN_POINT ( 'NONE',  ( -2.500000000000000000, 1419.382898234900267, 144.1038724149900077 ) ) ;
#48143 = CARTESIAN_POINT ( 'NONE',  ( 2.140036995326180090E-16, 1390.913060387289988, 209.1218459572589836 ) ) ;
#48144 = CARTESIAN_POINT ( 'NONE',  ( 14.73070258383249964, 1421.964157080649784, 230.3680856299650088 ) ) ;
#48145 = CARTESIAN_POINT ( 'NONE',  ( 10.93416347059999794, 1501.622886110689933, 205.7061242847990172 ) ) ;
#48146 = ORIENTED_EDGE ( 'NONE', *, *, #87461, .F. ) ;
#48147 = ORIENTED_EDGE ( 'NONE', *, *, #63757, .F. ) ;
#48148 = EDGE_CURVE ( 'NONE', #31839, #55731, #88352, .T. ) ;
#48149 = CARTESIAN_POINT ( 'NONE',  ( -23.00023858420000167, 1384.678484070659806, 202.3918768682790130 ) ) ;
#48150 = CARTESIAN_POINT ( 'NONE',  ( -22.92652434121600180, 1409.723337951930034, 209.1949791247940027 ) ) ;
#48151 = VERTEX_POINT ( 'NONE', #59483 ) ;
#48152 = CARTESIAN_POINT ( 'NONE',  ( -0.04545031206760000164, 1419.318382049229967, 227.3945661680980095 ) ) ;
#48153 = CIRCLE ( 'NONE', #110718, 2.000000000000000000 ) ;
#48154 = DIRECTION ( 'NONE',  ( 0.000000000000000000, 1.000000000000000000, 0.000000000000000000 ) ) ;
#48155 = EDGE_CURVE ( 'NONE', #35721, #78966, #51566, .T. ) ;
#48156 = B_SPLINE_CURVE_WITH_KNOTS ( 'NONE', 5,
 ( #71624, #72691, #63214, #88922, #48031, #73797 ),
 .UNSPECIFIED., .F., .F.,
 ( 6, 6 ),
 ( 0.000000000000000000, 1.000000000000000000 ),
 .UNSPECIFIED. ) ;
#48157 = CARTESIAN_POINT ( 'NONE',  ( -21.44134523410942350, 1436.476996378036119, 143.7821035677283703 ) ) ;
#48158 = FACE_OUTER_BOUND ( 'NONE', #39528, .T. ) ;
#48159 = EDGE_LOOP ( 'NONE', ( #19356, #75432, #23930, #90303 ) ) ;
#48160 = CARTESIAN_POINT ( 'NONE',  ( 45.10266683548830002, 1448.532721670820138, 268.2401720598069801 ) ) ;
#48161 = CARTESIAN_POINT ( 'NONE',  ( -12.40160425681999889, 1414.913057846380070, 220.2831263726729958 ) ) ;
#48162 = CARTESIAN_POINT ( 'NONE',  ( 0.01913614526999999829, 1420.208243963930045, 183.8949348176980152 ) ) ;
#48163 = CARTESIAN_POINT ( 'NONE',  ( 4.029572640705000985, 1516.858649670339901, 205.0803734583570019 ) ) ;
#48164 = VERTEX_POINT ( 'NONE', #46544 ) ;
#48165 = CARTESIAN_POINT ( 'NONE',  ( -3.154911953494088372, 1432.397052738174352, 216.9484949157356652 ) ) ;
#48166 = CARTESIAN_POINT ( 'NONE',  ( 13.23381494117745127, 1443.155553023363836, 187.6033365495667624 ) ) ;
#48167 = ORIENTED_EDGE ( 'NONE', *, *, #83652, .T. ) ;
#48168 = ORIENTED_EDGE ( 'NONE', *, *, #55884, .T. ) ;
#48169 = CARTESIAN_POINT ( 'NONE',  ( 0.4151546846839010985, 1522.906561336852974, 173.3106345060153046 ) ) ;
#48170 = CARTESIAN_POINT ( 'NONE',  ( 4.491293097786513755, 1508.884207228267314, 205.6342589212028713 ) ) ;
#48171 = CARTESIAN_POINT ( 'NONE',  ( -13.08508101585309902, 1512.436270050410030, 193.8787656426380011 ) ) ;
#48172 = CARTESIAN_POINT ( 'NONE',  ( -1.247677516857949989E-10, 1452.913060387320002, 152.5211338456990120 ) ) ;
#48173 = CARTESIAN_POINT ( 'NONE',  ( 11.61220494760000044, 1420.579219889470096, 199.3493800206389892 ) ) ;
#48174 = CARTESIAN_POINT ( 'NONE',  ( 19.28172097450000066, 1455.754227538689975, 211.0042463156089809 ) ) ;
#48175 = CARTESIAN_POINT ( 'NONE',  ( -109.2435801578418619, 1382.302282213249782, 297.4663600009405968 ) ) ;
#48176 = CARTESIAN_POINT ( 'NONE',  ( 10.04874238532330111, 1480.247552555629909, 205.9343909418280134 ) ) ;
#48177 = DIRECTION ( 'NONE',  ( 0.03489949670250328678, -0.9993908270190956511, 0.000000000000000000 ) ) ;
#48179 = DIRECTION ( 'NONE',  ( 1.056181180700544810E-06, 0.03085828021460187628, -0.9995237698729737552 ) ) ;
#48178 = CARTESIAN_POINT ( 'NONE',  ( -13.19868063547539805, 1434.864246101540175, 149.0205925190539915 ) ) ;
#48180 = CARTESIAN_POINT ( 'NONE',  ( 10.67027879645779898, 1424.424156321159899, 206.6093414022110153 ) ) ;
#48181 = CARTESIAN_POINT ( 'NONE',  ( -9.702105246842089414, 1440.203813892860126, 206.6216695874250036 ) ) ;
#48182 = CARTESIAN_POINT ( 'NONE',  ( 4.838067302830000749, 1426.802081400929865, 145.9750725641980011 ) ) ;
#48183 = ORIENTED_EDGE ( 'NONE', *, *, #32722, .T. ) ;
#48184 = LINE ( 'NONE', #14553, #58051 ) ;
#48185 = CIRCLE ( 'NONE', #91086, 1.000002391826645187 ) ;
#48186 = CARTESIAN_POINT ( 'NONE',  ( 4.163336342339999869E-15, 1416.181292664740113, 209.1218459616989946 ) ) ;
#48187 = CARTESIAN_POINT ( 'NONE',  ( -80.39083381333070122, 1384.992927882670074, 304.1219082020649580 ) ) ;
#48188 = B_SPLINE_SURFACE_WITH_KNOTS ( 'NONE', 5, 5, ( 
 ( #43523, #88823, #53033, #52481, #19390, #77666 ),
 ( #95018, #27817, #19954, #11569, #36768, #87739 ),
 ( #97215, #37323, #69285, #53593, #44631, #103390 ),
 ( #2087, #11017, #36216, #70401, #71519, #979 ),
 ( #104520, #45188, #105075, #54147, #88276, #45745 ),
 ( #18288, #86609, #9903, #78210, #22132, #13189 ),
 ( #3744, #47924, #98315, #40071, #64756, #13740 ),
 ( #22685, #73700, #48494, #12666, #82634, #56885 ),
 ( #80430, #21594, #72584, #91015, #5925, #4278 ),
 ( #99963, #107271, #31114, #65843, #37876, #74250 ),
 ( #64193, #65294, #5365, #30566, #90463, #98867 ),
 ( #108381, #82060, #39525, #107826, #81502, #99407 ) ),
 .UNSPECIFIED., .F., .F., .F.,
 ( 6, 3, 3, 6 ),
 ( 6, 6 ),
 ( 31.55396738929999856, 52.61810161070000191, 100.7782915239999966, 170.0026156580000247 ),
 ( 0.000000000000000000, 2.000000002120000175 ),
 .UNSPECIFIED. ) ;
#48189 = CARTESIAN_POINT ( 'NONE',  ( -9.123030677640000974, 1385.451960981700040, 199.9749920654289781 ) ) ;
#48190 = CARTESIAN_POINT ( 'NONE',  ( 20.17014401999999862, 1476.180243796189870, 211.1081103605989995 ) ) ;
#48192 = EDGE_LOOP ( 'NONE', ( #22462, #14593, #83379, #63983, #103758, #102708, #33331, #30786 ) ) ;
#48191 = CARTESIAN_POINT ( 'NONE',  ( 11.30832794868720015, 1425.224311524470068, 202.9888470784990204 ) ) ;
#48193 = CARTESIAN_POINT ( 'NONE',  ( 4.198346516710000031, 1429.752558846089869, 216.7561471261590214 ) ) ;
#48194 = CARTESIAN_POINT ( 'NONE',  ( -2.500000048262839947, 1439.241542145249923, 157.7315144758069891 ) ) ;
#48195 = AXIS2_PLACEMENT_3D ( 'NONE', #2377, #11308, #37040 ) ;
#48196 = DIRECTION ( 'NONE',  ( 2.041467857569999829E-16, -1.000000000000000000, 5.573852046271030309E-16 ) ) ;
#48197 = CARTESIAN_POINT ( 'NONE',  ( 11.54535135419999925, 1433.804361866699992, 151.2566013386979762 ) ) ;
#48198 = CARTESIAN_POINT ( 'NONE',  ( 31.70762145559999468, 1463.873751786229832, 271.1218459616979999 ) ) ;
#48199 = B_SPLINE_SURFACE_WITH_KNOTS ( 'NONE', 5, 5, ( 
 ( #103979, #79346, #62014, #46863, #36232, #27275 ),
 ( #12683, #61458, #53049, #63134, #78790, #95584 ),
 ( #106193, #46322, #71539, #37342, #2659, #2106 ),
 ( #104537, #36785, #80993, #44648, #88844, #70978 ),
 ( #80450, #3763, #105094, #88293, #105660, #37897 ),
 ( #63670, #96134, #29475, #72079, #28945, #97235 ),
 ( #70419, #79900, #27834, #28384, #4299, #19413 ),
 ( #62585, #53614, #97781, #21058, #96702, #11587 ),
 ( #55263, #87756, #89394, #20508, #54167, #45765 ) ),
 .UNSPECIFIED., .F., .F., .F.,
 ( 6, 3, 6 ),
 ( 6, 6 ),
 ( 4.283793212480669688, 5.549035871040000067, 6.814275327763410495 ),
 ( -0.0004314831893375249629, 2.000000000000000000 ),
 .UNSPECIFIED. ) ;
#48200 = CARTESIAN_POINT ( 'NONE',  ( 3.719802410872147913, 1370.319534414420104, 210.0106693369416178 ) ) ;
#48201 = CARTESIAN_POINT ( 'NONE',  ( -41.66135440509999910, 1443.796918820770088, 135.6885369501979994 ) ) ;
#48202 = CARTESIAN_POINT ( 'NONE',  ( -109.4000724753198170, 1387.258595658028071, 297.3646005980954783 ) ) ;
#48203 = CARTESIAN_POINT ( 'NONE',  ( 15.64949383239999925, 1417.427322289930089, 227.4411827007979809 ) ) ;
#48204 = EDGE_CURVE ( 'NONE', #98270, #13874, #66951, .T. ) ;
#48205 = CARTESIAN_POINT ( 'NONE',  ( -31.93049531883793790, 1525.394081235439444, 201.2251851172232762 ) ) ;
#48206 = CARTESIAN_POINT ( 'NONE',  ( 0.000000000000000000, 1524.090675761330203, 209.1218459616979999 ) ) ;
#48207 = CARTESIAN_POINT ( 'NONE',  ( 17.74184486700000107, 1415.163755984130148, 210.1742778932080000 ) ) ;
#48208 = CARTESIAN_POINT ( 'NONE',  ( -7.898270967410000232, 1498.870872765589866, 219.0971900149289979 ) ) ;
#48209 = AXIS2_PLACEMENT_3D ( 'NONE', #48483, #65283, #33297 ) ;
#48210 = CARTESIAN_POINT ( 'NONE',  ( -1.340879483539999750, 1420.508801203329995, 228.2428596365979843 ) ) ;
#48211 = CARTESIAN_POINT ( 'NONE',  ( 3.406070268200000140, 1459.762959874990202, 203.0322602957690208 ) ) ;
#48212 = CARTESIAN_POINT ( 'NONE',  ( -16.63038760358159962, 1409.493779246939994, 193.2365068857160111 ) ) ;
#48213 = CARTESIAN_POINT ( 'NONE',  ( -0.7244299514709989785, 1515.369718807090067, 204.8338105401389839 ) ) ;
#48214 = CYLINDRICAL_SURFACE ( 'NONE', #8376, 1.999999999999999556 ) ;
#48215 = CARTESIAN_POINT ( 'NONE',  ( -204.2714532754873744, 1524.382868172863937, 223.7095399770903725 ) ) ;
#48216 = CARTESIAN_POINT ( 'NONE',  ( -1.487490402750000218, 1415.934222462230082, 227.8159478362979939 ) ) ;
#48217 = CARTESIAN_POINT ( 'NONE',  ( 0.2162845618075959764, 1453.832447077659936, 183.2176829081640221 ) ) ;
#48218 = CARTESIAN_POINT ( 'NONE',  ( -13.47229708513430069, 1408.353351118039882, 210.5674428809980157 ) ) ;
#48219 = CARTESIAN_POINT ( 'NONE',  ( -14.85820445100000065, 1414.971262582530017, 201.3187579297980108 ) ) ;
#48220 = EDGE_CURVE ( 'NONE', #911, #83491, #54939, .T. ) ;
#48221 = CARTESIAN_POINT ( 'NONE',  ( -0.3977757332677263613, 1484.209072442955403, 198.4342325285878985 ) ) ;
#48222 = CARTESIAN_POINT ( 'NONE',  ( 12.40441713279999902, 1434.419921576160050, 147.2730273303979800 ) ) ;
#48223 = CARTESIAN_POINT ( 'NONE',  ( -3483.362668188789939, 1009.280138338860070, 1152.220656836879698 ) ) ;
#48224 = PLANE ( 'NONE',  #30034 ) ;
#48225 = ORIENTED_EDGE ( 'NONE', *, *, #83167, .T. ) ;
#48226 = CARTESIAN_POINT ( 'NONE',  ( -1.516559207410000054, 1485.748721136590120, 197.3030500067990261 ) ) ;
#48227 = CARTESIAN_POINT ( 'NONE',  ( 8.518975719829999349, 1479.750272970590004, 202.8267940536090066 ) ) ;
#48228 = CARTESIAN_POINT ( 'NONE',  ( -103.5788295108265231, 1379.883385647208115, 304.1094550558439664 ) ) ;
#48229 = CARTESIAN_POINT ( 'NONE',  ( -12.12815397179999977, 1490.956868768189906, 207.2466138458389935 ) ) ;
#48230 = CARTESIAN_POINT ( 'NONE',  ( -1.216112039750000040, 1452.488429528330016, 183.6485174699979837 ) ) ;
#48231 = CARTESIAN_POINT ( 'NONE',  ( 13.63492191947259968, 1509.148412430130065, 233.7524217023999995 ) ) ;
#48232 = CARTESIAN_POINT ( 'NONE',  ( 41.05947484210914666, 1425.981672987238881, 269.1009201124458627 ) ) ;
#48233 = CARTESIAN_POINT ( 'NONE',  ( -17.83486663330467437, 1523.678648413191695, 237.8759530894961642 ) ) ;
#48234 = CARTESIAN_POINT ( 'NONE',  ( 20.17495589095351605, 1508.361608986149804, 189.3322755138515276 ) ) ;
#48235 = CARTESIAN_POINT ( 'NONE',  ( 2.660639375519999739, 1425.975332079029840, 184.4015672484980257 ) ) ;
#48236 = CARTESIAN_POINT ( 'NONE',  ( -64.28120925927808571, 1385.082940760139991, 253.4381211720830436 ) ) ;
#48237 = CARTESIAN_POINT ( 'NONE',  ( -12.15078451844060048, 1490.894239016419988, 207.4451287176520111 ) ) ;
#48238 = CARTESIAN_POINT ( 'NONE',  ( -4.476507717933579933, 1508.551704408389924, 205.1212419221770062 ) ) ;
#48239 = CARTESIAN_POINT ( 'NONE',  ( -27.28818755810000241, 1451.506600565129929, 136.1456173926979716 ) ) ;
#48240 = CARTESIAN_POINT ( 'NONE',  ( -16.44809876050000241, 1409.864299044730160, 226.1127107795979896 ) ) ;
#48242 = ORIENTED_EDGE ( 'NONE', *, *, #99362, .T. ) ;
#48241 = CARTESIAN_POINT ( 'NONE',  ( 0.4944968420529889386, 1416.123307786990154, 184.8232262612689851 ) ) ;
#48243 = CARTESIAN_POINT ( 'NONE',  ( -109.8253977639999874, 1384.918085983840001, 311.3807728672589406 ) ) ;
#48244 = CARTESIAN_POINT ( 'NONE',  ( 9.673908127945217927, 1470.479523918640098, 212.0206101308270092 ) ) ;
#48245 = CARTESIAN_POINT ( 'NONE',  ( -19.21422196745478672, 1410.945657666566831, 222.5551157027674947 ) ) ;
#48246 = CARTESIAN_POINT ( 'NONE',  ( -109.8216762179999932, 1384.604528214259744, 311.3701024542589835 ) ) ;
#48247 = CARTESIAN_POINT ( 'NONE',  ( -0.07319975326350189326, 1420.201854830530237, 183.6697168662389856 ) ) ;
#48248 = CARTESIAN_POINT ( 'NONE',  ( 0.6994960599189999906, 1465.970851562730104, 235.7517331751979839 ) ) ;
#48249 = AXIS2_PLACEMENT_3D ( 'NONE', #28385, #19414, #95036 ) ;
#48250 = EDGE_CURVE ( 'NONE', #98647, #25318, #38950, .T. ) ;
#48251 = CARTESIAN_POINT ( 'NONE',  ( 22.01146773749999852, 1410.176833643329928, 215.5333753336580003 ) ) ;
#48252 = CARTESIAN_POINT ( 'NONE',  ( -2.187094087082049665, 1417.224187196630055, 186.0756805202190094 ) ) ;
#48253 = CARTESIAN_POINT ( 'NONE',  ( -20.39463414511109818, 1465.749978440089990, 211.0547928264969926 ) ) ;
#48254 = CARTESIAN_POINT ( 'NONE',  ( -16.69877117700000113, 1422.038596365629928, 226.9905822485980025 ) ) ;
#48256 = CARTESIAN_POINT ( 'NONE',  ( 22.03054413761287833, 1506.491018781251569, 209.0051989547683320 ) ) ;
#48255 = CARTESIAN_POINT ( 'NONE',  ( -4.936086582586449722, 1511.397679222030092, 200.6202249550506167 ) ) ;
#48257 = CARTESIAN_POINT ( 'NONE',  ( 26.29932063603849812, 1469.338010392229990, 207.9704851390930003 ) ) ;
#48258 = CARTESIAN_POINT ( 'NONE',  ( -100.1346419727999688, 1320.102705746890024, 290.9564879300593248 ) ) ;
#48259 = CYLINDRICAL_SURFACE ( 'NONE', #109839, 0.5000000000000022204 ) ;
#48260 = CARTESIAN_POINT ( 'NONE',  ( -23.98763429770000144, 1430.797664492329886, 210.9021853213379813 ) ) ;
#48261 = CARTESIAN_POINT ( 'NONE',  ( -5.439576477476709471, 1374.913517049739994, 203.3383520319619890 ) ) ;
#48262 = EDGE_CURVE ( 'NONE', #72816, #30026, #71771, .T. ) ;
#48263 = CARTESIAN_POINT ( 'NONE',  ( 4.997573787194999895, 1516.742629295279812, 205.6633194342169872 ) ) ;
#48264 = CARTESIAN_POINT ( 'NONE',  ( -17.73406580063780069, 1423.343214054229975, 226.1884525926029994 ) ) ;
#48265 = ORIENTED_EDGE ( 'NONE', *, *, #47656, .F. ) ;
#48266 = CARTESIAN_POINT ( 'NONE',  ( 3.350944662710000355, 1464.628126271390101, 199.8699733667390035 ) ) ;
#48267 = CARTESIAN_POINT ( 'NONE',  ( -4.221578081139290006, 1441.603993731499941, 169.6114286483189915 ) ) ;
#48269 = VERTEX_POINT ( 'NONE', #104224 ) ;
#48268 = CARTESIAN_POINT ( 'NONE',  ( -68.29419003885790573, 1379.746815713430124, 279.8507461170009947 ) ) ;
#48270 = EDGE_CURVE ( 'NONE', #93372, #5163, #53677, .T. ) ;
#48271 = VERTEX_POINT ( 'NONE', #86868 ) ;
#48272 = CARTESIAN_POINT ( 'NONE',  ( -8.214667976841889541, 1382.175473383424332, 218.4482751763555370 ) ) ;
#48273 = VERTEX_POINT ( 'NONE', #10727 ) ;
#48274 = CARTESIAN_POINT ( 'NONE',  ( -3.614223185717699405, 1512.187213306747481, 237.6097657867471469 ) ) ;
#48275 = CARTESIAN_POINT ( 'NONE',  ( 11.44311714350000031, 1501.817457610490237, 208.4257029495360030 ) ) ;
#48276 = CARTESIAN_POINT ( 'NONE',  ( 15.80576494213290317, 1409.464993575840026, 192.9618696935270066 ) ) ;
#48277 = CARTESIAN_POINT ( 'NONE',  ( 0.7559394982620020187, 1516.972341476009888, 210.2438793621770117 ) ) ;
#48278 = AXIS2_PLACEMENT_3D ( 'NONE', #9158, #35456, #102628 ) ;
#48279 = CARTESIAN_POINT ( 'NONE',  ( -107.0358864074350009, 1378.913060387289988, 307.2354898942079444 ) ) ;
#48280 = CARTESIAN_POINT ( 'NONE',  ( -3.208637253543818346, 1515.551704408389696, 212.9514661164405709 ) ) ;
#48281 = CARTESIAN_POINT ( 'NONE',  ( 8.197264105214189911, 1483.021012307500087, 216.7088607698530041 ) ) ;
#48282 = PRODUCT_CONTEXT ( 'NONE', #57061, 'mechanical' ) ;
#48283 = PRODUCT ( 'Cutting Blade', 'Cutting Blade', '', ( #58327 ) ) ;
#48284 = CARTESIAN_POINT ( 'NONE',  ( 36.33941889804810188, 1451.266910394200067, 134.0999999986779869 ) ) ;
#48285 = DIRECTION ( 'NONE',  ( 0.03489949670246784291, -0.9993908270190968723, 0.000000000000000000 ) ) ;
#48286 = CARTESIAN_POINT ( 'NONE',  ( 10.59813991459999905, 1477.524080022390081, 229.9254213492990004 ) ) ;
#48287 = CIRCLE ( 'NONE', #62627, 7.999657266239995401 ) ;
#48288 = CARTESIAN_POINT ( 'NONE',  ( -18.16246261389999717, 1458.250829203630019, 228.1248121254980106 ) ) ;
#48289 = EDGE_LOOP ( 'NONE', ( #32134, #86789, #15457, #85973, #95925 ) ) ;
#48290 = ORIENTED_EDGE ( 'NONE', *, *, #37186, .F. ) ;
#48291 = CARTESIAN_POINT ( 'NONE',  ( -7.014484281215001005, 1513.886778334009932, 216.7648687176869942 ) ) ;
#48292 = CARTESIAN_POINT ( 'NONE',  ( 16.55311983492223504, 1514.160701262335579, 194.8748343058166199 ) ) ;
#48293 = CARTESIAN_POINT ( 'NONE',  ( 12.42784828245430084, 1499.940815291620083, 206.6466454406019864 ) ) ;
#48294 = CARTESIAN_POINT ( 'NONE',  ( -3.428224537170000197, 1485.815345808829989, 182.6034298983980193 ) ) ;
#48295 = CARTESIAN_POINT ( 'NONE',  ( -2.500000000000000000, 1439.534676059920230, 164.5282244803989897 ) ) ;
#48296 = ADVANCED_FACE ( 'NONE', ( #61698 ), #79589, .F. ) ;
#48297 = TOROIDAL_SURFACE ( 'NONE', #8, 14.91144628110000170, 0.5000000000000000000 ) ;
#48298 = CARTESIAN_POINT ( 'NONE',  ( -2.620401159595308727, 1523.462669333491021, 242.1631858338596146 ) ) ;
#48299 = CARTESIAN_POINT ( 'NONE',  ( 12.54251639656375161, 1420.481606446594924, 200.4267854580531889 ) ) ;
#48300 = CARTESIAN_POINT ( 'NONE',  ( 0.8889729592620010390, 1465.607921463989896, 198.1135291515989820 ) ) ;
#48301 = CARTESIAN_POINT ( 'NONE',  ( 26.84000533130000221, 1441.581970243590149, 137.4710795520979900 ) ) ;
#48302 = ADVANCED_FACE ( 'NONE', ( #106426 ), #14055, .T. ) ;
#48303 = CARTESIAN_POINT ( 'NONE',  ( 1.241868258699999839, 1415.088275290029969, 191.2755884483979969 ) ) ;
#48304 = CARTESIAN_POINT ( 'NONE',  ( -81.95025445411960163, 1384.803819859970190, 285.5341702218789806 ) ) ;
#48305 = ORIENTED_EDGE ( 'NONE', *, *, #37265, .T. ) ;
#48306 = CARTESIAN_POINT ( 'NONE',  ( 3.454172615424999648, 1517.122088787240045, 201.3974225380069925 ) ) ;
#48307 = CARTESIAN_POINT ( 'NONE',  ( 3.253301381255000013, 1516.790374942449944, 207.9863856151469861 ) ) ;
#48308 = ORIENTED_EDGE ( 'NONE', *, *, #92582, .F. ) ;
#48309 = CARTESIAN_POINT ( 'NONE',  ( 37.22778720889070314, 1440.913060387330006, 263.9590491429840426 ) ) ;
#48310 = CARTESIAN_POINT ( 'NONE',  ( -0.0002512067421216920273, 1452.090905546908516, 153.9203152429142563 ) ) ;
#48311 = ORIENTED_EDGE ( 'NONE', *, *, #89334, .F. ) ;
#48312 = CARTESIAN_POINT ( 'NONE',  ( 0.03339020944234569882, 1451.699590288030095, 183.0337632313120082 ) ) ;
#48313 = CARTESIAN_POINT ( 'NONE',  ( 3.885417831612716366, 1424.874073124720098, 216.2340555961886821 ) ) ;
#48314 = CARTESIAN_POINT ( 'NONE',  ( -109.0682564771375098, 1384.413434012951711, 311.2315974213690311 ) ) ;
#48315 = B_SPLINE_CURVE_WITH_KNOTS ( 'NONE', 5,
 ( #13575, #109330, #23649, #38795, #14696, #22514, #100889, #24184, #74627, #92499, #72970, #48329 ),
 .UNSPECIFIED., .F., .F.,
 ( 6, 3, 3, 6 ),
 ( 0.000000000000000000, 0.2203430568107523080, 0.6610070094751656633, 1.000000000000000000 ),
 .UNSPECIFIED. ) ;
#48316 = CARTESIAN_POINT ( 'NONE',  ( -10.98772071141650031, 1462.627874614629945, 207.9149163331969987 ) ) ;
#48317 = CARTESIAN_POINT ( 'NONE',  ( 21.38516915557987375, 1512.187213306747481, 237.8497028174237471 ) ) ;
#48318 = CARTESIAN_POINT ( 'NONE',  ( -5.556441586205710159, 1511.478393686179970, 200.7426215012330033 ) ) ;
#48319 = CARTESIAN_POINT ( 'NONE',  ( -3.549608490489999824, 1507.276797643229884, 180.9704965481979855 ) ) ;
#48320 = CARTESIAN_POINT ( 'NONE',  ( -6.150246140235383407, 1510.808998927847597, 201.6520066974360077 ) ) ;
#48321 = CARTESIAN_POINT ( 'NONE',  ( -19.90023153800462552, 1526.278758871497530, 182.9652379492368652 ) ) ;
#48323 = DIRECTION ( 'NONE',  ( 0.03489949670250328678, -0.9993908270190956511, 0.000000000000000000 ) ) ;
#48322 = CARTESIAN_POINT ( 'NONE',  ( 13.91727111200000166, 1462.334475154630127, 230.6050055265979779 ) ) ;
#48324 = CARTESIAN_POINT ( 'NONE',  ( -0.5133638609672289688, 1410.311096993930050, 233.1717005261690190 ) ) ;
#48325 = AXIS2_PLACEMENT_3D ( 'NONE', #12937, #47118, #39247 ) ;
#48326 = B_SPLINE_SURFACE_WITH_KNOTS ( 'NONE', 5, 5, ( 
 ( #90009, #48587, #56986, #99498, #48024, #82721 ),
 ( #5460, #82161, #31757, #72683, #22781, #4904 ),
 ( #12762, #107914, #57544, #89468, #6011, #108473 ),
 ( #55336, #91667, #47478, #91117, #56429, #39620 ),
 ( #30097, #106807, #64292, #39043, #46942, #22230 ),
 ( #65393, #14393, #30663, #40164, #74346, #81061 ),
 ( #81600, #64848, #4375, #21684, #38505, #98412 ),
 ( #55890, #13286, #20402, #46754, #3102, #29362 ),
 ( #105543, #11481, #4181, #104982, #38314, #70314 ),
 ( #104428, #46203, #72493, #37231, #28272, #44533 ),
 ( #87641, #106084, #19859, #80337, #89277, #62465 ),
 ( #61907, #96587, #96025, #80885, #78678, #37783 ) ),
 .UNSPECIFIED., .F., .F., .F.,
 ( 6, 3, 3, 6 ),
 ( 6, 6 ),
 ( 3.686514310890000257, 6.076675143290000136, 7.815970586859999791, 8.927001670199999239 ),
 ( 0.000000000000000000, 1.000000000000000000 ),
 .UNSPECIFIED. ) ;
#48327 = CARTESIAN_POINT ( 'NONE',  ( -6.941727290454999810, 1516.882217593000178, 216.4530290611770056 ) ) ;
#48328 = ORIENTED_EDGE ( 'NONE', *, *, #44360, .T. ) ;
#48329 = CARTESIAN_POINT ( 'NONE',  ( -22.57319772750419773, 1409.701314710050156, 209.4509374963450057 ) ) ;
#48330 = CARTESIAN_POINT ( 'NONE',  ( -0.1280106238597930046, 1507.928448683369879, 180.6911020812059689 ) ) ;
#48331 = CARTESIAN_POINT ( 'NONE',  ( -2.478306858074999841, 1516.938330505699923, 212.5844667883370107 ) ) ;
#48332 = CARTESIAN_POINT ( 'NONE',  ( 3.829222805974359822, 1515.551704203360032, 211.9228896269929976 ) ) ;
#48333 = DIRECTION ( 'NONE',  ( -0.000000000000000000, -1.000000000000000000, -0.000000000000000000 ) ) ;
#48335 = ORIENTED_EDGE ( 'NONE', *, *, #58223, .F. ) ;
#48334 = CARTESIAN_POINT ( 'NONE',  ( 3.487584104944840391, 1508.551704408389924, 214.1089243997540166 ) ) ;
#48336 = DIRECTION ( 'NONE',  ( 0.000000000000000000, -1.000000000000000000, 0.000000000000000000 ) ) ;
#48337 = AXIS2_PLACEMENT_3D ( 'NONE', #71449, #62488, #53517 ) ;
#48338 = CARTESIAN_POINT ( 'NONE',  ( 11.62345946000000119, 1459.569834436530073, 221.5884500235979999 ) ) ;
#48339 = CARTESIAN_POINT ( 'NONE',  ( -10.94036871930000032, 1430.241478036630042, 151.4665561441980230 ) ) ;
#48340 = LINE ( 'NONE', #74638, #39675 ) ;
#48341 = CARTESIAN_POINT ( 'NONE',  ( -8.922484925833558123, 1440.999120902360119, 204.4963729060849857 ) ) ;
#48342 = CARTESIAN_POINT ( 'NONE',  ( 3.181555627136920084, 1425.362660434019972, 153.9433711340520290 ) ) ;
#48343 = DIRECTION ( 'NONE',  ( 0.000000000000000000, -0.02617694830788849791, -0.9996573249755569268 ) ) ;
#48344 = CARTESIAN_POINT ( 'NONE',  ( 12.59782697949999886, 1446.921545761879770, 188.3055334180980083 ) ) ;
#48346 = CARTESIAN_POINT ( 'NONE',  ( -10.22049849524720067, 1480.811388884020062, 206.5019967615200187 ) ) ;
#48345 = CARTESIAN_POINT ( 'NONE',  ( -19.18209465460000018, 1457.448691500030009, 226.5728852009980017 ) ) ;
#48347 = CARTESIAN_POINT ( 'NONE',  ( 6.596949724929999981, 1463.298537539390054, 209.1528258517670054 ) ) ;
#48348 = ORIENTED_EDGE ( 'NONE', *, *, #17290, .F. ) ;
#48349 = CARTESIAN_POINT ( 'NONE',  ( 3.448206878685000198, 1516.904492006980036, 205.0794281543969646 ) ) ;
#48350 = CARTESIAN_POINT ( 'NONE',  ( 3.713169866679999931, 1406.888986113030114, 269.6455940986979840 ) ) ;
#48351 = CARTESIAN_POINT ( 'NONE',  ( 0.1681183307230000035, 1408.918931226930226, 186.0198301081979935 ) ) ;
#48352 = CARTESIAN_POINT ( 'NONE',  ( 17.99612260190000157, 1410.880106602829983, 193.4662733174980076 ) ) ;
#48353 = CARTESIAN_POINT ( 'NONE',  ( 22.64711134129722225, 1431.381828419114072, 216.8252444415483922 ) ) ;
#48354 = CARTESIAN_POINT ( 'NONE',  ( 21.83550407203919974, 1523.678648413191695, 234.9693198511250785 ) ) ;
#48355 = CARTESIAN_POINT ( 'NONE',  ( 26.88907266892866943, 1508.006188459404939, 215.2210763183871052 ) ) ;
#48356 = CARTESIAN_POINT ( 'NONE',  ( -7.948879223625117341, 1438.924303876842714, 205.5137112676434299 ) ) ;
#48357 = CARTESIAN_POINT ( 'NONE',  ( -1.967245096925249737, 1450.337415777349861, 154.7913169777050086 ) ) ;
#48358 = FACE_OUTER_BOUND ( 'NONE', #47466, .T. ) ;
#48359 = CARTESIAN_POINT ( 'NONE',  ( 1.181727162679999887, 1450.812795825049989, 155.6080914332980001 ) ) ;
#48360 = CARTESIAN_POINT ( 'NONE',  ( -14.43876446305799988, 1416.576002138890090, 221.3723411449140031 ) ) ;
#48361 = CARTESIAN_POINT ( 'NONE',  ( -4.325405444010000267, 1515.219201233190006, 210.9648094371690092 ) ) ;
#48362 = B_SPLINE_CURVE_WITH_KNOTS ( 'NONE', 5,
 ( #1799, #35936, #70121, #63903, #39783, #99112 ),
 .UNSPECIFIED., .F., .F.,
 ( 6, 6 ),
 ( 0.4226397637529890061, 0.4682762820520000036 ),
 .UNSPECIFIED. ) ;
#48363 = VECTOR ( 'NONE', #61506, 1000.000000000000000 ) ;
#48364 = CARTESIAN_POINT ( 'NONE',  ( -19.62446893450000118, 1438.771933937510084, 214.3676144203579952 ) ) ;
#48365 = CARTESIAN_POINT ( 'NONE',  ( -26.88341108264370050, 1508.006303180540044, 211.8628327196680061 ) ) ;
#48366 = FACE_OUTER_BOUND ( 'NONE', #20551, .T. ) ;
#48367 = CARTESIAN_POINT ( 'NONE',  ( -6.133610941629999758, 1475.021496988630133, 269.4856170435980403 ) ) ;
#48368 = CARTESIAN_POINT ( 'NONE',  ( -4.237127966724729689, 1446.355013308460002, 163.3938685498860366 ) ) ;
#48369 = LINE ( 'NONE', #14183, #33394 ) ;
#48370 = CARTESIAN_POINT ( 'NONE',  ( -11.39147210054831305, 1486.510883767746691, 184.0968824713255856 ) ) ;
#48371 = CARTESIAN_POINT ( 'NONE',  ( -42.31304661141189882, 1384.776936385030012, 246.3345890605239958 ) ) ;
#48372 = CARTESIAN_POINT ( 'NONE',  ( -106.5026996092109925, 1391.913060387289988, 303.1716863602470085 ) ) ;
#48373 = CIRCLE ( 'NONE', #68046, 1.999999999999990452 ) ;
#48374 = CARTESIAN_POINT ( 'NONE',  ( -3.669386717783980068, 1517.051704642929963, 215.6629163041010031 ) ) ;
#48375 = B_SPLINE_CURVE_WITH_KNOTS ( 'NONE', 3,
 ( #41785, #33370, #67564, #24957, #25514, #59166, #77059, #26063, #60258, #29388, #61382 ),
 .UNSPECIFIED., .F., .F.,
 ( 4, 2, 1, 2, 2, 4 ),
 ( 0.000000000000000000, 0.2500000000007147616, 0.3750000000009557910, 0.4375000000011197709, 0.5000000000012837509, 1.000000000000000000 ),
 .UNSPECIFIED. ) ;
#48376 = CARTESIAN_POINT ( 'NONE',  ( 12.09325773686249939, 1491.439490036820189, 206.9352952286269840 ) ) ;
#48377 = CARTESIAN_POINT ( 'NONE',  ( -20.21716934225085183, 1526.104292489130103, 184.5497256588658672 ) ) ;
#48378 = CARTESIAN_POINT ( 'NONE',  ( 8.520846174749847179, 1511.399999645683920, 204.1281607283802089 ) ) ;
#48379 = CARTESIAN_POINT ( 'NONE',  ( -18.87340472369999844, 1410.495304298229939, 196.4667987001980123 ) ) ;
#48380 = CARTESIAN_POINT ( 'NONE',  ( -15.03298775838899992, 1422.459395939136130, 229.1221294577470076 ) ) ;
#48381 = CARTESIAN_POINT ( 'NONE',  ( 11.14671379024469999, 1434.019377051509991, 151.6529839732360188 ) ) ;
#48382 = EDGE_CURVE ( 'NONE', #66538, #11383, #8206, .T. ) ;
#48383 = ORIENTED_EDGE ( 'NONE', *, *, #81902, .T. ) ;
#48384 = DIRECTION ( 'NONE',  ( 0.000000000000000000, 1.000000000000000000, -0.000000000000000000 ) ) ;
#48385 = CARTESIAN_POINT ( 'NONE',  ( -7.458082279446967888, 1510.848430437142952, 215.3131282273689919 ) ) ;
#48386 = CARTESIAN_POINT ( 'NONE',  ( 18.68390456912029762, 1457.534965337250014, 220.6831945509709954 ) ) ;
#48388 = CARTESIAN_POINT ( 'NONE',  ( -12.16190383725469992, 1378.259213814440045, 211.1523455089300114 ) ) ;
#48387 = CARTESIAN_POINT ( 'NONE',  ( -15.98290998149800046, 1416.244087889359889, 209.6359233886850006 ) ) ;
#48389 = CARTESIAN_POINT ( 'NONE',  ( 16.57695357295475347, 1524.524650307243292, 237.5563529681140835 ) ) ;
#48390 = CARTESIAN_POINT ( 'NONE',  ( 11.89909614660000159, 1409.328585981029846, 191.4548601458980102 ) ) ;
#48391 = CARTESIAN_POINT ( 'NONE',  ( -8.170885357179999531, 1451.453810839889911, 203.6936318906290069 ) ) ;
#48392 = VECTOR ( 'NONE', #67256, 1000.000000000000000 ) ;
#48393 = CARTESIAN_POINT ( 'NONE',  ( -5.780861274184998955, 1516.783701990830195, 202.1826264492970324 ) ) ;
#48394 = CARTESIAN_POINT ( 'NONE',  ( 7.363774774100000364, 1426.339825040939786, 212.6604317995690110 ) ) ;
#48395 = CARTESIAN_POINT ( 'NONE',  ( -11.34254097917190585, 1398.249336051535238, 202.7613412656716037 ) ) ;
#48396 = CARTESIAN_POINT ( 'NONE',  ( 15.46640438443499832, 1511.810036768419877, 197.0767216879669945 ) ) ;
#48397 = FACE_BOUND ( 'NONE', #18115, .T. ) ;
#48398 = CARTESIAN_POINT ( 'NONE',  ( -18.76552339101630196, 1380.296266887499996, 210.4014709065379805 ) ) ;
#48399 = CARTESIAN_POINT ( 'NONE',  ( 2.864888263985923444, 1368.214942817532346, 207.6218459616988241 ) ) ;
#48401 = EDGE_LOOP ( 'NONE', ( #13952, #82778, #109245, #16248 ) ) ;
#48400 = CARTESIAN_POINT ( 'NONE',  ( -21.79878488383639734, 1379.715451835960039, 213.3535203440429768 ) ) ;
#48402 = VERTEX_POINT ( 'NONE', #27512 ) ;
#48403 = EDGE_CURVE ( 'NONE', #70982, #102300, #55191, .T. ) ;
#48404 = CARTESIAN_POINT ( 'NONE',  ( 0.001991325594910000121, 1395.912990848730033, 220.4358217525980024 ) ) ;
#48405 = CARTESIAN_POINT ( 'NONE',  ( -18.77065511170000178, 1409.568546107730072, 220.1541561005979872 ) ) ;
#48406 = DIRECTION ( 'NONE',  ( 0.9386936612375377242, 0.3031620644484189775, 0.1641553320237859603 ) ) ;
#48407 = CARTESIAN_POINT ( 'NONE',  ( -12.66067528227170946, 1445.026872531248500, 169.4635260004347970 ) ) ;
#48408 = CARTESIAN_POINT ( 'NONE',  ( 21.81321449130158285, 1509.707650915029944, 229.2662883381179029 ) ) ;
#48409 = CARTESIAN_POINT ( 'NONE',  ( -9.491012693391989759E-16, 1374.413060387289988, 209.1218459616989946 ) ) ;
#48411 = CARTESIAN_POINT ( 'NONE',  ( -21.52452246478599918, 1505.819333768819888, 209.2233725332250174 ) ) ;
#48410 = CARTESIAN_POINT ( 'NONE',  ( 2.551450060280000098, 1445.555848560289860, 200.0930493208989844 ) ) ;
#48412 = CIRCLE ( 'NONE', #105633, 2.000015520878148934 ) ;
#48413 = CARTESIAN_POINT ( 'NONE',  ( -30.61443310214375657, 1523.462669333491476, 196.4193608261409452 ) ) ;
#48414 = DIRECTION ( 'NONE',  ( -0.6736849260863839728, 0.000000000000000000, 0.7390186874254150995 ) ) ;
#48415 = EDGE_CURVE ( 'NONE', #28591, #81651, #32225, .T. ) ;
#48416 = CARTESIAN_POINT ( 'NONE',  ( 4.647212535750000484, 1424.553094292009973, 191.7362356993989749 ) ) ;
#48417 = PRESENTATION_STYLE_ASSIGNMENT (( #48971 ) ) ;
#48418 = CARTESIAN_POINT ( 'NONE',  ( 9.437563379819911447, 1396.242627386850018, 203.3496504048309816 ) ) ;
#48419 = CARTESIAN_POINT ( 'NONE',  ( 1.352297191989999980, 1415.128105759529944, 191.2895120243979932 ) ) ;
#48420 = CARTESIAN_POINT ( 'NONE',  ( 11.25794562449999958, 1429.128833963630086, 150.7790970959979973 ) ) ;
#48421 = CARTESIAN_POINT ( 'NONE',  ( 8.371228001764999149, 1512.069761553110084, 202.7380249772070044 ) ) ;
#48422 = ORIENTED_EDGE ( 'NONE', *, *, #37258, .T. ) ;
#48423 = CARTESIAN_POINT ( 'NONE',  ( 13.56071599880170098, 1435.044469485500031, 149.3995586837050098 ) ) ;
#48424 = CARTESIAN_POINT ( 'NONE',  ( 22.08327125186925954, 1523.604703353109699, 184.4267662568470598 ) ) ;
#48425 = B_SPLINE_CURVE_WITH_KNOTS ( 'NONE', 3,
 ( #98213, #29898, #64091, #4173, #21481, #89815 ),
 .UNSPECIFIED., .F., .F.,
 ( 4, 2, 4 ),
 ( -1.285435071114495078E-05, 0.001079388306740513117, 0.002171630964192170898 ),
 .UNSPECIFIED. ) ;
#48426 = ORIENTED_EDGE ( 'NONE', *, *, #34451, .T. ) ;
#48427 = ORIENTED_EDGE ( 'NONE', *, *, #74340, .F. ) ;
#48428 = DIRECTION ( 'NONE',  ( 0.000000000000000000, 0.000000000000000000, -1.000000000000000000 ) ) ;
#48429 = CARTESIAN_POINT ( 'NONE',  ( -13.53625262109999916, 1461.948139420029975, 230.2268504220980105 ) ) ;
#48430 = CARTESIAN_POINT ( 'NONE',  ( -108.4919463386471818, 1388.455631213034849, 310.4216145322829448 ) ) ;
#48431 = CARTESIAN_POINT ( 'NONE',  ( 30.51126001304307067, 1526.382868172863937, 198.3878992055866775 ) ) ;
#48432 = CARTESIAN_POINT ( 'NONE',  ( 0.7543881828220019292, 1516.727502608469877, 215.6727161143369926 ) ) ;
#48433 = CARTESIAN_POINT ( 'NONE',  ( -12.63851992163809967, 1379.319802075649932, 208.7650603020850042 ) ) ;
#48434 = ORIENTED_EDGE ( 'NONE', *, *, #10525, .T. ) ;
#48435 = CARTESIAN_POINT ( 'NONE',  ( -12.78956172709999883, 1502.763085786289821, 208.8827437375920226 ) ) ;
#48436 = CARTESIAN_POINT ( 'NONE',  ( -11.77320467545210114, 1509.437369347079994, 181.3954167328170115 ) ) ;
#48437 = CARTESIAN_POINT ( 'NONE',  ( -41.40570855549999862, 1380.117442312619914, 227.6002677670589947 ) ) ;
#48438 =( BOUNDED_CURVE ( )  B_SPLINE_CURVE ( 3, ( #16899, #34286, #51652, #100392 ),
 .UNSPECIFIED., .F., .F. ) 
 B_SPLINE_CURVE_WITH_KNOTS ( ( 4, 4 ),
 ( 3.141592653589793116, 4.712388980384689674 ),
 .UNSPECIFIED. ) 
 CURVE ( )  GEOMETRIC_REPRESENTATION_ITEM ( )  RATIONAL_B_SPLINE_CURVE ( ( 1.000000000000000000, 0.8047378541243649375, 0.8047378541243649375, 1.000000000000000000 ) ) 
 REPRESENTATION_ITEM ( '' )  );
#48439 = EDGE_CURVE ( 'NONE', #53641, #96281, #60619, .T. ) ;
#48440 = CARTESIAN_POINT ( 'NONE',  ( -2.298369507954999946, 1516.779243033999819, 205.8702346062869992 ) ) ;
#48441 = ORIENTED_EDGE ( 'NONE', *, *, #32448, .T. ) ;
#48442 = CARTESIAN_POINT ( 'NONE',  ( -1.127928371535000140, 1516.989863902050047, 209.1319708558790182 ) ) ;
#48443 = AXIS2_PLACEMENT_3D ( 'NONE', #88886, #47442, #97279 ) ;
#48444 = CARTESIAN_POINT ( 'NONE',  ( -7.446870712126620440, 1453.253929861869892, 203.4788461265429760 ) ) ;
#48445 = B_SPLINE_SURFACE_WITH_KNOTS ( 'NONE', 5, 1, ( 
 ( #101361, #43701 ),
 ( #44263, #42045 ),
 ( #77854, #35293 ),
 ( #17354, #24651 ),
 ( #8421, #50462 ),
 ( #95203, #76197 ) ),
 .UNSPECIFIED., .F., .F., .F.,
 ( 6, 6 ),
 ( 2, 2 ),
 ( 0.000000000000000000, 4.008920757899999465 ),
 ( 0.000000000000000000, 14.00000000000000000 ),
 .UNSPECIFIED. ) ;
#48446 = CARTESIAN_POINT ( 'NONE',  ( -13.59758770590147492, 1411.972790166096502, 269.3580573342126172 ) ) ;
#48447 = CARTESIAN_POINT ( 'NONE',  ( -0.8853909531090000673, 1410.323732749430064, 233.0849705860979952 ) ) ;
#48449 = VERTEX_POINT ( 'NONE', #39775 ) ;
#48448 = CARTESIAN_POINT ( 'NONE',  ( -11.89850863680000082, 1497.713060387329961, 190.2034600782980078 ) ) ;
#48450 = CARTESIAN_POINT ( 'NONE',  ( 5.513435558250590951, 1508.884207225577711, 216.6305528438562362 ) ) ;
#48451 = CARTESIAN_POINT ( 'NONE',  ( -34.33105695552479375, 1440.913060389319980, 249.5635140075729907 ) ) ;
#48452 = CARTESIAN_POINT ( 'NONE',  ( -43.08084643290000315, 1384.773678278489797, 247.5054735941590138 ) ) ;
#48453 = CARTESIAN_POINT ( 'NONE',  ( -0.2569123757260329821, 1466.030216462040016, 235.8399092281299829 ) ) ;
#48454 = CARTESIAN_POINT ( 'NONE',  ( 5.151086705716080516, 1410.620189125909974, 269.3380098377049876 ) ) ;
#48456 = CARTESIAN_POINT ( 'NONE',  ( -3.255340964424999761, 1516.962555622980062, 213.7459452615670159 ) ) ;
#48455 = AXIS2_PLACEMENT_3D ( 'NONE', #58438, #75787, #16392 ) ;
#48457 = CARTESIAN_POINT ( 'NONE',  ( 22.88862305450000179, 1409.720888560930007, 208.9462140200429872 ) ) ;
#48458 = CARTESIAN_POINT ( 'NONE',  ( -20.28810075950000069, 1508.873707194230064, 188.9657859483980076 ) ) ;
#48459 = CARTESIAN_POINT ( 'NONE',  ( 12.24972954961170046, 1492.464136767450100, 210.6849265718639970 ) ) ;
#48460 = CARTESIAN_POINT ( 'NONE',  ( -7.708997972447890312, 1516.533014244449987, 211.5310356469510111 ) ) ;
#48461 = CARTESIAN_POINT ( 'NONE',  ( 2.493697040924999886, 1516.977201124959947, 210.2401991861970032 ) ) ;
#48462 = CARTESIAN_POINT ( 'NONE',  ( 17.73225504275583830, 1524.152349020271004, 180.4731530606409819 ) ) ;
#48463 = VECTOR ( 'NONE', #67460, 1000.000000000000000 ) ;
#48464 = CARTESIAN_POINT ( 'NONE',  ( -14.34315653738819485, 1486.055971446375679, 185.9291880012369234 ) ) ;
#48466 = VERTEX_POINT ( 'NONE', #30254 ) ;
#48465 = CARTESIAN_POINT ( 'NONE',  ( -39.09877692349999734, 1389.679302472760128, 233.5893560917589866 ) ) ;
#48467 = CARTESIAN_POINT ( 'NONE',  ( -42.32708834505060480, 1385.168503165180255, 246.3381990889729991 ) ) ;
#48468 = CARTESIAN_POINT ( 'NONE',  ( 18.96271102769999928, 1416.819759739330038, 210.2433116420780266 ) ) ;
#48469 = CARTESIAN_POINT ( 'NONE',  ( -4.459845537155718631, 1370.469452523700738, 208.9750888997069467 ) ) ;
#48470 = AXIS2_PLACEMENT_3D ( 'NONE', #69836, #70392, #70952 ) ;
#48471 = CARTESIAN_POINT ( 'NONE',  ( -13.67687855990000045, 1421.535259874829990, 230.0823906799980136 ) ) ;
#48472 = DIRECTION ( 'NONE',  ( 0.8672669759446630655, -0.000000000000000000, -0.4978433412588735285 ) ) ;
#48473 = CARTESIAN_POINT ( 'NONE',  ( 11.62117845040000041, 1421.988945507780045, 205.3376110126490062 ) ) ;
#48474 = CARTESIAN_POINT ( 'NONE',  ( -11.87275636863970085, 1432.783179063080070, 147.6501916617970096 ) ) ;
#48476 = LINE ( 'NONE', #75332, #31876 ) ;
#48475 = CARTESIAN_POINT ( 'NONE',  ( 2.873329360754999673, 1516.572193931679976, 216.4439510378570048 ) ) ;
#48477 = CARTESIAN_POINT ( 'NONE',  ( -21.99779490583109975, 1409.845346897619947, 211.9582521639920003 ) ) ;
#48478 = CARTESIAN_POINT ( 'NONE',  ( 33.43367350703651653, 1524.397344074318426, 220.4773507679699662 ) ) ;
#48479 = ORIENTED_EDGE ( 'NONE', *, *, #106358, .T. ) ;
#48480 = CARTESIAN_POINT ( 'NONE',  ( -4.616861546545000472, 1516.666407245520077, 201.4093549791169835 ) ) ;
#48481 = CARTESIAN_POINT ( 'NONE',  ( 27.96976558946629865, 1509.201555284690130, 207.5796322897400046 ) ) ;
#48482 = ORIENTED_EDGE ( 'NONE', *, *, #63202, .T. ) ;
#48483 = CARTESIAN_POINT ( 'NONE',  ( 0.000000000000000000, 1518.913060387330006, 209.1218459616979999 ) ) ;
#48484 = CARTESIAN_POINT ( 'NONE',  ( 22.12750824849999987, 1452.642887229430244, 220.0678107083980137 ) ) ;
#48485 = CARTESIAN_POINT ( 'NONE',  ( 10.95263331896989811, 1461.248509904520006, 209.5029505453279910 ) ) ;
#48486 = CARTESIAN_POINT ( 'NONE',  ( 8.956968256945643247, 1424.994159167145881, 195.6940687255158480 ) ) ;
#48487 = CARTESIAN_POINT ( 'NONE',  ( 0.5411951686119990113, 1444.367775260089957, 218.0750552485089884 ) ) ;
#48488 = CARTESIAN_POINT ( 'NONE',  ( 7.212015265482224713, 1416.834466888146380, 231.0122356860012474 ) ) ;
#48489 = VECTOR ( 'NONE', #25579, 1000.000000000000000 ) ;
#48490 = CARTESIAN_POINT ( 'NONE',  ( -4.220206612590000184, 1446.210882134589838, 168.9980572494979754 ) ) ;
#48491 = CARTESIAN_POINT ( 'NONE',  ( -19.54046289729999941, 1426.642498283530131, 224.7160149891979870 ) ) ;
#48492 = CARTESIAN_POINT ( 'NONE',  ( -23.41403251080000203, 1435.314950308189964, 138.7792008531980059 ) ) ;
#48493 = CARTESIAN_POINT ( 'NONE',  ( -107.7927744079999997, 1388.954798810650118, 298.5901260703590196 ) ) ;
#48494 = CARTESIAN_POINT ( 'NONE',  ( 18.31256684599999929, 1461.935672362830019, 190.2221303580979850 ) ) ;
#48495 = CARTESIAN_POINT ( 'NONE',  ( -105.8185464679999939, 1391.163751785419890, 301.8501960914589972 ) ) ;
#48496 = CARTESIAN_POINT ( 'NONE',  ( -16.13319535987753284, 1469.080883781242164, 269.3696318216189525 ) ) ;
#48497 = ORIENTED_EDGE ( 'NONE', *, *, #18482, .T. ) ;
#48498 = CARTESIAN_POINT ( 'NONE',  ( -103.5801441629999857, 1379.883084196419986, 303.9981228830590112 ) ) ;
#48499 = CARTESIAN_POINT ( 'NONE',  ( 14.30333092830361075, 1506.380977037114235, 192.4362132687745941 ) ) ;
#48500 = B_SPLINE_CURVE_WITH_KNOTS ( 'NONE', 3,
 ( #104211, #44885, #10148, #45975, #62238, #11806, #17978, #61685, #60582, #26958, #96923, #2336, #34798, #52173, #79035, #35915 ),
 .UNSPECIFIED., .F., .F.,
 ( 4, 3, 3, 3, 3, 4 ),
 ( -7.293777645795730180, -6.759547601150760698, -5.814523359711800232, -4.874165951496349791, -3.935888733346409651, -3.000356897310000548 ),
 .UNSPECIFIED. ) ;
#48501 = CARTESIAN_POINT ( 'NONE',  ( 11.20607753534230078, 1470.380238220569936, 207.2284536391540257 ) ) ;
#48502 = CARTESIAN_POINT ( 'NONE',  ( -7.215398911020000305, 1408.913060387329779, 225.6058586963979735 ) ) ;
#48503 = CARTESIAN_POINT ( 'NONE',  ( -0.2286327670369999732, 1416.983677237929896, 234.1874105466980041 ) ) ;
#48504 = CARTESIAN_POINT ( 'NONE',  ( -13.07753579797488896, 1443.006526933015039, 186.6367630675282214 ) ) ;
#48505 = DIRECTION ( 'NONE',  ( 0.9822959463215400477, 0.1391731009607420078, -0.1254014426122810055 ) ) ;
#48506 = DIRECTION ( 'NONE',  ( 1.755985294532469921E-16, -1.000000000000000000, 1.338183447452831989E-16 ) ) ;
#48507 = CIRCLE ( 'NONE', #16326, 1.000000000000000888 ) ;
#48508 = FACE_OUTER_BOUND ( 'NONE', #77340, .T. ) ;
#48509 = CARTESIAN_POINT ( 'NONE',  ( -15.01193293222859815, 1415.677402202029953, 207.4711775341719999 ) ) ;
#48510 = CARTESIAN_POINT ( 'NONE',  ( 25.06810116750000006, 1436.599588250250008, 137.8027482626980031 ) ) ;
#48511 = CARTESIAN_POINT ( 'NONE',  ( 2.564633783425000146, 1511.308638870219966, 216.6940388207569868 ) ) ;
#48513 = VERTEX_POINT ( 'NONE', #57702 ) ;
#48512 = CARTESIAN_POINT ( 'NONE',  ( -13.30361737529999999, 1409.377632944630022, 226.2974604263980041 ) ) ;
#48514 = CARTESIAN_POINT ( 'NONE',  ( -103.7373262539999956, 1383.424473230740205, 296.9348076431590471 ) ) ;
#48515 = CARTESIAN_POINT ( 'NONE',  ( 14.42425704043469814, 1513.497693042480023, 224.2590841663360095 ) ) ;
#48516 = ORIENTED_EDGE ( 'NONE', *, *, #69339, .T. ) ;
#48517 = ORIENTED_EDGE ( 'NONE', *, *, #79618, .T. ) ;
#48518 = CARTESIAN_POINT ( 'NONE',  ( 17.85664671351629806, 1415.933499560010205, 208.9473542036010087 ) ) ;
#48519 = B_SPLINE_CURVE_WITH_KNOTS ( 'NONE', 5,
 ( #42474, #33501, #76631, #93422, #9430, #74997 ),
 .UNSPECIFIED., .F., .F.,
 ( 6, 6 ),
 ( 0.000000000000000000, 1.000000000000000000 ),
 .UNSPECIFIED. ) ;
#48520 = CARTESIAN_POINT ( 'NONE',  ( -20.53760542139750456, 1525.821544997590536, 233.5223198772807507 ) ) ;
#48522 = CARTESIAN_POINT ( 'NONE',  ( -24.09667683720000042, 1455.346816438730002, 238.1639138257980051 ) ) ;
#48521 = CARTESIAN_POINT ( 'NONE',  ( 4.758389699129999428, 1454.760432536389999, 217.3925755712789964 ) ) ;
#48523 = CARTESIAN_POINT ( 'NONE',  ( -20.10488467649999933, 1503.697545318330185, 189.3141326410979843 ) ) ;
#48524 = CARTESIAN_POINT ( 'NONE',  ( -11.88526705700000008, 1433.193525880590187, 149.9681886515980125 ) ) ;
#48525 = DIRECTION ( 'NONE',  ( 0.9858563016923833633, 0.000000000000000000, 0.1675928173085483863 ) ) ;
#48526 = CARTESIAN_POINT ( 'NONE',  ( -27.69925887780000195, 1441.434395789990049, 137.3015763680980115 ) ) ;
#48527 = CARTESIAN_POINT ( 'NONE',  ( -11.58478124459999847, 1415.063410489729904, 195.8970895505979968 ) ) ;
#48528 = DIRECTION ( 'NONE',  ( -0.9455185755993178454, 0.000000000000000000, 0.3255681544571539243 ) ) ;
#48529 = CARTESIAN_POINT ( 'NONE',  ( 1.167020444750000108, 1450.781019595759972, 181.8366706930980001 ) ) ;
#48530 = MECHANICAL_DESIGN_GEOMETRIC_PRESENTATION_REPRESENTATION (  '', ( #9198 ), #45032 ) ;
#48531 = CARTESIAN_POINT ( 'NONE',  ( -0.6941066948465304254, 1362.404256174842203, 209.6218459617148824 ) ) ;
#48532 = CARTESIAN_POINT ( 'NONE',  ( -10.09491806113956791, 1509.391460115556811, 237.3755645815038235 ) ) ;
#48534 = ORIENTED_EDGE ( 'NONE', *, *, #75449, .T. ) ;
#48533 = CARTESIAN_POINT ( 'NONE',  ( 4.873133187124399707E-09, 1406.012954286680042, 266.9164466110329954 ) ) ;
#48535 = ORIENTED_EDGE ( 'NONE', *, *, #18154, .T. ) ;
#48536 = EDGE_CURVE ( 'NONE', #91965, #109427, #41556, .T. ) ;
#48537 = CARTESIAN_POINT ( 'NONE',  ( -13.43029793530000049, 1505.160453439490084, 208.9607663354669853 ) ) ;
#48538 = CARTESIAN_POINT ( 'NONE',  ( 24.07100108422400098, 1495.446790078319964, 207.0356552236710002 ) ) ;
#48539 = CARTESIAN_POINT ( 'NONE',  ( -4.814686654720000902, 1471.386640766029814, 269.6174199348980096 ) ) ;
#48540 = CARTESIAN_POINT ( 'NONE',  ( 19.68364361584636768, 1517.051704408389924, 197.0079017806501156 ) ) ;
#48542 = AXIS2_PLACEMENT_3D ( 'NONE', #45012, #79157, #2465 ) ;
#48541 = CARTESIAN_POINT ( 'NONE',  ( 9.400735251840000473, 1432.346452651970139, 153.1462979580980175 ) ) ;
#48543 = CARTESIAN_POINT ( 'NONE',  ( 35.68489934706420286, 1450.614492635629858, 136.1526271777700288 ) ) ;
#48544 = CARTESIAN_POINT ( 'NONE',  ( 0.2255011766491570036, 1451.657143026270205, 182.8204767894659994 ) ) ;
#48545 = CARTESIAN_POINT ( 'NONE',  ( 19.30812218469289121, 1456.473178130213682, 228.7018492185203797 ) ) ;
#48546 = EDGE_CURVE ( 'NONE', #63032, #8806, #57015, .T. ) ;
#48547 = CARTESIAN_POINT ( 'NONE',  ( 10.03041208372980009, 1469.257739677249901, 209.6369766770589820 ) ) ;
#48548 = CARTESIAN_POINT ( 'NONE',  ( -6.124734198089999637, 1458.063336725389945, 216.4789210408089843 ) ) ;
#48549 = CARTESIAN_POINT ( 'NONE',  ( 11.73111152208969798, 1363.746748086613479, 208.3718459617010978 ) ) ;
#48550 = CARTESIAN_POINT ( 'NONE',  ( -33.35109133253590130, 1416.979667404030124, 269.1074273680090414 ) ) ;
#48551 = ORIENTED_EDGE ( 'NONE', *, *, #34273, .T. ) ;
#48552 = CARTESIAN_POINT ( 'NONE',  ( -3.539264903962820341, 1497.294491324139926, 181.3958076714880008 ) ) ;
#48553 = VERTEX_POINT ( 'NONE', #109195 ) ;
#48554 = EDGE_LOOP ( 'NONE', ( #103419, #75006, #757, #80415 ) ) ;
#48555 = CARTESIAN_POINT ( 'NONE',  ( -3.445685115514999897, 1516.778761582560037, 211.6139765934069885 ) ) ;
#48556 = AXIS2_PLACEMENT_3D ( 'NONE', #48206, #18416, #563 ) ;
#48557 = CARTESIAN_POINT ( 'NONE',  ( 4.436453144186142339, 1423.828612835836338, 183.6460411026642703 ) ) ;
#48558 = CARTESIAN_POINT ( 'NONE',  ( 40.92391338726710615, 1444.178192375350136, 136.9148929651390176 ) ) ;
#48560 = DIRECTION ( 'NONE',  ( 1.755985294532469921E-16, -1.000000000000000000, 1.338183447452831989E-16 ) ) ;
#48559 = CARTESIAN_POINT ( 'NONE',  ( -0.7356989727169980231, 1517.020847257979995, 212.5827121409169820 ) ) ;
#48561 = CARTESIAN_POINT ( 'NONE',  ( -16.89981363069999887, 1455.454529709330018, 189.6846976769979847 ) ) ;
#48562 = CARTESIAN_POINT ( 'NONE',  ( -2.281512216559187234, 1449.806067081884976, 182.9567416777415190 ) ) ;
#48563 = ORIENTED_EDGE ( 'NONE', *, *, #103887, .T. ) ;
#48564 = CARTESIAN_POINT ( 'NONE',  ( -26.49085951069999822, 1436.258304344430144, 136.6654738169979737 ) ) ;
#48565 = CARTESIAN_POINT ( 'NONE',  ( -5.780861274184998955, 1516.783701990830195, 202.1826264492970324 ) ) ;
#48566 = AXIS2_PLACEMENT_3D ( 'NONE', #83060, #56210, #66292 ) ;
#48567 = CARTESIAN_POINT ( 'NONE',  ( -17.29525745463784503, 1505.122270163578605, 223.1329967567506856 ) ) ;
#48569 =( BOUNDED_CURVE ( )  B_SPLINE_CURVE ( 3, ( #803, #68017, #34932, #59598 ),
 .UNSPECIFIED., .F., .F. ) 
 B_SPLINE_CURVE_WITH_KNOTS ( ( 4, 4 ),
 ( 1.018872757951490016, 2.122719868645289942 ),
 .UNSPECIFIED. ) 
 CURVE ( )  GEOMETRIC_REPRESENTATION_ITEM ( )  RATIONAL_B_SPLINE_CURVE ( ( 1.000000000000000000, 0.9010116851119320813, 0.9010116851119320813, 1.000000000000000000 ) ) 
 REPRESENTATION_ITEM ( '' )  );
#48568 = VECTOR ( 'NONE', #27256, 1000.000000000000114 ) ;
#48570 = CARTESIAN_POINT ( 'NONE',  ( 0.01096402816149999980, 1407.225809180230044, 196.1218459610979892 ) ) ;
#48571 = DIRECTION ( 'NONE',  ( 0.7067700363771036720, 0.03085824620770448445, -0.7067700363771035610 ) ) ;
#48572 = CARTESIAN_POINT ( 'NONE',  ( -6.240887331089999712, 1397.787773551729970, 197.7178372010980070 ) ) ;
#48574 = VERTEX_POINT ( 'NONE', #55490 ) ;
#48573 = CARTESIAN_POINT ( 'NONE',  ( -8.808902786682349273, 1364.914369817750185, 210.6218459617142003 ) ) ;
#48575 = ORIENTED_EDGE ( 'NONE', *, *, #38800, .T. ) ;
#48576 = CARTESIAN_POINT ( 'NONE',  ( 0.2959633938429999667, 1452.979674875830142, 183.2640183118980133 ) ) ;
#48577 = CARTESIAN_POINT ( 'NONE',  ( 3.752275789878676271, 1425.500837115214381, 185.1933876786509074 ) ) ;
#48578 = CARTESIAN_POINT ( 'NONE',  ( 10.92857032808210072, 1460.888924644350027, 208.5047758900509791 ) ) ;
#48579 = CARTESIAN_POINT ( 'NONE',  ( -14.55974755836840018, 1436.247439882689832, 149.8925174081419982 ) ) ;
#48580 = CARTESIAN_POINT ( 'NONE',  ( -0.03728113298654189833, 1409.749267624750019, 185.1545790610279880 ) ) ;
#48581 = CARTESIAN_POINT ( 'NONE',  ( 3.268859396054999866, 1516.922519270759949, 211.5998327024669834 ) ) ;
#48582 = AXIS2_PLACEMENT_3D ( 'NONE', #95127, #18389, #54255 ) ;
#48583 = CARTESIAN_POINT ( 'NONE',  ( 8.447516053086825849, 1461.289618066398816, 204.2828433158165069 ) ) ;
#48584 = CARTESIAN_POINT ( 'NONE',  ( -2.549249301710439841, 1484.259727321469882, 183.2432226763939980 ) ) ;
#48585 = CARTESIAN_POINT ( 'NONE',  ( 7.752047435854870550, 1438.685045526630120, 214.1104276491739711 ) ) ;
#48586 = CARTESIAN_POINT ( 'NONE',  ( 4.760896992130000172, 1449.971761959190189, 190.6385172635989704 ) ) ;
#48587 = CARTESIAN_POINT ( 'NONE',  ( 8.324963421445000122, 1511.468585915670019, 203.7405339563369751 ) ) ;
#48588 = CARTESIAN_POINT ( 'NONE',  ( -4.044321718124999521, 1517.001127920769704, 206.8363583507369867 ) ) ;
#48589 = ORIENTED_EDGE ( 'NONE', *, *, #94752, .F. ) ;
#48590 = DIRECTION ( 'NONE',  ( -2.479303797180243098E-05, 0.02617627755937491918, 0.9996573422320469415 ) ) ;
#48591 = CARTESIAN_POINT ( 'NONE',  ( -10.50362050230000044, 1471.648827043890151, 207.7636308339789650 ) ) ;
#48592 = CARTESIAN_POINT ( 'NONE',  ( -23.99652642515154000, 1445.345535593930663, 212.5605566193962943 ) ) ;
#48593 = ORIENTED_EDGE ( 'NONE', *, *, #46294, .F. ) ;
#48594 = CARTESIAN_POINT ( 'NONE',  ( 22.08327125186943718, 1523.604703353109699, 233.8169256665487694 ) ) ;
#48595 = CARTESIAN_POINT ( 'NONE',  ( 12.84218287614169896, 1435.936370184710086, 150.8117598946369924 ) ) ;
#48596 = CARTESIAN_POINT ( 'NONE',  ( 13.31050682230000071, 1414.983773854429955, 197.8499836438979855 ) ) ;
#48597 = CARTESIAN_POINT ( 'NONE',  ( -2.197413362389999847, 1507.220826622230106, 180.8381795179979861 ) ) ;
#48598 = CARTESIAN_POINT ( 'NONE',  ( 12.72284891840000043, 1416.311719779230089, 222.6852781584979653 ) ) ;
#48599 = CARTESIAN_POINT ( 'NONE',  ( 17.00063747520000135, 1410.433676325329998, 226.2701375890979989 ) ) ;
#48600 = CARTESIAN_POINT ( 'NONE',  ( 6.636923444789999849, 1488.278828811890207, 199.0403411110989964 ) ) ;
#48601 = DIRECTION ( 'NONE',  ( -9.439841191556039654E-47, 1.000000000000000000, -1.836970198721029688E-16 ) ) ;
#48602 = CARTESIAN_POINT ( 'NONE',  ( 24.03875944314501112, 1447.055054376208773, 215.2337187572886705 ) ) ;
#48603 = CARTESIAN_POINT ( 'NONE',  ( -18.16080229929628231, 1445.425848083091978, 203.8898520025014705 ) ) ;
#48604 = CARTESIAN_POINT ( 'NONE',  ( -7.512750246095000861, 1509.038615934239942, 214.6352815282469919 ) ) ;
#48605 = CARTESIAN_POINT ( 'NONE',  ( -2.871580426725000024, 1517.129577905929864, 216.0720609035170128 ) ) ;
#48606 = VERTEX_POINT ( 'NONE', #13437 ) ;
#48607 = CARTESIAN_POINT ( 'NONE',  ( 7.710157425188729263, 1516.577293414350152, 207.6821489692630109 ) ) ;
#48608 = STYLED_ITEM ( 'NONE', ( #62922 ), #43980 ) ;
#48609 = CARTESIAN_POINT ( 'NONE',  ( -34.89169900679999614, 1462.401046348830278, 269.8669090264980355 ) ) ;
#48610 = CARTESIAN_POINT ( 'NONE',  ( 0.6438251882000000093, 1419.376757820729836, 184.7188999000980232 ) ) ;
#48611 = CARTESIAN_POINT ( 'NONE',  ( -15.38373915201839992, 1508.451228047400036, 215.1348082370930115 ) ) ;
#48612 = ADVANCED_FACE ( 'NONE', ( #83416 ), #98563, .F. ) ;
#48613 = B_SPLINE_CURVE_WITH_KNOTS ( 'NONE', 3,
 ( #33438, #69294, #8240, #93357, #51928, #16082 ),
 .UNSPECIFIED., .F., .F.,
 ( 4, 2, 4 ),
 ( -1.131363979615587220E-05, 0.001067788114096031088, 0.002146889867988218108 ),
 .UNSPECIFIED. ) ;
#48614 = CARTESIAN_POINT ( 'NONE',  ( -3.009012269849999921, 1476.164698171590089, 219.7802673373990103 ) ) ;
#48615 = CARTESIAN_POINT ( 'NONE',  ( 30.39553402230279744, 1509.974493418120119, 207.3314266928840084 ) ) ;
#48616 = DIRECTION ( 'NONE',  ( 0.000000000000000000, 0.000000000000000000, -1.000000000000000000 ) ) ;
#48617 = CARTESIAN_POINT ( 'NONE',  ( 2.488503644649960655, 1417.702710168876592, 233.7328821538343107 ) ) ;
#48618 = CARTESIAN_POINT ( 'NONE',  ( -2.500000000000000000, 1419.383100980419840, 144.1003751433630100 ) ) ;
#48619 = ADVANCED_FACE ( 'NONE', ( #73934 ), #87462, .T. ) ;
#48620 = CARTESIAN_POINT ( 'NONE',  ( -105.0711645279999971, 1379.235653477059941, 303.4121855584589866 ) ) ;
#48621 = CARTESIAN_POINT ( 'NONE',  ( 8.742163716520650412E-12, 1408.913060387359792, 224.1216835645979870 ) ) ;
#48623 = ADVANCED_FACE ( 'NONE', ( #14554 ), #23509, .T. ) ;
#48622 = CARTESIAN_POINT ( 'NONE',  ( 29.80083709734149977, 1440.913060386300003, 237.7077141819719657 ) ) ;
#48625 = CARTESIAN_POINT ( 'NONE',  ( 9.999026927027419021, 1469.414161099939975, 210.1225948180470198 ) ) ;
#48624 = CARTESIAN_POINT ( 'NONE',  ( -9.774084277346261729, 1471.600999675089952, 211.8492761500930328 ) ) ;
#48626 = CARTESIAN_POINT ( 'NONE',  ( 12.95579922760000002, 1419.891847053030006, 221.9576903087979929 ) ) ;
#48627 = ORIENTED_EDGE ( 'NONE', *, *, #86894, .F. ) ;
#48628 = ORIENTED_EDGE ( 'NONE', *, *, #48536, .T. ) ;
#48629 = CARTESIAN_POINT ( 'NONE',  ( 10.53896813186729986, 1480.812051149729996, 208.6340423618050011 ) ) ;
#48630 = CARTESIAN_POINT ( 'NONE',  ( -19.67913117755652053, 1485.239616831768444, 190.3362610098068615 ) ) ;
#48631 = CIRCLE ( 'NONE', #82592, 0.4999999999999995559 ) ;
#48632 = CARTESIAN_POINT ( 'NONE',  ( -4.077180901879999375, 1442.282981986689947, 201.0855821934289906 ) ) ;
#48633 = DIRECTION ( 'NONE',  ( 0.02616798426500965835, 0.9993150019883683122, -0.02616798426500970692 ) ) ;
#48634 = DIRECTION ( 'NONE',  ( -0.9455185755993178454, 0.000000000000000000, 0.3255681544571537578 ) ) ;
#48635 = CARTESIAN_POINT ( 'NONE',  ( 10.90534049613379963, 1422.234868131600251, 210.9169051273459843 ) ) ;
#48636 = DIRECTION ( 'NONE',  ( 0.000000000000000000, 0.000000000000000000, 1.000000000000000000 ) ) ;
#48637 = CARTESIAN_POINT ( 'NONE',  ( -30.31644210120117577, 1523.530870145311383, 222.4932309826520793 ) ) ;
#48638 = CARTESIAN_POINT ( 'NONE',  ( -44.80631001358410259, 1383.820492996369921, 250.7713395079869656 ) ) ;
#48639 = CARTESIAN_POINT ( 'NONE',  ( 21.12212911287033279, 1512.187213306747481, 235.8226600804184443 ) ) ;
#48640 = CARTESIAN_POINT ( 'NONE',  ( -15.30113400179999772, 1507.624001450029937, 191.9539244739980006 ) ) ;
#48641 = EDGE_CURVE ( 'NONE', #110334, #7633, #69714, .T. ) ;
#48642 = CYLINDRICAL_SURFACE ( 'NONE', #37519, 1.999999999999915179 ) ;
#48643 = CARTESIAN_POINT ( 'NONE',  ( 11.50050621948940055, 1492.682587485599925, 212.1934388399340037 ) ) ;
#48645 = ORIENTED_EDGE ( 'NONE', *, *, #35240, .F. ) ;
#48644 = CARTESIAN_POINT ( 'NONE',  ( -0.9025875204510009908, 1457.243920652990028, 219.7495316366990039 ) ) ;
#48646 = CARTESIAN_POINT ( 'NONE',  ( 34.18677586421187442, 1522.382868172863937, 219.7932833225211766 ) ) ;
#48647 = TOROIDAL_SURFACE ( 'NONE', #379, 8.013264357029999729, 0.5000000000000000000 ) ;
#48648 = CARTESIAN_POINT ( 'NONE',  ( -19.95507914119999526, 1380.898749975469855, 218.5439484314190111 ) ) ;
#48649 = CARTESIAN_POINT ( 'NONE',  ( 4.333038849890169963, 1508.551704408389924, 204.9468833496109994 ) ) ;
#48650 = VERTEX_POINT ( 'NONE', #30810 ) ;
#48651 = ORIENTED_EDGE ( 'NONE', *, *, #67252, .F. ) ;
#48652 = ADVANCED_FACE ( 'NONE', ( #12906 ), #48743, .T. ) ;
#48653 = CARTESIAN_POINT ( 'NONE',  ( 0.8266031666246391740, 1416.818673872118779, 190.2123423678451957 ) ) ;
#48654 = CARTESIAN_POINT ( 'NONE',  ( -3.582801916544020138, 1515.224507089990084, 205.0446044820039901 ) ) ;
#48656 = CARTESIAN_POINT ( 'NONE',  ( -0.5624690339869999889, 1416.828040475229955, 227.7677324846980014 ) ) ;
#48655 = DIRECTION ( 'NONE',  ( 0.000000000000000000, 1.000000000000000000, 0.000000000000000000 ) ) ;
#48657 = CARTESIAN_POINT ( 'NONE',  ( -4.675540975309999681, 1462.620895424390028, 200.5633310686890241 ) ) ;
#48658 = CARTESIAN_POINT ( 'NONE',  ( -105.4616672789999967, 1378.899769895130021, 302.9954926620590072 ) ) ;
#48659 = DIRECTION ( 'NONE',  ( 0.000000000000000000, 1.000000000000000000, 0.000000000000000000 ) ) ;
#48660 = CARTESIAN_POINT ( 'NONE',  ( -15.94676957688830043, 1508.551704408389924, 213.8922084002869894 ) ) ;
#48661 = FACE_OUTER_BOUND ( 'NONE', #96914, .T. ) ;
#48662 = CARTESIAN_POINT ( 'NONE',  ( 18.80400137410000028, 1425.877418581729899, 225.3118762411980072 ) ) ;
#48663 = CARTESIAN_POINT ( 'NONE',  ( 17.17241001986483795, 1518.913060387330006, 179.6185504016043240 ) ) ;
#48664 = CARTESIAN_POINT ( 'NONE',  ( 8.009065970051258532, 1433.461148587649859, 203.5451095248959916 ) ) ;
#48665 = CARTESIAN_POINT ( 'NONE',  ( 11.76924708519999996, 1432.318127532269955, 150.8119212265980025 ) ) ;
#48666 = CIRCLE ( 'NONE', #11095, 6.771217174059998456 ) ;
#48667 = CARTESIAN_POINT ( 'NONE',  ( -22.52609268272879817, 1509.699688877640028, 190.9355248210520131 ) ) ;
#48668 = VERTEX_POINT ( 'NONE', #75043 ) ;
#48669 = CARTESIAN_POINT ( 'NONE',  ( 1.632486301776860348E-07, 1509.047264794319972, 239.1218459617020073 ) ) ;
#48670 = CARTESIAN_POINT ( 'NONE',  ( -10.86013104807563145, 1428.709904399815287, 134.0999999980980419 ) ) ;
#48671 = VECTOR ( 'NONE', #10246, 1000.000000000000114 ) ;
#48672 = CARTESIAN_POINT ( 'NONE',  ( -12.40096745299999981, 1434.347023119479900, 149.5501479441980166 ) ) ;
#48673 = CARTESIAN_POINT ( 'NONE',  ( 3.052975896485000007, 1516.551704408390151, 217.1245693350269903 ) ) ;
#48674 = CARTESIAN_POINT ( 'NONE',  ( -20.46943290138029781, 1503.635669217179839, 190.5120838222930217 ) ) ;
#48675 = ADVANCED_FACE ( 'NONE', ( #64987 ), #47085, .F. ) ;
#48676 = CARTESIAN_POINT ( 'NONE',  ( -15.59398630749999981, 1420.072677430659951, 211.3401063871789916 ) ) ;
#48677 = CARTESIAN_POINT ( 'NONE',  ( -109.1897705290000005, 1387.438473340760083, 310.9485453702590121 ) ) ;
#48678 = CARTESIAN_POINT ( 'NONE',  ( 17.40764059099999628, 1414.996444526030018, 210.6782161193179945 ) ) ;
#48679 = CARTESIAN_POINT ( 'NONE',  ( -11.11931780176117179, 1362.308639675578434, 209.6218459617033432 ) ) ;
#48680 = CARTESIAN_POINT ( 'NONE',  ( -29.86461515634900010, 1525.960063244516959, 220.9690070206027031 ) ) ;
#48681 = CARTESIAN_POINT ( 'NONE',  ( -22.72361261936710264, 1432.255920656152057, 217.6431712202583526 ) ) ;
#48682 = CARTESIAN_POINT ( 'NONE',  ( 14.06807837553630058, 1452.482298946410083, 222.8064072038120003 ) ) ;
#48683 = CARTESIAN_POINT ( 'NONE',  ( -3.269025173884999802, 1517.026534522949987, 208.0024068424170025 ) ) ;
#48684 = FACE_OUTER_BOUND ( 'NONE', #49138, .T. ) ;
#48685 = CARTESIAN_POINT ( 'NONE',  ( 13.40566205669149902, 1429.098591087019940, 222.0107402452829888 ) ) ;
#48686 = CARTESIAN_POINT ( 'NONE',  ( -14.32246179293609778, 1379.592251131270132, 207.9805893340429748 ) ) ;
#48687 = CARTESIAN_POINT ( 'NONE',  ( 7.476667830162710082, 1425.276938917010057, 212.2943805765499690 ) ) ;
#48688 = ORIENTED_EDGE ( 'NONE', *, *, #102331, .T. ) ;
#48689 = CARTESIAN_POINT ( 'NONE',  ( 31.95512683039999757, 1440.913060396209858, 244.1805851198980122 ) ) ;
#48690 = CARTESIAN_POINT ( 'NONE',  ( -28.34110756850000001, 1508.137170135529914, 209.4584315255609965 ) ) ;
#48692 = CARTESIAN_POINT ( 'NONE',  ( -17.59077195540000105, 1410.452734757129747, 194.3251796273980005 ) ) ;
#48691 = CARTESIAN_POINT ( 'NONE',  ( 0.5190711711569999665, 1464.113131884229915, 182.7836423421979930 ) ) ;
#48693 = DIRECTION ( 'NONE',  ( 5.980589973904019347E-17, -1.000000000000000000, 1.736889445713099699E-16 ) ) ;
#48694 = CARTESIAN_POINT ( 'NONE',  ( -20.53795889179999890, 1428.561159746129988, 220.8089596197980029 ) ) ;
#48695 = CARTESIAN_POINT ( 'NONE',  ( -1.450932694090000252, 1486.832070779689957, 220.2329197926989934 ) ) ;
#48696 = CARTESIAN_POINT ( 'NONE',  ( -20.21385637174950034, 1452.207176968400063, 142.9987421525109994 ) ) ;
#48697 = CARTESIAN_POINT ( 'NONE',  ( 21.25708630131437360, 1435.239819464457241, 139.1347687464948137 ) ) ;
#48698 = EDGE_LOOP ( 'NONE', ( #70932, #50264, #32192, #90547, #8578, #1187, #35826, #12487, #67526, #15406, #81717, #80637, #16946, #78575 ) ) ;
#48699 = CARTESIAN_POINT ( 'NONE',  ( -107.3712700886850087, 1378.913060387339783, 300.6990228053219312 ) ) ;
#48700 = DIRECTION ( 'NONE',  ( 0.9991156138703696232, -3.961952592064073292E-33, -0.04204747460233797945 ) ) ;
#48701 = CARTESIAN_POINT ( 'NONE',  ( 16.80536496183709971, 1423.594528387539867, 228.4229711109250047 ) ) ;
#48702 = CARTESIAN_POINT ( 'NONE',  ( 11.45577226660000036, 1502.286415424589904, 208.3140783707030153 ) ) ;
#48703 = ORIENTED_EDGE ( 'NONE', *, *, #90107, .F. ) ;
#48704 = ORIENTED_EDGE ( 'NONE', *, *, #77360, .F. ) ;
#48705 = CARTESIAN_POINT ( 'NONE',  ( -64.53155199309999546, 1384.701788983860297, 254.0354793386590018 ) ) ;
#48706 = CARTESIAN_POINT ( 'NONE',  ( -24.11864498019999914, 1411.115042655630077, 209.4126620446369884 ) ) ;
#48707 = EDGE_CURVE ( 'NONE', #38935, #102287, #38754, .T. ) ;
#48708 = CARTESIAN_POINT ( 'NONE',  ( -3.827327107099999903, 1424.046157849130168, 184.1455919444979656 ) ) ;
#48709 = DIRECTION ( 'NONE',  ( 1.755985294532464991E-16, -1.000000000000000000, 1.338183447452830017E-16 ) ) ;
#48710 = PLANE ( 'NONE',  #72446 ) ;
#48711 = EDGE_CURVE ( 'NONE', #59235, #43039, #67804, .T. ) ;
#48712 = CARTESIAN_POINT ( 'NONE',  ( -7.586230254490000213, 1507.634635854029966, 235.4684484327979987 ) ) ;
#48713 = CARTESIAN_POINT ( 'NONE',  ( -17.47806757639999731, 1410.883707539230045, 225.6330995444980090 ) ) ;
#48714 = ORIENTED_EDGE ( 'NONE', *, *, #26071, .T. ) ;
#48715 = CARTESIAN_POINT ( 'NONE',  ( 41.96559968512650585, 1455.508381183140045, 266.8112211961390017 ) ) ;
#48716 = CARTESIAN_POINT ( 'NONE',  ( 4.517196230222682019, 1517.051704408389924, 227.6318199458918343 ) ) ;
#48717 = CARTESIAN_POINT ( 'NONE',  ( -6.545266366469999930, 1426.912378977409844, 203.3789669689390109 ) ) ;
#48718 = CARTESIAN_POINT ( 'NONE',  ( -1.134358008724999811, 1516.744381837270112, 205.0932347109869909 ) ) ;
#48719 = ORIENTED_EDGE ( 'NONE', *, *, #105597, .F. ) ;
#48720 = DIRECTION ( 'NONE',  ( 0.3363363969981410517, -0.6659120918163093927, 0.6659120918162816372 ) ) ;
#48721 = CARTESIAN_POINT ( 'NONE',  ( 14.97619053132000033, 1512.179780174510142, 196.6274074352839989 ) ) ;
#48722 = CARTESIAN_POINT ( 'NONE',  ( 13.03096333729283529, 1442.971155689919669, 187.2524364873846707 ) ) ;
#48723 = EDGE_LOOP ( 'NONE', ( #73026, #74928, #81565, #38097 ) ) ;
#48724 = ORIENTED_EDGE ( 'NONE', *, *, #505, .T. ) ;
#48725 = CARTESIAN_POINT ( 'NONE',  ( 2.995039991590000117, 1448.960486182170143, 183.8207280578979805 ) ) ;
#48726 = CARTESIAN_POINT ( 'NONE',  ( -2.176449243140819778, 1508.203772142160233, 220.8519538129899900 ) ) ;
#48727 = CARTESIAN_POINT ( 'NONE',  ( -12.85932415441300058, 1512.319979277499897, 193.9537317410139963 ) ) ;
#48728 = CARTESIAN_POINT ( 'NONE',  ( 10.41399337298259908, 1502.882161159430098, 216.4575550115480098 ) ) ;
#48729 = CARTESIAN_POINT ( 'NONE',  ( 10.46140733719999893, 1420.326681975860083, 197.7779852210990157 ) ) ;
#48730 = CARTESIAN_POINT ( 'NONE',  ( 0.9509688288689980284, 1431.491297202929900, 218.5646205313049961 ) ) ;
#48731 = CARTESIAN_POINT ( 'NONE',  ( -4.161170142461470434, 1448.299083512420111, 185.1109003841999936 ) ) ;
#48732 = CARTESIAN_POINT ( 'NONE',  ( 10.19285232582329925, 1479.751836143369928, 205.9895992793150015 ) ) ;
#48733 = DIRECTION ( 'NONE',  ( 0.000000000000000000, 0.000000000000000000, 1.000000000000000000 ) ) ;
#48735 = CARTESIAN_POINT ( 'NONE',  ( 16.27110347889999886, 1489.469559537029909, 194.1428897389979795 ) ) ;
#48734 = CARTESIAN_POINT ( 'NONE',  ( -16.68466689124240077, 1411.595104653460112, 191.7171691803239924 ) ) ;
#48736 = CARTESIAN_POINT ( 'NONE',  ( 10.66784415300089961, 1424.355176726809987, 206.6195069038519989 ) ) ;
#48737 = CARTESIAN_POINT ( 'NONE',  ( -25.45358342560510323, 1509.770361827349916, 222.9816713348759833 ) ) ;
#48738 = EDGE_CURVE ( 'NONE', #103217, #84181, #4083, .T. ) ;
#48739 = CARTESIAN_POINT ( 'NONE',  ( 11.76598840989999850, 1428.979790717830156, 145.3128034382980047 ) ) ;
#48740 = ORIENTED_EDGE ( 'NONE', *, *, #2268, .T. ) ;
#48741 = CARTESIAN_POINT ( 'NONE',  ( 15.71554773450000297, 1429.441490238930101, 224.8635561783979711 ) ) ;
#48742 = CIRCLE ( 'NONE', #82698, 2.000000000000004885 ) ;
#48743 = CYLINDRICAL_SURFACE ( 'NONE', #8703, 2.000000000000007550 ) ;
#48744 = CARTESIAN_POINT ( 'NONE',  ( -100.5300167084300114, 1384.945107703380017, 310.8927782480189990 ) ) ;
#48745 = ADVANCED_FACE ( 'NONE', ( #34672 ), #93461, .F. ) ;
#48746 = CARTESIAN_POINT ( 'NONE',  ( -8.973420627790000381, 1387.914350804760033, 200.5228873143890098 ) ) ;
#48747 = CARTESIAN_POINT ( 'NONE',  ( 9.891757830708639787, 1427.006033834340087, 209.9233085989019969 ) ) ;
#48749 = EDGE_LOOP ( 'NONE', ( #65521, #6586, #44721, #96208 ) ) ;
#48748 = CARTESIAN_POINT ( 'NONE',  ( 11.05020669801949929, 1423.000693000939918, 203.3085683099579910 ) ) ;
#48750 = EDGE_CURVE ( 'NONE', #30887, #33927, #9474, .T. ) ;
#48751 = CARTESIAN_POINT ( 'NONE',  ( 4.271857500090000315, 1429.250640823790036, 216.3852677031590019 ) ) ;
#48752 = CARTESIAN_POINT ( 'NONE',  ( 16.58770733237511052, 1524.425415513989037, 237.5950306126129590 ) ) ;
#48753 = CARTESIAN_POINT ( 'NONE',  ( -13.58256621920000029, 1416.843576365230092, 221.9093687442980070 ) ) ;
#48754 = CARTESIAN_POINT ( 'NONE',  ( 11.34078683589999947, 1433.855572862709778, 151.4803113887979862 ) ) ;
#48755 = CARTESIAN_POINT ( 'NONE',  ( 43.50000000000000000, 1440.913060387330006, 271.1218459616979999 ) ) ;
#48756 = CARTESIAN_POINT ( 'NONE',  ( 3.295895095316650814, 1370.244911477964024, 210.1744081590250630 ) ) ;
#48757 = CARTESIAN_POINT ( 'NONE',  ( -11.60004869885203860, 1428.971947790929107, 136.1000015555673599 ) ) ;
#48758 = CARTESIAN_POINT ( 'NONE',  ( -6.148099858600874157, 1457.597472786487742, 216.4201080312880379 ) ) ;
#48759 = CARTESIAN_POINT ( 'NONE',  ( -4.963802804109999300, 1497.713060387329961, 230.9126810519979927 ) ) ;
#48760 = CARTESIAN_POINT ( 'NONE',  ( 12.18971934853500194, 1512.123542805230272, 223.8476153537669973 ) ) ;
#48761 = EDGE_CURVE ( 'NONE', #60549, #62781, #66768, .T. ) ;
#48762 = DIRECTION ( 'NONE',  ( 0.3390050494208932674, 0.7071067811868654296, 0.6205445805634662859 ) ) ;
#48763 = CARTESIAN_POINT ( 'NONE',  ( -17.57236383969999949, 1410.451431512329918, 225.4462110255979894 ) ) ;
#48764 = FACE_OUTER_BOUND ( 'NONE', #99084, .T. ) ;
#48765 = ADVANCED_FACE ( 'NONE', ( #16194 ), #33009, .F. ) ;
#48766 = CARTESIAN_POINT ( 'NONE',  ( -2.823272442860000009, 1474.899276188389877, 216.0777664757990237 ) ) ;
#48767 = DIRECTION ( 'NONE',  ( 0.000000000000000000, 0.07083107041561081951, -0.9974883254774358221 ) ) ;
#48768 = CARTESIAN_POINT ( 'NONE',  ( 6.866540673400110493E-07, 1408.860257358530134, 194.6498732444090081 ) ) ;
#48769 = CARTESIAN_POINT ( 'NONE',  ( 11.17826893112730957, 1434.135999025848378, 151.6295705600838062 ) ) ;
#48770 = DIRECTION ( 'NONE',  ( -1.755985294532469921E-16, 1.000000000000000000, -1.338183447452831989E-16 ) ) ;
#48772 = EDGE_CURVE ( 'NONE', #38113, #73081, #24589, .T. ) ;
#48771 = CARTESIAN_POINT ( 'NONE',  ( -5.548131016090000145, 1414.913060387229962, 224.8407497847980210 ) ) ;
#48773 = CARTESIAN_POINT ( 'NONE',  ( 0.2074342776960350077, 1458.792499532430156, 183.0048892579440007 ) ) ;
#48775 = ORIENTED_EDGE ( 'NONE', *, *, #13885, .F. ) ;
#48774 = CARTESIAN_POINT ( 'NONE',  ( 23.55087631299999984, 1411.110694763729953, 207.7642880164279973 ) ) ;
#48776 = CARTESIAN_POINT ( 'NONE',  ( 1.530052826864370052, 1452.704406626560058, 183.4894965714629791 ) ) ;
#48777 = DIRECTION ( 'NONE',  ( -0.9998780014336184907, 0.000000000000000000, 0.01561993114942984012 ) ) ;
#48778 = CARTESIAN_POINT ( 'NONE',  ( 11.87922978499999971, 1433.311594856540069, 149.1894924501980313 ) ) ;
#48779 = CARTESIAN_POINT ( 'NONE',  ( -40.85417709071609949, 1440.196123997409813, 134.0999999980799657 ) ) ;
#48780 = CYLINDRICAL_SURFACE ( 'NONE', #62211, 2.999999999999999556 ) ;
#48781 = VERTEX_POINT ( 'NONE', #25149 ) ;
#48783 = ADVANCED_FACE ( 'NONE', ( #67746 ), #77248, .F. ) ;
#48782 = CARTESIAN_POINT ( 'NONE',  ( -17.22627284987310148, 1525.856065479244762, 181.7773037624300798 ) ) ;
#48784 = B_SPLINE_CURVE_WITH_KNOTS ( 'NONE', 3,
 ( #108658, #90188, #13472, #31946, #98044, #82361, #48221, #5659, #47662, #49318, #21318, #55522, #89649, #47116, #81243, #38691, #107002, #65017, #30290, #81789, #5092 ),
 .UNSPECIFIED., .F., .F.,
 ( 4, 2, 1, 1, 1, 2, 2, 2, 1, 1, 2, 2, 4 ),
 ( 0.000000000000000000, 0.1250000000001823541, 0.1875000000002875200, 0.2187500000003548828, 0.2343750000003742007, 0.2421875000003838596, 0.2500000000003935186, 0.3750000000002933764, 0.4375000000002595146, 0.4687500000002259304, 0.4843750000002263745, 0.5000000000002269296, 1.000000000000000000 ),
 .UNSPECIFIED. ) ;
#48785 = CARTESIAN_POINT ( 'NONE',  ( 2.470955850358387718, 1523.580204110581235, 175.3687159778809814 ) ) ;
#48786 = CARTESIAN_POINT ( 'NONE',  ( -105.1938507991023783, 1381.037482386520196, 308.6129917943122791 ) ) ;
#48787 = CARTESIAN_POINT ( 'NONE',  ( -11.10863372729999909, 1491.777316212490177, 207.8912015286890096 ) ) ;
#48788 = EDGE_CURVE ( 'NONE', #98856, #69002, #20113, .T. ) ;
#48789 = CARTESIAN_POINT ( 'NONE',  ( 18.22805055419890152, 1459.311389626190021, 227.8763770136359881 ) ) ;
#48790 = CARTESIAN_POINT ( 'NONE',  ( -4.992349872352332518, 1391.620913799028131, 214.5306134754782761 ) ) ;
#48791 = CARTESIAN_POINT ( 'NONE',  ( 45.63713418245465903, 1439.235619164679065, 268.9747475081824746 ) ) ;
#48792 = CARTESIAN_POINT ( 'NONE',  ( -17.71563513420000291, 1420.335625605900077, 207.4269338723890144 ) ) ;
#48793 = CARTESIAN_POINT ( 'NONE',  ( -12.93896584940000061, 1379.674138171649929, 211.0424427186889886 ) ) ;
#48794 = CARTESIAN_POINT ( 'NONE',  ( 2.985881150139999995, 1431.471105595659992, 184.5967258471980017 ) ) ;
#48795 = CARTESIAN_POINT ( 'NONE',  ( -57.23345819662650058, 1385.048296059559789, 238.2082995797720173 ) ) ;
#48796 = CARTESIAN_POINT ( 'NONE',  ( 17.84338787571921969, 1523.382868172864164, 180.3600277896298110 ) ) ;
#48797 = CARTESIAN_POINT ( 'NONE',  ( -3.816599468434689779, 1508.551704408389924, 204.5159469375300034 ) ) ;
#48798 = EDGE_CURVE ( 'NONE', #90688, #30404, #85611, .T. ) ;
#48799 = CARTESIAN_POINT ( 'NONE',  ( -28.61821586814939877, 1509.224669311890011, 208.7631243191599992 ) ) ;
#48800 = CARTESIAN_POINT ( 'NONE',  ( -15.94765147786550052, 1409.469968486390144, 225.3462237114930247 ) ) ;
#48802 = ORIENTED_EDGE ( 'NONE', *, *, #91174, .T. ) ;
#48801 = CARTESIAN_POINT ( 'NONE',  ( 0.5031299281221360831, 1413.437613018619913, 184.9381903630110173 ) ) ;
#48803 = CARTESIAN_POINT ( 'NONE',  ( -9.234134023826198856, 1461.205490114660051, 206.1827678865119822 ) ) ;
#48804 = CARTESIAN_POINT ( 'NONE',  ( 11.10467535518500171, 1471.705490391439980, 211.8499711634750042 ) ) ;
#48805 = CARTESIAN_POINT ( 'NONE',  ( 21.04382134430000306, 1508.388118399029963, 226.0922268082980224 ) ) ;
#48806 = CARTESIAN_POINT ( 'NONE',  ( -109.3108433829999910, 1384.813040219950153, 311.2635926062589533 ) ) ;
#48807 = CARTESIAN_POINT ( 'NONE',  ( -0.08869625257939200980, 1419.939914807589957, 184.0372427730129914 ) ) ;
#48808 = CARTESIAN_POINT ( 'NONE',  ( 1.221557978829999946, 1466.110857312230110, 235.2972512431979908 ) ) ;
#48809 = CARTESIAN_POINT ( 'NONE',  ( 18.44309112110000015, 1409.721912672129974, 221.4648865221980145 ) ) ;
#48810 = LINE ( 'NONE', #4588, #83899 ) ;
#48811 = CARTESIAN_POINT ( 'NONE',  ( -16.97269670290000221, 1423.671420843229953, 228.0577291709979875 ) ) ;
#48813 = CARTESIAN_POINT ( 'NONE',  ( -2.500000000000000000, 1439.615672362210034, 183.5288080682979910 ) ) ;
#48812 = CARTESIAN_POINT ( 'NONE',  ( 11.78380890789823354, 1499.475951658889471, 204.3830416974864193 ) ) ;
#48814 = CARTESIAN_POINT ( 'NONE',  ( -9.959589622450000235, 1382.751681251990021, 218.0704319110489848 ) ) ;
#48815 = CARTESIAN_POINT ( 'NONE',  ( -119.7968474381516302, 1366.350733876288814, 293.4380634648589989 ) ) ;
#48816 = DIRECTION ( 'NONE',  ( 1.224646799147350002E-16, -1.836970198721029688E-16, -1.000000000000000000 ) ) ;
#48817 = CARTESIAN_POINT ( 'NONE',  ( -1.377961559329999863, 1416.217220538330139, 233.2979951139980130 ) ) ;
#48818 = CARTESIAN_POINT ( 'NONE',  ( 7.340269731169999368, 1361.836778001490075, 210.6218459616991936 ) ) ;
#48819 = CARTESIAN_POINT ( 'NONE',  ( 5.772727908745000747, 1516.691414181030041, 205.6645793267070133 ) ) ;
#48820 = CARTESIAN_POINT ( 'NONE',  ( -17.69798016750000258, 1424.268916621029803, 226.8670750680979893 ) ) ;
#48821 = VERTEX_POINT ( 'NONE', #109730 ) ;
#48822 = CARTESIAN_POINT ( 'NONE',  ( -109.1310292459999829, 1384.726238503300010, 311.2600142160089831 ) ) ;
#48823 = CARTESIAN_POINT ( 'NONE',  ( -4.239667262353160382, 1441.443752683740058, 162.8307151194100015 ) ) ;
#48825 = EDGE_LOOP ( 'NONE', ( #80250, #100873, #81455, #9522, #102802 ) ) ;
#48824 = CARTESIAN_POINT ( 'NONE',  ( -68.54407940739999106, 1379.747756885790068, 280.1275194418589649 ) ) ;
#48826 = ORIENTED_EDGE ( 'NONE', *, *, #4504, .T. ) ;
#48827 = ADVANCED_FACE ( 'NONE', ( #548 ), #92921, .F. ) ;
#48828 = CARTESIAN_POINT ( 'NONE',  ( -9.188021672635125370, 1380.611693761624338, 217.4304852955527281 ) ) ;
#48829 = VERTEX_POINT ( 'NONE', #78339 ) ;
#48830 = CARTESIAN_POINT ( 'NONE',  ( 2.229471592959419990, 1485.171155440719758, 220.7696600089880121 ) ) ;
#48831 = CARTESIAN_POINT ( 'NONE',  ( 11.83904535559999971, 1500.842106766089955, 208.3226773703530057 ) ) ;
#48833 = CARTESIAN_POINT ( 'NONE',  ( 15.85187002026029823, 1410.856221003509972, 191.5210852716889747 ) ) ;
#48832 = CARTESIAN_POINT ( 'NONE',  ( -11.64262758805663545, 1425.861298859939552, 144.5853139168677046 ) ) ;
#48834 = CARTESIAN_POINT ( 'NONE',  ( 2.299667965875000331, 1516.965971551240045, 210.2399506998270056 ) ) ;
#48835 = EDGE_CURVE ( 'NONE', #2195, #26364, #18709, .T. ) ;
#48836 = CARTESIAN_POINT ( 'NONE',  ( 36.40062700991159517, 1436.005110244360139, 135.0217463105349793 ) ) ;
#48837 = B_SPLINE_CURVE_WITH_KNOTS ( 'NONE', 3,
 ( #99597, #57646, #49235, #5001, #101239, #56527, #83358, #32420, #24539, #48686, #66599, #65487, #5565, #22880, #6103, #100703 ),
 .UNSPECIFIED., .F., .F.,
 ( 4, 3, 3, 3, 3, 4 ),
 ( -1.546267078793030159, -1.336910296889620042, -1.002126681165210087, -0.6673763298341559569, -0.3329907222668331279, 0.000000000000000000 ),
 .UNSPECIFIED. ) ;
#48838 = CARTESIAN_POINT ( 'NONE',  ( -107.9127952440289988, 1378.913060387289988, 308.3607811453639442 ) ) ;
#48839 = FACE_OUTER_BOUND ( 'NONE', #50856, .T. ) ;
#48840 = CARTESIAN_POINT ( 'NONE',  ( 11.21601427816997720, 1464.187623198618212, 231.8855071244460646 ) ) ;
#48841 = SHAPE_DEFINITION_REPRESENTATION ( #87531, #45156 ) ;
#48842 = CARTESIAN_POINT ( 'NONE',  ( 39.34220581737610445, 1449.349331648660154, 134.0999999980729740 ) ) ;
#48843 = CARTESIAN_POINT ( 'NONE',  ( -26.86204968941349946, 1508.007394745769943, 212.0120970035400205 ) ) ;
#48844 = ORIENTED_EDGE ( 'NONE', *, *, #63832, .F. ) ;
#48845 = CARTESIAN_POINT ( 'NONE',  ( 19.38665381416110023, 1498.811973477250149, 221.8202357131370093 ) ) ;
#48846 = CARTESIAN_POINT ( 'NONE',  ( -18.59366615780000132, 1458.580092697230157, 227.5321056525980055 ) ) ;
#48847 = ORIENTED_EDGE ( 'NONE', *, *, #31167, .T. ) ;
#48848 = ORIENTED_EDGE ( 'NONE', *, *, #93114, .T. ) ;
#48849 = CARTESIAN_POINT ( 'NONE',  ( 16.66094735743510213, 1410.867388111209948, 226.5061907891179942 ) ) ;
#48850 = CARTESIAN_POINT ( 'NONE',  ( 18.19590854888164699, 1522.382868172863937, 238.2026672068774644 ) ) ;
#48851 = EDGE_CURVE ( 'NONE', #89451, #59085, #46321, .T. ) ;
#48852 = CARTESIAN_POINT ( 'NONE',  ( 0.1797482706320000234, 1451.166081239530058, 182.5410796217979907 ) ) ;
#48853 = CARTESIAN_POINT ( 'NONE',  ( -2.987575625429999882, 1484.703021631029969, 183.3076216214979866 ) ) ;
#48854 = CARTESIAN_POINT ( 'NONE',  ( -2.500000000000000000, 1439.621629191349939, 170.0481657697840205 ) ) ;
#48855 = CARTESIAN_POINT ( 'NONE',  ( 4.327507137520000491, 1515.138941066290045, 209.8355549535610010 ) ) ;
#48856 = CARTESIAN_POINT ( 'NONE',  ( -2.500000000000000000, 1448.210448412289907, 183.1418046154980175 ) ) ;
#48857 = CARTESIAN_POINT ( 'NONE',  ( 33.91369104887559871, 1451.728768199629940, 135.6938360226120039 ) ) ;
#48858 = CARTESIAN_POINT ( 'NONE',  ( 1.153790625369999878, 1463.908919862690027, 199.3495073382590022 ) ) ;
#48859 = CARTESIAN_POINT ( 'NONE',  ( 25.85996285490000091, 1436.538141094960110, 136.9113464714980068 ) ) ;
#48860 = CARTESIAN_POINT ( 'NONE',  ( 5.548131867839999565, 1414.913060387229962, 193.4029425950980112 ) ) ;
#48861 = CARTESIAN_POINT ( 'NONE',  ( -83.83778724580230346, 1384.812601443120002, 287.5995587299269687 ) ) ;
#48862 = ORIENTED_EDGE ( 'NONE', *, *, #65142, .T. ) ;
#48863 = CARTESIAN_POINT ( 'NONE',  ( -3.260378293205000055, 1516.582197289609894, 201.4115600944169842 ) ) ;
#48864 = CARTESIAN_POINT ( 'NONE',  ( -0.007128875282218469743, 1517.006509894990131, 208.3750284165899984 ) ) ;
#48865 = ORIENTED_EDGE ( 'NONE', *, *, #108900, .T. ) ;
#48866 = CARTESIAN_POINT ( 'NONE',  ( 33.53994528179689638, 1440.913060387330006, 258.5778273533969696 ) ) ;
#48867 = ADVANCED_FACE ( 'NONE', ( #2214 ), #8178, .T. ) ;
#48868 = FACE_OUTER_BOUND ( 'NONE', #22233, .T. ) ;
#48869 = EDGE_LOOP ( 'NONE', ( #61611, #110674, #100793, #79355, #83628 ) ) ;
#48870 = CARTESIAN_POINT ( 'NONE',  ( -0.05401770104373219972, 1452.351257629399925, 183.2652781389920165 ) ) ;
#48871 = CARTESIAN_POINT ( 'NONE',  ( 7.801033191672110512, 1428.789703093460048, 214.5172910005400126 ) ) ;
#48872 = CARTESIAN_POINT ( 'NONE',  ( -10.22326110114815556, 1375.913060387289988, 213.8507217284212345 ) ) ;
#48873 = CARTESIAN_POINT ( 'NONE',  ( -10.61991956690710026, 1462.990895942619773, 206.0507601276690082 ) ) ;
#48874 = CARTESIAN_POINT ( 'NONE',  ( -13.20685506100000062, 1422.970547187230068, 222.0985264004979740 ) ) ;
#48875 = EDGE_CURVE ( 'NONE', #54897, #65239, #10587, .T. ) ;
#48876 = CARTESIAN_POINT ( 'NONE',  ( 13.07458372279550041, 1436.035484542389895, 150.7116094860570001 ) ) ;
#48877 = CARTESIAN_POINT ( 'NONE',  ( -0.8107957177449999220, 1507.658530268329969, 180.8255026719979810 ) ) ;
#48878 = CARTESIAN_POINT ( 'NONE',  ( -11.94171318070000076, 1433.614828344400166, 146.4341822532980188 ) ) ;
#48879 = CARTESIAN_POINT ( 'NONE',  ( -19.63708787179735538, 1526.382868172863937, 183.4208852702759884 ) ) ;
#48881 = CARTESIAN_POINT ( 'NONE',  ( -10.16646205815034953, 1422.467730556536253, 137.0999999980976725 ) ) ;
#48880 = CARTESIAN_POINT ( 'NONE',  ( 15.43028253750000189, 1459.840836958929913, 230.9090760540979943 ) ) ;
#48882 = DIRECTION ( 'NONE',  ( 0.8775825618903700942, 0.000000000000000000, -0.4794255386042075018 ) ) ;
#48883 = CARTESIAN_POINT ( 'NONE',  ( -1.125509888415000104, 1517.203017563489766, 216.4609531728469847 ) ) ;
#48884 = ORIENTED_EDGE ( 'NONE', *, *, #7006, .T. ) ;
#48885 = DIRECTION ( 'NONE',  ( -0.8672669759446595128, -0.000000000000000000, 0.4978433412588795237 ) ) ;
#48886 = CARTESIAN_POINT ( 'NONE',  ( -0.05571092667383620300, 1508.705957002570130, 179.9923125561219877 ) ) ;
#48887 = CARTESIAN_POINT ( 'NONE',  ( -21.55491250604931608, 1524.059663615499630, 234.2080302846968891 ) ) ;
#48888 = CARTESIAN_POINT ( 'NONE',  ( -6.935457963315000640, 1516.627618683580067, 212.5772239474869991 ) ) ;
#48889 = CARTESIAN_POINT ( 'NONE',  ( 4.136749811987169956, 1515.492902828930028, 212.0199439695689989 ) ) ;
#48890 = CARTESIAN_POINT ( 'NONE',  ( -11.60004869885203682, 1426.109592824957417, 139.1549331605903035 ) ) ;
#48892 = VERTEX_POINT ( 'NONE', #45313 ) ;
#48891 = CARTESIAN_POINT ( 'NONE',  ( 4.369720457535109404, 1508.879003890470131, 213.2412450826520001 ) ) ;
#48893 = CARTESIAN_POINT ( 'NONE',  ( -16.64711273905149724, 1523.843263703803132, 237.7438622704431737 ) ) ;
#48894 = CARTESIAN_POINT ( 'NONE',  ( 3.406451235749999640, 1507.508084657790050, 220.3277233380989912 ) ) ;
#48895 = EDGE_CURVE ( 'NONE', #103816, #33631, #67720, .T. ) ;
#48896 = CARTESIAN_POINT ( 'NONE',  ( -11.86497210549999970, 1432.257141527180011, 149.9820204226980138 ) ) ;
#48897 = CARTESIAN_POINT ( 'NONE',  ( 19.13240566025299927, 1456.933378143550044, 225.0294012906809940 ) ) ;
#48898 = CARTESIAN_POINT ( 'NONE',  ( -5.466351949607379801, 1442.136625457690116, 201.6172741276789964 ) ) ;
#48899 = CARTESIAN_POINT ( 'NONE',  ( -18.62956325327520091, 1444.934402157219893, 206.0431600358409980 ) ) ;
#48900 = CARTESIAN_POINT ( 'NONE',  ( -7.866319717195060512, 1425.555983808420024, 204.1407689886210051 ) ) ;
#48901 = CARTESIAN_POINT ( 'NONE',  ( 12.13521690389999996, 1446.772554461140089, 188.0265662329979932 ) ) ;
#48902 = EDGE_CURVE ( 'NONE', #24522, #77826, #11989, .T. ) ;
#48904 = CARTESIAN_POINT ( 'NONE',  ( -17.70278889250000276, 1504.268309054989913, 209.3612281098589847 ) ) ;
#48903 = CARTESIAN_POINT ( 'NONE',  ( -24.77779169540000126, 1482.720791717229986, 217.1592320706580210 ) ) ;
#48905 = CARTESIAN_POINT ( 'NONE',  ( -2.446862982530000341, 1485.861691786529946, 182.3251207059980175 ) ) ;
#48906 = ORIENTED_EDGE ( 'NONE', *, *, #1457, .T. ) ;
#48907 = CARTESIAN_POINT ( 'NONE',  ( -1.135185082175000026, 1516.778853242349896, 205.6747174714770097 ) ) ;
#48908 = CARTESIAN_POINT ( 'NONE',  ( 9.910131830190000102, 1406.621495965729991, 267.1956846989980363 ) ) ;
#48909 = CARTESIAN_POINT ( 'NONE',  ( 0.3331931608689999713, 1408.924695757129939, 186.0526652876979767 ) ) ;
#48910 = CARTESIAN_POINT ( 'NONE',  ( -7.105427357599999217E-15, 1410.913060387329779, 137.0999999980979851 ) ) ;
#48911 = EDGE_CURVE ( 'NONE', #49402, #46101, #82004, .T. ) ;
#48912 = CARTESIAN_POINT ( 'NONE',  ( 23.63185289614832385, 1434.172427200277298, 214.7039615058700690 ) ) ;
#48913 = CARTESIAN_POINT ( 'NONE',  ( -8.107194294532323653, 1387.417305483015980, 218.5499404544749211 ) ) ;
#48914 = CARTESIAN_POINT ( 'NONE',  ( 28.13477516149999857, 1508.112005763430034, 210.1092937961579992 ) ) ;
#48915 = CARTESIAN_POINT ( 'NONE',  ( -10.19077500720859852, 1447.300597530319919, 210.8667737859159956 ) ) ;
#48916 = CARTESIAN_POINT ( 'NONE',  ( -2.434526125190220380, 1449.527760103650053, 155.0642341674960107 ) ) ;
#48917 = FACE_OUTER_BOUND ( 'NONE', #79734, .T. ) ;
#48918 = CARTESIAN_POINT ( 'NONE',  ( -19.88572122277579979, 1484.728771715989751, 191.0592865161910083 ) ) ;
#48919 = CARTESIAN_POINT ( 'NONE',  ( -14.09832007171429957, 1415.595619977640126, 221.0238313356500157 ) ) ;
#48920 = DIRECTION ( 'NONE',  ( 1.962482049179999770E-13, -8.350987443300000121E-15, -1.000000000000000000 ) ) ;
#48921 = CARTESIAN_POINT ( 'NONE',  ( -8.555769954617961304, 1409.211834457770010, 196.8452873928659983 ) ) ;
#48922 = EDGE_CURVE ( 'NONE', #15037, #97242, #98153, .T. ) ;
#48923 = CARTESIAN_POINT ( 'NONE',  ( -26.91728171915830004, 1508.004642862799983, 211.7160872265129967 ) ) ;
#48924 = CARTESIAN_POINT ( 'NONE',  ( 3.118963903650000091, 1441.197690497029953, 165.1033354352979927 ) ) ;
#48925 = CARTESIAN_POINT ( 'NONE',  ( -3.441725452600000068, 1475.954703585829975, 268.4787010635980096 ) ) ;
#48926 = CARTESIAN_POINT ( 'NONE',  ( -4.242885033098620085, 1446.408270998030048, 162.3196225285890080 ) ) ;
#48927 = CARTESIAN_POINT ( 'NONE',  ( -15.15772398740000071, 1439.441663529990137, 221.0618115286989962 ) ) ;
#48928 = EDGE_CURVE ( 'NONE', #94174, #22669, #65973, .T. ) ;
#48929 = CARTESIAN_POINT ( 'NONE',  ( -18.43055515643429842, 1486.478983240757998, 188.6801967137396616 ) ) ;
#48930 = CARTESIAN_POINT ( 'NONE',  ( -55.04194086205259850, 1384.716586501660004, 271.8950046832100043 ) ) ;
#48931 = CARTESIAN_POINT ( 'NONE',  ( -106.6599773620300056, 1391.913060387289988, 302.5710412761980024 ) ) ;
#48932 = DIRECTION ( 'NONE',  ( -1.755985294532469921E-16, 1.000000000000000000, -1.338183447452831989E-16 ) ) ;
#48933 = CARTESIAN_POINT ( 'NONE',  ( -106.7897227899999990, 1379.694571751269905, 299.8550812676590454 ) ) ;
#48934 = CARTESIAN_POINT ( 'NONE',  ( 32.05523756949320813, 1525.253972588461465, 217.0243587599946409 ) ) ;
#48935 = CARTESIAN_POINT ( 'NONE',  ( 8.652776089875690246, 1511.435001055579960, 203.7363227723449768 ) ) ;
#48936 = CARTESIAN_POINT ( 'NONE',  ( -18.88112913370000001, 1409.572403950229955, 198.2284472637979889 ) ) ;
#48937 = CARTESIAN_POINT ( 'NONE',  ( -15.23233646464800195, 1422.123670831245818, 227.7537345013419952 ) ) ;
#48938 = CARTESIAN_POINT ( 'NONE',  ( -9.999959670399999112, 1407.452792677830075, 269.6172309327980088 ) ) ;
#48939 = ORIENTED_EDGE ( 'NONE', *, *, #22039, .F. ) ;
#48940 = CARTESIAN_POINT ( 'NONE',  ( -19.83859993069999916, 1467.194195006989958, 209.1218459616989946 ) ) ;
#48941 = CARTESIAN_POINT ( 'NONE',  ( 28.25086641300000068, 1508.135711190629991, 209.3856964555159834 ) ) ;
#48942 = CARTESIAN_POINT ( 'NONE',  ( -3.005262499256480258, 1450.300071509800091, 188.5532295967200014 ) ) ;
#48944 = CARTESIAN_POINT ( 'NONE',  ( -13.44545695640730010, 1379.581665062349884, 211.7224066084869776 ) ) ;
#48943 = CARTESIAN_POINT ( 'NONE',  ( 10.70806905399999920, 1424.991205926329940, 137.4294028545979813 ) ) ;
#48945 = CARTESIAN_POINT ( 'NONE',  ( 16.51370421206613059, 1525.137906803776559, 237.1983439667824030 ) ) ;
#48946 = LINE ( 'NONE', #66307, #29415 ) ;
#48947 = CARTESIAN_POINT ( 'NONE',  ( 39.20827873999350288, 1450.609082524699943, 136.0286972522910105 ) ) ;
#48948 = AXIS2_PLACEMENT_3D ( 'NONE', #43048, #25108, #43596 ) ;
#48949 = CARTESIAN_POINT ( 'NONE',  ( -2.486474780875000512, 1516.560253536979872, 202.1879665292270261 ) ) ;
#48950 = CARTESIAN_POINT ( 'NONE',  ( 7.231061069169999911, 1427.019244165460123, 212.9903255762889955 ) ) ;
#48951 = CARTESIAN_POINT ( 'NONE',  ( -7.255983564230000127, 1427.866122641229822, 147.4806042202980052 ) ) ;
#48952 = CARTESIAN_POINT ( 'NONE',  ( 15.84317032663500058, 1513.136578080079744, 194.8016171615669805 ) ) ;
#48953 = CARTESIAN_POINT ( 'NONE',  ( -20.61542114843588536, 1508.364347659817440, 190.3921826368226675 ) ) ;
#48954 = CARTESIAN_POINT ( 'NONE',  ( -3.771520277320000503, 1377.099040908540019, 211.4935541149690152 ) ) ;
#48955 = CARTESIAN_POINT ( 'NONE',  ( 21.32616491865039876, 1509.431678241010104, 227.8426383757489759 ) ) ;
#48957 = VERTEX_POINT ( 'NONE', #89489 ) ;
#48956 = CARTESIAN_POINT ( 'NONE',  ( -43.47249194799999827, 1379.734446420929999, 233.2730947026589661 ) ) ;
#48958 = ORIENTED_EDGE ( 'NONE', *, *, #47350, .T. ) ;
#48959 = CARTESIAN_POINT ( 'NONE',  ( 11.92728121149999865, 1433.973591798999905, 150.6941211948980026 ) ) ;
#48960 = CARTESIAN_POINT ( 'NONE',  ( -10.69384198020000021, 1396.286497578129911, 212.3513119892680265 ) ) ;
#48961 = CARTESIAN_POINT ( 'NONE',  ( -18.45264828540000224, 1409.557441064630211, 220.8691094444980081 ) ) ;
#48962 = EDGE_LOOP ( 'NONE', ( #84356, #41022, #97297, #23740 ) ) ;
#48963 = CARTESIAN_POINT ( 'NONE',  ( -12.85133220204726001, 1444.958534272496763, 169.4430044350944513 ) ) ;
#48964 = CARTESIAN_POINT ( 'NONE',  ( 22.24050427028109311, 1509.699967146265180, 228.5561123524984168 ) ) ;
#48965 = CARTESIAN_POINT ( 'NONE',  ( -7.629870583244999338, 1512.332007210709889, 211.6709574174969930 ) ) ;
#48967 = CARTESIAN_POINT ( 'NONE',  ( -13.70786035851040019, 1507.754328159320039, 184.2519299535370010 ) ) ;
#48966 = CARTESIAN_POINT ( 'NONE',  ( 1.234729273729999965, 1445.364456438190018, 199.0923708265989944 ) ) ;
#48968 = CARTESIAN_POINT ( 'NONE',  ( 0.3355459311639999997, 1449.243710373649947, 183.3896813568979951 ) ) ;
#48969 = CARTESIAN_POINT ( 'NONE',  ( -10.07457507059999813, 1416.825421875629900, 193.4554633978979723 ) ) ;
#48970 = CARTESIAN_POINT ( 'NONE',  ( -1.139751506879999932, 1423.243574032600009, 191.2093741592990170 ) ) ;
#48971 = SURFACE_STYLE_USAGE ( .BOTH. , #49519 ) ;
#48972 = B_SPLINE_SURFACE_WITH_KNOTS ( 'NONE', 2, 5, ( 
 ( #22252, #90582, #73812, #4926, #39070, #73246 ),
 ( #13863, #107941, #106830, #99521, #71640, #22806 ),
 ( #64315, #46963, #106292, #55357, #89490, #12784 ) ),
 .UNSPECIFIED., .F., .F., .F.,
 ( 3, 3 ),
 ( 6, 6 ),
 ( 72.92379873290001058, 73.89199858150000466 ),
 ( 0.000000000000000000, 2.000000000000000000 ),
 .UNSPECIFIED. ) ;
#48973 = CARTESIAN_POINT ( 'NONE',  ( 9.707456031250101702, 1396.252052236789723, 203.8125232392220028 ) ) ;
#48974 = CARTESIAN_POINT ( 'NONE',  ( 1.159637561179999832, 1415.063410489729904, 191.5788536471979739 ) ) ;
#48975 = CARTESIAN_POINT ( 'NONE',  ( 10.86749701439999960, 1425.819625802929977, 148.2249929719979775 ) ) ;
#48976 = CARTESIAN_POINT ( 'NONE',  ( 7.660003937574999533, 1511.444830760690138, 203.0229484186070010 ) ) ;
#48977 = EDGE_LOOP ( 'NONE', ( #35164, #12442, #81181, #50526, #13264, #41821 ) ) ;
#48978 = CARTESIAN_POINT ( 'NONE',  ( 13.08958089826340121, 1434.843138717199963, 149.4032511664449885 ) ) ;
#48979 = ORIENTED_EDGE ( 'NONE', *, *, #108387, .F. ) ;
#48980 = ORIENTED_EDGE ( 'NONE', *, *, #104250, .F. ) ;
#48981 = CARTESIAN_POINT ( 'NONE',  ( -17.84980107695580287, 1458.247813499710219, 228.0953541232100008 ) ) ;
#48982 = CARTESIAN_POINT ( 'NONE',  ( -8.298541131280000371, 1464.648652832329844, 233.2149708747980128 ) ) ;
#48983 = CARTESIAN_POINT ( 'NONE',  ( -107.4005018563592273, 1389.804008732182183, 309.3201767723587068 ) ) ;
#48984 = CARTESIAN_POINT ( 'NONE',  ( -2.483322492024999661, 1517.139039350860003, 215.6851008610869940 ) ) ;
#48985 = CARTESIAN_POINT ( 'NONE',  ( -13.17437943089760033, 1379.876859876259914, 208.7616546775940094 ) ) ;
#48986 = ORIENTED_EDGE ( 'NONE', *, *, #65112, .F. ) ;
#48987 = CARTESIAN_POINT ( 'NONE',  ( -12.40467953689999980, 1502.876200019789849, 208.6411846686590081 ) ) ;
#48988 = CARTESIAN_POINT ( 'NONE',  ( 2.500000000000000000, 1448.200164369519825, 169.1292575994999936 ) ) ;
#48989 = CARTESIAN_POINT ( 'NONE',  ( -59.84652512769999788, 1375.824862300619998, 258.3077303912590423 ) ) ;
#48990 = ORIENTED_EDGE ( 'NONE', *, *, #63669, .T. ) ;
#48991 = CARTESIAN_POINT ( 'NONE',  ( 2.284526458645000258, 1516.956048353049937, 205.6588971355569981 ) ) ;
#48992 = ORIENTED_EDGE ( 'NONE', *, *, #50710, .T. ) ;
#48993 = CARTESIAN_POINT ( 'NONE',  ( 6.949703334655000120, 1517.130100026000036, 209.8609679372960102 ) ) ;
#48994 = CARTESIAN_POINT ( 'NONE',  ( -20.67559711379999854, 1509.531575931029920, 229.8721981546979976 ) ) ;
#48995 = CARTESIAN_POINT ( 'NONE',  ( -18.44378729667023009, 1413.503667190741908, 269.3810517491084511 ) ) ;
#48996 = CARTESIAN_POINT ( 'NONE',  ( 6.169347524795000481, 1511.326779185850000, 216.6603264655069836 ) ) ;
#48997 = B_SPLINE_CURVE_WITH_KNOTS ( 'NONE', 3,
 ( #32543, #30326, #64515, #5127, #75112, #24109, #6226, #40381, #47696, #58301, #99721, #100822, #21898, #22449, #92423, #74558, #13508, #4591, #38724, #81824, #72899, #107589, #31983, #107039, #82398, #108691, #90783, #66173, #39839, #23014, #100293, #23574, #39283, #74002, #57767, #108134, #31427, #73458, #91886, #30875, #65054, #56650, #48255, #15159, #6770, #40934, #109259, #17914, #607 ),
 .UNSPECIFIED., .F., .F.,
 ( 4, 2, 1, 2, 2, 2, 1, 1, 2, 2, 2, 2, 1, 1, 1, 2, 2, 2, 2, 1, 1, 1, 2, 2, 2, 1, 1, 2, 2, 4 ),
 ( 0.000000000000000000, 0.06249999999932660810, 0.09374999999899018277, 0.1093749999988207072, 0.1249999999986512178, 0.1874999999982259469, 0.2187499999980131726, 0.2343749999978273768, 0.2421874999977315923, 0.2499999999976357801, 0.3749999999976260656, 0.4374999999976176834, 0.4687499999975849874, 0.4843749999975918707, 0.4921874999975986431, 0.4960937499975791587, 0.4999999999975597298, 0.6249999999982577270, 0.6874999999986254329, 0.7187499999988058441, 0.7343749999988899990, 0.7421874999989331867, 0.7460937499989542809, 0.7499999999989752641, 0.8124999999992322808, 0.8437499999993610666, 0.8593749999994289013, 0.8671874999994627631, 0.8749999999994966249, 1.000000000000000000 ),
 .UNSPECIFIED. ) ;
#48999 = VERTEX_POINT ( 'NONE', #107386 ) ;
#48998 = CARTESIAN_POINT ( 'NONE',  ( 0.08022770239931510672, 1416.524489948229984, 227.2134237566240245 ) ) ;
#49000 = DIRECTION ( 'NONE',  ( 9.261055619630009070E-47, -1.000000000000000000, 1.836970198721029688E-16 ) ) ;
#49001 = CARTESIAN_POINT ( 'NONE',  ( -30.26655853036449884, 1440.913060387089899, 239.1917914571189954 ) ) ;
#49002 = CARTESIAN_POINT ( 'NONE',  ( -81.27653993580000247, 1383.775959360260003, 304.8043613862590746 ) ) ;
#49003 = CARTESIAN_POINT ( 'NONE',  ( -0.06241017250561379376, 1466.769691485820204, 235.6256240966490054 ) ) ;
#49004 = CARTESIAN_POINT ( 'NONE',  ( 7.240562320799770468, 1410.843301754160166, 269.3412962850030112 ) ) ;
#49005 = CARTESIAN_POINT ( 'NONE',  ( -2.867803664234999772, 1516.994127245590107, 213.7465828294170080 ) ) ;
#49006 = CARTESIAN_POINT ( 'NONE',  ( 22.91622274789999736, 1409.721715511730054, 209.0611398913850110 ) ) ;
#49007 = CARTESIAN_POINT ( 'NONE',  ( 29.55269881708361979, 1525.821544997590536, 197.1295836072963539 ) ) ;
#49008 = CARTESIAN_POINT ( 'NONE',  ( 2.975355613810000133, 1441.383001986190038, 218.5845790346389776 ) ) ;
#49009 = CARTESIAN_POINT ( 'NONE',  ( -7.709324863577120546, 1516.545501335879862, 211.7787317697519995 ) ) ;
#49010 = CARTESIAN_POINT ( 'NONE',  ( 6.564578685215000320, 1517.199196846569976, 210.8299485595169926 ) ) ;
#49011 = CARTESIAN_POINT ( 'NONE',  ( -2.506258803592136264, 1448.698841201256073, 154.6270693172046151 ) ) ;
#49012 = CARTESIAN_POINT ( 'NONE',  ( 0.4863422716760000264, 1418.702333073229966, 184.7128037028979861 ) ) ;
#49013 = CARTESIAN_POINT ( 'NONE',  ( 1.160687054150907116, 1409.478223960041987, 232.4137843514840824 ) ) ;
#49015 = ORIENTED_EDGE ( 'NONE', *, *, #63868, .T. ) ;
#49014 = CARTESIAN_POINT ( 'NONE',  ( -77.04812550189998888, 1389.484839475800072, 284.7597100018589913 ) ) ;
#49016 = CARTESIAN_POINT ( 'NONE',  ( -41.13573424065770467, 1385.175475063010026, 244.1333310952810223 ) ) ;
#49017 = EDGE_CURVE ( 'NONE', #80871, #37685, #78177, .T. ) ;
#49018 = CARTESIAN_POINT ( 'NONE',  ( 37.00351967400000319, 1461.786612606330209, 266.5576464536979984 ) ) ;
#49019 = EDGE_CURVE ( 'NONE', #31779, #23279, #106291, .T. ) ;
#49020 = DIRECTION ( 'NONE',  ( -0.4794255386042027833, 0.000000000000000000, 0.8775825618903728698 ) ) ;
#49021 = CARTESIAN_POINT ( 'NONE',  ( -17.28556289930000034, 1479.740378035829963, 228.8535607617980361 ) ) ;
#49022 = CARTESIAN_POINT ( 'NONE',  ( -5.423605666139999393, 1436.253592627979742, 154.6924226254979828 ) ) ;
#49023 = CARTESIAN_POINT ( 'NONE',  ( 12.66524796160000044, 1426.904560545630147, 205.5255884876389985 ) ) ;
#49024 = CARTESIAN_POINT ( 'NONE',  ( -0.4036693690347583630, 1498.351677242009828, 197.8065570372807827 ) ) ;
#49025 = AXIS2_PLACEMENT_3D ( 'NONE', #16595, #95549, #85470 ) ;
#49027 = DIRECTION ( 'NONE',  ( 3.531714064933559186E-16, 1.000000000000000000, 0.000000000000000000 ) ) ;
#49026 = CARTESIAN_POINT ( 'NONE',  ( -2.290256301855000398, 1517.170721208160103, 216.0730210990169837 ) ) ;
#49028 = CARTESIAN_POINT ( 'NONE',  ( 18.66420869458061205, 1526.382868172863937, 232.7837831374278039 ) ) ;
#49029 = CARTESIAN_POINT ( 'NONE',  ( 10.56467116463950084, 1423.845360445598999, 137.4573436676088818 ) ) ;
#49030 = ORIENTED_EDGE ( 'NONE', *, *, #84235, .F. ) ;
#49031 = CARTESIAN_POINT ( 'NONE',  ( 3.452289182574999948, 1517.069378699710114, 202.5601595088670024 ) ) ;
#49032 = CARTESIAN_POINT ( 'NONE',  ( -16.30040994386499875, 1513.841826332629807, 223.7820414851669852 ) ) ;
#49033 = DIRECTION ( 'NONE',  ( 0.000000000000000000, 1.000000000000000000, 0.000000000000000000 ) ) ;
#49034 = CIRCLE ( 'NONE', #16754, 2.458500000000000352 ) ;
#49035 = EDGE_CURVE ( 'NONE', #98070, #92390, #58793, .T. ) ;
#49036 = CARTESIAN_POINT ( 'NONE',  ( 23.35526608410000193, 1448.827836771670036, 218.6598503475479731 ) ) ;
#49037 = CARTESIAN_POINT ( 'NONE',  ( 10.78159844869479933, 1461.896569297480028, 211.1674770051990038 ) ) ;
#49038 = CARTESIAN_POINT ( 'NONE',  ( 8.375776142020290749, 1424.393421303552714, 195.8297818163817112 ) ) ;
#49039 = CARTESIAN_POINT ( 'NONE',  ( -0.7466494764550010155, 1444.875944096290141, 218.0743976162490014 ) ) ;
#49040 = CARTESIAN_POINT ( 'NONE',  ( 11.66756983127008063, 1418.593453235695961, 229.5266030089004516 ) ) ;
#49041 = CARTESIAN_POINT ( 'NONE',  ( 38.47356468767819848, 1448.369015667859912, 136.4419166358019879 ) ) ;
#49042 = CARTESIAN_POINT ( 'NONE',  ( -18.65431773610000121, 1425.340119975330026, 225.0950243718980062 ) ) ;
#49043 = CARTESIAN_POINT ( 'NONE',  ( -30.50754839409947650, 1466.330398693723737, 269.3461395109432033 ) ) ;
#49044 = CARTESIAN_POINT ( 'NONE',  ( -104.4016991209999929, 1389.881826709800180, 301.9201043558590527 ) ) ;
#49045 = CARTESIAN_POINT ( 'NONE',  ( -17.23770320690000091, 1413.292237373229909, 226.2052584196979979 ) ) ;
#49046 = CARTESIAN_POINT ( 'NONE',  ( 0.0001165990426140000018, 1408.913064459030011, 231.7797585373979814 ) ) ;
#49047 = CARTESIAN_POINT ( 'NONE',  ( -28.45928379452146473, 1463.335201769019932, 269.4551648148650429 ) ) ;
#49048 = ORIENTED_EDGE ( 'NONE', *, *, #70715, .F. ) ;
#49049 = CARTESIAN_POINT ( 'NONE',  ( -4.304798037349998904E-15, 1432.353341358199941, 150.3995506339979897 ) ) ;
#49051 = CARTESIAN_POINT ( 'NONE',  ( 8.861632801989001607, 1506.578946199044594, 188.8712608442579608 ) ) ;
#49050 = B_SPLINE_CURVE_WITH_KNOTS ( 'NONE', 3,
 ( #41510, #32556, #100835, #58314, #50472, #82416, #92436, #15712, #84048, #42058, #7347, #39855 ),
 .UNSPECIFIED., .F., .F.,
 ( 4, 2, 2, 2, 2, 4 ),
 ( -0.09623281651891979482, -0.08712861168082250418, -0.07809605755948040295, -0.05948248759999250068, -0.03461062426328559427, -2.460911216473071761E-08 ),
 .UNSPECIFIED. ) ;
#49052 = CARTESIAN_POINT ( 'NONE',  ( 11.16354646297939901, 1470.309690817349747, 207.0219044217840008 ) ) ;
#49053 = CARTESIAN_POINT ( 'NONE',  ( 11.41287573240554032, 1427.618782186570115, 209.6357587079445182 ) ) ;
#49054 = CARTESIAN_POINT ( 'NONE',  ( -1.804213505890000180, 1410.351307731129964, 186.0507930254979954 ) ) ;
#49055 = CARTESIAN_POINT ( 'NONE',  ( -13.51254418754115427, 1443.799311687372438, 187.1419075245657666 ) ) ;
#49056 = ADVANCED_FACE ( 'NONE', ( #98433 ), #6960, .T. ) ;
#49057 = CARTESIAN_POINT ( 'NONE',  ( -8.833352578285419199, 1438.178637326770058, 209.2923841634130042 ) ) ;
#49058 = CARTESIAN_POINT ( 'NONE',  ( -4.138326087764060190, 1515.492270357739926, 211.4517668545689730 ) ) ;
#49059 = LINE ( 'NONE', #73145, #50347 ) ;
#49060 = CARTESIAN_POINT ( 'NONE',  ( -106.4346700481279981, 1383.759796027640050, 311.0497744043260013 ) ) ;
#49061 = CARTESIAN_POINT ( 'NONE',  ( 17.60594182058157386, 1424.146952378337346, 228.5308900134957071 ) ) ;
#49063 = EDGE_CURVE ( 'NONE', #105370, #32165, #17636, .T. ) ;
#49062 = CARTESIAN_POINT ( 'NONE',  ( -12.61661106525792952, 1442.788675913401448, 169.4674439222872024 ) ) ;
#49065 = ORIENTED_EDGE ( 'NONE', *, *, #72591, .T. ) ;
#49064 = CARTESIAN_POINT ( 'NONE',  ( 18.28672154731980015, 1425.324301384940100, 225.4653420784370326 ) ) ;
#49066 = CARTESIAN_POINT ( 'NONE',  ( 0.4156091144216609856, 1414.971513442450032, 192.3333892557660079 ) ) ;
#49067 = CARTESIAN_POINT ( 'NONE',  ( -0.9647690717699999308, 1408.946750865729882, 231.5874088180979982 ) ) ;
#49068 = ORIENTED_EDGE ( 'NONE', *, *, #82333, .F. ) ;
#49069 = ORIENTED_EDGE ( 'NONE', *, *, #30443, .T. ) ;
#49070 = CARTESIAN_POINT ( 'NONE',  ( 17.65703761238349756, 1415.429375168339902, 209.4485410505009781 ) ) ;
#49071 = CARTESIAN_POINT ( 'NONE',  ( 13.43167055049999981, 1509.382104692529992, 235.1752292677980165 ) ) ;
#49073 = CARTESIAN_POINT ( 'NONE',  ( -25.74056229059999978, 1440.913060583030074, 220.8687942643980193 ) ) ;
#49072 = CARTESIAN_POINT ( 'NONE',  ( 4.199771657899999511, 1453.975215170089996, 217.5101452743190009 ) ) ;
#49074 = CARTESIAN_POINT ( 'NONE',  ( -20.55886062980000162, 1506.532306263230112, 190.1125840497979880 ) ) ;
#49075 = CARTESIAN_POINT ( 'NONE',  ( -11.82447129959999899, 1433.241336066939994, 150.5548711859979676 ) ) ;
#49076 = CARTESIAN_POINT ( 'NONE',  ( -9.867588125367669605, 1445.429986924526702, 184.5009753814391615 ) ) ;
#49077 = CARTESIAN_POINT ( 'NONE',  ( 27.88515232864000026, 1499.645912665409924, 209.4023683382970091 ) ) ;
#49078 = CARTESIAN_POINT ( 'NONE',  ( -26.46046315050000075, 1441.626270684899964, 137.7338459625980249 ) ) ;
#49079 = CARTESIAN_POINT ( 'NONE',  ( -24.24596083330000340, 1438.629152405760124, 212.1147215154179833 ) ) ;
#49080 = CARTESIAN_POINT ( 'NONE',  ( -4.187288789294350444, 1453.810560376779904, 199.5230725183479876 ) ) ;
#49081 = CARTESIAN_POINT ( 'NONE',  ( 1.546925190270000083, 1450.646712626299859, 182.0032008381979836 ) ) ;
#49082 = CARTESIAN_POINT ( 'NONE',  ( 8.631039101008498804, 1364.365412828926765, 210.6218459617142003 ) ) ;
#49083 = CARTESIAN_POINT ( 'NONE',  ( -28.15666966853906672, 1510.007892114357674, 198.7595920586345244 ) ) ;
#49085 = EDGE_LOOP ( 'NONE', ( #94374, #91601, #61263, #19981, #52713 ) ) ;
#49084 = DIRECTION ( 'NONE',  ( -1.755985294532469921E-16, 1.000000000000000000, -1.338183447452831989E-16 ) ) ;
#49086 = VERTEX_POINT ( 'NONE', #82742 ) ;
#49087 = CARTESIAN_POINT ( 'NONE',  ( -2.161027938733468545, 1508.551740403373060, 220.4424620650312363 ) ) ;
#49088 = CARTESIAN_POINT ( 'NONE',  ( -21.44083287200000143, 1507.004319579390085, 216.1313484145690040 ) ) ;
#49089 = CARTESIAN_POINT ( 'NONE',  ( -3.196891731540000059, 1474.092834640029878, 270.1354749226979379 ) ) ;
#49090 = DIRECTION ( 'NONE',  ( -0.000000000000000000, -1.000000000000000000, -0.000000000000000000 ) ) ;
#49091 =( BOUNDED_CURVE ( )  B_SPLINE_CURVE ( 3, ( #16631, #15539, #49738, #76025 ),
 .UNSPECIFIED., .F., .T. ) 
 B_SPLINE_CURVE_WITH_KNOTS ( ( 4, 4 ),
 ( 1.008471431651680073, 2.133121240772390070 ),
 .UNSPECIFIED. ) 
 CURVE ( )  GEOMETRIC_REPRESENTATION_ITEM ( )  RATIONAL_B_SPLINE_CURVE ( ( 1.000000000000000000, 0.8973452434195507976, 0.8973452434195507976, 1.000000000000000000 ) ) 
 REPRESENTATION_ITEM ( '' )  );
#49092 = CARTESIAN_POINT ( 'NONE',  ( -121.4211954113599461, 1309.112692017089330, 302.1736985104333257 ) ) ;
#49093 = CARTESIAN_POINT ( 'NONE',  ( 37.13154625033060086, 1450.996886497350033, 135.1616079744260048 ) ) ;
#49094 = DIRECTION ( 'NONE',  ( 0.000000000000000000, 1.000000000000000000, 0.000000000000000000 ) ) ;
#49095 = CARTESIAN_POINT ( 'NONE',  ( -20.60448988230000111, 1484.737042837089803, 209.1218459616989946 ) ) ;
#49096 = DIRECTION ( 'NONE',  ( -0.001614263105659359630, 0.06164622090537578980, 0.9980967576356069015 ) ) ;
#49097 = CARTESIAN_POINT ( 'NONE',  ( -3.550708236880000257, 1457.374719892490020, 218.1022976105089981 ) ) ;
#49098 = CARTESIAN_POINT ( 'NONE',  ( 11.08126538406277461, 1363.947071503807592, 210.6218459617030021 ) ) ;
#49099 = CARTESIAN_POINT ( 'NONE',  ( -43.70846434600260011, 1429.985737363310136, 268.5715736658989954 ) ) ;
#49100 = ORIENTED_EDGE ( 'NONE', *, *, #10427, .F. ) ;
#49101 = CARTESIAN_POINT ( 'NONE',  ( -4.329448781177520189, 1515.064792686469900, 210.9648092169189795 ) ) ;
#49102 = CIRCLE ( 'NONE', #61656, 2.000175714736120991 ) ;
#49103 = ORIENTED_EDGE ( 'NONE', *, *, #52259, .T. ) ;
#49104 = ORIENTED_EDGE ( 'NONE', *, *, #101584, .T. ) ;
#49105 = CARTESIAN_POINT ( 'NONE',  ( 0.7578857918350010436, 1516.872851364150165, 211.6022732247369902 ) ) ;
#49106 = CARTESIAN_POINT ( 'NONE',  ( 4.639095080327251708, 1423.703679602264856, 183.8752827255912052 ) ) ;
#49107 = CARTESIAN_POINT ( 'NONE',  ( -108.3070719650000058, 1383.318204079829911, 297.4475841893589632 ) ) ;
#49109 = CYLINDRICAL_SURFACE ( 'NONE', #65124, 1.999999999999999556 ) ;
#49108 = CARTESIAN_POINT ( 'NONE',  ( -2.865588722415000067, 1516.890356958860139, 212.3900816908670208 ) ) ;
#49110 = CARTESIAN_POINT ( 'NONE',  ( -13.58956681059999916, 1455.448334937230129, 187.8199450490979814 ) ) ;
#49111 = AXIS2_PLACEMENT_3D ( 'NONE', #80903, #80356, #38331 ) ;
#49112 = CARTESIAN_POINT ( 'NONE',  ( -11.60004869885203682, 1428.983126981193436, 135.0999999980979851 ) ) ;
#49113 = B_SPLINE_SURFACE_WITH_KNOTS ( 'NONE', 5, 1, ( 
 ( #66049, #5006 ),
 ( #22884, #57094 ),
 ( #12854, #91219 ),
 ( #47035, #72784 ),
 ( #107462, #55981 ),
 ( #39153, #62574 ) ),
 .UNSPECIFIED., .F., .F., .F.,
 ( 6, 6 ),
 ( 2, 2 ),
 ( 0.000000000000000000, 14.21110430600000107 ),
 ( 0.000000000000000000, 14.00000000000000000 ),
 .UNSPECIFIED. ) ;
#49114 = EDGE_LOOP ( 'NONE', ( #27409, #16634, #55143, #47607 ) ) ;
#49115 = CARTESIAN_POINT ( 'NONE',  ( -26.79697582150000201, 1435.433282762789986, 135.3785755500979917 ) ) ;
#49116 = CARTESIAN_POINT ( 'NONE',  ( 4.034280915654999689, 1517.049325831759916, 202.1735242262370207 ) ) ;
#49117 = B_SPLINE_SURFACE_WITH_KNOTS ( 'NONE', 5, 5, ( 
 ( #104832, #53916, #2954, #105389, #62884, #9650 ),
 ( #96996, #95329, #20259, #77971, #54459, #88596 ),
 ( #1278, #35418, #18590, #52785, #86922, #10213 ),
 ( #44390, #78533, #1844, #35979, #70170, #5116 ),
 ( #38171, #14616, #39272, #72889, #47686, #91331 ),
 ( #5685, #23003, #55548, #106481, #20806, #81814 ) ),
 .UNSPECIFIED., .F., .F., .F.,
 ( 6, 6 ),
 ( 6, 6 ),
 ( 11.44766861079999920, 30.74049611620000277 ),
 ( 0.000000000000000000, 2.000000000000000000 ),
 .UNSPECIFIED. ) ;
#49118 = PLANE ( 'NONE',  #87397 ) ;
#49119 = CARTESIAN_POINT ( 'NONE',  ( -18.95489208017639982, 1384.531068566690010, 201.4205921255219778 ) ) ;
#49120 = CARTESIAN_POINT ( 'NONE',  ( -34.80158685906719995, 1420.241074056469870, 270.2980797153470007 ) ) ;
#49121 = CARTESIAN_POINT ( 'NONE',  ( 5.864566082395450408, 1522.051704408389924, 226.1537825710409777 ) ) ;
#49122 = CARTESIAN_POINT ( 'NONE',  ( -5.072028222450000179, 1397.441753602630115, 197.1461490164979864 ) ) ;
#49124 = ORIENTED_EDGE ( 'NONE', *, *, #104866, .F. ) ;
#49123 = DIRECTION ( 'NONE',  ( 0.4794255386042028388, 0.000000000000000000, 0.8775825618903727587 ) ) ;
#49125 = ORIENTED_EDGE ( 'NONE', *, *, #39902, .T. ) ;
#49126 = CARTESIAN_POINT ( 'NONE',  ( -8.881784196999999612E-15, 1446.564900598709983, 126.8032249175980155 ) ) ;
#49127 = FACE_OUTER_BOUND ( 'NONE', #41490, .T. ) ;
#49128 = CARTESIAN_POINT ( 'NONE',  ( 1.809416385432540242, 1425.955702030009888, 191.1749219456789888 ) ) ;
#49129 = CARTESIAN_POINT ( 'NONE',  ( -3.958634283238929630, 1508.551704408389924, 204.1347675023280033 ) ) ;
#49130 = CARTESIAN_POINT ( 'NONE',  ( -24.48327685399999609, 1441.929089702420015, 211.0380465236279690 ) ) ;
#49131 = AXIS2_PLACEMENT_3D ( 'NONE', #80212, #53944, #52820 ) ;
#49132 = CARTESIAN_POINT ( 'NONE',  ( -4.995726007844999650, 1516.651306816259876, 211.4173314712770093 ) ) ;
#49133 = CARTESIAN_POINT ( 'NONE',  ( -68.77190080519999071, 1379.747925807450201, 280.3125203366930123 ) ) ;
#49134 = CARTESIAN_POINT ( 'NONE',  ( -2.616546427032389932, 1484.260686020460071, 183.2626519981290016 ) ) ;
#49135 = CARTESIAN_POINT ( 'NONE',  ( 8.306907985085359769, 1439.017606053439977, 211.8916603637549940 ) ) ;
#49136 = FACE_OUTER_BOUND ( 'NONE', #92067, .T. ) ;
#49137 = CARTESIAN_POINT ( 'NONE',  ( -5.013274999515000552, 1517.068517094990057, 206.8347616620369820 ) ) ;
#49138 = EDGE_LOOP ( 'NONE', ( #58012, #108607, #108170, #11109 ) ) ;
#49139 = CARTESIAN_POINT ( 'NONE',  ( -38.81202644809479807, 1436.797832379780175, 134.4203394024459897 ) ) ;
#49140 = CARTESIAN_POINT ( 'NONE',  ( -11.00427874533239958, 1425.778358600110096, 91.15460183957679874 ) ) ;
#49141 = CIRCLE ( 'NONE', #70839, 0.4999999999999995559 ) ;
#49142 = CARTESIAN_POINT ( 'NONE',  ( -20.86737114567692331, 1455.046213227785756, 223.5104812541308092 ) ) ;
#49143 = ORIENTED_EDGE ( 'NONE', *, *, #37884, .F. ) ;
#49144 = DIRECTION ( 'NONE',  ( -6.123233995736769734E-17, -1.000000000000000000, -1.124819836996399911E-32 ) ) ;
#49145 = CARTESIAN_POINT ( 'NONE',  ( -25.48530486458319899, 1509.803026911279630, 223.7268176318329722 ) ) ;
#49146 = CARTESIAN_POINT ( 'NONE',  ( 14.15450645269999974, 1415.628674276829770, 197.1631309957980136 ) ) ;
#49147 = CARTESIAN_POINT ( 'NONE',  ( -41.66135440509999910, 1443.796918820770088, 135.6885369501979994 ) ) ;
#49148 = CARTESIAN_POINT ( 'NONE',  ( 26.54193529589999656, 1451.986209443830148, 134.9390663417979965 ) ) ;
#49149 = CARTESIAN_POINT ( 'NONE',  ( 10.83224975562239933, 1490.714117854160122, 210.9222104128400019 ) ) ;
#49150 = CARTESIAN_POINT ( 'NONE',  ( 9.061725897470001456, 1489.261074100890028, 201.5581573919090204 ) ) ;
#49151 = CARTESIAN_POINT ( 'NONE',  ( 0.09512346046118322351, 1506.606278688875818, 186.9942562802339125 ) ) ;
#49152 = CARTESIAN_POINT ( 'NONE',  ( 23.59327449265760990, 1448.793542086508069, 216.5857998349242450 ) ) ;
#49153 = CARTESIAN_POINT ( 'NONE',  ( -11.91388749740000108, 1435.945967586000052, 151.0354243678980026 ) ) ;
#49154 = CARTESIAN_POINT ( 'NONE',  ( 34.59585293901231751, 1451.704947487630079, 134.6974134653648605 ) ) ;
#49155 = CARTESIAN_POINT ( 'NONE',  ( 6.943602653455000606, 1516.858069504249897, 216.0629462479770098 ) ) ;
#49156 = VERTEX_POINT ( 'NONE', #14965 ) ;
#49157 = CARTESIAN_POINT ( 'NONE',  ( 7.714865528678569895, 1516.757088632780096, 208.5051077213929887 ) ) ;
#49158 = CARTESIAN_POINT ( 'NONE',  ( -3.349195415509999663, 1474.892783691989962, 198.1874921133990028 ) ) ;
#49159 = CARTESIAN_POINT ( 'NONE',  ( 0.4863418399100000178, 1418.702334915129995, 184.7127967600980014 ) ) ;
#49160 = EDGE_CURVE ( 'NONE', #86968, #642, #89525, .T. ) ;
#49161 = CARTESIAN_POINT ( 'NONE',  ( -13.82287742442830059, 1508.446990094839748, 216.5222845503169822 ) ) ;
#49162 = CARTESIAN_POINT ( 'NONE',  ( -2.127304298620000367, 1475.553256189390140, 219.6136142033990097 ) ) ;
#49163 = DIRECTION ( 'NONE',  ( 0.000000000000000000, -1.000000000000000000, 0.000000000000000000 ) ) ;
#49164 = CARTESIAN_POINT ( 'NONE',  ( 11.60004869885203682, 1426.458005118043047, 139.1709647423215301 ) ) ;
#49165 = CARTESIAN_POINT ( 'NONE',  ( -7.077403913657799528, 1508.382900477385647, 219.7413862116793268 ) ) ;
#49166 = DIRECTION ( 'NONE',  ( 0.000000000000000000, 1.000000000000000000, 0.000000000000000000 ) ) ;
#49167 = DIRECTION ( 'NONE',  ( -0.02616798426398481495, -0.9993150019883594304, -0.02616798426637241201 ) ) ;
#49168 = EDGE_CURVE ( 'NONE', #103079, #68646, #82184, .T. ) ;
#49169 = CARTESIAN_POINT ( 'NONE',  ( -4.946301771011410109E-07, 1406.984793698239855, 222.1228995466940148 ) ) ;
#49170 = CARTESIAN_POINT ( 'NONE',  ( 29.22677911810859896, 1440.913060387069891, 235.7684569196479742 ) ) ;
#49172 = CARTESIAN_POINT ( 'NONE',  ( 4.327871496238250515, 1515.125026768150065, 208.3313100357229928 ) ) ;
#49171 = CARTESIAN_POINT ( 'NONE',  ( -9.842598580781601214, 1471.074680866249992, 212.0444714742759800 ) ) ;
#49173 = LINE ( 'NONE', #83305, #97564 ) ;
#49174 = ORIENTED_EDGE ( 'NONE', *, *, #27002, .T. ) ;
#49175 = CARTESIAN_POINT ( 'NONE',  ( -4.626591905484999323, 1517.096587378560116, 207.4170511287669854 ) ) ;
#49176 = ORIENTED_EDGE ( 'NONE', *, *, #13686, .F. ) ;
#49177 = CIRCLE ( 'NONE', #38363, 15.09021984820000029 ) ;
#49178 = CARTESIAN_POINT ( 'NONE',  ( 10.53150541081210001, 1481.128416490849986, 211.0448888799710119 ) ) ;
#49179 = CARTESIAN_POINT ( 'NONE',  ( -13.27700466185214090, 1506.366982258753751, 226.6204409654947085 ) ) ;
#49180 = CARTESIAN_POINT ( 'NONE',  ( -3.258755850400000043, 1441.659648558289973, 200.8802078077489739 ) ) ;
#49181 = CARTESIAN_POINT ( 'NONE',  ( 11.38148961198079867, 1502.618718762939807, 211.1685771008779966 ) ) ;
#49182 = CARTESIAN_POINT ( 'NONE',  ( -1829.302631503789826, 11216.44053380569858, -1188.015784187918598 ) ) ;
#49183 = AXIS2_PLACEMENT_3D ( 'NONE', #71784, #62837, #106439 ) ;
#49184 = CARTESIAN_POINT ( 'NONE',  ( 27.54247199862367523, 1509.986917861693200, 221.0135325175801029 ) ) ;
#49185 = CARTESIAN_POINT ( 'NONE',  ( -0.8041292380773119586, 1508.551704408389924, 220.0687458904899927 ) ) ;
#49186 = CARTESIAN_POINT ( 'NONE',  ( -52.84872043374259931, 1383.807289815149943, 267.1640630856880421 ) ) ;
#49188 = B_SPLINE_CURVE_WITH_KNOTS ( 'NONE', 5,
 ( #14338, #7057, #83214, #102208, #101093, #31698, #32260, #48527, #82667 ),
 .UNSPECIFIED., .F., .F.,
 ( 6, 3, 6 ),
 ( 0.000000000000000000, 0.5050532947641763748, 1.000000000000000000 ),
 .UNSPECIFIED. ) ;
#49187 = CARTESIAN_POINT ( 'NONE',  ( -5.160317838924999734, 1510.729589429620091, 201.5648160248170200 ) ) ;
#49189 = FACE_OUTER_BOUND ( 'NONE', #14586, .T. ) ;
#49190 = CARTESIAN_POINT ( 'NONE',  ( -11.89599453256210104, 1434.596263801839996, 147.6475367371979814 ) ) ;
#49191 = CARTESIAN_POINT ( 'NONE',  ( 10.69502106051730017, 1492.057597410500193, 212.3896476547330110 ) ) ;
#49193 = ORIENTED_EDGE ( 'NONE', *, *, #49655, .F. ) ;
#49192 = CARTESIAN_POINT ( 'NONE',  ( 33.23571934791666393, 1511.187213306747708, 198.7594255952494677 ) ) ;
#49194 = CARTESIAN_POINT ( 'NONE',  ( 34.18677586421137704, 1522.906561336852064, 219.7932833225227114 ) ) ;
#49195 = B_SPLINE_SURFACE_WITH_KNOTS ( 'NONE', 5, 1, ( 
 ( #14154, #82479 ),
 ( #30962, #84116 ),
 ( #92510, #66800 ),
 ( #65137, #108773 ),
 ( #39921, #57843 ),
 ( #49979, #6852 ),
 ( #99805, #40463 ),
 ( #15777, #24198 ),
 ( #100375, #99250 ) ),
 .UNSPECIFIED., .F., .F., .F.,
 ( 6, 3, 6 ),
 ( 2, 2 ),
 ( 0.000000000000000000, 3.461179286750000195, 6.897024932289999910 ),
 ( 0.000000000000000000, 14.00000000000000000 ),
 .UNSPECIFIED. ) ;
#49196 = CARTESIAN_POINT ( 'NONE',  ( -68.61981551019999870, 1383.223412842329935, 263.4739815647590149 ) ) ;
#49197 = CARTESIAN_POINT ( 'NONE',  ( -20.92480426329999688, 1409.643770653630099, 213.2359878676279834 ) ) ;
#49198 = ORIENTED_EDGE ( 'NONE', *, *, #98132, .T. ) ;
#49199 = VERTEX_POINT ( 'NONE', #92789 ) ;
#49200 = CARTESIAN_POINT ( 'NONE',  ( -8.105405351571780770, 1386.750627257020142, 218.6043960686319849 ) ) ;
#49201 = DIRECTION ( 'NONE',  ( -0.6742693640212151784, 0.000000000000000000, -0.7384854939282328168 ) ) ;
#49203 = CARTESIAN_POINT ( 'NONE',  ( 3.584503077415259753, 1486.500511906220027, 219.3043361390229791 ) ) ;
#49202 = CARTESIAN_POINT ( 'NONE',  ( -11.57168670579999947, 1440.669964955550086, 147.8294280051980252 ) ) ;
#49204 = CARTESIAN_POINT ( 'NONE',  ( -9.806574738260000146, 1463.377913006889912, 203.8363535297289957 ) ) ;
#49205 = CARTESIAN_POINT ( 'NONE',  ( -105.0671882769999996, 1380.670236109440111, 300.1379999032590149 ) ) ;
#49206 = CARTESIAN_POINT ( 'NONE',  ( -20.27427188162093330, 1519.551704408389924, 208.7383139970561672 ) ) ;
#49207 = DIRECTION ( 'NONE',  ( 0.3255681544571546460, 0.000000000000000000, 0.9455185755993176233 ) ) ;
#49208 = CARTESIAN_POINT ( 'NONE',  ( 11.70547067012559950, 1409.321824430400056, 199.8234607599930257 ) ) ;
#49209 = CARTESIAN_POINT ( 'NONE',  ( 0.3331978421699999804, 1408.924695912329980, 186.0526675979979814 ) ) ;
#49210 = DIRECTION ( 'NONE',  ( 0.000000000000000000, -1.000000000000000000, 0.000000000000000000 ) ) ;
#49211 = CARTESIAN_POINT ( 'NONE',  ( -1.956232596697950132, 1468.321003611494234, 219.3647435431511781 ) ) ;
#49212 = CARTESIAN_POINT ( 'NONE',  ( -3.126071747161609515, 1441.074179428409934, 162.1943810228259792 ) ) ;
#49213 = B_SPLINE_CURVE_WITH_KNOTS ( 'NONE', 5,
 ( #91304, #55519, #89647, #71804, #90186, #12933, #81240, #22411, #14587 ),
 .UNSPECIFIED., .F., .F.,
 ( 6, 3, 6 ),
 ( 0.000000000000000000, 0.4424181324985710373, 1.000000000000000000 ),
 .UNSPECIFIED. ) ;
#49214 = CARTESIAN_POINT ( 'NONE',  ( -2.499996273572980154, 1448.894362898710142, 183.1109776662320030 ) ) ;
#49215 = ORIENTED_EDGE ( 'NONE', *, *, #85776, .T. ) ;
#49216 = AXIS2_PLACEMENT_3D ( 'NONE', #50231, #48014, #75434 ) ;
#49217 = CARTESIAN_POINT ( 'NONE',  ( -2.439001525050000119, 1430.488531030629929, 150.2249694046979869 ) ) ;
#49218 = CARTESIAN_POINT ( 'NONE',  ( 18.39664307513569952, 1458.152682626249771, 227.7204897826050001 ) ) ;
#49219 = CARTESIAN_POINT ( 'NONE',  ( -13.01562633140000003, 1434.791942642399817, 149.6201245377980058 ) ) ;
#49220 = CARTESIAN_POINT ( 'NONE',  ( 12.88439093021430004, 1420.965050148459795, 203.2552933692489887 ) ) ;
#49221 = CARTESIAN_POINT ( 'NONE',  ( -1.550651194838236657, 1515.551704408390606, 213.0145024707716175 ) ) ;
#49222 = CARTESIAN_POINT ( 'NONE',  ( -15.57808732350000014, 1420.358151750999923, 210.5578191881789678 ) ) ;
#49223 = CARTESIAN_POINT ( 'NONE',  ( -109.2341786859999928, 1385.225129184130083, 311.2612912872589845 ) ) ;
#49224 = AXIS2_PLACEMENT_3D ( 'NONE', #55031, #1877, #18620 ) ;
#49225 = CARTESIAN_POINT ( 'NONE',  ( 0.1762042766570000030, 1476.674948662830047, 182.2372324101980041 ) ) ;
#49226 = CARTESIAN_POINT ( 'NONE',  ( -11.43307569840619387, 1362.816133835241999, 209.6218459617033432 ) ) ;
#49227 = CARTESIAN_POINT ( 'NONE',  ( -5.316196955749759923, 1517.151704408390060, 231.0177287530028423 ) ) ;
#49228 = CARTESIAN_POINT ( 'NONE',  ( 13.80301174034419986, 1509.225260488219874, 234.1284213510270149 ) ) ;
#49229 = CARTESIAN_POINT ( 'NONE',  ( -1.637338503800000122, 1444.255706267190135, 199.2007328904890073 ) ) ;
#49230 = CARTESIAN_POINT ( 'NONE',  ( -5.786847777804999815, 1517.104497701820037, 208.3841784293060186 ) ) ;
#49231 = B_SPLINE_CURVE_WITH_KNOTS ( 'NONE', 3,
 ( #108843, #14778, #83095, #56244, #31027, #83635, #5846, #65756, #75265, #48408, #99873, #100443, #23726, #15317, #41088, #109955, #48964, #6931, #40536, #74712, #39986, #66325 ),
 .UNSPECIFIED., .F., .F.,
 ( 4, 2, 2, 2, 2, 2, 2, 2, 2, 2, 4 ),
 ( 0.000000000000000000, 0.2500000000000318634, 0.3750000000000477951, 0.4375000000000460187, 0.5000000000000442979, 0.6250000000000214273, 0.6875000000000214273, 0.7500000000000214273, 0.8125000000000214273, 0.8750000000000213163, 1.000000000000000000 ),
 .UNSPECIFIED. ) ;
#49232 = CARTESIAN_POINT ( 'NONE',  ( -3.827327205999999649, 1432.413060387330006, 146.1721969590979882 ) ) ;
#49233 = CARTESIAN_POINT ( 'NONE',  ( -4.026786250540000722, 1421.741487512030062, 169.4417495807979890 ) ) ;
#49234 = B_SPLINE_SURFACE_WITH_KNOTS ( 'NONE', 5, 5, ( 
 ( #28016, #62771, #96886, #104727, #62204, #63850 ),
 ( #44849, #72250, #29122, #106378, #29665, #3394 ),
 ( #10115, #53245, #105843, #86824, #19609, #52688 ),
 ( #37524, #97427, #53811, #87386, #70065, #11238 ),
 ( #28573, #105280, #20696, #45400, #79539, #54892 ),
 ( #44287, #104177, #27461, #61649, #95776, #19043 ),
 ( #10681, #38613, #82821, #73335, #64398, #55444 ),
 ( #40822, #21232, #100181, #91770, #14507, #89571 ),
 ( #90112, #22892, #22339, #5577, #39160, #4482 ),
 ( #72791, #47582, #57658, #30767, #99608, #82279 ),
 ( #81707, #57102, #39727, #73893, #97962, #21787 ),
 ( #12862, #108019, #30207, #47043, #31868, #81167 ) ),
 .UNSPECIFIED., .F., .F., .F.,
 ( 6, 3, 3, 6 ),
 ( 6, 6 ),
 ( 13.40444266900000159, 16.17473073229999869, 20.23252678009999883, 23.15004421629999953 ),
 ( 0.000000000000000000, 1.553560449149999911 ),
 .UNSPECIFIED. ) ;
#49235 = CARTESIAN_POINT ( 'NONE',  ( -14.45214300844910227, 1379.635521336690090, 208.1492130568690015 ) ) ;
#49236 = CARTESIAN_POINT ( 'NONE',  ( 7.201669765347830321, 1424.954475730090053, 212.8464732492809901 ) ) ;
#49237 = ORIENTED_EDGE ( 'NONE', *, *, #29171, .F. ) ;
#49238 = CARTESIAN_POINT ( 'NONE',  ( 30.28727320009999957, 1436.978278694869914, 240.1330978273979895 ) ) ;
#49240 = CARTESIAN_POINT ( 'NONE',  ( -16.69108649869999894, 1409.495925968330084, 194.8380977668979881 ) ) ;
#49239 = CARTESIAN_POINT ( 'NONE',  ( -0.4818462150879999628, 1464.109908317130021, 182.6611701878979943 ) ) ;
#49241 = DIRECTION ( 'NONE',  ( -1.755985294532469921E-16, 1.000000000000000000, -1.338183447452831989E-16 ) ) ;
#49242 = B_SPLINE_CURVE_WITH_KNOTS ( 'NONE', 3,
 ( #40052, #65826, #108915, #30548 ),
 .UNSPECIFIED., .F., .F.,
 ( 4, 4 ),
 ( 0.000000000000000000, 1.000000000000000000 ),
 .UNSPECIFIED. ) ;
#49243 = CARTESIAN_POINT ( 'NONE',  ( -25.50660914920000266, 1437.541738164299886, 220.8252629115979744 ) ) ;
#49244 = CARTESIAN_POINT ( 'NONE',  ( -1.952464535469999873, 1487.388627956889877, 219.9077361037989817 ) ) ;
#49245 = CARTESIAN_POINT ( 'NONE',  ( -1.965429846505029943, 1452.844426064699974, 152.4682849505009870 ) ) ;
#49246 = CARTESIAN_POINT ( 'NONE',  ( -2.372478608332516892, 1522.382868172863937, 243.3440112565233449 ) ) ;
#49247 = ORIENTED_EDGE ( 'NONE', *, *, #65142, .F. ) ;
#49248 = CARTESIAN_POINT ( 'NONE',  ( -2.500000000000000000, 1419.454841297830171, 146.2312480424980095 ) ) ;
#49249 = CARTESIAN_POINT ( 'NONE',  ( 16.79131591733570161, 1422.584993768290133, 227.0552595885409914 ) ) ;
#49250 = CARTESIAN_POINT ( 'NONE',  ( 10.82976971369999930, 1461.788039422589918, 210.9060527513990166 ) ) ;
#49251 = EDGE_LOOP ( 'NONE', ( #80363, #73826 ) ) ;
#49252 = ORIENTED_EDGE ( 'NONE', *, *, #61018, .T. ) ;
#49253 = B_SPLINE_CURVE_WITH_KNOTS ( 'NONE', 3,
 ( #8340, #26811, #25687, #52031, #17272, #101281 ),
 .UNSPECIFIED., .F., .F.,
 ( 4, 2, 4 ),
 ( 0.000000000000000000, 0.5000000000000000000, 1.000000000000000000 ),
 .UNSPECIFIED. ) ;
#49254 = B_SPLINE_CURVE_WITH_KNOTS ( 'NONE', 3,
 ( #64087, #81390, #5257, #97120, #13082, #39411, #97664, #56218, #12559, #56773, #89263, #46189, #90348, #4703, #22568, #65182, #105527, #45643, #80322, #38846, #106069, #38299, #90911, #47267, #37216, #31003, #98760, #46739, #29349 ),
 .UNSPECIFIED., .F., .F.,
 ( 4, 2, 2, 2, 2, 2, 2, 2, 2, 2, 2, 2, 2, 1, 4 ),
 ( 0.000000000000000000, 0.06995772642207957748, 0.1049365896331837661, 0.1224260212388009333, 0.1311707370415980956, 0.1399154528443952439, 0.2098731792674686514, 0.2448520424790045502, 0.2798309056905404768, 0.4197463585366428829, 0.4897040849595805656, 0.4984488007624685579, 0.5071935165653566058, 0.5246829481713172205, 0.5596618113830474917 ),
 .UNSPECIFIED. ) ;
#49255 = CARTESIAN_POINT ( 'NONE',  ( -79.49669931849999216, 1385.035068832460183, 282.9465538581589499 ) ) ;
#49256 = CARTESIAN_POINT ( 'NONE',  ( -22.91314480545359800, 1409.722892369710053, 209.2608525687020062 ) ) ;
#49257 = DIRECTION ( 'NONE',  ( 0.9455185755993178454, 0.000000000000000000, -0.3255681544571537578 ) ) ;
#49258 = FACE_OUTER_BOUND ( 'NONE', #47407, .T. ) ;
#49259 = CARTESIAN_POINT ( 'NONE',  ( 5.442563054701103908, 1446.864248024533254, 154.6441915987726645 ) ) ;
#49260 = CARTESIAN_POINT ( 'NONE',  ( -1.947314920589999998, 1498.352006593830083, 236.6548988695980142 ) ) ;
#49261 = CARTESIAN_POINT ( 'NONE',  ( -20.07053839829999831, 1410.870413675929967, 220.7218785659979972 ) ) ;
#49262 = CARTESIAN_POINT ( 'NONE',  ( 41.12904693102370146, 1456.837557776329959, 266.8381811544340394 ) ) ;
#49263 = CARTESIAN_POINT ( 'NONE',  ( -4.159841847218469724, 1508.728286212990042, 204.6953463774560191 ) ) ;
#49264 = CARTESIAN_POINT ( 'NONE',  ( 0.02416417718109999807, 1419.738504350029871, 184.3877211754980010 ) ) ;
#49265 = CARTESIAN_POINT ( 'NONE',  ( 6.935457925184999262, 1516.627618683580067, 205.6664679548470076 ) ) ;
#49266 = ORIENTED_EDGE ( 'NONE', *, *, #80850, .F. ) ;
#49267 = CARTESIAN_POINT ( 'NONE',  ( 10.51881725948639890, 1481.320945440649893, 214.4817285840509840 ) ) ;
#49268 = CARTESIAN_POINT ( 'NONE',  ( 15.21580400995989812, 1513.293387711960122, 194.9022240235440222 ) ) ;
#49269 = CARTESIAN_POINT ( 'NONE',  ( 1.852152499140000019, 1428.774755345290032, 214.2804808353390058 ) ) ;
#49270 = VERTEX_POINT ( 'NONE', #17705 ) ;
#49271 = CARTESIAN_POINT ( 'NONE',  ( 2.500000005880000042, 1448.917482167679964, 182.8661755616980145 ) ) ;
#49272 = CARTESIAN_POINT ( 'NONE',  ( 27.01376952885669880, 1451.969717919180084, 134.9180436286740132 ) ) ;
#49273 = CARTESIAN_POINT ( 'NONE',  ( -14.08695220650660218, 1513.170547668159998, 193.8693523408769863 ) ) ;
#49274 = CARTESIAN_POINT ( 'NONE',  ( 5.662343758720000508, 1504.894618425089902, 220.5557215505990314 ) ) ;
#49275 = CARTESIAN_POINT ( 'NONE',  ( 7.840123310800001022, 1421.694352030239997, 195.8842445130989915 ) ) ;
#49276 = CARTESIAN_POINT ( 'NONE',  ( 1.338019250827790163, 1431.361302059610125, 218.5179660117710227 ) ) ;
#49277 = CARTESIAN_POINT ( 'NONE',  ( -11.14995156302100021, 1492.106312947269998, 203.9618532963989992 ) ) ;
#49278 = CARTESIAN_POINT ( 'NONE',  ( -5.387808366170000696, 1496.648306349289896, 199.2595289264190228 ) ) ;
#49279 = CARTESIAN_POINT ( 'NONE',  ( 7.487843116287019818, 1409.174541630780141, 188.9631191401809929 ) ) ;
#49281 = CARTESIAN_POINT ( 'NONE',  ( -18.48751025675699111, 1424.257012546406941, 225.0485682924247328 ) ) ;
#49280 = CARTESIAN_POINT ( 'NONE',  ( 29.55269881708354163, 1525.821544997590308, 197.1295836072964391 ) ) ;
#49282 = CARTESIAN_POINT ( 'NONE',  ( 10.89583921004300038, 1423.141224889920068, 206.8676328055360045 ) ) ;
#49283 = CARTESIAN_POINT ( 'NONE',  ( -13.73096378239999993, 1379.766844552289967, 213.0184681208289987 ) ) ;
#49284 = CARTESIAN_POINT ( 'NONE',  ( 11.74015320060000001, 1428.979986575930070, 144.1938086916980239 ) ) ;
#49285 = VERTEX_POINT ( 'NONE', #83290 ) ;
#49286 = CARTESIAN_POINT ( 'NONE',  ( 20.74408967690000338, 1436.077466332870017, 224.8635562027979802 ) ) ;
#49287 = CARTESIAN_POINT ( 'NONE',  ( 3.118629927103340194, 1507.020745903789930, 237.9289446147130036 ) ) ;
#49288 = LINE ( 'NONE', #24043, #42774 ) ;
#49289 = AXIS2_PLACEMENT_3D ( 'NONE', #28044, #19638, #9040 ) ;
#49290 = CARTESIAN_POINT ( 'NONE',  ( -8.598235764689999172, 1385.896259083729774, 199.9307053391690090 ) ) ;
#49291 = CARTESIAN_POINT ( 'NONE',  ( 20.21728935790000037, 1475.862786327189951, 209.1218459616989946 ) ) ;
#49292 = CARTESIAN_POINT ( 'NONE',  ( 11.94906839412739963, 1421.563497253679998, 203.4275386238590215 ) ) ;
#49293 = CARTESIAN_POINT ( 'NONE',  ( -11.02848016370420048, 1462.482799370420025, 208.5648133604260011 ) ) ;
#49294 = CARTESIAN_POINT ( 'NONE',  ( -12.85916294179999930, 1469.933320803330162, 268.3665355202980436 ) ) ;
#49295 = CARTESIAN_POINT ( 'NONE',  ( -8.101358069183218547, 1477.152134414194506, 215.6221709765751484 ) ) ;
#49296 = CARTESIAN_POINT ( 'NONE',  ( 11.36329992970000013, 1433.927233001689956, 151.4629445730980137 ) ) ;
#49297 = EDGE_CURVE ( 'NONE', #80453, #18655, #23004, .T. ) ;
#49298 = CARTESIAN_POINT ( 'NONE',  ( 5.052203704720000133, 1465.000168608229842, 255.3819207742980097 ) ) ;
#49299 = DIRECTION ( 'NONE',  ( 0.000000000000000000, 4.493040424372315268E-15, -1.000000000000000000 ) ) ;
#49300 = AXIS2_PLACEMENT_3D ( 'NONE', #23869, #58065, #30076 ) ;
#49301 = CARTESIAN_POINT ( 'NONE',  ( -16.85895935491750208, 1420.422674679470219, 203.4210585105750226 ) ) ;
#49302 = FACE_OUTER_BOUND ( 'NONE', #91137, .T. ) ;
#49303 = CARTESIAN_POINT ( 'NONE',  ( -14.77963593050276181, 1422.241748325693834, 229.4612819255225986 ) ) ;
#49304 = CARTESIAN_POINT ( 'NONE',  ( -17.74110947659999837, 1486.349883151629911, 188.0997659469979908 ) ) ;
#49305 = CARTESIAN_POINT ( 'NONE',  ( 9.939393902556568960, 1441.236512650339819, 153.4167242010410064 ) ) ;
#49306 = CARTESIAN_POINT ( 'NONE',  ( -16.66219966870000135, 1409.494917224029905, 225.0851005536980267 ) ) ;
#49307 = CARTESIAN_POINT ( 'NONE',  ( -1.546867746839999835, 1416.839692138929877, 228.0214409766979884 ) ) ;
#49308 = CARTESIAN_POINT ( 'NONE',  ( -2.175315985799999741, 1479.578773637490031, 229.4213946198989902 ) ) ;
#49309 = CARTESIAN_POINT ( 'NONE',  ( -12.26979726809049964, 1416.828039266780024, 194.6643405733680083 ) ) ;
#49310 = CARTESIAN_POINT ( 'NONE',  ( 12.78723769039999958, 1416.835809830829930, 222.7043020969979921 ) ) ;
#49311 = CARTESIAN_POINT ( 'NONE',  ( -5.027589337301257899, 1391.774060041337634, 203.8075142969989884 ) ) ;
#49312 = CARTESIAN_POINT ( 'NONE',  ( 0.5779273184081700210, 1519.551704408389924, 232.1634304495918002 ) ) ;
#49313 = CARTESIAN_POINT ( 'NONE',  ( 0.7910245917146940808, 1426.918876941764893, 134.0999999980980135 ) ) ;
#49314 = CARTESIAN_POINT ( 'NONE',  ( 0.2052161641460210073, 1460.044096025570070, 182.9511842453609916 ) ) ;
#49316 = ORIENTED_EDGE ( 'NONE', *, *, #74348, .T. ) ;
#49315 = CARTESIAN_POINT ( 'NONE',  ( 4.203127346707122847, 1464.947251126380934, 200.1638074967223986 ) ) ;
#49317 = CARTESIAN_POINT ( 'NONE',  ( -27.68130203340000151, 1444.740067931809790, 168.8183730152979933 ) ) ;
#49318 = CARTESIAN_POINT ( 'NONE',  ( -0.3078888690928980321, 1484.233364050224282, 198.4302670740845542 ) ) ;
#49319 = CARTESIAN_POINT ( 'NONE',  ( 11.87573510900000073, 1433.006578257460205, 147.2728728793979940 ) ) ;
#49320 = CARTESIAN_POINT ( 'NONE',  ( -41.63894744326280062, 1444.312235790899877, 134.0999999983169744 ) ) ;
#49321 = CARTESIAN_POINT ( 'NONE',  ( -109.7179933470000037, 1384.899991331759793, 297.0862032941589632 ) ) ;
#49322 = ORIENTED_EDGE ( 'NONE', *, *, #37123, .T. ) ;
#49323 = CARTESIAN_POINT ( 'NONE',  ( -16.49871591222072809, 1525.320827368861501, 181.2023419493034169 ) ) ;
#49324 = CARTESIAN_POINT ( 'NONE',  ( 0.000000000000000000, 1398.755125754900064, 209.1218459616989946 ) ) ;
#49325 = CARTESIAN_POINT ( 'NONE',  ( -105.2493395317690954, 1381.076302546985289, 308.6808743251384044 ) ) ;
#49326 = CARTESIAN_POINT ( 'NONE',  ( -3.451191875628180750, 1523.678648413191695, 243.0729557893954791 ) ) ;
#49327 = ADVANCED_FACE ( 'NONE', ( #34538 ), #106246, .F. ) ;
#49328 = CARTESIAN_POINT ( 'NONE',  ( -5.047164175452439672, 1434.247983095549898, 217.4094108637509919 ) ) ;
#49329 = CARTESIAN_POINT ( 'NONE',  ( 22.39898792957995965, 1411.068911948053938, 269.4880229147564705 ) ) ;
#49330 = CARTESIAN_POINT ( 'NONE',  ( -17.62923792119999788, 1419.134474756159989, 207.1478831079190002 ) ) ;
#49331 = CARTESIAN_POINT ( 'NONE',  ( -12.48493277280000058, 1379.220736522750030, 210.8106142036189965 ) ) ;
#49332 = CARTESIAN_POINT ( 'NONE',  ( 2.663080543119999977, 1439.661674899039781, 183.7921143496980108 ) ) ;
#49333 = CARTESIAN_POINT ( 'NONE',  ( -59.64316829561520450, 1385.059617650149903, 243.2224340318209670 ) ) ;
#49334 = CARTESIAN_POINT ( 'NONE',  ( -18.40343465886406094, 1525.402221411349501, 238.3904617729373001 ) ) ;
#49335 = CARTESIAN_POINT ( 'NONE',  ( 10.72891033486649981, 1425.799916289779958, 207.0245073530009847 ) ) ;
#49336 = CARTESIAN_POINT ( 'NONE',  ( -30.95328531120000193, 1451.376546782129935, 136.0329327139980080 ) ) ;
#49337 = CARTESIAN_POINT ( 'NONE',  ( -16.32630028360690133, 1410.439485329699892, 226.5641403730199954 ) ) ;
#49338 = AXIS2_PLACEMENT_3D ( 'NONE', #55199, #104469, #2594 ) ;
#49340 = ORIENTED_EDGE ( 'NONE', *, *, #6879, .F. ) ;
#49339 = DIRECTION ( 'NONE',  ( -0.6736849260863841948, 0.000000000000000000, 0.7390186874254148774 ) ) ;
#49341 = CARTESIAN_POINT ( 'NONE',  ( 5.102416067990000137, 1474.008965365689846, 219.3522235086990122 ) ) ;
#49343 = CARTESIAN_POINT ( 'NONE',  ( 10.00447882353569895, 1469.985636142700059, 210.3446379253909981 ) ) ;
#49342 = AXIS2_PLACEMENT_3D ( 'NONE', #95485, #18752, #52949 ) ;
#49344 = CARTESIAN_POINT ( 'NONE',  ( -21.19290736559898747, 1411.012288320353946, 217.7512743417428283 ) ) ;
#49345 = CARTESIAN_POINT ( 'NONE',  ( -109.8262402379999969, 1384.894770817870040, 311.3808756572590255 ) ) ;
#49346 = CARTESIAN_POINT ( 'NONE',  ( -0.3495969842318680243, 1418.819586111129865, 184.6927620590689969 ) ) ;
#49347 = CARTESIAN_POINT ( 'NONE',  ( 17.57263694539999932, 1409.691668943730065, 222.6387570695980003 ) ) ;
#49348 = CARTESIAN_POINT ( 'NONE',  ( -18.86027053263874009, 1512.187213306747481, 230.7762769316009042 ) ) ;
#49349 = CARTESIAN_POINT ( 'NONE',  ( -16.92248609410000171, 1422.998996083129896, 227.1571761638979865 ) ) ;
#49350 = CARTESIAN_POINT ( 'NONE',  ( 2.475018581880529922, 1497.111080376900190, 196.9667223532030107 ) ) ;
#49351 = CARTESIAN_POINT ( 'NONE',  ( 5.024380392590000355, 1446.652863129090065, 201.3514328607089965 ) ) ;
#49352 = CARTESIAN_POINT ( 'NONE',  ( -104.0812585028399866, 1311.832804576489934, 306.6013113658122506 ) ) ;
#49353 = CARTESIAN_POINT ( 'NONE',  ( -2.824235741780000364, 1454.999275414490057, 199.7442147925889913 ) ) ;
#49354 = CARTESIAN_POINT ( 'NONE',  ( -5.786837717054999608, 1517.040132827679827, 205.8646253294070050 ) ) ;
#49355 = CARTESIAN_POINT ( 'NONE',  ( -8.345708061868009509, 1484.725363963600103, 184.3707301608639852 ) ) ;
#49356 = VERTEX_POINT ( 'NONE', #76541 ) ;
#49357 = CARTESIAN_POINT ( 'NONE',  ( -109.1287995176789991, 1384.695877130179952, 311.2584553912229808 ) ) ;
#49358 = CARTESIAN_POINT ( 'NONE',  ( -4.245709548939140099, 1441.390156672689955, 161.8216553765309982 ) ) ;
#49360 = ORIENTED_EDGE ( 'NONE', *, *, #88472, .F. ) ;
#49359 = CARTESIAN_POINT ( 'NONE',  ( -68.59216743310000197, 1379.747776907659954, 280.1820150773590399 ) ) ;
#49361 = CARTESIAN_POINT ( 'NONE',  ( -8.820749743162084044, 1381.135727412223105, 217.8385779988905142 ) ) ;
#49362 = EDGE_LOOP ( 'NONE', ( #55822, #74235, #20893, #10841, #21008 ) ) ;
#49363 = CARTESIAN_POINT ( 'NONE',  ( -16.23489791427282114, 1514.585431660245149, 223.9400827068218689 ) ) ;
#49364 = EDGE_CURVE ( 'NONE', #32914, #108746, #9412, .T. ) ;
#49365 = DIRECTION ( 'NONE',  ( 0.9786619618251634067, 0.000000000000000000, -0.2054769195713292418 ) ) ;
#49367 = CARTESIAN_POINT ( 'NONE',  ( 16.17926374062649941, 1410.436583420409988, 191.6392560135060137 ) ) ;
#49366 = CARTESIAN_POINT ( 'NONE',  ( -11.15476667854829884, 1425.160639125820126, 144.1599692811499835 ) ) ;
#49368 = EDGE_CURVE ( 'NONE', #99066, #52145, #69578, .T. ) ;
#49369 = CARTESIAN_POINT ( 'NONE',  ( 1.135898785685000023, 1516.958737650239982, 210.2414381519470226 ) ) ;
#49370 = CARTESIAN_POINT ( 'NONE',  ( 40.28310057935370025, 1441.046327069720064, 136.8133136135640200 ) ) ;
#49371 = EDGE_CURVE ( 'NONE', #10428, #65683, #13346, .T. ) ;
#49372 = CARTESIAN_POINT ( 'NONE',  ( -106.3019370990619876, 1378.913060387450059, 306.0560277516660221 ) ) ;
#49373 = CARTESIAN_POINT ( 'NONE',  ( 5.898235284490000119, 1476.924971998690125, 199.0552711020989705 ) ) ;
#49374 = ADVANCED_FACE ( 'NONE', ( #59761 ), #28909, .F. ) ;
#49375 = CARTESIAN_POINT ( 'NONE',  ( 12.70216927250840122, 1500.518191181640077, 209.0698827285919776 ) ) ;
#49376 = PRODUCT_CONTEXT ( 'NONE', #43481, 'mechanical' ) ;
#49377 = EDGE_CURVE ( 'NONE', #31391, #105138, #68138, .T. ) ;
#49378 = CARTESIAN_POINT ( 'NONE',  ( 39.03583412974440137, 1449.647124672710106, 134.0999999981079895 ) ) ;
#49379 = CYLINDRICAL_SURFACE ( 'NONE', #68607, 1.999999999999912514 ) ;
#49380 = CARTESIAN_POINT ( 'NONE',  ( -19.73707911742420151, 1467.795398142200156, 204.3773320539029896 ) ) ;
#49381 = DIRECTION ( 'NONE',  ( 0.000000000000000000, 1.000000000000000000, 0.000000000000000000 ) ) ;
#49382 = EDGE_LOOP ( 'NONE', ( #89541, #57370, #92576, #30807, #42404 ) ) ;
#49383 = VERTEX_POINT ( 'NONE', #10444 ) ;
#49384 = EDGE_CURVE ( 'NONE', #108726, #74706, #87726, .T. ) ;
#49385 = CARTESIAN_POINT ( 'NONE',  ( 11.60004869885203682, 1425.894332500278097, 137.5113157688821275 ) ) ;
#49386 = CARTESIAN_POINT ( 'NONE',  ( -17.60627563539920004, 1410.895669414250051, 194.0661810348550205 ) ) ;
#49387 = CARTESIAN_POINT ( 'NONE',  ( 12.34885615716000018, 1499.864449722190102, 206.2962984148029761 ) ) ;
#49388 = FACE_OUTER_BOUND ( 'NONE', #86522, .T. ) ;
#49389 = CARTESIAN_POINT ( 'NONE',  ( -2.500000000000309974, 1439.152017482790143, 158.1892368472379928 ) ) ;
#49390 = CARTESIAN_POINT ( 'NONE',  ( 33.36586802512179162, 1518.913060387330006, 216.3367586934468818 ) ) ;
#49391 = CARTESIAN_POINT ( 'NONE',  ( -3.487587049029018171, 1508.884207228266860, 204.6305528343158642 ) ) ;
#49392 = CARTESIAN_POINT ( 'NONE',  ( 38.81202640299100182, 1450.612734557460044, 135.6938359136109966 ) ) ;
#49393 = CARTESIAN_POINT ( 'NONE',  ( 2.591728129302680372, 1421.338677576370173, 183.3108762431510002 ) ) ;
#49394 = CARTESIAN_POINT ( 'NONE',  ( 25.38578281050000029, 1437.608079703630210, 137.6409390164979811 ) ) ;
#49395 = SHAPE_REPRESENTATION ( 'Grinder Body', ( #21632 ), #91264 ) ;
#49396 = CARTESIAN_POINT ( 'NONE',  ( -11.24942739399999958, 1391.648629103060102, 213.8067856546890084 ) ) ;
#49397 = EDGE_CURVE ( 'NONE', #95189, #31615, #28383, .T. ) ;
#49398 = CARTESIAN_POINT ( 'NONE',  ( -80.38025116429729167, 1384.796184643460037, 283.6024437732969545 ) ) ;
#49399 = ORIENTED_EDGE ( 'NONE', *, *, #56340, .T. ) ;
#49400 = CARTESIAN_POINT ( 'NONE',  ( 5.003848121975000396, 1517.005755693489846, 201.7875176594370146 ) ) ;
#49401 = CARTESIAN_POINT ( 'NONE',  ( -7.339107240745000205, 1517.203017563489766, 207.9963360818169917 ) ) ;
#49402 = VERTEX_POINT ( 'NONE', #87155 ) ;
#49403 = CARTESIAN_POINT ( 'NONE',  ( 32.02808312589916540, 1522.382868172863937, 198.2787714533495489 ) ) ;
#49404 = B_SPLINE_CURVE_WITH_KNOTS ( 'NONE', 5,
 ( #9410, #9958, #86117, #67683, #50865, #59828, #7747, #60945, #33481 ),
 .UNSPECIFIED., .F., .F.,
 ( 6, 3, 6 ),
 ( 0.000000000000000000, 0.6063230996941525452, 1.000000000000000000 ),
 .UNSPECIFIED. ) ;
#49405 = CARTESIAN_POINT ( 'NONE',  ( -0.0008045307254439123222, 1451.918653371962137, 154.0008071823928333 ) ) ;
#49406 = ORIENTED_EDGE ( 'NONE', *, *, #78222, .F. ) ;
#49407 = CARTESIAN_POINT ( 'NONE',  ( -13.61423569610000150, 1415.579607672129896, 221.4543120760979775 ) ) ;
#49408 = FACE_OUTER_BOUND ( 'NONE', #69375, .T. ) ;
#49409 = CARTESIAN_POINT ( 'NONE',  ( -9.956645445956299412, 1519.551704408389924, 185.5808665542169820 ) ) ;
#49410 = ADVANCED_FACE ( 'NONE', ( #70388 ), #96379, .F. ) ;
#49411 = CARTESIAN_POINT ( 'NONE',  ( -9.524909850325949279, 1462.104426478840196, 206.5005804455079783 ) ) ;
#49412 = CARTESIAN_POINT ( 'NONE',  ( 21.41707235578040169, 1409.688061885250136, 206.3726929586279653 ) ) ;
#49413 = CARTESIAN_POINT ( 'NONE',  ( -32.02808312589930040, 1511.187213306747708, 198.2787714533499752 ) ) ;
#49414 = CARTESIAN_POINT ( 'NONE',  ( 0.01756135629899999856, 1508.846989029630095, 179.8793381870979999 ) ) ;
#49415 = EDGE_CURVE ( 'NONE', #20993, #108510, #49895, .T. ) ;
#49416 = CARTESIAN_POINT ( 'NONE',  ( -5.980914397353036094, 1510.675349062206351, 201.6120256252374645 ) ) ;
#49417 = DIRECTION ( 'NONE',  ( -0.4770263929449307105, 0.7067418228238977473, -0.5224574779879248565 ) ) ;
#49419 = CARTESIAN_POINT ( 'NONE',  ( 28.84709936330000346, 1507.919204206129962, 206.0039977793879871 ) ) ;
#49418 = CARTESIAN_POINT ( 'NONE',  ( 15.74698736379999708, 1461.435657786630145, 229.5665177702979918 ) ) ;
#49420 = CARTESIAN_POINT ( 'NONE',  ( 20.12874795999999833, 1473.837606016890049, 209.1218459616989946 ) ) ;
#49421 = FACE_OUTER_BOUND ( 'NONE', #109698, .T. ) ;
#49422 = EDGE_LOOP ( 'NONE', ( #76735, #42353, #43014, #32908 ) ) ;
#49423 = ADVANCED_FACE ( 'NONE', ( #36753 ), #52468, .F. ) ;
#49424 = DIRECTION ( 'NONE',  ( 0.000000000000000000, -1.000000000000000000, 0.000000000000000000 ) ) ;
#49425 = CARTESIAN_POINT ( 'NONE',  ( -29.75208676459999779, 1462.665512622030064, 268.3665355202980436 ) ) ;
#49426 = B_SPLINE_CURVE_WITH_KNOTS ( 'NONE', 3,
 ( #19821, #87033, #88706, #54028 ),
 .UNSPECIFIED., .F., .F.,
 ( 4, 4 ),
 ( 0.000000000000000000, 0.0002220129587134773411 ),
 .UNSPECIFIED. ) ;
#49427 = DIRECTION ( 'NONE',  ( -0.9996573249755569268, -0.02617694830788839730, 1.602875797835060096E-18 ) ) ;
#49428 = FACE_OUTER_BOUND ( 'NONE', #35866, .T. ) ;
#49429 = CARTESIAN_POINT ( 'NONE',  ( 4.623787969365000805, 1516.947419719950176, 212.5709951659769956 ) ) ;
#49430 = CARTESIAN_POINT ( 'NONE',  ( 18.46438756899999944, 1509.557851009430124, 186.5303332271980139 ) ) ;
#49431 = CARTESIAN_POINT ( 'NONE',  ( -11.60004869885203682, 1426.340588536289033, 138.4439388390336205 ) ) ;
#49433 = VERTEX_POINT ( 'NONE', #18825 ) ;
#49432 = CARTESIAN_POINT ( 'NONE',  ( 4.426491198842340324, 1508.728286123109910, 213.2817096034670215 ) ) ;
#49434 = CARTESIAN_POINT ( 'NONE',  ( -1.439851189675433574, 1526.382868172864164, 178.7402778767507243 ) ) ;
#49435 = CARTESIAN_POINT ( 'NONE',  ( 2.910278962130000480, 1507.875172689290139, 220.4768199434989810 ) ) ;
#49436 = CARTESIAN_POINT ( 'NONE',  ( -11.85381821950000081, 1431.481266617950041, 149.9176055244979864 ) ) ;
#49437 = CARTESIAN_POINT ( 'NONE',  ( 19.03103510197079729, 1456.919749049050097, 225.5349545045000070 ) ) ;
#49438 = CARTESIAN_POINT ( 'NONE',  ( -109.8677307403279997, 1383.889131247379964, 311.3700200510110108 ) ) ;
#49439 = CARTESIAN_POINT ( 'NONE',  ( 11.73563908010000034, 1425.610159190430068, 144.1657657165980027 ) ) ;
#49440 = CARTESIAN_POINT ( 'NONE',  ( -5.068030367662819557, 1427.701625857500176, 201.2694279692279906 ) ) ;
#49441 = CARTESIAN_POINT ( 'NONE',  ( 12.70812379699999894, 1446.012777043369852, 188.2701611988979948 ) ) ;
#49443 = CARTESIAN_POINT ( 'NONE',  ( -5.360233013665446578, 1422.336972233150618, 139.1415641799490004 ) ) ;
#49442 = CARTESIAN_POINT ( 'NONE',  ( -19.87113920289999669, 1482.731852092930012, 227.4655975904979925 ) ) ;
#49444 = CARTESIAN_POINT ( 'NONE',  ( -6.569077907430000529, 1472.000453839789998, 211.3893757832889833 ) ) ;
#49445 = ORIENTED_EDGE ( 'NONE', *, *, #12608, .T. ) ;
#49446 = CARTESIAN_POINT ( 'NONE',  ( -6.561995998525000040, 1517.083030555940013, 205.8633713531569924 ) ) ;
#49447 = CARTESIAN_POINT ( 'NONE',  ( 3.729773516839999914, 1406.618697554530172, 269.4937607996980091 ) ) ;
#49448 = CARTESIAN_POINT ( 'NONE',  ( 0.1940371082550000070, 1409.861619517429972, 185.0322270696979956 ) ) ;
#49449 = DIRECTION ( 'NONE',  ( -0.06949073829049068340, 0.8615482456355327834, -0.5028972635978229411 ) ) ;
#49450 = ADVANCED_FACE ( 'NONE', ( #62547 ), #92792, .F. ) ;
#49451 = CIRCLE ( 'NONE', #10028, 1.999999999999999556 ) ;
#49452 = CARTESIAN_POINT ( 'NONE',  ( 24.51739935401977633, 1438.724131266478480, 212.6264403365555893 ) ) ;
#49453 = EDGE_CURVE ( 'NONE', #1304, #45857, #19939, .T. ) ;
#49454 = CARTESIAN_POINT ( 'NONE',  ( -8.890791467111871071, 1388.784675205049780, 217.7635828254234696 ) ) ;
#49455 = CARTESIAN_POINT ( 'NONE',  ( -10.93162295028230169, 1470.132889486390013, 212.2376398131100075 ) ) ;
#49456 = DIRECTION ( 'NONE',  ( 0.000000000000000000, -1.000000000000000000, 6.123233995736769734E-17 ) ) ;
#49457 = FACE_OUTER_BOUND ( 'NONE', #21134, .T. ) ;
#49458 = CARTESIAN_POINT ( 'NONE',  ( -12.61676759610000076, 1445.618655625439942, 187.3523340095979961 ) ) ;
#49459 = CARTESIAN_POINT ( 'NONE',  ( 0.8767898189759999461, 1450.882442212169963, 155.6080914335980196 ) ) ;
#49460 = CARTESIAN_POINT ( 'NONE',  ( -8.606197445582770555, 1437.745991313129934, 208.0916336407960046 ) ) ;
#49461 = CARTESIAN_POINT ( 'NONE',  ( -4.091781189539999808, 1515.531881637889910, 210.2416342621790193 ) ) ;
#49462 = CARTESIAN_POINT ( 'NONE',  ( -18.74729292449999818, 1442.199705176290081, 209.1218459616989946 ) ) ;
#49463 = B_SPLINE_CURVE_WITH_KNOTS ( 'NONE', 3,
 ( #3406, #18503, #12321, #2315, #52699, #10128, #1756, #19054, #87398, #10692, #79014, #62216, #96343, #72804, #55456, #74466, #49259, #12875 ),
 .UNSPECIFIED., .F., .F.,
 ( 4, 2, 2, 2, 2, 1, 1, 2, 2, 4 ),
 ( 0.000000000000000000, 0.1250000000000460743, 0.1875000000000671407, 0.2500000000000882072, 0.3750000000001271760, 0.4375000000001487699, 0.4687500000001563749, 0.4843750000001555422, 0.5000000000001546541, 1.000000000000000000 ),
 .UNSPECIFIED. ) ;
#49464 = EDGE_CURVE ( 'NONE', #65829, #33249, #44540, .T. ) ;
#49465 = CARTESIAN_POINT ( 'NONE',  ( 4.329791490734999471, 1515.051704408389924, 205.7917117663369879 ) ) ;
#49466 = CARTESIAN_POINT ( 'NONE',  ( 7.891238773745893553, 1521.951704408389787, 189.5145166091198803 ) ) ;
#49467 = CARTESIAN_POINT ( 'NONE',  ( -2.732294677939999694, 1474.989683629730052, 269.6477038462979863 ) ) ;
#49468 = CARTESIAN_POINT ( 'NONE',  ( -4.222017444537139674, 1446.225621437700056, 168.0528712459710050 ) ) ;
#49469 = CARTESIAN_POINT ( 'NONE',  ( -12.05354680877381490, 1513.055463255244376, 192.5148414102740446 ) ) ;
#49470 = CARTESIAN_POINT ( 'NONE',  ( -11.94336904982903746, 1486.509466811693073, 184.3567047474556944 ) ) ;
#49471 = CARTESIAN_POINT ( 'NONE',  ( -58.94955636626019668, 1384.699952765490025, 279.1418893135149801 ) ) ;
#49472 = CARTESIAN_POINT ( 'NONE',  ( -107.3094561203379982, 1391.913060387289988, 301.0960456400809448 ) ) ;
#49473 = CARTESIAN_POINT ( 'NONE',  ( -4.590060415194109567, 1517.051704403100075, 216.8444262830430205 ) ) ;
#49474 = CARTESIAN_POINT ( 'NONE',  ( -24.72115217916500285, 1457.432886049350145, 211.5135014677179868 ) ) ;
#49475 = CYLINDRICAL_SURFACE ( 'NONE', #14311, 33.13701971169416538 ) ;
#49476 = CARTESIAN_POINT ( 'NONE',  ( -46.27885827404714547, 1440.913026088479455, 267.5894365880741361 ) ) ;
#49477 = CARTESIAN_POINT ( 'NONE',  ( -0.2491233477655999673, 1395.921759966339778, 220.1232053259499821 ) ) ;
#49478 = CARTESIAN_POINT ( 'NONE',  ( -11.24213639542480436, 1378.800280137626714, 204.0324849010276580 ) ) ;
#49479 = CARTESIAN_POINT ( 'NONE',  ( 12.58642104890130042, 1421.533884203790194, 206.9918965626969793 ) ) ;
#49480 = EDGE_CURVE ( 'NONE', #14771, #42031, #98303, .T. ) ;
#49481 = FACE_OUTER_BOUND ( 'NONE', #20088, .T. ) ;
#49482 = ORIENTED_EDGE ( 'NONE', *, *, #109065, .F. ) ;
#49483 = CARTESIAN_POINT ( 'NONE',  ( -7.608841146861992755, 1410.551743274452065, 230.8008565250618744 ) ) ;
#49484 = B_SPLINE_CURVE_WITH_KNOTS ( 'NONE', 5,
 ( #31927, #65557, #24059, #100768, #72849, #40330 ),
 .UNSPECIFIED., .F., .F.,
 ( 6, 6 ),
 ( -2.000000000000000000, 0.000000000000000000 ),
 .UNSPECIFIED. ) ;
#49485 = CARTESIAN_POINT ( 'NONE',  ( -9.299413003310359471, 1446.922194731980198, 190.6945041834079859 ) ) ;
#49486 = DIRECTION ( 'NONE',  ( -0.6736849260863841948, 0.000000000000000000, 0.7390186874254148774 ) ) ;
#49487 = CARTESIAN_POINT ( 'NONE',  ( -20.43379628966849637, 1466.940213777560075, 211.2182826552119934 ) ) ;
#49489 = CARTESIAN_POINT ( 'NONE',  ( -12.39029767569030049, 1378.874140544039847, 211.3238570842829915 ) ) ;
#49488 = CARTESIAN_POINT ( 'NONE',  ( 11.43729884800000107, 1425.481263111430053, 144.1595926346979866 ) ) ;
#49490 = CARTESIAN_POINT ( 'NONE',  ( 16.58903855651479020, 1524.412928176729110, 237.5994789871142814 ) ) ;
#49491 = CARTESIAN_POINT ( 'NONE',  ( -15.92986207429999901, 1416.139014782290133, 209.7537124246929920 ) ) ;
#49492 = EDGE_CURVE ( 'NONE', #3178, #67457, #93473, .T. ) ;
#49493 = CARTESIAN_POINT ( 'NONE',  ( -4.523944061129999916, 1455.378620928990131, 200.8408218435490085 ) ) ;
#49494 = CARTESIAN_POINT ( 'NONE',  ( 3.259101798884999734, 1517.102359858469754, 202.1722709844570147 ) ) ;
#49495 = SPHERICAL_SURFACE ( 'NONE', #89318, 2.000000000000000000 ) ;
#49496 = CARTESIAN_POINT ( 'NONE',  ( -4.838067302830000749, 1426.802081400929865, 145.9750725641980011 ) ) ;
#49497 = CARTESIAN_POINT ( 'NONE',  ( 16.53923913363500020, 1512.406775501100128, 196.8368690890669939 ) ) ;
#49498 = CARTESIAN_POINT ( 'NONE',  ( -18.79896864135620049, 1419.283855142989978, 205.9425027332000013 ) ) ;
#49499 = CARTESIAN_POINT ( 'NONE',  ( -27.71065821358619985, 1379.782896911970056, 216.6336370555119970 ) ) ;
#49500 = CARTESIAN_POINT ( 'NONE',  ( 20.12920962994530427, 1508.860404140810033, 229.2672809891759869 ) ) ;
#49503 = ORIENTED_EDGE ( 'NONE', *, *, #48013, .T. ) ;
#49502 = CARTESIAN_POINT ( 'NONE',  ( -40.71370360497250118, 1379.670045600320009, 229.2404297411889900 ) ) ;
#49501 = VECTOR ( 'NONE', #18564, 1000.000000000000000 ) ;
#49504 = VERTEX_POINT ( 'NONE', #39512 ) ;
#49505 = CARTESIAN_POINT ( 'NONE',  ( 11.45674231629960005, 1434.121012763210047, 151.3920262788900004 ) ) ;
#49506 = CARTESIAN_POINT ( 'NONE',  ( -2.455548337050000196, 1396.059955855629823, 220.7626888616979954 ) ) ;
#49507 = CARTESIAN_POINT ( 'NONE',  ( -19.20692459609999858, 1410.079524434029736, 222.1170233296979859 ) ) ;
#49508 = VERTEX_POINT ( 'NONE', #63640 ) ;
#49509 = CARTESIAN_POINT ( 'NONE',  ( -13.32429459549980066, 1444.551508282647774, 169.3762542488305201 ) ) ;
#49510 = EDGE_CURVE ( 'NONE', #64407, #69273, #89619, .T. ) ;
#49511 = CARTESIAN_POINT ( 'NONE',  ( -27.04494217939999956, 1509.634156510529920, 201.2636846103279709 ) ) ;
#49512 = CARTESIAN_POINT ( 'NONE',  ( -7.585404424514999633, 1511.813148765560072, 211.5972449069469974 ) ) ;
#49514 = CARTESIAN_POINT ( 'NONE',  ( 17.91995256730000108, 1424.306612487629991, 226.0000067931979970 ) ) ;
#49513 = CARTESIAN_POINT ( 'NONE',  ( -0.1531850412299990138, 1444.288508142990167, 199.7853600647590042 ) ) ;
#49515 = CARTESIAN_POINT ( 'NONE',  ( 2.537021495169999863, 1468.705327849529795, 183.0181505298980085 ) ) ;
#49516 = EDGE_CURVE ( 'NONE', #22747, #17568, #24525, .T. ) ;
#49517 = CARTESIAN_POINT ( 'NONE',  ( -3.357869919927010116, 1463.835494135860017, 199.7544149164289990 ) ) ;
#49518 = FACE_OUTER_BOUND ( 'NONE', #75200, .T. ) ;
#49519 = SURFACE_SIDE_STYLE ('',( #57380 ) ) ;
#49520 = CARTESIAN_POINT ( 'NONE',  ( 10.27541959654410064, 1396.271885950119895, 205.0171044993250007 ) ) ;
#49521 = CARTESIAN_POINT ( 'NONE',  ( 2.500000000000000000, 1419.524771318244348, 137.0999999980979851 ) ) ;
#49522 = CARTESIAN_POINT ( 'NONE',  ( 11.76949914230000083, 1432.337435368489878, 150.8120642620980050 ) ) ;
#49523 = FACE_OUTER_BOUND ( 'NONE', #18857, .T. ) ;
#49524 = VERTEX_POINT ( 'NONE', #73685 ) ;
#49525 = CARTESIAN_POINT ( 'NONE',  ( 13.15339656435630111, 1434.869048593249772, 149.3633147529739915 ) ) ;
#49526 = EDGE_LOOP ( 'NONE', ( #99757, #55049, #55450, #107755 ) ) ;
#49527 = EDGE_LOOP ( 'NONE', ( #22767, #62981, #95794, #18984 ) ) ;
#49528 = EDGE_CURVE ( 'NONE', #46291, #83462, #44132, .T. ) ;
#49529 = CARTESIAN_POINT ( 'NONE',  ( -20.15504139832039954, 1507.862952778380077, 228.9029379167619993 ) ) ;
#49530 = CARTESIAN_POINT ( 'NONE',  ( -4.974760226879999969, 1466.059548552929982, 234.4497863035979890 ) ) ;
#49531 = CARTESIAN_POINT ( 'NONE',  ( -109.8668234651519242, 1385.921405704401877, 311.3699157048114898 ) ) ;
#49532 = CARTESIAN_POINT ( 'NONE',  ( 2.486474742745000022, 1516.560253536979872, 216.0557253731069807 ) ) ;
#49533 = CARTESIAN_POINT ( 'NONE',  ( -6.961461350099999557, 1472.923786193189926, 208.7096068999990166 ) ) ;
#49534 = ADVANCED_FACE ( 'NONE', ( #82619 ), #84963, .T. ) ;
#49535 = ORIENTED_EDGE ( 'NONE', *, *, #84859, .T. ) ;
#49536 = CARTESIAN_POINT ( 'NONE',  ( -11.37049282409999940, 1501.435198116990023, 207.7796432001189828 ) ) ;
#49537 = CARTESIAN_POINT ( 'NONE',  ( 2.500000000000000000, 1448.224507101739846, 166.8031351735940007 ) ) ;
#49538 = CARTESIAN_POINT ( 'NONE',  ( -7.611657828410000270, 1379.436956584469954, 206.9293838566389923 ) ) ;
#49539 = ORIENTED_EDGE ( 'NONE', *, *, #8655, .F. ) ;
#49540 = CARTESIAN_POINT ( 'NONE',  ( -1.715361130375000043, 1516.743010792419909, 205.6766444437269854 ) ) ;
#49541 = ORIENTED_EDGE ( 'NONE', *, *, #35575, .F. ) ;
#49542 = CARTESIAN_POINT ( 'NONE',  ( 6.562094069294999166, 1517.122674412569950, 209.8604508749069737 ) ) ;
#49543 = CARTESIAN_POINT ( 'NONE',  ( -9.173749095941850840, 1450.559996438570124, 208.1432995907519796 ) ) ;
#49544 = CARTESIAN_POINT ( 'NONE',  ( -35.43904686644575008, 1424.538195867626882, 269.5376332876632546 ) ) ;
#49545 = CARTESIAN_POINT ( 'NONE',  ( -1.331498055899999811, 1408.959557324029902, 231.4960598541979948 ) ) ;
#49547 = ORIENTED_EDGE ( 'NONE', *, *, #60651, .F. ) ;
#49546 = CARTESIAN_POINT ( 'NONE',  ( -0.08760820896872960339, 1414.971390223319986, 225.8230290847160120 ) ) ;
#49548 = CARTESIAN_POINT ( 'NONE',  ( 22.94282329279999999, 1432.044723198870088, 216.2486866827079837 ) ) ;
#49549 = CARTESIAN_POINT ( 'NONE',  ( -14.38287540707779932, 1508.551704408389924, 210.3535996512349868 ) ) ;
#49550 = CARTESIAN_POINT ( 'NONE',  ( -73.57334958110000400, 1384.359832552789840, 298.9349810372589786 ) ) ;
#49551 = CARTESIAN_POINT ( 'NONE',  ( -0.09294118512049590053, 1465.101552668469822, 237.0126441520749836 ) ) ;
#49552 = CARTESIAN_POINT ( 'NONE',  ( 7.954910151169818811, 1410.785611874080132, 269.6217138226900261 ) ) ;
#49553 = EDGE_CURVE ( 'NONE', #82793, #66538, #60197, .T. ) ;
#49554 = CARTESIAN_POINT ( 'NONE',  ( 4.621267883935000320, 1516.830644417779922, 214.1213023606370029 ) ) ;
#49555 = CARTESIAN_POINT ( 'NONE',  ( 22.91422305780000102, 1409.721956062029903, 209.2901359145519962 ) ) ;
#49556 = CARTESIAN_POINT ( 'NONE',  ( 28.62766089293252136, 1526.344110814219675, 198.0439708941995605 ) ) ;
#49557 = DIRECTION ( 'NONE',  ( 0.6709778558543655347, 0.000000000000000000, -0.7414773880254732497 ) ) ;
#49558 = CARTESIAN_POINT ( 'NONE',  ( -7.719818767491180900, 1516.946282269519997, 209.0807804088159969 ) ) ;
#49559 = CARTESIAN_POINT ( 'NONE',  ( 2.494757998004999866, 1516.937508036699910, 210.8228737931069929 ) ) ;
#49560 = CARTESIAN_POINT ( 'NONE',  ( 9.627346003815750564, 1434.811529568090009, 207.3365483151889919 ) ) ;
#49561 = CARTESIAN_POINT ( 'NONE',  ( 0.1282414636960000076, 1420.458860909030136, 183.3323408609980163 ) ) ;
#49562 = CARTESIAN_POINT ( 'NONE',  ( 4.331998614493840272, 1420.009893967346898, 137.0999999980978146 ) ) ;
#49564 = ORIENTED_EDGE ( 'NONE', *, *, #23393, .F. ) ;
#49563 = CARTESIAN_POINT ( 'NONE',  ( -61.45118310290000352, 1388.282453012750011, 249.7659151349589877 ) ) ;
#49565 = CARTESIAN_POINT ( 'NONE',  ( -45.48467309282600013, 1385.149558475349977, 252.4883491809910083 ) ) ;
#49566 = CARTESIAN_POINT ( 'NONE',  ( 30.31052258194586102, 1523.604703353109699, 195.7506062427368079 ) ) ;
#49567 = CARTESIAN_POINT ( 'NONE',  ( -3.467356662694556668, 1370.274142583225967, 208.1271013349179100 ) ) ;
#49568 = AXIS2_PLACEMENT_3D ( 'NONE', #40734, #80122, #75465 ) ;
#49569 = CARTESIAN_POINT ( 'NONE',  ( -1.565589935376011876, 1494.863348305362479, 220.1740265712254541 ) ) ;
#49570 = CARTESIAN_POINT ( 'NONE',  ( 6.284801111650899941, 1485.306667862180120, 217.9298748690059995 ) ) ;
#49571 = CARTESIAN_POINT ( 'NONE',  ( -22.83376452409999757, 1450.736906982369874, 218.4795132163679909 ) ) ;
#49572 = CARTESIAN_POINT ( 'NONE',  ( -18.19590854888185305, 1522.382868172863937, 180.0410247165186490 ) ) ;
#49574 = CYLINDRICAL_SURFACE ( 'NONE', #33618, 1.999999999999994449 ) ;
#49573 = DIRECTION ( 'NONE',  ( -0.000000000000000000, -1.000000000000000000, -0.000000000000000000 ) ) ;
#49575 = DIRECTION ( 'NONE',  ( 0.9455185755993178454, 0.000000000000000000, -0.3255681544571539243 ) ) ;
#49576 = CARTESIAN_POINT ( 'NONE',  ( 33.93019615848955084, 1522.382868172863937, 220.5829544587960811 ) ) ;
#49577 = ORIENTED_EDGE ( 'NONE', *, *, #45891, .T. ) ;
#49578 = CARTESIAN_POINT ( 'NONE',  ( -5.780861274184998955, 1516.783701990830195, 202.1826264492970324 ) ) ;
#49579 = CARTESIAN_POINT ( 'NONE',  ( 11.94203325640082269, 1433.494999503054714, 149.8940326207935243 ) ) ;
#49580 = CARTESIAN_POINT ( 'NONE',  ( -27.03405988100176671, 1451.512678451428883, 136.1495578053978477 ) ) ;
#49581 = CIRCLE ( 'NONE', #35248, 7.513435694540000043 ) ;
#49582 = CARTESIAN_POINT ( 'NONE',  ( 20.99698467690000214, 1453.431242447430122, 222.6481362127979935 ) ) ;
#49583 = CARTESIAN_POINT ( 'NONE',  ( 10.94239808399780145, 1461.353457147069776, 209.7851273180980058 ) ) ;
#49584 = DIRECTION ( 'NONE',  ( -1.305148739725796033E-31, 1.000000000000000000, -1.836970198721029688E-16 ) ) ;
#49585 = CARTESIAN_POINT ( 'NONE',  ( -1.329471185999999916, 1444.143595228889808, 218.0942866151389978 ) ) ;
#49586 = CARTESIAN_POINT ( 'NONE',  ( 10.91475598504960409, 1418.233546538132714, 229.8208136691085031 ) ) ;
#49587 = CARTESIAN_POINT ( 'NONE',  ( 28.37194653194559635, 1436.817231666380167, 136.7331909724399850 ) ) ;
#49588 = CARTESIAN_POINT ( 'NONE',  ( -18.18137283760000145, 1507.546748828630143, 231.7129783355979669 ) ) ;
#49589 = CARTESIAN_POINT ( 'NONE',  ( -20.85759521329999799, 1428.229804328530236, 220.8445560111979944 ) ) ;
#49590 = CARTESIAN_POINT ( 'NONE',  ( -30.96124148313727886, 1466.023121715494426, 269.3370833597967362 ) ) ;
#49591 = CARTESIAN_POINT ( 'NONE',  ( -105.0165902910000000, 1390.482592109759935, 303.1217258594589907 ) ) ;
#49592 = CARTESIAN_POINT ( 'NONE',  ( 15.36989447449999879, 1507.878420424329761, 186.8363077536980086 ) ) ;
#49593 = CARTESIAN_POINT ( 'NONE',  ( -20.88377839292641625, 1525.556090473914082, 184.5817676602346751 ) ) ;
#49594 = CARTESIAN_POINT ( 'NONE',  ( -34.97375764654307062, 1457.803496076289548, 269.5311906646001034 ) ) ;
#49595 = ORIENTED_EDGE ( 'NONE', *, *, #103402, .T. ) ;
#49596 = CARTESIAN_POINT ( 'NONE',  ( -8.744120078331269141, 1440.655636409200042, 205.1339896302730210 ) ) ;
#49597 = CARTESIAN_POINT ( 'NONE',  ( 9.082050437914793051, 1506.560172253591418, 188.9861834009692529 ) ) ;
#49598 = EDGE_CURVE ( 'NONE', #17762, #90799, #77018, .T. ) ;
#49599 = CARTESIAN_POINT ( 'NONE',  ( 22.86388141461030088, 1452.114636054890070, 134.1000000004160029 ) ) ;
#49600 = CARTESIAN_POINT ( 'NONE',  ( -7.612906430609999830, 1431.113060387329824, 226.5499313142980213 ) ) ;
#49601 = CARTESIAN_POINT ( 'NONE',  ( -15.50799805586373026, 1451.351354359962215, 222.5219775576906045 ) ) ;
#49602 = AXIS2_PLACEMENT_3D ( 'NONE', #83674, #84771, #25404 ) ;
#49603 = CARTESIAN_POINT ( 'NONE',  ( -29.78122807940000172, 1510.000412734329757, 209.3782614727080045 ) ) ;
#49604 = CARTESIAN_POINT ( 'NONE',  ( -9.126921779760198916, 1438.547899077590046, 209.4465929603159964 ) ) ;
#49605 = CARTESIAN_POINT ( 'NONE',  ( -4.136749821589599918, 1515.492902831140100, 212.0199450294899748 ) ) ;
#49606 = CARTESIAN_POINT ( 'NONE',  ( -2.133044466942135564, 1415.621662746755874, 232.9983725193774262 ) ) ;
#49607 = CARTESIAN_POINT ( 'NONE',  ( -9.280787195236113618, 1451.345929965323649, 152.5707864879639715 ) ) ;
#49608 = CARTESIAN_POINT ( 'NONE',  ( -9.519812938348620079, 1460.017558366200092, 210.6311618255110147 ) ) ;
#49609 = CARTESIAN_POINT ( 'NONE',  ( 3.780286388835000011, 1510.542924508009946, 216.6739878845270084 ) ) ;
#49611 = VERTEX_POINT ( 'NONE', #106443 ) ;
#49610 = CARTESIAN_POINT ( 'NONE',  ( 18.52154166987810058, 1425.594020092049732, 225.5394061038540201 ) ) ;
#49612 = EDGE_CURVE ( 'NONE', #104566, #99650, #100240, .T. ) ;
#49613 = CARTESIAN_POINT ( 'NONE',  ( 1.027470347560650143, 1414.913060387399810, 192.7325489235379905 ) ) ;
#49614 = CARTESIAN_POINT ( 'NONE',  ( 21.41430793513470121, 1509.039033305942212, 226.4051922569614419 ) ) ;
#49615 = EDGE_LOOP ( 'NONE', ( #99110, #48862, #13130, #78577 ) ) ;
#49616 = ORIENTED_EDGE ( 'NONE', *, *, #8534, .F. ) ;
#49617 = CARTESIAN_POINT ( 'NONE',  ( 17.84204394271100114, 1415.932840154009909, 208.7774965389979798 ) ) ;
#49618 = CARTESIAN_POINT ( 'NONE',  ( -20.70484064406360503, 1525.907212628473644, 233.2025904124107285 ) ) ;
#49620 = CARTESIAN_POINT ( 'NONE',  ( 1.813411856763470054, 1456.528622295709965, 219.5870533402340072 ) ) ;
#49619 = CARTESIAN_POINT ( 'NONE',  ( 2.857814868949999809, 1456.075906465790013, 218.9302595098089910 ) ) ;
#49621 = CARTESIAN_POINT ( 'NONE',  ( -2.363918620589999797, 1443.448698872290151, 218.8950620034389942 ) ) ;
#49622 = CARTESIAN_POINT ( 'NONE',  ( -11.04995494539999967, 1433.656863779019886, 151.7239346888979981 ) ) ;
#49623 = LINE ( 'NONE', #47958, #107186 ) ;
#49624 = CIRCLE ( 'NONE', #76461, 0.9999999999999865663 ) ;
#49625 = CARTESIAN_POINT ( 'NONE',  ( 9.699117481028789456, 1463.751773247410028, 210.5389327360290110 ) ) ;
#49626 = CARTESIAN_POINT ( 'NONE',  ( -2.580915939757335575, 1524.130440953581001, 242.3512492075526552 ) ) ;
#49627 = CARTESIAN_POINT ( 'NONE',  ( -24.36776551069999996, 1440.043862457850082, 211.3220141222980146 ) ) ;
#49628 = FACE_BOUND ( 'NONE', #74626, .T. ) ;
#49629 = CARTESIAN_POINT ( 'NONE',  ( 2.236830499208590339, 1495.676457082710158, 221.2569898128769807 ) ) ;
#49630 = CARTESIAN_POINT ( 'NONE',  ( 6.820918190075792253, 1362.920728698377161, 210.6218459617142003 ) ) ;
#49631 = CARTESIAN_POINT ( 'NONE',  ( -28.53389208509380026, 1510.020793257407377, 218.3937296574966638 ) ) ;
#49633 = ORIENTED_EDGE ( 'NONE', *, *, #77581, .T. ) ;
#49632 = CARTESIAN_POINT ( 'NONE',  ( -2.164019640618629963E-09, 1415.934403820770058, 241.0787384265379956 ) ) ;
#49634 = EDGE_LOOP ( 'NONE', ( #77319, #106944, #58315, #40022 ) ) ;
#49635 = CARTESIAN_POINT ( 'NONE',  ( -11.83710954711010110, 1430.357175028169877, 149.6181111097540111 ) ) ;
#49636 = CARTESIAN_POINT ( 'NONE',  ( 0.1433731509459970077, 1503.026203598089978, 233.3025785448990064 ) ) ;
#49637 = CARTESIAN_POINT ( 'NONE',  ( -6.266569382469999283, 1471.715264099330170, 270.0731618598979935 ) ) ;
#49638 = CARTESIAN_POINT ( 'NONE',  ( -1.397588342842136067, 1473.980173416578509, 219.2767284909027978 ) ) ;
#49639 = CARTESIAN_POINT ( 'NONE',  ( -119.6058480740470031, 1348.229899472569969, 304.2218459572590064 ) ) ;
#49640 = CARTESIAN_POINT ( 'NONE',  ( 38.48525439408140159, 1449.940833192290029, 135.6993408459150032 ) ) ;
#49641 = CARTESIAN_POINT ( 'NONE',  ( 13.92102725570000032, 1408.913060387329779, 196.5791615931979948 ) ) ;
#49642 = EDGE_CURVE ( 'NONE', #67100, #54363, #88159, .T. ) ;
#49643 = CARTESIAN_POINT ( 'NONE',  ( -20.40422799699999956, 1484.238920065389721, 212.0834907045089892 ) ) ;
#49644 = CARTESIAN_POINT ( 'NONE',  ( 18.17843454563659833, 1431.368984425399731, 207.2510453969530033 ) ) ;
#49645 = CARTESIAN_POINT ( 'NONE',  ( -22.93995821741350127, 1507.616838180419791, 207.8436709359779968 ) ) ;
#49646 = CARTESIAN_POINT ( 'NONE',  ( 9.369782510130001185, 1366.497526915280105, 207.6218459616989946 ) ) ;
#49647 = CARTESIAN_POINT ( 'NONE',  ( -33.55732945208360007, 1416.697737133469900, 266.7792439498080057 ) ) ;
#49648 = ADVANCED_FACE ( 'NONE', ( #12919 ), #19777, .T. ) ;
#49649 = EDGE_LOOP ( 'NONE', ( #26377, #20702, #24704, #32719 ) ) ;
#49650 = CARTESIAN_POINT ( 'NONE',  ( -8.301987938657498844, 1512.913060387330006, 185.0111222839169898 ) ) ;
#49651 = ORIENTED_EDGE ( 'NONE', *, *, #21399, .T. ) ;
#49652 = VECTOR ( 'NONE', #154, 999.9999999999998863 ) ;
#49653 = ORIENTED_EDGE ( 'NONE', *, *, #52310, .T. ) ;
#49654 = CARTESIAN_POINT ( 'NONE',  ( -2.864326125434999870, 1516.826109302209943, 211.6149197999869784 ) ) ;
#49655 = EDGE_CURVE ( 'NONE', #98249, #96193, #32330, .T. ) ;
#49656 = CARTESIAN_POINT ( 'NONE',  ( 5.186873127341490530, 1424.212018954599898, 193.3034105768099948 ) ) ;
#49657 = B_SPLINE_CURVE_WITH_KNOTS ( 'NONE', 5,
 ( #63630, #29980, #98293, #55778, #81479, #73675 ),
 .UNSPECIFIED., .F., .F.,
 ( 6, 6 ),
 ( 0.000000000000000000, 1.000000000000000000 ),
 .UNSPECIFIED. ) ;
#49659 = CARTESIAN_POINT ( 'NONE',  ( 22.69876404240077505, 1522.382868172863937, 181.3483716558180276 ) ) ;
#49658 = CARTESIAN_POINT ( 'NONE',  ( 3.266349474065000091, 1516.797038924770050, 213.1501537103870021 ) ) ;
#49660 = CARTESIAN_POINT ( 'NONE',  ( -17.60065947509999873, 1485.486750496030027, 188.6130784315979838 ) ) ;
#49661 = TOROIDAL_SURFACE ( 'NONE', #24590, 11.23850026409999892, 0.5000000000000000000 ) ;
#49662 = EDGE_CURVE ( 'NONE', #54701, #28004, #41199, .T. ) ;
#49663 = CARTESIAN_POINT ( 'NONE',  ( -17.05283090761910003, 1489.045462354059964, 229.1850863498580111 ) ) ;
#49664 = VERTEX_POINT ( 'NONE', #96953 ) ;
#49665 = CARTESIAN_POINT ( 'NONE',  ( -26.35085852639999970, 1436.712581025230065, 136.8307534946980013 ) ) ;
#49666 = B_SPLINE_CURVE_WITH_KNOTS ( 'NONE', 3,
 ( #35394, #44364, #61729, #69025, #26428, #79624, #78510, #19118, #53321, #35956, #60623, #61189, #28094, #70142, #104256 ),
 .UNSPECIFIED., .F., .F.,
 ( 4, 2, 2, 1, 1, 1, 2, 2, 4 ),
 ( 0.000000000000000000, 0.2500000000001068035, 0.3750000000001622036, 0.4375000000001886824, 0.4687500000001994516, 0.4843750000002050582, 0.4921875000002064460, 0.5000000000002078338, 1.000000000000000000 ),
 .UNSPECIFIED. ) ;
#49667 = CARTESIAN_POINT ( 'NONE',  ( -4.618119704395000191, 1516.706638732659940, 202.1845071865270143 ) ) ;
#49668 = DIRECTION ( 'NONE',  ( -0.01484500364079610613, 0.5669078173018522460, 0.8236474686107853049 ) ) ;
#49669 = CARTESIAN_POINT ( 'NONE',  ( -44.90400487128380291, 1384.599132857919813, 218.2254928299460062 ) ) ;
#49670 = CARTESIAN_POINT ( 'NONE',  ( -40.17393788466059590, 1425.544852429910179, 270.1489469183769643 ) ) ;
#49671 = LINE ( 'NONE', #74871, #105339 ) ;
#49673 = ORIENTED_EDGE ( 'NONE', *, *, #70951, .T. ) ;
#49672 = CARTESIAN_POINT ( 'NONE',  ( 15.49546526515152323, 1506.491018782020319, 193.4614169200511355 ) ) ;
#49674 = ORIENTED_EDGE ( 'NONE', *, *, #25313, .T. ) ;
#49675 = CARTESIAN_POINT ( 'NONE',  ( 19.01216659339999993, 1456.124166689789945, 212.8700632932389851 ) ) ;
#49676 = CARTESIAN_POINT ( 'NONE',  ( 14.38344716668426138, 1473.391868309870915, 269.5847338116742549 ) ) ;
#49677 = B_SPLINE_CURVE_WITH_KNOTS ( 'NONE', 3,
 ( #7817, #8360, #92927, #49293, #77253, #51487, #84529, #42529, #91824, #6717, #50401, #102424, #25705, #75605, #85618, #16738, #109201, #24050, #15639, #59907, #49845, #94028, #8917, #41987, #58244, #83975, #7275, #41439, #33015, #35232, #53158, #26834, #69420, #87298, #2766, #79456, #28493 ),
 .UNSPECIFIED., .F., .F.,
 ( 4, 3, 3, 3, 3, 3, 3, 3, 3, 3, 3, 3, 4 ),
 ( -7.354143352820449842, -7.102020254820109457, -6.848251370393399817, -6.567365280386119331, -6.254732362112719990, -5.795795420936189934, -5.472496633131050281, -5.187277023006039656, -5.019032731589150309, -4.627402102584190047, -4.173454028035540553, -3.481905268385339536, -3.020409492390000672 ),
 .UNSPECIFIED. ) ;
#49678 = PLANE ( 'NONE',  #78913 ) ;
#49679 = CARTESIAN_POINT ( 'NONE',  ( -24.45793889359999795, 1435.630516549809954, 137.6701772224979834 ) ) ;
#49680 = CARTESIAN_POINT ( 'NONE',  ( -24.90839019419999900, 1441.482377299550080, 210.4444839806880054 ) ) ;
#49681 = AXIS2_PLACEMENT_3D ( 'NONE', #18792, #72014, #79286 ) ;
#49682 = ADVANCED_FACE ( 'NONE', ( #47098 ), #53476, .T. ) ;
#49683 = CARTESIAN_POINT ( 'NONE',  ( -7.708770045145000083, 1516.524310051880093, 211.4128934593470035 ) ) ;
#49684 = CARTESIAN_POINT ( 'NONE',  ( -68.77199811340000224, 1379.747924854809980, 280.1875869621590027 ) ) ;
#49685 = CARTESIAN_POINT ( 'NONE',  ( 4.253771920025769759, 1442.472176597800171, 216.9083527837719885 ) ) ;
#49686 = CARTESIAN_POINT ( 'NONE',  ( -13.31050689240000118, 1414.983771850430003, 220.3937082497979816 ) ) ;
#49687 = CARTESIAN_POINT ( 'NONE',  ( 6.933587655514999781, 1516.542957540330008, 207.4124872689769745 ) ) ;
#49688 = EDGE_CURVE ( 'NONE', #29251, #56464, #49484, .T. ) ;
#49689 = ORIENTED_EDGE ( 'NONE', *, *, #44527, .T. ) ;
#49690 = CARTESIAN_POINT ( 'NONE',  ( -2.338016501012529780, 1451.953771032099894, 184.5921950015619757 ) ) ;
#49691 = CARTESIAN_POINT ( 'NONE',  ( -10.21277674610000119, 1472.144828979990052, 207.6413912857090054 ) ) ;
#49692 = CARTESIAN_POINT ( 'NONE',  ( -19.87038186279464114, 1456.668401910016200, 225.4203470789150288 ) ) ;
#49693 = EDGE_LOOP ( 'NONE', ( #48011, #52160, #62912, #17884, #53434, #94914, #42606, #30550, #100182, #109983 ) ) ;
#49694 = CARTESIAN_POINT ( 'NONE',  ( 7.334060111060000331, 1482.070333873989966, 210.1443983621290101 ) ) ;
#49695 = CARTESIAN_POINT ( 'NONE',  ( -22.68369965143373435, 1509.726148796831694, 228.1704579189521098 ) ) ;
#49696 = CARTESIAN_POINT ( 'NONE',  ( -4.079975117419219366, 1440.506274563688521, 185.2719822077098115 ) ) ;
#49697 = CARTESIAN_POINT ( 'NONE',  ( 17.04521188157742984, 1526.211528530236592, 182.6481290776079334 ) ) ;
#49698 = LINE ( 'NONE', #14953, #88862 ) ;
#49699 = CARTESIAN_POINT ( 'NONE',  ( 8.613733814799999777, 1488.162647577689995, 202.3373066378090073 ) ) ;
#49700 = DIRECTION ( 'NONE',  ( -1.000000000000000000, 0.000000000000000000, 0.000000000000000000 ) ) ;
#49701 = CARTESIAN_POINT ( 'NONE',  ( 4.258542316545229411, 1441.260261168030183, 159.7577179058740171 ) ) ;
#49702 = CIRCLE ( 'NONE', #97945, 3.058258088409981923 ) ;
#49704 = CARTESIAN_POINT ( 'NONE',  ( -11.89522282729999958, 1434.541161981840105, 151.0452005854980086 ) ) ;
#49703 = CARTESIAN_POINT ( 'NONE',  ( -4.612507312034999529, 1516.886345593249871, 214.1313240375470173 ) ) ;
#49705 = PLANE ( 'NONE',  #49568 ) ;
#49706 = CARTESIAN_POINT ( 'NONE',  ( 6.942973629204999497, 1516.833844030519913, 216.4505221401170161 ) ) ;
#49707 = VERTEX_POINT ( 'NONE', #90730 ) ;
#49708 = CARTESIAN_POINT ( 'NONE',  ( -17.42486771672220058, 1470.242291900930013, 228.5603268348579888 ) ) ;
#49709 = CARTESIAN_POINT ( 'NONE',  ( 16.11683780530001897, 1409.475866348431737, 193.1327335431978725 ) ) ;
#49710 = CARTESIAN_POINT ( 'NONE',  ( 2.261143588150000383, 1421.220611668830088, 183.2247237651980356 ) ) ;
#49711 = CARTESIAN_POINT ( 'NONE',  ( 0.4394944473979990329, 1474.293113249590078, 219.5254300097989812 ) ) ;
#49712 = CARTESIAN_POINT ( 'NONE',  ( -4.500000000000000000, 1432.413060387330006, 146.1721969590979882 ) ) ;
#49713 = CARTESIAN_POINT ( 'NONE',  ( -1234.711986934499919, 50.13405481564039690, -9668.243368258868941 ) ) ;
#49714 = CARTESIAN_POINT ( 'NONE',  ( -11.33492574265600084, 1471.089256498150007, 207.7878841706139781 ) ) ;
#49715 = CARTESIAN_POINT ( 'NONE',  ( 1.797565579689999860, 1415.903556134529936, 232.4419632246980143 ) ) ;
#49716 = CARTESIAN_POINT ( 'NONE',  ( 18.73327636269999985, 1416.067629296030191, 210.6711993623479771 ) ) ;
#49717 = CARTESIAN_POINT ( 'NONE',  ( -6.954065720117950100, 1521.551704408389924, 183.5505540514350002 ) ) ;
#49718 = CARTESIAN_POINT ( 'NONE',  ( -21.53712143570592730, 1523.621879633028584, 183.9400870382964968 ) ) ;
#49719 = CARTESIAN_POINT ( 'NONE',  ( 43.06295132563239747, 1440.913060355180050, 263.2597293094730162 ) ) ;
#49721 = CARTESIAN_POINT ( 'NONE',  ( 4.328283507529889995, 1515.109292691759947, 208.1261415868569884 ) ) ;
#49720 = CYLINDRICAL_SURFACE ( 'NONE', #33977, 2.000000000000003109 ) ;
#49722 = CARTESIAN_POINT ( 'NONE',  ( 13.21848706260000128, 1426.029874525029982, 222.0236330272979899 ) ) ;
#49723 = ORIENTED_EDGE ( 'NONE', *, *, #104902, .F. ) ;
#49724 = ORIENTED_EDGE ( 'NONE', *, *, #22731, .F. ) ;
#49725 = AXIS2_PLACEMENT_3D ( 'NONE', #88033, #77954, #104261 ) ;
#49726 = CARTESIAN_POINT ( 'NONE',  ( -19.87223104929999806, 1484.291808912129909, 191.2808552885979907 ) ) ;
#49727 = CARTESIAN_POINT ( 'NONE',  ( -24.40934744099999776, 1441.356666734659939, 212.0571328766980059 ) ) ;
#49728 = CARTESIAN_POINT ( 'NONE',  ( 12.89607781515299934, 1434.724834403989917, 149.2206011272099886 ) ) ;
#49729 = AXIS2_PLACEMENT_3D ( 'NONE', #59648, #57458, #15950 ) ;
#49730 = DIRECTION ( 'NONE',  ( -0.9824080081115912355, 0.000000000000000000, -0.1867471702549089174 ) ) ;
#49731 = CARTESIAN_POINT ( 'NONE',  ( -1.835536242490369840, 1450.383119622699951, 182.7750508701979868 ) ) ;
#49732 = VECTOR ( 'NONE', #56753, 1000.000000000000000 ) ;
#49733 = CARTESIAN_POINT ( 'NONE',  ( -1.947517617149490121, 1508.551704408389924, 220.0725308712329991 ) ) ;
#49734 = CARTESIAN_POINT ( 'NONE',  ( 20.17436656406337292, 1524.841055067847719, 180.5047911526335440 ) ) ;
#49735 = CARTESIAN_POINT ( 'NONE',  ( -66.20371065853919390, 1383.789130863189939, 290.1023055280760445 ) ) ;
#49736 = CIRCLE ( 'NONE', #80184, 2.000000000000001776 ) ;
#49737 = CARTESIAN_POINT ( 'NONE',  ( -13.34833196689999824, 1435.008643399920174, 194.9659071978979910 ) ) ;
#49739 =( BOUNDED_CURVE ( )  B_SPLINE_CURVE ( 3, ( #104665, #62144, #96270, #19547 ),
 .UNSPECIFIED., .F., .T. ) 
 B_SPLINE_CURVE_WITH_KNOTS ( ( 4, 4 ),
 ( 2.061459541078140223, 2.471661985137465045 ),
 .UNSPECIFIED. ) 
 CURVE ( )  GEOMETRIC_REPRESENTATION_ITEM ( )  RATIONAL_B_SPLINE_CURVE ( ( 1.000000000000000000, 0.9860269160151746703, 0.9860269160151746703, 1.000000000000000000 ) ) 
 REPRESENTATION_ITEM ( '' )  );
#49738 = CARTESIAN_POINT ( 'NONE',  ( 4.546874241639798697, 1466.877133849231996, 217.9623086141598662 ) ) ;
#49740 = CARTESIAN_POINT ( 'NONE',  ( 10.67479214083029859, 1490.933195892699814, 211.7486846328050092 ) ) ;
#49742 = ORIENTED_EDGE ( 'NONE', *, *, #67514, .F. ) ;
#49741 = CARTESIAN_POINT ( 'NONE',  ( 1.003916534810000094, 1455.812332551789950, 218.6660764286289691 ) ) ;
#49743 = DIRECTION ( 'NONE',  ( -1.000000000000000000, 0.000000000000000000, 0.000000000000000000 ) ) ;
#49744 = CARTESIAN_POINT ( 'NONE',  ( -42.16437246579999254, 1379.922095110709961, 237.2117980744589829 ) ) ;
#49745 = CARTESIAN_POINT ( 'NONE',  ( 8.224891776136750821, 1436.419357605579989, 206.5810456655080145 ) ) ;
#49746 = ORIENTED_EDGE ( 'NONE', *, *, #64602, .F. ) ;
#49747 = ORIENTED_EDGE ( 'NONE', *, *, #81481, .T. ) ;
#49748 = LINE ( 'NONE', #16103, #58209 ) ;
#49749 = CARTESIAN_POINT ( 'NONE',  ( 35.84871811701600564, 1437.378613743899905, 136.5365654117910026 ) ) ;
#49751 = CARTESIAN_POINT ( 'NONE',  ( -32.02808312589908013, 1501.977400791986611, 219.9649204700466782 ) ) ;
#49750 = DIRECTION ( 'NONE',  ( 0.000000000000000000, 1.000000000000000000, 0.000000000000000000 ) ) ;
#49752 = CARTESIAN_POINT ( 'NONE',  ( -6.533716117800000056, 1463.955653170889946, 200.7628773010889915 ) ) ;
#49753 = CARTESIAN_POINT ( 'NONE',  ( -106.2456710219999962, 1378.874444167599904, 300.8956198461589793 ) ) ;
#49754 = CARTESIAN_POINT ( 'NONE',  ( 2.508384027800000027, 1444.574164590290138, 203.3639928317590204 ) ) ;
#49755 = CARTESIAN_POINT ( 'NONE',  ( -29.36867415615329335, 1526.382868172863937, 200.9843407519612981 ) ) ;
#49756 = CARTESIAN_POINT ( 'NONE',  ( -9.371448800484090569, 1508.551704408389924, 218.5138698305420064 ) ) ;
#49757 = AXIS2_PLACEMENT_3D ( 'NONE', #52761, #86897, #71240 ) ;
#49758 = DIRECTION ( 'NONE',  ( -0.2781944220536289869, 0.3718881641442650099, -0.8856111205871658454 ) ) ;
#49759 = CARTESIAN_POINT ( 'NONE',  ( 18.28845126389499853, 1425.323877885890170, 225.4753632769809997 ) ) ;
#49760 = DIRECTION ( 'NONE',  ( 0.6450708608689574852, -0.04363816677874634425, -0.7628756745748105361 ) ) ;
#49761 = CARTESIAN_POINT ( 'NONE',  ( 4.934384483489999695, 1432.131467662490195, 200.8226675911659811 ) ) ;
#49762 = CARTESIAN_POINT ( 'NONE',  ( -2.500000000000000000, 1439.638128487539916, 168.7284197513979791 ) ) ;
#49763 = CARTESIAN_POINT ( 'NONE',  ( 32.85805783624308418, 1523.678648413191695, 217.1983043299902931 ) ) ;
#49764 = ORIENTED_EDGE ( 'NONE', *, *, #54811, .F. ) ;
#49765 = CARTESIAN_POINT ( 'NONE',  ( -2.416798835000000256, 1426.601114010129777, 146.0361887655980127 ) ) ;
#49766 = CARTESIAN_POINT ( 'NONE',  ( 19.14017132134949861, 1456.338359336380108, 227.2099314066680051 ) ) ;
#49767 = CARTESIAN_POINT ( 'NONE',  ( 16.15368040339999922, 1468.829548787329941, 189.5967691369980059 ) ) ;
#49768 = CARTESIAN_POINT ( 'NONE',  ( -9.751780903386149743E-09, 1474.814788804160116, 265.0004365400300230 ) ) ;
#49769 = ADVANCED_FACE ( 'NONE', ( #49302 ), #30271, .T. ) ;
#49770 = DIRECTION ( 'NONE',  ( -0.4794255386042040046, 2.935634756405673411E-17, 0.8775825618903723147 ) ) ;
#49771 = CARTESIAN_POINT ( 'NONE',  ( 1.063863508520000112, 1476.023003326389926, 197.6717150904989921 ) ) ;
#49772 = CARTESIAN_POINT ( 'NONE',  ( -105.5817487570000139, 1391.853821388999904, 305.4363301085589910 ) ) ;
#49773 = CARTESIAN_POINT ( 'NONE',  ( -0.5526888975579999919, 1482.197366675030025, 182.0017022400980125 ) ) ;
#49774 = CARTESIAN_POINT ( 'NONE',  ( -8.706712734255761532, 1361.212830504819522, 210.6218459617030021 ) ) ;
#49775 = CARTESIAN_POINT ( 'NONE',  ( -34.68852446352935459, 1522.382868172863937, 218.2490599186011764 ) ) ;
#49776 = CARTESIAN_POINT ( 'NONE',  ( 13.74984697784300103, 1509.157712962339929, 234.0060514757300041 ) ) ;
#49777 = CARTESIAN_POINT ( 'NONE',  ( -8.952944454599998991, 1424.162919053179849, 206.7489373822789673 ) ) ;
#49778 = CARTESIAN_POINT ( 'NONE',  ( 1.709766494024999917, 1516.959716008189844, 209.1091877442879934 ) ) ;
#49779 = VECTOR ( 'NONE', #89421, 1000.000000000000000 ) ;
#49780 = CARTESIAN_POINT ( 'NONE',  ( -7.878537825433329367, 1517.051704408389924, 218.1850669711710111 ) ) ;
#49781 = FACE_OUTER_BOUND ( 'NONE', #93668, .T. ) ;
#49782 = CARTESIAN_POINT ( 'NONE',  ( 7.401232516239121040, 1425.131641740689929, 212.4511809372470168 ) ) ;
#49783 = CARTESIAN_POINT ( 'NONE',  ( -25.80443457887890091, 1452.006586394169972, 135.2613506968589832 ) ) ;
#49784 = EDGE_LOOP ( 'NONE', ( #34453, #49316, #75559, #2705 ) ) ;
#49785 = EDGE_CURVE ( 'NONE', #99465, #101208, #6177, .T. ) ;
#49786 = CARTESIAN_POINT ( 'NONE',  ( 19.57999166029999927, 1422.088355037530164, 238.2202656793979827 ) ) ;
#49788 = CARTESIAN_POINT ( 'NONE',  ( -17.41346946009999996, 1410.020394389830017, 194.0661810129979870 ) ) ;
#49787 = CARTESIAN_POINT ( 'NONE',  ( -11.93165340550180176, 1491.195427457339974, 206.6891418979790274 ) ) ;
#49789 = CARTESIAN_POINT ( 'NONE',  ( -1.880825668594659827, 1419.500193221429981, 185.7240730368970105 ) ) ;
#49790 = FACE_OUTER_BOUND ( 'NONE', #87811, .T. ) ;
#49791 = CARTESIAN_POINT ( 'NONE',  ( -4.644345245587025772, 1378.331153274604731, 214.5506328342511893 ) ) ;
#49792 = EDGE_CURVE ( 'NONE', #26950, #23648, #30624, .T. ) ;
#49793 = CARTESIAN_POINT ( 'NONE',  ( -3.970108626409070585, 1452.774421139130027, 152.2533984705749788 ) ) ;
#49794 = CARTESIAN_POINT ( 'NONE',  ( -18.96271102769999928, 1416.819759739330038, 208.0003802813079972 ) ) ;
#49795 = ORIENTED_EDGE ( 'NONE', *, *, #67279, .F. ) ;
#49796 = CARTESIAN_POINT ( 'NONE',  ( -2.500000000000000000, 1424.573971167730178, 154.8453096575980226 ) ) ;
#49797 = DIRECTION ( 'NONE',  ( 1.755985294532464991E-16, -1.000000000000000000, 1.338183447452830017E-16 ) ) ;
#49798 = DIRECTION ( 'NONE',  ( 0.6205445805634681733, -0.7071067811868637643, 0.3390050494208930454 ) ) ;
#49800 = B_SPLINE_CURVE_WITH_KNOTS ( 'NONE', 3,
 ( #6666, #49791, #57099, #66054, #55986, #5575, #81704, #22337, #91225, #40820, #108017, #100178, #39725, #109686 ),
 .UNSPECIFIED., .F., .F.,
 ( 4, 2, 2, 1, 1, 2, 2, 4 ),
 ( 0.000000000000000000, 0.2500000000026890712, 0.3750000000040576986, 0.4375000000044669823, 0.4687500000046716520, 0.4843750000049625859, 0.5000000000052535754, 1.000000000000000000 ),
 .UNSPECIFIED. ) ;
#49799 = CARTESIAN_POINT ( 'NONE',  ( -3.121529044914340467, 1448.960344233920068, 184.5768609971525791 ) ) ;
#49801 = VERTEX_POINT ( 'NONE', #14570 ) ;
#49802 = VERTEX_POINT ( 'NONE', #81770 ) ;
#49803 = CARTESIAN_POINT ( 'NONE',  ( -53.46943927250000428, 1384.767240279849830, 230.7494116872589984 ) ) ;
#49804 = CARTESIAN_POINT ( 'NONE',  ( -23.63025210133929832, 1410.151946025710231, 209.7191186103189864 ) ) ;
#49805 = FACE_OUTER_BOUND ( 'NONE', #23339, .T. ) ;
#49806 = CARTESIAN_POINT ( 'NONE',  ( -106.3607387814799949, 1309.112692017090239, 308.0674118875990075 ) ) ;
#49807 = CARTESIAN_POINT ( 'NONE',  ( -45.54451795790711088, 1438.304327561658965, 266.1921463157105450 ) ) ;
#49808 = CIRCLE ( 'NONE', #101566, 0.9999999999999972244 ) ;
#49809 = AXIS2_PLACEMENT_3D ( 'NONE', #20692, #12303, #46494 ) ;
#49810 = CARTESIAN_POINT ( 'NONE',  ( -0.05455680805710000358, 1507.644790440630004, 237.3838523299980068 ) ) ;
#49811 = CARTESIAN_POINT ( 'NONE',  ( 4.678144193461809763, 1508.611354624159958, 211.6097691212250140 ) ) ;
#49812 = ORIENTED_EDGE ( 'NONE', *, *, #22156, .T. ) ;
#49813 = AXIS2_PLACEMENT_3D ( 'NONE', #77495, #41678, #795 ) ;
#49814 = CARTESIAN_POINT ( 'NONE',  ( 45.70155086610489548, 1446.155617659590007, 268.2197227342359724 ) ) ;
#49815 = CARTESIAN_POINT ( 'NONE',  ( -10.74720057723740041, 1391.913060387210180, 205.3639615661770108 ) ) ;
#49816 = CARTESIAN_POINT ( 'NONE',  ( -7.703846517339999700, 1425.539117803740055, 205.4402351432489979 ) ) ;
#49817 = CARTESIAN_POINT ( 'NONE',  ( -2.490245952555000031, 1516.691389976299888, 204.5134284255869943 ) ) ;
#49818 = ADVANCED_FACE ( 'NONE', ( #5073 ), #8086, .T. ) ;
#49819 = EDGE_LOOP ( 'NONE', ( #72629, #53078, #25402 ) ) ;
#49820 = CARTESIAN_POINT ( 'NONE',  ( -11.93818408299999945, 1433.480074519959999, 149.8972116839979947 ) ) ;
#49821 = CARTESIAN_POINT ( 'NONE',  ( 15.19269320784599842, 1513.356256558030054, 194.8382808670130260 ) ) ;
#49822 = DIRECTION ( 'NONE',  ( 0.9858563016923833633, 0.000000000000000000, 0.1675928173085483863 ) ) ;
#49823 = ORIENTED_EDGE ( 'NONE', *, *, #79881, .F. ) ;
#49824 = CARTESIAN_POINT ( 'NONE',  ( -10.52288318266220024, 1480.315364330569992, 209.5795690133369931 ) ) ;
#49825 = CARTESIAN_POINT ( 'NONE',  ( 26.55535786486069938, 1451.985785255079918, 135.0211946108499887 ) ) ;
#49826 = CARTESIAN_POINT ( 'NONE',  ( -16.66936639845609847, 1512.187213306747481, 237.7608804993221838 ) ) ;
#49827 = CARTESIAN_POINT ( 'NONE',  ( 9.921621853607028640, 1503.139275714190262, 217.1109786641990240 ) ) ;
#49828 = CARTESIAN_POINT ( 'NONE',  ( 7.616185062369999592, 1421.938201076239693, 195.7452753503989697 ) ) ;
#49829 = CARTESIAN_POINT ( 'NONE',  ( 21.97669732130000142, 1409.680503568630002, 212.0880462296879898 ) ) ;
#49830 = CARTESIAN_POINT ( 'NONE',  ( 10.41266471604430066, 1479.358872247189993, 205.9982438997039935 ) ) ;
#49831 = CARTESIAN_POINT ( 'NONE',  ( 1.838013827845350168, 1408.977245244529968, 186.8835531457910122 ) ) ;
#49833 = CARTESIAN_POINT ( 'NONE',  ( 29.61076903484002898, 1526.107876515966609, 220.7510285220318167 ) ) ;
#49832 = CARTESIAN_POINT ( 'NONE',  ( 2.163834958349999837, 1417.651400129230069, 234.2791204608979854 ) ) ;
#49834 = CARTESIAN_POINT ( 'NONE',  ( 10.70954747716070088, 1424.785111699970230, 206.5629283040009909 ) ) ;
#49835 = CIRCLE ( 'NONE', #69517, 7.932410439649999923 ) ;
#49836 = CARTESIAN_POINT ( 'NONE',  ( -11.08791805799999963, 1380.264457071439892, 215.5269815452789999 ) ) ;
#49837 = CARTESIAN_POINT ( 'NONE',  ( 11.15268687969999917, 1425.700851675330114, 101.7515397216980091 ) ) ;
#49838 = EDGE_LOOP ( 'NONE', ( #64298, #39337, #97041, #70405 ) ) ;
#49839 = CARTESIAN_POINT ( 'NONE',  ( 12.84940689358530008, 1416.524489948229984, 221.8577937504570059 ) ) ;
#49840 = CARTESIAN_POINT ( 'NONE',  ( -17.30770383199540419, 1417.598457286296025, 206.4021992971377699 ) ) ;
#49841 = CARTESIAN_POINT ( 'NONE',  ( 0.000000000000000000, 1526.382868172863937, 209.1218459616979999 ) ) ;
#49842 = CARTESIAN_POINT ( 'NONE',  ( -12.29865477999999968, 1392.006778701819940, 209.7413185055909821 ) ) ;
#49843 = CARTESIAN_POINT ( 'NONE',  ( 18.19590854888164699, 1522.382868172863937, 238.2026672068774644 ) ) ;
#49844 = CARTESIAN_POINT ( 'NONE',  ( 11.87355315023980040, 1421.630887076790032, 203.4247053331970108 ) ) ;
#49845 = CARTESIAN_POINT ( 'NONE',  ( -10.92292198257390012, 1462.727308076620147, 207.4371260179439957 ) ) ;
#49846 = CARTESIAN_POINT ( 'NONE',  ( -40.73184307449999864, 1445.563106277890029, 268.3665355202980436 ) ) ;
#49847 = CARTESIAN_POINT ( 'NONE',  ( -21.93662986374314627, 1509.528752971103586, 191.4093251536967273 ) ) ;
#49848 = CARTESIAN_POINT ( 'NONE',  ( 11.94328307949999868, 1433.499933921140155, 150.0080830760979893 ) ) ;
#49849 = CARTESIAN_POINT ( 'NONE',  ( 4.934393719438509684, 1432.131471246516185, 200.8226737949341612 ) ) ;
#49850 = CARTESIAN_POINT ( 'NONE',  ( -9.684192816560390327, 1460.964679204169897, 209.2041052100069862 ) ) ;
#49851 = CARTESIAN_POINT ( 'NONE',  ( 0.7241444745577421127, 1467.041521348942524, 235.5044523316612697 ) ) ;
#49852 = CARTESIAN_POINT ( 'NONE',  ( -107.1210572734698729, 1390.321908692038505, 299.4947318525922810 ) ) ;
#49853 = CARTESIAN_POINT ( 'NONE',  ( 6.937455853977830600, 1464.940067841279870, 217.7536605638889853 ) ) ;
#49854 = CARTESIAN_POINT ( 'NONE',  ( -15.71374344840000070, 1486.113479385830033, 186.6263592044980157 ) ) ;
#49855 = CARTESIAN_POINT ( 'NONE',  ( 4.090209565960320148, 1474.271260243390088, 219.7854241566030282 ) ) ;
#49856 = CARTESIAN_POINT ( 'NONE',  ( -17.63293958180000232, 1409.693803940329872, 224.3174265464980124 ) ) ;
#49857 = CARTESIAN_POINT ( 'NONE',  ( -8.124763164904772239, 1425.330096299151137, 208.9405766535813314 ) ) ;
#49858 = CARTESIAN_POINT ( 'NONE',  ( -0.3742911815734584757, 1477.585138614035486, 198.7218481745984775 ) ) ;
#49859 = CARTESIAN_POINT ( 'NONE',  ( -16.19484051460299767, 1409.478596682770103, 193.4350318415109768 ) ) ;
#49860 = CARTESIAN_POINT ( 'NONE',  ( 1.842962231260000028, 1515.064792882589927, 204.7923971856590128 ) ) ;
#49861 = DIRECTION ( 'NONE',  ( 0.9774101051267758411, 0.000000000000000000, 0.2113515706023144369 ) ) ;
#49862 = CARTESIAN_POINT ( 'NONE',  ( -16.83568187507700031, 1418.884533216219779, 201.2565367485750016 ) ) ;
#49863 = CARTESIAN_POINT ( 'NONE',  ( 2.370970874524634286, 1427.002265528474027, 134.0999999980980135 ) ) ;
#49864 = CARTESIAN_POINT ( 'NONE',  ( -19.43345977031810179, 1418.906471912719780, 207.3470523668889882 ) ) ;
#49865 = CARTESIAN_POINT ( 'NONE',  ( 0.1732173507811780033, 1478.442703680379964, 182.1612834630160194 ) ) ;
#49867 = ORIENTED_EDGE ( 'NONE', *, *, #54225, .T. ) ;
#49866 = CARTESIAN_POINT ( 'NONE',  ( -18.66420869458026388, 1526.382868172863937, 232.7837831374280881 ) ) ;
#49868 = CARTESIAN_POINT ( 'NONE',  ( 1.313045906442016575, 1526.382868172864619, 178.8771780891984804 ) ) ;
#49869 = CARTESIAN_POINT ( 'NONE',  ( 2.175409717514719593E-31, 1397.551704408390151, 209.1218459616989946 ) ) ;
#49870 = CARTESIAN_POINT ( 'NONE',  ( 12.06083241689999852, 1433.903765800100018, 149.9805303072979825 ) ) ;
#49871 = CARTESIAN_POINT ( 'NONE',  ( -40.98974505614270214, 1446.927689381900109, 134.0999999985419890 ) ) ;
#49872 = CARTESIAN_POINT ( 'NONE',  ( -109.5350879309999925, 1384.896829517670085, 297.1231432122589808 ) ) ;
#49873 = ORIENTED_EDGE ( 'NONE', *, *, #31699, .F. ) ;
#49874 = B_SPLINE_SURFACE_WITH_KNOTS ( 'NONE', 5, 5, ( 
 ( #48657, #81662, #106872, #82231, #81123, #73293 ),
 ( #91184, #14463, #82783, #107427, #40229, #74412 ),
 ( #108537, #20650, #4441, #54853, #30723, #3904 ),
 ( #30165, #92282, #67111, #17193, #49752, #93380 ),
 ( #24509, #83882, #101769, #84973, #50843, #15006 ),
 ( #32387, #6628, #91732, #41342, #83332, #40782 ),
 ( #15552, #50312, #32921, #7187, #84441, #49204 ),
 ( #34033, #109108, #101213, #42431, #23422, #67662 ),
 ( #66014, #58700, #66570, #33460, #25060, #59262 ) ),
 .UNSPECIFIED., .F., .F., .F.,
 ( 6, 3, 6 ),
 ( 6, 6 ),
 ( 11.38875369420000006, 15.52868752870000080, 24.98742667679999840 ),
 ( 0.000000000000000000, 2.000000000000000000 ),
 .UNSPECIFIED. ) ;
#49875 = CARTESIAN_POINT ( 'NONE',  ( -16.58903855651428572, 1524.412928176728428, 180.6442129362811784 ) ) ;
#49876 = CARTESIAN_POINT ( 'NONE',  ( 10.35181298299999852, 1478.133428305090092, 203.4857779180190107 ) ) ;
#49877 = CARTESIAN_POINT ( 'NONE',  ( -16.67289555338749807, 1420.528706056600186, 203.2438192415110052 ) ) ;
#49878 = CARTESIAN_POINT ( 'NONE',  ( -16.53242990339613883, 1526.073434386619283, 182.3092812937424583 ) ) ;
#49879 = CARTESIAN_POINT ( 'NONE',  ( -5.540266061381259988, 1433.565922541270083, 215.6367219123060011 ) ) ;
#49880 = FACE_OUTER_BOUND ( 'NONE', #25258, .T. ) ;
#49881 = CARTESIAN_POINT ( 'NONE',  ( 17.15254153798861481, 1516.660421270691131, 195.1616943382034322 ) ) ;
#49882 = DIRECTION ( 'NONE',  ( -0.8539859765994315399, 0.000000000000000000, 0.5202960232132425311 ) ) ;
#49883 = CARTESIAN_POINT ( 'NONE',  ( 4.325405441727872002, 1515.219201590508419, 210.9648081759952163 ) ) ;
#49884 = B_SPLINE_SURFACE_WITH_KNOTS ( 'NONE', 5, 5, ( 
 ( #105284, #29126, #107473, #96335, #55448, #30771 ),
 ( #89575, #71730, #28576, #46503, #106383, #45941 ),
 ( #11243, #29669, #47047, #20161, #39164, #73339 ),
 ( #80079, #2846, #45404, #37528, #53815, #3398 ),
 ( #38618, #106922, #30211, #64402, #21791, #55993 ),
 ( #90116, #13399, #13955, #5581, #58195, #76095 ) ),
 .UNSPECIFIED., .F., .F., .F.,
 ( 6, 6 ),
 ( 6, 6 ),
 ( 0.000000000000000000, 21.60352440750000014 ),
 ( 0.000000000000000000, 0.4689189027120000408 ),
 .UNSPECIFIED. ) ;
#49885 = CARTESIAN_POINT ( 'NONE',  ( -51.93884728859359967, 1385.026165428789909, 228.3837409096330191 ) ) ;
#49886 = CARTESIAN_POINT ( 'NONE',  ( -10.44852243557409999, 1391.913060387289988, 213.6776970188900009 ) ) ;
#49887 = CARTESIAN_POINT ( 'NONE',  ( 10.60756267625500016, 1423.066441122550032, 207.7293007016729973 ) ) ;
#49888 = ORIENTED_EDGE ( 'NONE', *, *, #83701, .T. ) ;
#49889 = CIRCLE ( 'NONE', #26683, 63.69383906210463664 ) ;
#49890 = CARTESIAN_POINT ( 'NONE',  ( -29.82725556129999944, 1451.416006550429984, 136.0664794209980073 ) ) ;
#49891 = CARTESIAN_POINT ( 'NONE',  ( 13.32090919908814719, 1443.086052842850677, 169.4274452085888072 ) ) ;
#49893 = EDGE_LOOP ( 'NONE', ( #9832, #105017, #55741, #12096, #66627 ) ) ;
#49892 = CARTESIAN_POINT ( 'NONE',  ( 5.508554876272072853, 1427.333971811663332, 134.0999999980980135 ) ) ;
#49894 = CARTESIAN_POINT ( 'NONE',  ( 2.125574643609999814, 1472.895346367389948, 219.1091941688290206 ) ) ;
#49895 = CIRCLE ( 'NONE', #3385, 1.000000000000009104 ) ;
#49896 = CARTESIAN_POINT ( 'NONE',  ( 18.19723846073130247, 1429.891490729359930, 209.9056605128800186 ) ) ;
#49897 = CARTESIAN_POINT ( 'NONE',  ( -109.8277101070000015, 1384.853340824010047, 311.3803954542589736 ) ) ;
#49898 = CARTESIAN_POINT ( 'NONE',  ( -0.09506836101312440834, 1419.889005963919999, 184.0928500010010112 ) ) ;
#49899 = PLANE ( 'NONE',  #98388 ) ;
#49900 = CARTESIAN_POINT ( 'NONE',  ( -16.98323195629999915, 1422.783711030229824, 226.9778976059980096 ) ) ;
#49901 = CARTESIAN_POINT ( 'NONE',  ( 33.91369114349999592, 1451.728768196330066, 134.7155302118979989 ) ) ;
#49902 = CARTESIAN_POINT ( 'NONE',  ( 7.374335209140000735, 1448.578211398790017, 202.8746320373990102 ) ) ;
#49903 = CARTESIAN_POINT ( 'NONE',  ( -117.0812559398341222, 1348.229899472569286, 298.0159978832119236 ) ) ;
#49904 = CARTESIAN_POINT ( 'NONE',  ( 12.54268436849999979, 1408.913060387329779, 223.0428732173979824 ) ) ;
#49905 = CARTESIAN_POINT ( 'NONE',  ( -29.74444329485024596, 1526.348417187218502, 217.2213265034480969 ) ) ;
#49906 = CARTESIAN_POINT ( 'NONE',  ( -7.337153806245000354, 1517.119374999550018, 205.8621166342670108 ) ) ;
#49907 = CIRCLE ( 'NONE', #14074, 1.999999999999911182 ) ;
#49908 = CARTESIAN_POINT ( 'NONE',  ( 4.222550915190000254, 1446.229941110429991, 170.5491765577980061 ) ) ;
#49909 = ORIENTED_EDGE ( 'NONE', *, *, #26542, .T. ) ;
#49910 = CARTESIAN_POINT ( 'NONE',  ( 15.57748978360000081, 1507.212883781729943, 225.5460497861979832 ) ) ;
#49911 = CARTESIAN_POINT ( 'NONE',  ( -20.86254339170000094, 1504.682062816289999, 214.2159060785090219 ) ) ;
#49913 = ORIENTED_EDGE ( 'NONE', *, *, #102212, .F. ) ;
#49912 = CARTESIAN_POINT ( 'NONE',  ( -68.57748934099369365, 1379.747497746340287, 280.1964141449130352 ) ) ;
#49914 = CARTESIAN_POINT ( 'NONE',  ( -8.926802433111017621, 1380.976221376709873, 217.7251549208844494 ) ) ;
#49915 = VERTEX_POINT ( 'NONE', #41995 ) ;
#49916 = CARTESIAN_POINT ( 'NONE',  ( -16.30010424779411338, 1514.508970279820687, 223.8444557749070327 ) ) ;
#49917 = CARTESIAN_POINT ( 'NONE',  ( 12.24365554470000106, 1500.600794515889902, 208.6479362693279711 ) ) ;
#49919 = CARTESIAN_POINT ( 'NONE',  ( 16.42165607296470142, 1410.864361973030100, 191.6455063637129967 ) ) ;
#49918 = CARTESIAN_POINT ( 'NONE',  ( -11.16129001045304037, 1425.156829533156497, 144.5843009260746044 ) ) ;
#49920 = CARTESIAN_POINT ( 'NONE',  ( 4.625359524845000792, 1517.025470194390209, 211.6020329869469947 ) ) ;
#49921 = CARTESIAN_POINT ( 'NONE',  ( 41.66477750127440061, 1443.168168707889890, 136.0651127029709926 ) ) ;
#49922 = CARTESIAN_POINT ( 'NONE',  ( -45.67177476579999507, 1438.126719573170021, 266.1885948884980166 ) ) ;
#49923 = CARTESIAN_POINT ( 'NONE',  ( -1.139345301468810190, 1509.018038237069959, 179.3524220471120145 ) ) ;
#49924 = CARTESIAN_POINT ( 'NONE',  ( 11.50641715432830736, 1464.045072788057723, 231.7617761124168965 ) ) ;
#49925 = CARTESIAN_POINT ( 'NONE',  ( -15.15808450826500042, 1514.857962383129916, 193.1672320681669817 ) ) ;
#49926 = CARTESIAN_POINT ( 'NONE',  ( -34.01975398719280008, 1437.014669684349883, 136.5579423247930038 ) ) ;
#49927 = ORIENTED_EDGE ( 'NONE', *, *, #97413, .T. ) ;
#49928 = CARTESIAN_POINT ( 'NONE',  ( -11.77904797301389905, 1483.168249568389911, 228.2502144964559818 ) ) ;
#49929 = CARTESIAN_POINT ( 'NONE',  ( -5.923682464646780943, 1517.151704408390060, 223.8623791742500089 ) ) ;
#49930 = ORIENTED_EDGE ( 'NONE', *, *, #109496, .F. ) ;
#49931 = VERTEX_POINT ( 'NONE', #85078 ) ;
#49932 = FACE_OUTER_BOUND ( 'NONE', #20515, .T. ) ;
#49933 = CARTESIAN_POINT ( 'NONE',  ( 14.10951807380980050, 1475.045409909879936, 225.3878574613659964 ) ) ;
#49934 = CARTESIAN_POINT ( 'NONE',  ( -14.25663218980999858, 1380.283631336060125, 210.3482944585310008 ) ) ;
#49935 = CARTESIAN_POINT ( 'NONE',  ( -14.74403395979999942, 1507.703932417990245, 209.3705301297690085 ) ) ;
#49936 = CARTESIAN_POINT ( 'NONE',  ( 4.325805487360000257, 1515.203924463989779, 210.5850643037490215 ) ) ;
#49937 = AXIS2_PLACEMENT_3D ( 'NONE', #16234, #66691, #42022 ) ;
#49938 = CARTESIAN_POINT ( 'NONE',  ( -12.33252012460000024, 1378.517259988440173, 208.8147234668570036 ) ) ;
#49939 = CARTESIAN_POINT ( 'NONE',  ( 40.71747595839759981, 1438.773003563400152, 135.3769917806320109 ) ) ;
#49940 = CARTESIAN_POINT ( 'NONE',  ( 3.254300166275531314, 1516.622698719816071, 215.8883720907380450 ) ) ;
#49941 = DIRECTION ( 'NONE',  ( -1.224227143275518948E-16, 0.02617694830788859853, 0.9996573249755569268 ) ) ;
#49942 = CARTESIAN_POINT ( 'NONE',  ( 38.70145357755679782, 1443.913060387331370, 136.9791754767358611 ) ) ;
#49943 = CARTESIAN_POINT ( 'NONE',  ( -79.02094512940820437, 1384.789308648159931, 281.7664325557580014 ) ) ;
#49944 = VERTEX_POINT ( 'NONE', #67758 ) ;
#49945 = CARTESIAN_POINT ( 'NONE',  ( 7.328676169885000036, 1516.833844030519913, 202.1788723028969912 ) ) ;
#49946 = CARTESIAN_POINT ( 'NONE',  ( 5.000329995535000016, 1516.770163853809890, 208.3657552043160024 ) ) ;
#49947 = ORIENTED_EDGE ( 'NONE', *, *, #57059, .T. ) ;
#49948 = CARTESIAN_POINT ( 'NONE',  ( 11.77042837613340076, 1427.129776104949997, 146.4520242493910018 ) ) ;
#49949 = CIRCLE ( 'NONE', #94602, 2.005929996893950573 ) ;
#49950 = CARTESIAN_POINT ( 'NONE',  ( 20.01779028520000026, 1497.692402115730147, 228.4662795307979763 ) ) ;
#49951 = VERTEX_POINT ( 'NONE', #25162 ) ;
#49952 = CARTESIAN_POINT ( 'NONE',  ( -13.43950372030000118, 1415.041103191730144, 220.5860819401979995 ) ) ;
#49953 = CARTESIAN_POINT ( 'NONE',  ( -11.81416737476160073, 1432.336398752800051, 150.4603277358870059 ) ) ;
#49954 = DIRECTION ( 'NONE',  ( -0.9455185755993178454, 0.000000000000000000, 0.3255681544571539798 ) ) ;
#49955 = CARTESIAN_POINT ( 'NONE',  ( -10.46614408832069998, 1462.592476666500033, 207.4320058997580247 ) ) ;
#49956 = CARTESIAN_POINT ( 'NONE',  ( 21.36074642202770235, 1409.675868270709998, 206.3811398801530004 ) ) ;
#49957 = CARTESIAN_POINT ( 'NONE',  ( -6.123233995736771213E-16, 1379.913060387289988, 209.1218459616989946 ) ) ;
#49958 = CARTESIAN_POINT ( 'NONE',  ( -10.18040284890000002, 1472.197773114690108, 205.9807533724089978 ) ) ;
#49959 = CARTESIAN_POINT ( 'NONE',  ( -8.704510423752683579, 1410.592478084298364, 187.9732723534475554 ) ) ;
#49960 = CARTESIAN_POINT ( 'NONE',  ( -57.97118228820000496, 1379.732619669730184, 257.2286833013590126 ) ) ;
#49961 = CARTESIAN_POINT ( 'NONE',  ( -16.43752754770000024, 1507.637957936329940, 224.7124590378979860 ) ) ;
#49963 = CARTESIAN_POINT ( 'NONE',  ( 5.811772643825870333, 1467.189857448589919, 199.6405403245489936 ) ) ;
#49962 = CARTESIAN_POINT ( 'NONE',  ( 15.10715599449999935, 1460.034514856529995, 231.8277951913980246 ) ) ;
#49964 = CARTESIAN_POINT ( 'NONE',  ( 19.96781675539999767, 1474.314029133290205, 212.0813829049089918 ) ) ;
#49965 = CARTESIAN_POINT ( 'NONE',  ( 5.779603100124999671, 1516.738222552470233, 216.8362174732170047 ) ) ;
#49966 = ORIENTED_EDGE ( 'NONE', *, *, #93911, .F. ) ;
#49967 = CIRCLE ( 'NONE', #82155, 1.000002391210522257 ) ;
#49968 = CARTESIAN_POINT ( 'NONE',  ( 18.04482939365169969, 1424.490669045140066, 224.3459621598859997 ) ) ;
#49969 = VECTOR ( 'NONE', #58155, 1000.000000000000114 ) ;
#49970 = CARTESIAN_POINT ( 'NONE',  ( 1.417628642355521551, 1516.580839848236337, 216.8320962620632599 ) ) ;
#49971 = CARTESIAN_POINT ( 'NONE',  ( -7.712490991114999694, 1516.666407245520077, 213.7387074786470009 ) ) ;
#49972 = CARTESIAN_POINT ( 'NONE',  ( 2.849563100782139813, 1515.551843419129909, 213.1048050505769993 ) ) ;
#49973 = CARTESIAN_POINT ( 'NONE',  ( -11.60004869885203682, 1425.972729341162221, 137.6380926570295173 ) ) ;
#49975 = ORIENTED_EDGE ( 'NONE', *, *, #65090, .T. ) ;
#49974 = CARTESIAN_POINT ( 'NONE',  ( 4.668116770205860355, 1508.551704407329908, 213.4552354802430045 ) ) ;
#49976 = CARTESIAN_POINT ( 'NONE',  ( 0.7195380765500000164, 1435.002040243880174, 189.5252041397980065 ) ) ;
#49977 = CARTESIAN_POINT ( 'NONE',  ( -0.3510182098590010069, 1508.319869606589918, 220.7744203783990145 ) ) ;
#49978 = CARTESIAN_POINT ( 'NONE',  ( -11.67186513969999950, 1426.308431726130038, 146.8889338853980178 ) ) ;
#49979 = CARTESIAN_POINT ( 'NONE',  ( -0.7666883967970010705, 1430.262722078590059, 214.7518399592089793 ) ) ;
#49980 = CARTESIAN_POINT ( 'NONE',  ( -6.384336360429650803, 1441.163446422609923, 202.7784055348689947 ) ) ;
#49981 = CARTESIAN_POINT ( 'NONE',  ( 3.165116523870669774, 1422.680542800070043, 151.1404971254699774 ) ) ;
#49982 = CARTESIAN_POINT ( 'NONE',  ( 8.206329918199999796, 1502.256773578390039, 208.4091422247220180 ) ) ;
#49983 = FACE_OUTER_BOUND ( 'NONE', #66788, .T. ) ;
#49985 = CARTESIAN_POINT ( 'NONE',  ( -10.39513868812339936, 1481.808198652379815, 206.4190733064540098 ) ) ;
#49984 = CARTESIAN_POINT ( 'NONE',  ( -23.52532681639999979, 1495.365128451330065, 222.1069804199980240 ) ) ;
#49986 = CARTESIAN_POINT ( 'NONE',  ( -16.61688624562800243, 1459.964452065093838, 228.4923530358620098 ) ) ;
#49987 = CIRCLE ( 'NONE', #26705, 2.009043929815852891 ) ;
#49988 = EDGE_LOOP ( 'NONE', ( #47553, #56012, #30508, #27159 ) ) ;
#49989 = CARTESIAN_POINT ( 'NONE',  ( -4.042729840925000317, 1516.919782530640077, 205.8674445284970034 ) ) ;
#49990 = CARTESIAN_POINT ( 'NONE',  ( 3.425626849559999965, 1406.160538305030059, 269.0410133635979832 ) ) ;
#49991 = CARTESIAN_POINT ( 'NONE',  ( 0.2517737633129999986, 1408.921852534829895, 186.0321150700980013 ) ) ;
#49992 = CARTESIAN_POINT ( 'NONE',  ( 24.61387732900000103, 1469.149509504730077, 202.9020163039279794 ) ) ;
#49993 = EDGE_CURVE ( 'NONE', #7587, #107938, #21263, .T. ) ;
#49994 = CARTESIAN_POINT ( 'NONE',  ( 9.898869979169477418, 1506.751914348593118, 229.0672400497726073 ) ) ;
#49995 = EDGE_CURVE ( 'NONE', #78944, #48269, #85338, .T. ) ;
#49996 = CARTESIAN_POINT ( 'NONE',  ( 1.663997124576299891, 1454.715882351969867, 218.3807490822640034 ) ) ;
#49997 = CARTESIAN_POINT ( 'NONE',  ( -1.634203459049999863, 1450.563733768360180, 183.1247155458980274 ) ) ;
#49998 = LINE ( 'NONE', #163, #3177 ) ;
#49999 = CARTESIAN_POINT ( 'NONE',  ( -15.17668577640000116, 1418.088921015730193, 203.1694998214689747 ) ) ;
#50000 = VECTOR ( 'NONE', #47960, 1000.000000000000000 ) ;
#50001 = CARTESIAN_POINT ( 'NONE',  ( -13.55026637619999974, 1443.926177729530082, 187.1800506178979902 ) ) ;
#50002 = EDGE_CURVE ( 'NONE', #83651, #88136, #80604, .T. ) ;
#50003 = CARTESIAN_POINT ( 'NONE',  ( -20.64585313979999981, 1475.513060387329915, 209.1218459620799877 ) ) ;
#50004 = EDGE_CURVE ( 'NONE', #1876, #87891, #37690, .T. ) ;
#50005 = CARTESIAN_POINT ( 'NONE',  ( -5.387811863060000483, 1496.648312753189884, 199.2595355468089906 ) ) ;
#50006 = CARTESIAN_POINT ( 'NONE',  ( 6.501109236959999649, 1407.992916451829842, 270.1283629016979830 ) ) ;
#50007 = CARTESIAN_POINT ( 'NONE',  ( 0.7498365066470009666, 1478.145630918389998, 201.5100879341690074 ) ) ;
#50008 = DIRECTION ( 'NONE',  ( 0.9858563016923833633, 0.000000000000000000, 0.1675928173085483863 ) ) ;
#50009 = B_SPLINE_SURFACE_WITH_KNOTS ( 'NONE', 5, 5, ( 
 ( #4141, #48905, #108782, #107685, #98725, #89776 ),
 ( #89228, #39929, #56177, #55104, #12524, #14161 ),
 ( #72450, #106580, #29867, #30969, #91439, #64053 ),
 ( #4675, #74098, #23107, #90316, #98172, #38814 ),
 ( #31514, #65145, #13594, #30419, #99258, #22536 ),
 ( #65696, #57312, #83032, #14715, #75199, #24206 ) ),
 .UNSPECIFIED., .F., .F., .F.,
 ( 6, 6 ),
 ( 6, 6 ),
 ( 5.115886119869999860, 6.089794067229999719 ),
 ( 0.000000000000000000, 2.000000000000000000 ),
 .UNSPECIFIED. ) ;
#50010 = CARTESIAN_POINT ( 'NONE',  ( 10.47511427260239891, 1482.040461736080033, 210.7458695605469927 ) ) ;
#50011 = CARTESIAN_POINT ( 'NONE',  ( -12.20132663145084351, 1377.775742761213451, 210.7787750133890086 ) ) ;
#50012 = CARTESIAN_POINT ( 'NONE',  ( -14.64892204319999891, 1474.348028616230067, 267.7626043892980192 ) ) ;
#50013 = FACE_OUTER_BOUND ( 'NONE', #56540, .T. ) ;
#50014 = CARTESIAN_POINT ( 'NONE',  ( -22.37111836880000126, 1509.698977978930088, 189.8981514860979871 ) ) ;
#50015 = CARTESIAN_POINT ( 'NONE',  ( -11.14879642162034834, 1486.511453154069613, 183.9882609373381683 ) ) ;
#50016 = CARTESIAN_POINT ( 'NONE',  ( -51.04490180185960213, 1384.735057055360130, 263.8868331049799849 ) ) ;
#50017 = CARTESIAN_POINT ( 'NONE',  ( -106.4061662575890068, 1391.913060387279984, 303.9266446755360676 ) ) ;
#50018 = CARTESIAN_POINT ( 'NONE',  ( -9.470907091730000005, 1435.946707556030105, 153.1784963645979758 ) ) ;
#50019 = B_SPLINE_SURFACE_WITH_KNOTS ( 'NONE', 5, 5, ( 
 ( #94166, #17436, #7962, #51634, #33161, #52744 ),
 ( #24737, #86878, #75737, #42129, #26412, #59494 ),
 ( #76279, #16883, #51088, #19100, #97488, #3453 ),
 ( #20756, #79059, #27525, #53873, #61710, #80690 ),
 ( #2907, #20216, #28075, #37581, #96392, #10172 ),
 ( #104789, #105903, #71219, #29723, #19668, #46002 ) ),
 .UNSPECIFIED., .F., .F., .F.,
 ( 6, 6 ),
 ( 6, 6 ),
 ( 6.633448128299999524, 17.60361827769999721 ),
 ( 0.000000000000000000, 2.000000000000000000 ),
 .UNSPECIFIED. ) ;
#50020 = CARTESIAN_POINT ( 'NONE',  ( -107.4284469309999963, 1379.017123567839917, 299.7421770867589998 ) ) ;
#50021 = CARTESIAN_POINT ( 'NONE',  ( -19.38211899475993860, 1526.344110814221267, 185.3185741806069871 ) ) ;
#50022 = LINE ( 'NONE', #25333, #25008 ) ;
#50023 = CARTESIAN_POINT ( 'NONE',  ( -17.22539857820000009, 1409.514584561230095, 195.8673760792980261 ) ) ;
#50024 = ADVANCED_FACE ( 'NONE', ( #61569 ), #3331, .T. ) ;
#50025 = CARTESIAN_POINT ( 'NONE',  ( -10.68354539818558457, 1379.426651953353030, 202.9127243954700646 ) ) ;
#50026 = DIRECTION ( 'NONE',  ( -0.000000000000000000, -1.000000000000000000, -0.000000000000000000 ) ) ;
#50027 = CIRCLE ( 'NONE', #32112, 1.000000000000000888 ) ;
#50028 = CARTESIAN_POINT ( 'NONE',  ( 10.99410683563099767, 1478.963161965750032, 206.4867629818700152 ) ) ;
#50029 = B_SPLINE_SURFACE_WITH_KNOTS ( 'NONE', 5, 1, ( 
 ( #102994, #87890 ),
 ( #19549, #1126 ),
 ( #94050, #34700 ),
 ( #70000, #26291 ),
 ( #27963, #96272 ),
 ( #94599, #59933 ) ),
 .UNSPECIFIED., .F., .F., .F.,
 ( 6, 6 ),
 ( 2, 2 ),
 ( 0.000000000000000000, 3.242714680140000194 ),
 ( 0.000000000000000000, 14.00000000000000000 ),
 .UNSPECIFIED. ) ;
#50030 = CARTESIAN_POINT ( 'NONE',  ( 0.8197920095480000224, 1434.541746329560056, 150.4759714514979976 ) ) ;
#50031 = CARTESIAN_POINT ( 'NONE',  ( -8.627774960320888198, 1437.492597821660183, 228.3379533698820012 ) ) ;
#50033 = EDGE_CURVE ( 'NONE', #33676, #99683, #105395, .T. ) ;
#50032 = CARTESIAN_POINT ( 'NONE',  ( -7.542447059886042027, 1510.549724835355164, 214.8727189264162121 ) ) ;
#50034 = CARTESIAN_POINT ( 'NONE',  ( -9.299436816696520225, 1446.922293005960000, 190.6945112479180011 ) ) ;
#50036 = CARTESIAN_POINT ( 'NONE',  ( -15.37680651676500077, 1514.414736986979960, 193.7541704988670119 ) ) ;
#50035 = CARTESIAN_POINT ( 'NONE',  ( -16.09548523901650086, 1416.444417915309941, 209.3983194699009971 ) ) ;
#50037 = FACE_OUTER_BOUND ( 'NONE', #86715, .T. ) ;
#50038 = DIRECTION ( 'NONE',  ( 1.755985294532469921E-16, -1.000000000000000000, 1.338183447452831989E-16 ) ) ;
#50039 = AXIS2_PLACEMENT_3D ( 'NONE', #8730, #34499, #57660 ) ;
#50040 = FACE_OUTER_BOUND ( 'NONE', #4451, .T. ) ;
#50041 = EDGE_CURVE ( 'NONE', #13824, #58183, #54282, .T. ) ;
#50042 = CARTESIAN_POINT ( 'NONE',  ( 7.718983249339360420, 1448.959774226909985, 202.2765896645470036 ) ) ;
#50043 = CARTESIAN_POINT ( 'NONE',  ( -0.01096399726330679961, 1407.225809184080163, 222.1218459612420020 ) ) ;
#50044 = CARTESIAN_POINT ( 'NONE',  ( 1.124289655455000148, 1517.184063036290127, 202.5579304082170040 ) ) ;
#50045 = LINE ( 'NONE', #32676, #15996 ) ;
#50046 = CARTESIAN_POINT ( 'NONE',  ( -13.01311093543085029, 1398.298642562823261, 209.5298158007715301 ) ) ;
#50047 = CARTESIAN_POINT ( 'NONE',  ( 16.74824990173500083, 1512.868709057579963, 195.8013333919669776 ) ) ;
#50048 = DIRECTION ( 'NONE',  ( -6.123233995736769734E-17, -1.000000000000000000, -1.124819836996399911E-32 ) ) ;
#50049 = CARTESIAN_POINT ( 'NONE',  ( -27.28088378283840143, 1377.835389488949886, 217.2864041108829838 ) ) ;
#50050 = CIRCLE ( 'NONE', #23244, 2.000000000000003109 ) ;
#50051 = CARTESIAN_POINT ( 'NONE',  ( 21.06226352934189805, 1509.331904505479997, 228.5875131670700000 ) ) ;
#50053 = ORIENTED_EDGE ( 'NONE', *, *, #33017, .F. ) ;
#50052 = CARTESIAN_POINT ( 'NONE',  ( -21.69319346089070066, 1379.597678304780175, 213.6345187343300154 ) ) ;
#50054 = ORIENTED_EDGE ( 'NONE', *, *, #56436, .F. ) ;
#50055 = CARTESIAN_POINT ( 'NONE',  ( 12.00150264383820087, 1433.875911295109745, 150.4160741115419739 ) ) ;
#50056 = CARTESIAN_POINT ( 'NONE',  ( -2.669690553840000202, 1397.993164424230145, 222.1390482242979942 ) ) ;
#50057 = VERTEX_POINT ( 'NONE', #96258 ) ;
#50058 = CARTESIAN_POINT ( 'NONE',  ( -4.602356253840000022, 1468.583955076089978, 189.7619545879989857 ) ) ;
#50059 = CARTESIAN_POINT ( 'NONE',  ( -26.26217022840000226, 1509.606683261929902, 199.1929658363279998 ) ) ;
#50060 = CARTESIAN_POINT ( 'NONE',  ( 0.0002840614181677549835, 1443.913060387330006, 126.7977857662820043 ) ) ;
#50061 =( BOUNDED_SURFACE ( )  B_SPLINE_SURFACE ( 3, 2, ( 
 ( #22983, #30846, #58274 ),
 ( #108103, #82366, #73424 ),
 ( #92397, #66145, #101333 ),
 ( #49875, #99691, #24623 ),
 ( #58820, #39250, #31399 ),
 ( #57188, #91312, #57739 ),
 ( #107560, #13477, #32517 ),
 ( #65022, #14594, #84008 ),
 ( #15133, #75634, #100268 ),
 ( #49323, #23547, #47667 ),
 ( #5097, #99140, #15670 ),
 ( #5664, #22417, #65579 ),
 ( #14034, #39812, #48782 ),
 ( #40351, #40903, #74532 ) ),
 .UNSPECIFIED., .F., .F., .T. ) 
 B_SPLINE_SURFACE_WITH_KNOTS ( ( 4, 2, 2, 2, 2, 2, 4 ),
 ( 3, 3 ),
 ( 0.000000000000000000, 0.0009440840677143893080, 0.001416126101571584016, 0.001888168135428778616, 0.002360210169285973433, 0.002832252203143168032, 0.003776336270857557232 ),
 ( 0.000000000000000000, 1.000000000000000000 ),
 .UNSPECIFIED. ) 
 GEOMETRIC_REPRESENTATION_ITEM ( )  RATIONAL_B_SPLINE_SURFACE ( (
 ( 1.000000000000000000, 0.8070209408750173008, 1.000000000000000000),
 ( 1.000000000000000000, 0.8215603905299677656, 1.000000000000000000),
 ( 1.000000000000000000, 0.8340988699039975085, 1.000000000000000000),
 ( 1.000000000000000000, 0.8516751610468989986, 1.000000000000000000),
 ( 1.000000000000000000, 0.8573697395150979839, 1.000000000000000000),
 ( 1.000000000000000000, 0.8683586635665277997, 1.000000000000000000),
 ( 1.000000000000000000, 0.8736518481714815598, 1.000000000000000000),
 ( 1.000000000000000000, 0.8840377753023912488, 1.000000000000000000),
 ( 1.000000000000000000, 0.8891294171303538718, 1.000000000000000000),
 ( 1.000000000000000000, 0.8992456600576697046, 1.000000000000000000),
 ( 1.000000000000000000, 0.9042785869253191500, 1.000000000000000000),
 ( 1.000000000000000000, 0.9189749222837818587, 1.000000000000000000),
 ( 1.000000000000000000, 0.9283978182348824326, 1.000000000000000000),
 ( 1.000000000000000000, 0.9376006582765940012, 1.000000000000000000) ) ) 
 REPRESENTATION_ITEM ( '' )  SURFACE ( )  );
#50063 = CARTESIAN_POINT ( 'NONE',  ( -11.75869035456349998, 1521.951704408389787, 190.9442076542370046 ) ) ;
#50062 = CARTESIAN_POINT ( 'NONE',  ( 2.375134825399999539, 1444.621758423489837, 200.4616579052089946 ) ) ;
#50064 = CARTESIAN_POINT ( 'NONE',  ( 17.76240486127710128, 1488.411413908479972, 229.6751878506049991 ) ) ;
#50065 = CARTESIAN_POINT ( 'NONE',  ( 12.55860337799999904, 1449.228661195309996, 188.0919213263979941 ) ) ;
#50066 = CARTESIAN_POINT ( 'NONE',  ( -9.626137457809999631, 1415.087974639930053, 194.4605678413980172 ) ) ;
#50067 = CARTESIAN_POINT ( 'NONE',  ( 17.84338787571921969, 1501.977400791986611, 180.3600277896298110 ) ) ;
#50068 = FILL_AREA_STYLE ('',( #77470 ) ) ;
#50069 = CARTESIAN_POINT ( 'NONE',  ( 0.5697989934087799302, 1450.893162568020216, 155.6080914323170248 ) ) ;
#50070 = CARTESIAN_POINT ( 'NONE',  ( 14.45556168306229949, 1416.765224586759814, 196.8540595995450246 ) ) ;
#50071 = CARTESIAN_POINT ( 'NONE',  ( 11.30246509490000051, 1432.392618652180090, 151.5218479388979915 ) ) ;
#50072 = CARTESIAN_POINT ( 'NONE',  ( 17.22592475670000312, 1443.913060387330006, 162.9227486557980171 ) ) ;
#50073 = ORIENTED_EDGE ( 'NONE', *, *, #82319, .F. ) ;
#50074 = CARTESIAN_POINT ( 'NONE',  ( 13.11641504695559846, 1435.029372730620025, 149.9328725522570096 ) ) ;
#50075 = VERTEX_POINT ( 'NONE', #2776 ) ;
#50076 = ORIENTED_EDGE ( 'NONE', *, *, #107596, .T. ) ;
#50077 = CARTESIAN_POINT ( 'NONE',  ( 13.16074665768760887, 1444.747289922009486, 169.3968467459069416 ) ) ;
#50078 = CARTESIAN_POINT ( 'NONE',  ( -8.514170057680001236, 1463.332792388330063, 234.7542372413980161 ) ) ;
#50079 = AXIS2_PLACEMENT_3D ( 'NONE', #17575, #49573, #93201 ) ;
#50080 = CARTESIAN_POINT ( 'NONE',  ( -106.3976693117229928, 1390.939243848519936, 307.7527733253859878 ) ) ;
#50081 = CARTESIAN_POINT ( 'NONE',  ( 4.036748838804999906, 1516.667393516340098, 216.0582443258770127 ) ) ;
#50082 = CARTESIAN_POINT ( 'NONE',  ( -8.431984396555888495, 1511.395334939771374, 213.8483103588398819 ) ) ;
#50083 = PRODUCT_RELATED_PRODUCT_CATEGORY ( 'part', '', ( #31272 ) ) ;
#50084 = VERTEX_POINT ( 'NONE', #18970 ) ;
#50085 = CARTESIAN_POINT ( 'NONE',  ( -12.14270316730000054, 1503.406043248689912, 208.4356947272389959 ) ) ;
#50086 = CARTESIAN_POINT ( 'NONE',  ( 2.500000000000000000, 1448.206111001999943, 170.1385578322760068 ) ) ;
#50087 = CARTESIAN_POINT ( 'NONE',  ( -26.37171023209999987, 1375.557882964970077, 211.7994354413090150 ) ) ;
#50088 = ORIENTED_EDGE ( 'NONE', *, *, #26725, .F. ) ;
#50089 = CARTESIAN_POINT ( 'NONE',  ( -7.336844680545000053, 1517.106845464700200, 205.6683011064770312 ) ) ;
#50090 = ORIENTED_EDGE ( 'NONE', *, *, #4346, .F. ) ;
#50091 = CARTESIAN_POINT ( 'NONE',  ( 21.61868135606060193, 1440.913060387330006, 225.5306503608640014 ) ) ;
#50092 = VECTOR ( 'NONE', #109670, 1000.000000000000000 ) ;
#50093 = CARTESIAN_POINT ( 'NONE',  ( -18.84923767200000100, 1508.518338890729865, 229.8981134190979958 ) ) ;
#50094 = CARTESIAN_POINT ( 'NONE',  ( -5.849946180559999931, 1410.053889712929958, 187.1442103566980109 ) ) ;
#50095 = CARTESIAN_POINT ( 'NONE',  ( 6.760013121875000586, 1512.520476835140016, 216.7629435481970006 ) ) ;
#50097 = ORIENTED_EDGE ( 'NONE', *, *, #82206, .F. ) ;
#50096 = CARTESIAN_POINT ( 'NONE',  ( -0.6611933175131969875, 1415.434635989099888, 227.0678344611339980 ) ) ;
#50098 = CARTESIAN_POINT ( 'NONE',  ( 18.32525213830000155, 1425.583872255029974, 224.3060837809979660 ) ) ;
#50099 = CARTESIAN_POINT ( 'NONE',  ( 26.79413740735880367, 1436.761939593030093, 136.7822073642480234 ) ) ;
#50100 = CARTESIAN_POINT ( 'NONE',  ( -109.9987472809999929, 1384.581606379090090, 311.2589846932590376 ) ) ;
#50102 = EDGE_CURVE ( 'NONE', #74270, #33006, #69840, .T. ) ;
#50101 = CARTESIAN_POINT ( 'NONE',  ( 6.012564370750140813E-06, 1465.118921926949952, 238.1343525961189869 ) ) ;
#50103 = EDGE_CURVE ( 'NONE', #36027, #33006, #53784, .T. ) ;
#50104 = CARTESIAN_POINT ( 'NONE',  ( 13.58968549309999929, 1409.153350369530017, 270.0972160545979932 ) ) ;
#50105 = CARTESIAN_POINT ( 'NONE',  ( -0.7360974767499980365, 1517.045004075700035, 213.1642344714070134 ) ) ;
#50106 = CARTESIAN_POINT ( 'NONE',  ( 23.01274080199999972, 1409.742907276529877, 209.3054936816029965 ) ) ;
#50107 = CARTESIAN_POINT ( 'NONE',  ( -20.80191066480000117, 1508.906210763929948, 189.9702950884980055 ) ) ;
#50108 = CARTESIAN_POINT ( 'NONE',  ( 2.594761893819999887, 1441.567844146989955, 218.7008844616090073 ) ) ;
#50109 = CARTESIAN_POINT ( 'NONE',  ( 7.320051241770920036, 1508.610505977480216, 215.2032452850019695 ) ) ;
#50110 = CARTESIAN_POINT ( 'NONE',  ( -1.701027861004999808, 1516.937508036699910, 211.6166039682370013 ) ) ;
#50111 = DIRECTION ( 'NONE',  ( 1.000000000000000000, -3.330669073900915523E-12, -7.524258993698327080E-10 ) ) ;
#50112 = PLANE ( 'NONE',  #17986 ) ;
#50113 = CARTESIAN_POINT ( 'NONE',  ( 1.356522472024429993, 1410.335674015750101, 232.6399073486850000 ) ) ;
#50115 = ORIENTED_EDGE ( 'NONE', *, *, #41192, .F. ) ;
#50114 = CARTESIAN_POINT ( 'NONE',  ( -67.70705029779999506, 1388.282036916160223, 263.9074574844589733 ) ) ;
#50116 = CARTESIAN_POINT ( 'NONE',  ( -47.51462801197750707, 1385.137171588540014, 256.6091612487379621 ) ) ;
#50117 = CIRCLE ( 'NONE', #7174, 2.000000000000001776 ) ;
#50118 = EDGE_CURVE ( 'NONE', #75143, #67449, #107374, .T. ) ;
#50119 = B_SPLINE_SURFACE_WITH_KNOTS ( 'NONE', 5, 5, ( 
 ( #108117, #65035, #63952, #39265, #98067, #4575 ),
 ( #31968, #4039, #56080, #48239, #90206, #14610 ),
 ( #90769, #57203, #5111, #55543, #89667, #73440 ),
 ( #12953, #31411, #99152, #47134, #22431, #82380 ),
 ( #59403, #42032, #41486, #101908, #92971, #6758 ),
 ( #102466, #34174, #91874, #25200, #25756, #32530 ),
 ( #15147, #16244, #16787, #49890, #58287, #85119 ),
 ( #84573, #7865, #42580, #49336, #75647, #66701 ),
 ( #50990, #57753, #84022, #7323, #8407, #109246 ),
 ( #110331, #76731, #109786, #43, #68360, #76181 ),
 ( #67253, #59956, #94072, #93515, #15684, #33064 ),
 ( #33603, #67799, #83463, #40918, #101347, #75098 ) ),
 .UNSPECIFIED., .F., .F., .F.,
 ( 6, 3, 3, 6 ),
 ( 6, 6 ),
 ( 47.73522590250000519, 49.52849703180000063, 53.11503929029999682, 57.48082753679999968 ),
 ( 0.000000000000000000, 1.553560449149999911 ),
 .UNSPECIFIED. ) ;
#50120 = CARTESIAN_POINT ( 'NONE',  ( 39.71670572960000101, 1443.385948747099974, 259.0959245980980086 ) ) ;
#50121 = CARTESIAN_POINT ( 'NONE',  ( -4.472278223723283652, 1370.472180122668533, 209.2025140426527230 ) ) ;
#50122 = CARTESIAN_POINT ( 'NONE',  ( -2.948785487947506390, 1495.323990659472429, 219.9171465939708980 ) ) ;
#50123 = AXIS2_PLACEMENT_3D ( 'NONE', #20681, #63838, #55429 ) ;
#50124 = CARTESIAN_POINT ( 'NONE',  ( -23.94395295139999646, 1445.403820339119875, 213.0920108038580167 ) ) ;
#50125 = LINE ( 'NONE', #84792, #84450 ) ;
#50127 = CARTESIAN_POINT ( 'NONE',  ( -8.581225640119999554, 1384.892862025920067, 218.6696712321190148 ) ) ;
#50126 = CARTESIAN_POINT ( 'NONE',  ( 4.616861508414999093, 1516.666407245520077, 216.8343369232169948 ) ) ;
#50128 = CARTESIAN_POINT ( 'NONE',  ( -9.181507157277641440, 1449.803788077400213, 209.6493162511999913 ) ) ;
#50129 = CARTESIAN_POINT ( 'NONE',  ( 10.62911018238626681, 1424.057524227967860, 137.5666922152020106 ) ) ;
#50130 = ORIENTED_EDGE ( 'NONE', *, *, #19897, .T. ) ;
#50131 = CARTESIAN_POINT ( 'NONE',  ( 3.258474578945000033, 1517.083030555940013, 202.5598499717069956 ) ) ;
#50132 = ADVANCED_FACE ( 'NONE', ( #12241 ), #19533, .F. ) ;
#50133 = CIRCLE ( 'NONE', #103749, 0.5000000000000029976 ) ;
#50134 = CARTESIAN_POINT ( 'NONE',  ( 7.460636200844970034, 1509.035273823678153, 215.1586051060212412 ) ) ;
#50135 = EDGE_CURVE ( 'NONE', #63792, #30404, #36016, .T. ) ;
#50136 = CARTESIAN_POINT ( 'NONE',  ( 12.73639929490000178, 1425.726110608229874, 223.7524270774979982 ) ) ;
#50137 = CARTESIAN_POINT ( 'NONE',  ( -19.66678637246580053, 1517.051704408389924, 215.8936635744080093 ) ) ;
#50138 = CARTESIAN_POINT ( 'NONE',  ( -2.157536728407480009, 1378.013060387289897, 210.3005136483574518 ) ) ;
#50139 = CARTESIAN_POINT ( 'NONE',  ( 4.378631935749999649, 1467.806944014989995, 218.0906305500190001 ) ) ;
#50140 = CARTESIAN_POINT ( 'NONE',  ( -37.66849514949689848, 1445.052233488579986, 137.0436250779820000 ) ) ;
#50141 = ADVANCED_FACE ( 'NONE', ( #105214 ), #63360, .F. ) ;
#50142 = CARTESIAN_POINT ( 'NONE',  ( 27.59657415728649710, 1435.460754930439862, 135.6994131913330079 ) ) ;
#50143 = CARTESIAN_POINT ( 'NONE',  ( -38.62863167585439328, 1444.143249040989986, 137.1666610592409938 ) ) ;
#50144 = CARTESIAN_POINT ( 'NONE',  ( -23.74109072509999763, 1436.296643562969848, 212.5883282660480234 ) ) ;
#50145 = CARTESIAN_POINT ( 'NONE',  ( -38.58901838188198496, 1459.202134673285173, 269.1648952399591508 ) ) ;
#50146 = CARTESIAN_POINT ( 'NONE',  ( -109.2771419979999905, 1386.778010587349854, 297.3694738813589993 ) ) ;
#50147 = CARTESIAN_POINT ( 'NONE',  ( -17.07770202869999565, 1418.344327071730049, 226.6533663141979957 ) ) ;
#50148 = CARTESIAN_POINT ( 'NONE',  ( -20.49599333844888349, 1525.960063244516959, 184.3798832129037635 ) ) ;
#50149 = CARTESIAN_POINT ( 'NONE',  ( -32.18870921241107652, 1460.503927282295081, 269.4955099690564566 ) ) ;
#50150 = VERTEX_POINT ( 'NONE', #70349 ) ;
#50151 = CARTESIAN_POINT ( 'NONE',  ( -26.68654750115280194, 1491.210633211110007, 210.8409592960780117 ) ) ;
#50152 = CARTESIAN_POINT ( 'NONE',  ( -32.12964233707795358, 1416.641442875106577, 269.3130421961114394 ) ) ;
#50153 = EDGE_CURVE ( 'NONE', #27470, #60953, #76037, .T. ) ;
#50154 = CARTESIAN_POINT ( 'NONE',  ( -765.6063658702573775, -8383.748406600814633, -1617.797774209815316 ) ) ;
#50155 = CARTESIAN_POINT ( 'NONE',  ( 14.15078481402130173, 1419.841391265170159, 190.8422908333620285 ) ) ;
#50156 = VECTOR ( 'NONE', #109920, 1000.000000000000000 ) ;
#50157 = CARTESIAN_POINT ( 'NONE',  ( -2.193083880730000129E-05, 1417.262443296330048, 235.9145984659979831 ) ) ;
#50158 = CARTESIAN_POINT ( 'NONE',  ( -28.45309225929999641, 1509.159855972630112, 208.7911923258060085 ) ) ;
#50159 = B_SPLINE_SURFACE_WITH_KNOTS ( 'NONE', 5, 5, ( 
 ( #22495, #87115, #10967, #88230, #70353, #2590, #36716, #65105, #48306, #99217, #82447, #69796, #90275, #11521, #10406, #3141, #78720, #104465, #70908, #45697, #105024, #75159, #15209, #48863, #7925, #109306, #33670, #7381, #100868, #24159, #109849, #93572, #25259 ),
 ( #5744, #40429, #108741, #74606, #57271, #49400, #91398, #93031, #32592, #16847, #92474, #42095, #66769, #76243, #16302, #50506, #57811, #24702, #58349, #83526, #31474, #41546, #65655, #75702, #67862, #15744, #100340, #39887, #84628, #82989, #67313, #91935, #33126 ),
 ( #51050, #49945, #23061, #23629, #14676, #110390, #74054, #101410, #101973, #6281, #58899, #59462, #32032, #108183, #66221, #99772, #6820, #40979, #84083, #94690, #18511, #52708, #26375, #17963, #19630, #70631, #655, #104749, #95795, #62226, #10136, #103074, #52158 ),
 ( #96352, #19062, #53267, #87406, #104198, #103647, #68419, #86843, #44307, #28036, #60570, #35339, #86291, #43747, #9575, #17403, #10699, #77898, #2324, #44871, #79022, #78451, #36434, #85182, #51599, #1205, #69527, #27483, #34786, #35902, #8468, #26945, #1764 ),
 ( #42641, #76794, #111, #70085, #34233, #102521, #77353, #61672, #61134, #95248, #25813, #60011, #94132, #85732, #68973, #9031, #43203, #30228, #105864, #46518, #80096, #98539, #72811, #38635, #106402, #21807, #63870, #97985, #21252, #5036, #105302, #106943, #29143 ),
 ( #55463, #54376, #13414, #64418, #89591, #63331, #4501, #38092, #36986, #72268, #107491, #39181, #87970, #56007, #30785, #11260, #28592, #64965, #12882, #71747, #90131, #29686, #81185, #3416, #47061, #47602, #81728, #53831, #88508, #45959, #11792, #62793, #97451 ),
 ( #73355, #2865, #96908, #37545, #45422, #20719, #99079, #79564, #71180, #20178, #80652, #54914, #89040, #12328, #3967, #108039, #58213, #92896, #91792, #22359, #31334, #49817, #15611, #40846, #82842, #40290, #32983, #67725, #15068, #39748, #6133, #73911, #24568 ),
 ( #50373, #65520, #75576, #84499, #99627, #109708, #22914, #48163, #67172, #41955, #5598, #31890, #66631, #100732, #74474, #66076, #56559, #7789, #48718, #76109, #101271, #110249, #92339, #108602, #100201, #58758, #57122, #23485, #16170, #57678, #33523, #90687, #83947 ),
 ( #7247, #13975, #49265, #83392, #6689, #75019, #91248, #109169, #32455, #41408, #24016, #82300, #14528, #8883, #35202, #102396, #61536, #10002, #69389, #525, #52575, #86159, #85042, #9451, #44735, #87267, #25125, #86709, #78885, #59329, #76654, #2191, #103500 ),
 ( #43616, #77765, #95115, #36305, #10561, #101832, #110804, #68834, #102936, #26802, #16709, #1076, #34096, #50911, #35761, #8332, #68288, #93999, #93440, #25679, #18379, #18934, #60989, #42496, #94545, #44173, #78310, #59872, #17263, #51455, #1625, #95666, #60427 ),
 ( #69945, #85587, #104059, #77224, #27352, #53130, #43064, #34650, #26238, #17818, #52019, #64294, #38506, #21130, #97855, #105738, #11662, #80528, #3844, #71053, #28467, #55891, #88916, #19497, #37971, #81062, #12202, #90010, #63208, #97315, #53699, #55337, #54784 ),
 ( #54246, #46397, #36860, #96781, #88372, #4377, #81602, #72685, #106808, #30099, #89469, #72153, #87840, #106271, #29557, #13287, #45838, #20585, #79971, #29022, #3289, #2739, #98413, #63742, #21685, #47479, #4907, #12764, #70500, #104617, #46943, #11128, #27913 ),
 ( #62095, #96220, #37420, #71618, #45287, #79428, #20052, #105175, #62659, #16042, #74888, #56987, #6012, #7117, #48025, #91118, #41272, #40165, #109581, #101151, #109039, #100608, #74347, #107916, #98958, #48588, #40716, #49137, #14942, #15490, #14394, #31758, #65394 ),
 ( #83817, #6566, #49687, #58633, #5461, #65944, #82722, #58086, #99499, #23892, #75445, #108475, #83270, #39622, #32852, #92219, #32322, #100069, #67044, #23354, #22232, #57545, #92765, #24445, #73225, #50243, #84372, #107368, #13840, #39045, #66504, #91668, #30664 ),
 ( #22782, #64849, #56430, #90561, #82162, #73790, #31210, #76519, #59195, #17125, #93314, #94983, #77090, #95531, #94405, #9868, #68696, #78173, #18251, #52447, #59736, #26658, #398, #51315, #33397, #43487, #67592, #9324, #35616, #34517, #102264, #7659, #86575 ),
 ( #26096, #68156, #25544, #44035, #52999, #102801, #24990, #93855, #16576, #1484, #41816, #943, #69812, #50771, #60859, #103929, #84906, #27228, #8197, #101699, #103356, #60286, #61408, #17681, #51887, #86023, #18803, #42364, #75972, #85451, #110669, #110124, #77631 ),
 ( #33962, #35068, #8749, #69248, #42932, #70367, #71483, #29972, #72551, #10422, #37840, #64164, #44591, #61966, #98282, #20456, #105043, #89339, #105604, #3710, #36732, #88793, #28888, #63083, #87132, #10982, #79296, #45157, #27776, #96647, #96080, #63620, #45712 ),
 ( #2607, #78736, #87702, #80396, #4241, #97182, #2051, #79849, #72027, #54665, #19355, #70927, #53556, #12075, #46812, #3160, #36184, #28332, #106142, #29421, #46268, #62524, #19915, #97736, #21559, #37292, #104483, #54116, #88244, #12635, #11537, #21007, #38375 ),
 ( #55210, #80942, #106681, #13704, #41135, #74217, #4772, #65807, #66371, #108346, #75315, #48461, #82599, #38918, #40586, #40035, #109458, #81468, #39491, #31628, #22097, #82027, #73662, #100490, #66917, #23771, #57958, #92091, #74758, #99926, #73099, #23220, #91546 ),
 ( #65261, #57420, #14823, #49010, #32187, #107794, #5889, #5331, #15369, #108895, #101026, #49559, #83687, #6983, #32737, #83146, #107238, #6441, #55769, #89884, #31078, #13154, #99372, #14270, #22645, #98837, #47340, #30529, #64721, #56296, #90426, #47891, #56850 ),
 ( #90982, #34396, #86452, #75851, #9204, #110548, #101573, #92637, #25968, #78051, #58507, #26540, #18131, #51764, #15910, #43908, #16454, #60167, #59606, #42801, #76395, #41692, #84236, #110001, #84781, #94856, #68025, #94285, #8626, #76961, #17563, #1358, #35500 ),
 ( #59063, #50650, #93186, #33278, #33835, #67468, #814, #93722, #69692, #270, #60735, #85329, #52329, #34940, #69127, #102134, #43365, #16999, #25413, #50110, #85898, #7536, #77512, #9742, #51199, #8077, #24324, #103230, #24861, #42248, #68571, #102670, #37711 ),
 ( #62394, #10292, #87577, #44469, #106028, #103812, #97076, #20889, #78614, #46143, #55087, #1929, #80273, #36067, #18678, #71912, #12509, #87003, #2489, #37165, #71360, #45037, #36606, #38250, #89215, #19223, #46688, #3587, #80819, #28760, #10865, #70806, #29304 ),
 ( #63501, #104920, #97620, #4125, #62964, #54546, #28205, #61842, #52874, #96518, #105473, #3039, #79730, #27111, #79182, #19796, #53429, #61296, #11957, #88679, #45589, #95414, #20341, #70252, #104359, #27656, #95962, #53999, #88131, #11420, #29852, #74082, #15237 ),
 ( #39912, #81899, #23091, #56721, #55638, #90857, #49429, #57834, #106564, #57297, #83551, #64038, #47218, #6844, #5769, #90298, #74630, #14144, #99797, #21970, #108211, #48331, #82471, #72434, #107112, #64591, #30400, #13031, #5206, #81345, #48888, #30954, #98155 ),
 ( #21428, #72973, #65679, #100366, #31499, #89760, #65129, #91424, #14699, #4659, #98710, #38798, #83016, #32058, #99242, #56162, #13579, #6308, #40453, #108765, #47765, #39359, #66247, #73533, #22518, #107668, #23652, #91960, #44753, #41005, #35782, #70519, #58376 ),
 ( #52596, #41572, #109872, #27931, #61010, #100892, #86731, #53150, #95137, #62114, #33696, #67891, #24187, #27373, #26825, #96239, #66792, #24728, #18398, #7407, #67339, #58925, #87288, #61555, #10022, #84107, #33151, #15769, #78335, #2210, #110416, #75183, #49971 ),
 ( #104079, #16329, #1646, #10583, #101438, #109333, #75727, #69966, #93056, #36322, #78902, #95688, #18954, #76268, #50529, #44192, #104634, #84654, #7951, #19515, #53720, #92502, #87857, #32616, #42120, #103521, #3860, #37988, #105194, #106826, #106287, #107383, #36876 ),
 ( #46959, #29040, #88932, #90025, #20069, #63225, #13302, #12219, #81619, #73243, #81079, #72701, #46413, #79988, #71071, #20602, #12781, #21146, #97871, #98430, #97331, #72170, #37438, #55907, #30116, #64311, #63758, #47495, #55353, #89486, #4396, #30679, #62677 ),
 ( #88390, #79445, #38523, #64866, #45308, #4922, #39064, #21702, #2756, #98974, #3308, #22248, #80545, #29572, #54800, #28485, #96799, #54262, #71635, #56446, #11145, #11678, #45855, #105755, #83836, #67610, #110141, #33414, #65411, #57563, #91685, #23909, #5479 ),
 ( #99517, #67062, #49155, #101720, #66522, #92785, #40735, #50263, #101168, #24462, #31778, #109600, #83287, #22802, #65965, #16060, #14960, #84392, #41835, #15507, #41292, #6585, #48605, #39639, #100090, #92236, #100626, #58105, #58651, #23372, #74909, #6030, #7679 ),
 ( #32342, #75991, #49706, #7137, #75466, #25012, #31229, #32872, #109059, #57008, #48042, #90578, #13858, #82181, #73808, #107937, #91136, #14413, #82739, #40183, #74365, #108493, #77649, #417, #76538, #8217, #110690, #8769, #18822, #102822, #60877, #43505, #963 ),
 ( #95003, #35087, #69268, #59213, #93878, #51335, #17144, #33981, #68717, #68176, #35636, #17701, #36201, #103374, #61426, #9343, #53017, #69830, #103947, #34535, #78193, #51905, #26116, #84924, #18271, #42382, #52464, #87152, #86045, #42950, #93332, #27245, #102283 ) ),
 .UNSPECIFIED., .F., .F., .F.,
 ( 6, 3, 3, 3, 3, 3, 3, 3, 3, 3, 6 ),
 ( 6, 3, 3, 3, 3, 3, 3, 3, 3, 3, 6 ),
 ( 0.000000000000000000, 1.936717162300000128, 3.873434324599999812, 4.841792905749999321, 5.810151486899999718, 7.746868649199999624, 9.683585811500000418, 10.65194439270000082, 11.62030297379999944, 13.55702013610000023, 15.49373729840000102 ),
 ( 0.000000000000000000, 1.936717162300000128, 3.873434324599999812, 4.841792905749999321, 5.810151486899999718, 7.746868649199999624, 9.683585811500000418, 10.65194439270000082, 11.62030297379999944, 13.55702013610000023, 15.49373729840000102 ),
 .UNSPECIFIED. ) ;
#50160 = CARTESIAN_POINT ( 'NONE',  ( -13.92686555291570194, 1517.051704405520013, 226.1812314194930025 ) ) ;
#50161 = CARTESIAN_POINT ( 'NONE',  ( -4.324121584285179232, 1515.222544093250008, 212.0786738497689896 ) ) ;
#50162 = EDGE_CURVE ( 'NONE', #3955, #20783, #64481, .T. ) ;
#50163 = CARTESIAN_POINT ( 'NONE',  ( 44.93133457081440696, 1436.268913138369953, 269.6838197541450199 ) ) ;
#50164 = CARTESIAN_POINT ( 'NONE',  ( -19.99928269779077894, 1450.982390009973869, 145.5778244573470488 ) ) ;
#50165 = CARTESIAN_POINT ( 'NONE',  ( -16.96258009527109678, 1415.088012641449950, 209.3926123311109961 ) ) ;
#50166 = CARTESIAN_POINT ( 'NONE',  ( 24.63108249569999941, 1435.637769007679935, 137.3321585077979989 ) ) ;
#50167 = CARTESIAN_POINT ( 'NONE',  ( 2.930838039564999775, 1510.983859056260144, 216.6855341620170350 ) ) ;
#50168 = ORIENTED_EDGE ( 'NONE', *, *, #1619, .F. ) ;
#50169 = VECTOR ( 'NONE', #68171, 1000.000000000000114 ) ;
#50170 = CARTESIAN_POINT ( 'NONE',  ( -0.1956065448698070253, 1414.913060387399810, 193.0575752666509857 ) ) ;
#50171 = CARTESIAN_POINT ( 'NONE',  ( -20.20959865099451847, 1511.187213306747708, 236.2316688286741453 ) ) ;
#50172 = VERTEX_POINT ( 'NONE', #36713 ) ;
#50173 = VERTEX_POINT ( 'NONE', #88227 ) ;
#50174 = CARTESIAN_POINT ( 'NONE',  ( 17.97082642953529685, 1416.218047878440075, 208.7667215553299798 ) ) ;
#50176 = CARTESIAN_POINT ( 'NONE',  ( -7.528156686780000051, 1459.758987806329969, 216.2975364203180106 ) ) ;
#50175 = CARTESIAN_POINT ( 'NONE',  ( 3.561219592449999638, 1455.895344195389953, 218.7021084924690228 ) ) ;
#50177 = CARTESIAN_POINT ( 'NONE',  ( -1.194279839290000034, 1444.571198474990069, 218.0071126885590047 ) ) ;
#50178 = ADVANCED_FACE ( 'NONE', ( #3693 ), #68080, .T. ) ;
#50179 = CARTESIAN_POINT ( 'NONE',  ( -10.98575270039999907, 1433.172656335930014, 151.7674558586979856 ) ) ;
#50180 = CARTESIAN_POINT ( 'NONE',  ( -12.29868253919850041, 1378.334373735910049, 209.9676400962160301 ) ) ;
#50181 = CARTESIAN_POINT ( 'NONE',  ( -2.712300100236232581, 1420.170182972836528, 186.0200053761597587 ) ) ;
#50182 = CARTESIAN_POINT ( 'NONE',  ( 7.541206810410000294, 1424.198099201060131, 212.4425681308690059 ) ) ;
#50184 = EDGE_CURVE ( 'NONE', #57810, #967, #86746, .T. ) ;
#50183 = CARTESIAN_POINT ( 'NONE',  ( -24.29993749309999984, 1439.467978180069849, 211.6888154952279990 ) ) ;
#50185 = FACE_BOUND ( 'NONE', #7380, .T. ) ;
#50186 = CARTESIAN_POINT ( 'NONE',  ( 3.322969174999999886, 1451.336469026030045, 183.9873339521979858 ) ) ;
#50187 = EDGE_CURVE ( 'NONE', #97278, #10122, #54648, .T. ) ;
#50188 = CARTESIAN_POINT ( 'NONE',  ( 9.258247136812819633, 1363.198586359113960, 210.6218459616987957 ) ) ;
#50189 = CARTESIAN_POINT ( 'NONE',  ( -20.67345146974625081, 1509.752679656905684, 230.8614569593614760 ) ) ;
#50191 = VERTEX_POINT ( 'NONE', #38354 ) ;
#50190 = CARTESIAN_POINT ( 'NONE',  ( 4.987078435459999071, 1508.551704408389924, 209.1218459616989946 ) ) ;
#50192 = ORIENTED_EDGE ( 'NONE', *, *, #51415, .T. ) ;
#50193 = CARTESIAN_POINT ( 'NONE',  ( -11.76828283236710071, 1427.072440769260083, 146.3134061956550056 ) ) ;
#50194 = CARTESIAN_POINT ( 'NONE',  ( 7.548952298499977509, 1510.510563526942860, 203.4716113541371385 ) ) ;
#50195 = CARTESIAN_POINT ( 'NONE',  ( -6.401487761410000310, 1472.929829178429827, 270.4245279986980108 ) ) ;
#50196 = CARTESIAN_POINT ( 'NONE',  ( 11.99692654816771764, 1433.680601540482940, 147.5897107170167999 ) ) ;
#50197 = CARTESIAN_POINT ( 'NONE',  ( -113.4000000000000057, 1340.114449826970031, 321.4803018775700139 ) ) ;
#50198 = CIRCLE ( 'NONE', #51942, 1.999999999999996669 ) ;
#50199 = CARTESIAN_POINT ( 'NONE',  ( 20.64585313979999981, 1475.513060387329915, 209.1218459613160121 ) ) ;
#50200 = CARTESIAN_POINT ( 'NONE',  ( -7.967089726150001106, 1384.601477608269988, 199.5004311937889838 ) ) ;
#50201 = B_SPLINE_SURFACE_WITH_KNOTS ( 'NONE', 4, 5, ( 
 ( #36894, #88405, #31795, #101743, #7154, #16615 ),
 ( #15526, #6600, #50812, #109616, #49722, #58669 ),
 ( #92805, #100108, #101186, #5499, #16077, #39655 ),
 ( #24483, #65986, #91705, #48626, #57579, #108508 ),
 ( #33432, #67083, #83854, #50280, #40200, #65429 ) ),
 .UNSPECIFIED., .F., .F., .F.,
 ( 5, 5 ),
 ( 6, 6 ),
 ( 140.3375011859999972, 157.7108139780000045 ),
 ( -2.775557561569999727E-17, 1.000000000000000000 ),
 .UNSPECIFIED. ) ;
#50202 = CARTESIAN_POINT ( 'NONE',  ( 3.552713678799999608E-15, 1413.913060387330006, 209.1218459616989946 ) ) ;
#50203 = CARTESIAN_POINT ( 'NONE',  ( -15.53391875520000021, 1431.113060387329824, 198.5194791727979862 ) ) ;
#50204 = CARTESIAN_POINT ( 'NONE',  ( 8.988338641398978979, 1366.896325247141931, 210.6218459616991936 ) ) ;
#50205 = CARTESIAN_POINT ( 'NONE',  ( -9.499875067660077832, 1448.112547453520165, 210.0994082806479923 ) ) ;
#50206 = CARTESIAN_POINT ( 'NONE',  ( -6.096347920628879535, 1406.294202297779975, 266.9462307650929915 ) ) ;
#50207 = CARTESIAN_POINT ( 'NONE',  ( -13.24203370085249887, 1434.890687171669924, 149.2201380983239858 ) ) ;
#50208 = ORIENTED_EDGE ( 'NONE', *, *, #23454, .F. ) ;
#50209 = DIRECTION ( 'NONE',  ( 0.000000000000000000, 1.000000000000000000, 0.000000000000000000 ) ) ;
#50210 = ORIENTED_EDGE ( 'NONE', *, *, #10940, .T. ) ;
#50211 = ORIENTED_EDGE ( 'NONE', *, *, #14464, .T. ) ;
#50212 = CARTESIAN_POINT ( 'NONE',  ( 4.969930027270518913, 1422.577112182319297, 184.4052530213058958 ) ) ;
#50213 = CARTESIAN_POINT ( 'NONE',  ( 6.664268339219599824, 1424.601171630709814, 193.8494905227429967 ) ) ;
#50215 = DIRECTION ( 'NONE',  ( -1.156023075842281927E-31, 1.000000000000000000, -1.698192320643030073E-16 ) ) ;
#50214 = CARTESIAN_POINT ( 'NONE',  ( 4.041472473744999405, 1516.858649670339901, 213.1514186109370144 ) ) ;
#50216 = CARTESIAN_POINT ( 'NONE',  ( 7.487063056100070391, 1517.051702153270071, 209.5621714086410066 ) ) ;
#50217 = CIRCLE ( 'NONE', #94876, 0.5869591139725545137 ) ;
#50218 = CARTESIAN_POINT ( 'NONE',  ( -17.58460357419609821, 1489.029734904510178, 229.1403506008609838 ) ) ;
#50219 = ORIENTED_EDGE ( 'NONE', *, *, #13848, .F. ) ;
#50220 = CARTESIAN_POINT ( 'NONE',  ( -105.7397520800000166, 1374.768546414190041, 302.6503159984590070 ) ) ;
#50221 = CARTESIAN_POINT ( 'NONE',  ( -2.292940207144999576, 1516.565291103010168, 202.5758065368070220 ) ) ;
#50222 = DIRECTION ( 'NONE',  ( 0.7063774289747313251, 0.04540766091858282338, 0.7063774289747313251 ) ) ;
#50223 = CARTESIAN_POINT ( 'NONE',  ( -43.91345046917300010, 1384.595606055820099, 217.0465566091490075 ) ) ;
#50224 = DIRECTION ( 'NONE',  ( 3.828568698926946970E-16, 0.000000000000000000, -1.000000000000000000 ) ) ;
#50225 = AXIS2_PLACEMENT_3D ( 'NONE', #18464, #110343, #33616 ) ;
#50226 = CARTESIAN_POINT ( 'NONE',  ( -8.106555885276549134, 1438.741351455190170, 205.9368832915250209 ) ) ;
#50228 = ORIENTED_EDGE ( 'NONE', *, *, #38568, .T. ) ;
#50227 = DIRECTION ( 'NONE',  ( 0.3679048462383223694, -0.7071067811868645414, 0.6038592750913975848 ) ) ;
#50229 = CARTESIAN_POINT ( 'NONE',  ( -26.62563451980019735, 1469.324738576180152, 209.5519976422650075 ) ) ;
#50230 = CARTESIAN_POINT ( 'NONE',  ( 25.57394743849999941, 1488.682087793829851, 216.3815040199180260 ) ) ;
#50231 = CARTESIAN_POINT ( 'NONE',  ( 16.16632277704778176, 1512.187213306747481, 181.3470724465435069 ) ) ;
#50232 = CARTESIAN_POINT ( 'NONE',  ( 10.92202464131200124, 1460.857965367780025, 208.4167310687169845 ) ) ;
#50233 = EDGE_CURVE ( 'NONE', #18362, #44275, #66744, .T. ) ;
#50234 = CARTESIAN_POINT ( 'NONE',  ( -4.429742689765809871, 1508.551704408389924, 204.3196046976010223 ) ) ;
#50235 = VECTOR ( 'NONE', #48762, 999.9999999999998863 ) ;
#50236 = CARTESIAN_POINT ( 'NONE',  ( -24.35749803060000218, 1441.519803165160056, 211.7220366884380098 ) ) ;
#50237 = CARTESIAN_POINT ( 'NONE',  ( 2.494020282435000180, 1516.876240617270014, 211.4047611534970201 ) ) ;
#50238 = CARTESIAN_POINT ( 'NONE',  ( -68.62428177750000202, 1379.748209670530059, 279.8484656398590005 ) ) ;
#50239 = CARTESIAN_POINT ( 'NONE',  ( -2.064501014040000193, 1497.911843841890004, 200.8390656523289977 ) ) ;
#50240 = CIRCLE ( 'NONE', #86081, 24.94174191160003318 ) ;
#50241 = CARTESIAN_POINT ( 'NONE',  ( -14.37239935340000052, 1413.178551036030058, 226.9209306701980040 ) ) ;
#50242 = DIRECTION ( 'NONE',  ( 0.000000000000000000, 1.000000000000000000, 0.000000000000000000 ) ) ;
#50243 = CARTESIAN_POINT ( 'NONE',  ( -4.045182518055000287, 1517.057265928030120, 207.4180663268770104 ) ) ;
#50244 = VERTEX_POINT ( 'NONE', #78716 ) ;
#50245 = CARTESIAN_POINT ( 'NONE',  ( -2.111185581749480011, 1451.947978409319830, 184.4701806085570013 ) ) ;
#50246 = CARTESIAN_POINT ( 'NONE',  ( -11.16643432470000086, 1471.372555798990106, 206.7508257807689915 ) ) ;
#50247 = CARTESIAN_POINT ( 'NONE',  ( -19.12315338958239153, 1457.731911782933594, 226.6848971428718471 ) ) ;
#50248 = ORIENTED_EDGE ( 'NONE', *, *, #48772, .T. ) ;
#50250 = CIRCLE ( 'NONE', #59202, 1.000000000000000888 ) ;
#50249 = DIRECTION ( 'NONE',  ( 0.000000000000000000, 1.000000000000000000, -1.836970198721029688E-16 ) ) ;
#50251 = EDGE_CURVE ( 'NONE', #10827, #74353, #39597, .T. ) ;
#50252 = CARTESIAN_POINT ( 'NONE',  ( 12.78027909502899995, 1434.687120491519863, 149.6292676778430177 ) ) ;
#50253 = CARTESIAN_POINT ( 'NONE',  ( 12.69480686662079805, 1459.299630678179938, 231.0330950081669812 ) ) ;
#50254 = CARTESIAN_POINT ( 'NONE',  ( -9.608263814349999876, 1414.782003256130110, 207.8393504740089952 ) ) ;
#50255 = CARTESIAN_POINT ( 'NONE',  ( -3.171072485709999889, 1451.871858332230204, 182.7750508701979868 ) ) ;
#50256 = EDGE_CURVE ( 'NONE', #69935, #84966, #1284, .T. ) ;
#50257 = CARTESIAN_POINT ( 'NONE',  ( 4.151488833330000183, 1485.695544300589972, 199.1893064789089749 ) ) ;
#50258 = CARTESIAN_POINT ( 'NONE',  ( 3.791557891630739974, 1430.522366444419958, 217.8194754324450173 ) ) ;
#50259 = CARTESIAN_POINT ( 'NONE',  ( 19.53786426059039982, 1511.187213306747708, 236.7197124308265188 ) ) ;
#50261 = CARTESIAN_POINT ( 'NONE',  ( -11.98890328080000067, 1442.756953654919926, 147.5994355510979688 ) ) ;
#50260 = CARTESIAN_POINT ( 'NONE',  ( 0.7564342142240020328, 1516.783665406140017, 213.7345173100169973 ) ) ;
#50262 = CARTESIAN_POINT ( 'NONE',  ( 20.50069307629999926, 1509.057110917230148, 189.1022581845979857 ) ) ;
#50263 = CARTESIAN_POINT ( 'NONE',  ( 4.036748838804999906, 1516.667393516340098, 216.0582443258770127 ) ) ;
#50264 = ORIENTED_EDGE ( 'NONE', *, *, #77712, .T. ) ;
#50265 = CARTESIAN_POINT ( 'NONE',  ( 7.719451313342379883, 1516.932212683739863, 209.1137067812010173 ) ) ;
#50266 = CARTESIAN_POINT ( 'NONE',  ( -16.72115780329999879, 1420.505589990380031, 203.2363230761090165 ) ) ;
#50267 = CARTESIAN_POINT ( 'NONE',  ( 0.4555793700929999801, 1420.350633689530014, 183.9786678279979810 ) ) ;
#50268 = CARTESIAN_POINT ( 'NONE',  ( -1.281400930710000052, 1474.396637362589900, 219.3408303083989779 ) ) ;
#50269 = CARTESIAN_POINT ( 'NONE',  ( 2.646287650837769956, 1525.055427061254704, 176.5934666753861677 ) ) ;
#50270 = CARTESIAN_POINT ( 'NONE',  ( -7.545095448910339897, 1384.908268029229930, 219.0876225167260145 ) ) ;
#50271 = CARTESIAN_POINT ( 'NONE',  ( -11.40295414052340028, 1470.727202249070160, 209.2846016133759974 ) ) ;
#50272 = CARTESIAN_POINT ( 'NONE',  ( -4.849196095585594612, 1508.218303878354391, 220.4640527089468662 ) ) ;
#50273 = CARTESIAN_POINT ( 'NONE',  ( -17.68237282055029880, 1522.051704408389924, 205.6847408665509818 ) ) ;
#50275 = EDGE_CURVE ( 'NONE', #74400, #76524, #71700, .T. ) ;
#50274 = CARTESIAN_POINT ( 'NONE',  ( 18.24476709642540584, 1425.305388862659356, 224.8416608642366725 ) ) ;
#50276 = CARTESIAN_POINT ( 'NONE',  ( -2.482344662330000062, 1440.444625599219989, 150.5580151863979950 ) ) ;
#50277 = CARTESIAN_POINT ( 'NONE',  ( 27.74152896581870209, 1446.393007474679962, 137.1637341980689939 ) ) ;
#50279 = CARTESIAN_POINT ( 'NONE',  ( -17.14943674877569890, 1460.897686246159992, 228.2718295297070199 ) ) ;
#50278 = CARTESIAN_POINT ( 'NONE',  ( -4.558402699344750175, 1421.324977942919986, 193.7899644519529829 ) ) ;
#50280 = CARTESIAN_POINT ( 'NONE',  ( 12.86077854309999857, 1416.823634022829992, 221.8629616260980129 ) ) ;
#50281 = ORIENTED_EDGE ( 'NONE', *, *, #7636, .F. ) ;
#50282 = EDGE_CURVE ( 'NONE', #55064, #79230, #8764, .T. ) ;
#50283 = ORIENTED_EDGE ( 'NONE', *, *, #72947, .F. ) ;
#50284 = DIRECTION ( 'NONE',  ( -0.9455185755993178454, 0.000000000000000000, 0.3255681544571537578 ) ) ;
#50285 = EDGE_CURVE ( 'NONE', #57273, #35617, #32866, .T. ) ;
#50286 = CARTESIAN_POINT ( 'NONE',  ( -5.243297302279999350, 1438.659032880589848, 207.2722467018089958 ) ) ;
#50287 = CARTESIAN_POINT ( 'NONE',  ( -28.23788176520000093, 1509.669894704329863, 211.0744985972580139 ) ) ;
#50288 = CARTESIAN_POINT ( 'NONE',  ( 2.410646146274223245, 1410.375392720130321, 185.5500677950892623 ) ) ;
#50289 = CARTESIAN_POINT ( 'NONE',  ( 17.02668221408760019, 1422.112876149069962, 226.8213126862850118 ) ) ;
#50290 = CIRCLE ( 'NONE', #48455, 32.13701971169416538 ) ;
#50291 = DIRECTION ( 'NONE',  ( -0.03489949670254138131, 0.9993908270190944299, 0.000000000000000000 ) ) ;
#50292 = EDGE_CURVE ( 'NONE', #53580, #3936, #100018, .T. ) ;
#50293 = CARTESIAN_POINT ( 'NONE',  ( -3.736170183908800180, 1487.848895934140046, 219.5114665497349904 ) ) ;
#50294 = CARTESIAN_POINT ( 'NONE',  ( -4.287909922120000772, 1515.369373403189911, 208.3886085559139758 ) ) ;
#50295 = CARTESIAN_POINT ( 'NONE',  ( -75.11158180925109207, 1383.780721093889952, 299.9085192912519915 ) ) ;
#50296 = CARTESIAN_POINT ( 'NONE',  ( 3.636730251570000405, 1451.537370930130010, 154.1168901888979974 ) ) ;
#50297 = CARTESIAN_POINT ( 'NONE',  ( 10.21500163810000039, 1470.289493831289747, 209.7507578853689836 ) ) ;
#50299 = TOROIDAL_SURFACE ( 'NONE', #2029, 32.13701971169416538, 1.000000000000000000 ) ;
#50298 = CARTESIAN_POINT ( 'NONE',  ( 11.22342845537009914, 1492.268138787170074, 211.5860973086979868 ) ) ;
#50301 = ORIENTED_EDGE ( 'NONE', *, *, #80887, .T. ) ;
#50300 = CARTESIAN_POINT ( 'NONE',  ( 1.217071433320000118, 1456.474392760389946, 219.2743944847990178 ) ) ;
#50302 = DIRECTION ( 'NONE',  ( 0.9993902469235412811, 0.03489947644508400310, -0.001077449749359510062 ) ) ;
#50303 = CARTESIAN_POINT ( 'NONE',  ( -39.07702096660000279, 1382.326711360479976, 238.9772120006589944 ) ) ;
#50304 = CARTESIAN_POINT ( 'NONE',  ( 19.78127211569570321, 1508.034666168520062, 229.2988164385099878 ) ) ;
#50305 = ORIENTED_EDGE ( 'NONE', *, *, #63312, .F. ) ;
#50306 = EDGE_LOOP ( 'NONE', ( #90619, #30335, #81189, #42136 ) ) ;
#50307 = CARTESIAN_POINT ( 'NONE',  ( -9.102552902454579709, 1386.249080320570101, 218.4336176387340061 ) ) ;
#50308 = CARTESIAN_POINT ( 'NONE',  ( 38.23937796074390860, 1438.847880936179990, 136.6258318260159967 ) ) ;
#50310 = DIRECTION ( 'NONE',  ( -1.755985294532469921E-16, 1.000000000000000000, -1.338183447452831989E-16 ) ) ;
#50309 = DIRECTION ( 'NONE',  ( -0.02616798426619638615, 0.9993150019883495494, -0.02616798426453459045 ) ) ;
#50311 = ADVANCED_FACE ( 'NONE', ( #25559 ), #42945, .T. ) ;
#50312 = CARTESIAN_POINT ( 'NONE',  ( -8.550067366969999583, 1462.070379093089969, 204.3084576837289887 ) ) ;
#50313 = CARTESIAN_POINT ( 'NONE',  ( -107.8363875370000073, 1380.933530015289989, 298.5630966836590119 ) ) ;
#50314 = CARTESIAN_POINT ( 'NONE',  ( 2.237652899700000031, 1444.342138342490216, 203.2451014604889963 ) ) ;
#50315 = VECTOR ( 'NONE', #41999, 1000.000000000000000 ) ;
#50316 = CARTESIAN_POINT ( 'NONE',  ( -12.84158769360459651, 1435.935367691730562, 150.8118236764398716 ) ) ;
#50317 = CARTESIAN_POINT ( 'NONE',  ( -3.482404828285579956, 1485.996524617339901, 182.2044860649310181 ) ) ;
#50318 = CYLINDRICAL_SURFACE ( 'NONE', #59348, 2.000000000000003553 ) ;
#50319 = CARTESIAN_POINT ( 'NONE',  ( 3.015183704140000032, 1410.395849601029795, 185.7217229209980189 ) ) ;
#50320 = CARTESIAN_POINT ( 'NONE',  ( 2.335054519268260353, 1486.771262222820042, 197.4158623816819897 ) ) ;
#50321 = ADVANCED_FACE ( 'NONE', ( #41830 ), #46668, .T. ) ;
#50322 = CARTESIAN_POINT ( 'NONE',  ( 3.373264501941120042, 1432.691143165750191, 201.1530439168859914 ) ) ;
#50323 = CARTESIAN_POINT ( 'NONE',  ( 11.86593337849999941, 1432.333320123749900, 150.3971781299979966 ) ) ;
#50324 = CARTESIAN_POINT ( 'NONE',  ( 11.74015299229400000, 1428.979986577520094, 144.1937996693850152 ) ) ;
#50325 = ORIENTED_EDGE ( 'NONE', *, *, #11795, .T. ) ;
#50326 = ADVANCED_FACE ( 'NONE', ( #33975 ), #100261, .T. ) ;
#50327 = CARTESIAN_POINT ( 'NONE',  ( -19.78154490129999843, 1468.390536983390120, 204.4459624408089837 ) ) ;
#50328 = CARTESIAN_POINT ( 'NONE',  ( 4.304798037349998904E-15, 1432.353341358199941, 150.3995506339979897 ) ) ;
#50329 = CARTESIAN_POINT ( 'NONE',  ( -2.370970874524634286, 1427.002265528474027, 134.0999999980980135 ) ) ;
#50330 = CARTESIAN_POINT ( 'NONE',  ( 17.38693183890000071, 1507.629775627629897, 188.3940375129979827 ) ) ;
#50331 = AXIS2_PLACEMENT_3D ( 'NONE', #93196, #57967, #74767 ) ;
#50332 = CARTESIAN_POINT ( 'NONE',  ( -9.458129699028839708E-09, 1472.949333146100116, 261.1319930289780018 ) ) ;
#50333 = CARTESIAN_POINT ( 'NONE',  ( 9.146299198640271300, 1461.861878385089767, 205.8341600298289791 ) ) ;
#50334 = CARTESIAN_POINT ( 'NONE',  ( -0.5679639878839999323, 1416.568813547830132, 227.7576290933980090 ) ) ;
#50335 = CARTESIAN_POINT ( 'NONE',  ( 0.1511760582950009979, 1477.260385247390104, 198.7062178346990038 ) ) ;
#50336 = CARTESIAN_POINT ( 'NONE',  ( -107.2920023509999936, 1387.482252157660241, 310.2753093912590430 ) ) ;
#50337 = VECTOR ( 'NONE', #5634, 1000.000000000000000 ) ;
#50338 = CARTESIAN_POINT ( 'NONE',  ( -0.2120479655457991053, 1485.995122961834340, 181.8315243526895983 ) ) ;
#50339 = CARTESIAN_POINT ( 'NONE',  ( -11.26379070871446331, 1362.773408316262476, 208.3718459617010978 ) ) ;
#50340 = CARTESIAN_POINT ( 'NONE',  ( -45.65239911430659703, 1439.849390212310027, 266.1890414226530197 ) ) ;
#50341 = CARTESIAN_POINT ( 'NONE',  ( -3.087788399999999989, 1439.686999668429962, 185.1123624746980170 ) ) ;
#50342 = CARTESIAN_POINT ( 'NONE',  ( -7.968780129149999780, 1425.481181651620091, 207.4285999761289929 ) ) ;
#50343 = CARTESIAN_POINT ( 'NONE',  ( -3.267039729984999585, 1517.012231669750008, 208.3862772893259887 ) ) ;
#50344 = CARTESIAN_POINT ( 'NONE',  ( -2.478556036580000121, 1437.233840397999984, 157.6736397610980021 ) ) ;
#50345 = CARTESIAN_POINT ( 'NONE',  ( 19.26968731915079047, 1456.385665059119447, 224.8316692866741562 ) ) ;
#50346 = CARTESIAN_POINT ( 'NONE',  ( 7.263451787643480095, 1426.472202734280017, 212.8712549859859848 ) ) ;
#50347 = VECTOR ( 'NONE', #13757, 1000.000000000000000 ) ;
#50348 = CARTESIAN_POINT ( 'NONE',  ( -26.66940587972800003, 1451.815323532959837, 135.6567935292860057 ) ) ;
#50349 = EDGE_LOOP ( 'NONE', ( #99468, #63416 ) ) ;
#50350 = CARTESIAN_POINT ( 'NONE',  ( 29.87497007670000215, 1438.990456222089961, 238.0574376903979896 ) ) ;
#50352 = CARTESIAN_POINT ( 'NONE',  ( -17.06592007889999962, 1409.674274294630095, 194.3954626038980109 ) ) ;
#50351 = CARTESIAN_POINT ( 'NONE',  ( -2.471035510942674485, 1525.556090473913855, 176.9933286210197423 ) ) ;
#50353 = CARTESIAN_POINT ( 'NONE',  ( -2.644608989403160137, 1419.519946857050172, 186.1458476411769993 ) ) ;
#50354 = CARTESIAN_POINT ( 'NONE',  ( -16.45840115875039800, 1508.541818857670023, 213.5626919147919978 ) ) ;
#50355 = CARTESIAN_POINT ( 'NONE',  ( -10.37096375755954192, 1396.275222422115121, 217.1218459616979999 ) ) ;
#50356 = CARTESIAN_POINT ( 'NONE',  ( -33.93019615848960768, 1512.187213306747481, 197.6607374646001176 ) ) ;
#50357 = CARTESIAN_POINT ( 'NONE',  ( -34.18677586421195969, 1512.187213306747481, 198.4504086008750505 ) ) ;
#50358 = ORIENTED_EDGE ( 'NONE', *, *, #26227, .T. ) ;
#50359 = CARTESIAN_POINT ( 'NONE',  ( -0.5945626521397818776, 1410.034456817089904, 269.8654418808179685 ) ) ;
#50360 = CARTESIAN_POINT ( 'NONE',  ( 17.02686444325469850, 1422.113038003860083, 226.8212050067879773 ) ) ;
#50361 = CARTESIAN_POINT ( 'NONE',  ( 8.090998277665431004, 1435.786064241179929, 206.2615718783590069 ) ) ;
#50362 = ORIENTED_EDGE ( 'NONE', *, *, #85403, .T. ) ;
#50363 = ORIENTED_EDGE ( 'NONE', *, *, #956, .F. ) ;
#50364 = CARTESIAN_POINT ( 'NONE',  ( -23.33367609749780414, 1409.843005415879816, 208.9560767717839838 ) ) ;
#50365 = EDGE_LOOP ( 'NONE', ( #9274, #74291, #11513, #73827 ) ) ;
#50366 = CARTESIAN_POINT ( 'NONE',  ( 16.18975884877226790, 1409.478419224255049, 223.4272596155709039 ) ) ;
#50367 = CARTESIAN_POINT ( 'NONE',  ( -41.79795361626952399, 1426.458837659412211, 266.3001450109010193 ) ) ;
#50368 = CARTESIAN_POINT ( 'NONE',  ( -3.369548796489999720, 1498.349935238530179, 236.3379732119980190 ) ) ;
#50369 = CARTESIAN_POINT ( 'NONE',  ( -22.03715318569999937, 1410.866002606429902, 214.8824533464280080 ) ) ;
#50370 = CARTESIAN_POINT ( 'NONE',  ( 45.76102518337949476, 1443.713172479500145, 266.4159216563020323 ) ) ;
#50371 = DIRECTION ( 'NONE',  ( 0.7882878497004317531, 0.000000000000000000, 0.6153066438895888890 ) ) ;
#50372 = CARTESIAN_POINT ( 'NONE',  ( -16.44336187847212827, 1421.265292702081524, 226.9958026168290246 ) ) ;
#50373 = CARTESIAN_POINT ( 'NONE',  ( 7.711550677984999602, 1516.630499592039996, 205.0863552195469879 ) ) ;
#50374 = EDGE_LOOP ( 'NONE', ( #106238, #5018, #109271, #45808 ) ) ;
#50375 = CARTESIAN_POINT ( 'NONE',  ( 19.00753814766553518, 1457.296012680650620, 226.5174060896799233 ) ) ;
#50376 = CARTESIAN_POINT ( 'NONE',  ( 15.24308028946400029, 1512.436270050410030, 196.0367649543779862 ) ) ;
#50377 = DIRECTION ( 'NONE',  ( -5.980589973904019347E-17, 1.000000000000000000, -1.736889445713099699E-16 ) ) ;
#50378 = ORIENTED_EDGE ( 'NONE', *, *, #80868, .F. ) ;
#50379 = FACE_OUTER_BOUND ( 'NONE', #59837, .T. ) ;
#50380 = CARTESIAN_POINT ( 'NONE',  ( 26.87482465513500074, 1451.958209271989972, 135.1663978525000118 ) ) ;
#50381 = CARTESIAN_POINT ( 'NONE',  ( -14.97085961631660034, 1514.147575501539905, 194.3487857625829918 ) ) ;
#50382 = CARTESIAN_POINT ( 'NONE',  ( 8.642986837300808745, 1452.611240636269940, 151.1117272551699955 ) ) ;
#50383 = CARTESIAN_POINT ( 'NONE',  ( 7.516769032520000060, 1422.170349638209927, 195.6959265412990021 ) ) ;
#50384 = CARTESIAN_POINT ( 'NONE',  ( -4.134291178206661144, 1425.982862007858557, 186.1112856665070865 ) ) ;
#50385 = CARTESIAN_POINT ( 'NONE',  ( 11.05853588759599937, 1478.760309791250165, 205.9079366425139881 ) ) ;
#50386 = CARTESIAN_POINT ( 'NONE',  ( 1.776918358778360130, 1408.975111743729940, 186.8671107929409914 ) ) ;
#50388 = CARTESIAN_POINT ( 'NONE',  ( 4.038582018629999659, 1515.598601288590089, 209.1218459616989946 ) ) ;
#50387 = CARTESIAN_POINT ( 'NONE',  ( 30.51923195337197114, 1524.059547553518769, 196.3739828646224055 ) ) ;
#50389 = CARTESIAN_POINT ( 'NONE',  ( -4.026786250540000722, 1418.913060387330006, 172.2701767054979882 ) ) ;
#50390 = CIRCLE ( 'NONE', #77161, 1.999999999999999556 ) ;
#50391 = CARTESIAN_POINT ( 'NONE',  ( -12.11621817370000009, 1378.266527857250139, 211.6883570098989935 ) ) ;
#50392 = CARTESIAN_POINT ( 'NONE',  ( 2.865544263339262265, 1525.651286436460623, 241.1072443789812496 ) ) ;
#50393 = VERTEX_POINT ( 'NONE', #33409 ) ;
#50394 = CARTESIAN_POINT ( 'NONE',  ( 12.93261306534300026, 1416.826860677879949, 221.7400780573829877 ) ) ;
#50395 = CARTESIAN_POINT ( 'NONE',  ( 11.24996440847739976, 1432.343753997600061, 151.5214208984010043 ) ) ;
#50396 = CARTESIAN_POINT ( 'NONE',  ( -10.71760456835239950, 1483.213272081000014, 203.9247400436699991 ) ) ;
#50397 = CARTESIAN_POINT ( 'NONE',  ( -12.77874876509999957, 1390.744078294579822, 206.9966459296790049 ) ) ;
#50398 = CARTESIAN_POINT ( 'NONE',  ( 8.482184659042799169, 1423.325493229070162, 211.9867658860320034 ) ) ;
#50399 =( BOUNDED_CURVE ( )  B_SPLINE_CURVE ( 3, ( #42853, #59661, #42292, #100536 ),
 .UNSPECIFIED., .F., .F. ) 
 B_SPLINE_CURVE_WITH_KNOTS ( ( 4, 4 ),
 ( 4.712388980384689674, 6.283185307179586232 ),
 .UNSPECIFIED. ) 
 CURVE ( )  GEOMETRIC_REPRESENTATION_ITEM ( )  RATIONAL_B_SPLINE_CURVE ( ( 1.000000000000000000, 0.8047378541243649375, 0.8047378541243649375, 1.000000000000000000 ) ) 
 REPRESENTATION_ITEM ( '' )  );
#50400 = CARTESIAN_POINT ( 'NONE',  ( 11.52796152851120048, 1425.560458258250264, 202.9256552550970127 ) ) ;
#50401 = CARTESIAN_POINT ( 'NONE',  ( -11.00543052331669891, 1462.571841119889996, 208.1677703206260048 ) ) ;
#50402 = CIRCLE ( 'NONE', #16379, 23.69926344187880929 ) ;
#50403 = EDGE_CURVE ( 'NONE', #76210, #22976, #51996, .T. ) ;
#50404 = CARTESIAN_POINT ( 'NONE',  ( -18.93537658710000215, 1468.059964608330120, 268.3665355204980187 ) ) ;
#50405 = CARTESIAN_POINT ( 'NONE',  ( -8.883323636877099361, 1384.529732085800106, 218.6638821885779862 ) ) ;
#50407 = EDGE_CURVE ( 'NONE', #94948, #38397, #66329, .T. ) ;
#50406 = CARTESIAN_POINT ( 'NONE',  ( 11.68281581620000154, 1433.662110734889893, 151.0231821035980033 ) ) ;
#50408 = CARTESIAN_POINT ( 'NONE',  ( 11.47403709489999990, 1467.186912539730201, 262.6648722463980334 ) ) ;
#50409 = CARTESIAN_POINT ( 'NONE',  ( 12.30902781860649853, 1415.426561690380140, 196.6799914669740019 ) ) ;
#50410 = CARTESIAN_POINT ( 'NONE',  ( -17.51543113656909867, 1417.552258021759826, 206.7803033077899784 ) ) ;
#50411 = CARTESIAN_POINT ( 'NONE',  ( 9.043577616344240511, 1419.744760940520109, 194.5516119844990044 ) ) ;
#50412 = CARTESIAN_POINT ( 'NONE',  ( 6.494921822917000043, 1465.840553322820142, 216.8173835122059927 ) ) ;
#50413 = CARTESIAN_POINT ( 'NONE',  ( -15.76003452500000179, 1486.230153518429915, 186.5609880657980284 ) ) ;
#50414 = CARTESIAN_POINT ( 'NONE',  ( 11.86363518809157647, 1398.264811432181887, 214.4375779453321513 ) ) ;
#50415 = CARTESIAN_POINT ( 'NONE',  ( -17.85347883109999856, 1410.900113656230133, 225.0193030873980149 ) ) ;
#50416 = AXIS2_PLACEMENT_3D ( 'NONE', #4148, #5797, #32085 ) ;
#50417 = CARTESIAN_POINT ( 'NONE',  ( -8.110034436179123674, 1425.494577458902768, 208.5273439571141409 ) ) ;
#50418 = DIRECTION ( 'NONE',  ( 0.4978433412588673113, 0.000000000000000000, -0.8672669759446667292 ) ) ;
#50419 = LINE ( 'NONE', #83993, #32564 ) ;
#50420 = CARTESIAN_POINT ( 'NONE',  ( -15.13920057018590093, 1383.858439105669959, 219.2872454811189868 ) ) ;
#50421 = CARTESIAN_POINT ( 'NONE',  ( 12.71867950848070095, 1426.806024775080004, 204.8922107218619999 ) ) ;
#50422 = DIRECTION ( 'NONE',  ( 0.7414773880254711402, -0.000000000000000000, 0.6709778558543678662 ) ) ;
#50423 = B_SPLINE_CURVE_WITH_KNOTS ( 'NONE', 3,
 ( #37915, #12700, #77301, #1704, #1152, #98355, #69468, #599, #72096, #103019, #26315, #94630, #106211, #17905, #35844, #103586, #26888, #55282, #61078, #46884, #38445, #70029, #106751, #19007, #104142, #27427, #61610, #30039, #98901, #74283, #107856, #101091, #89954, #56369, #82102, #22718, #56919, #41211, #38989, #99441, #92160, #32796, #57484, #91050, #65878, #109520, #49625, #14336, #24390 ),
 .UNSPECIFIED., .F., .F.,
 ( 4, 3, 3, 3, 3, 3, 3, 3, 3, 3, 3, 3, 3, 3, 3, 3, 4 ),
 ( 0.000000000000000000, 1.367534301173350064, 2.791361796389739691, 4.169044824514560155, 5.615944553276730034, 7.062844282038899912, 8.459574530849598872, 9.876103170593360403, 11.24898385078170016, 12.61392778173159890, 13.96829556498239988, 14.12568908982460059, 14.94249011817409922, 15.71017679274670087, 16.35253358467650031, 16.91884759190949694, 17.37853207929999755 ),
 .UNSPECIFIED. ) ;
#50425 = AXIS2_PLACEMENT_3D ( 'NONE', #57653, #16148, #73886 ) ;
#50424 = CARTESIAN_POINT ( 'NONE',  ( -17.63599094636219888, 1419.790072980149944, 206.1021312808440200 ) ) ;
#50426 = CARTESIAN_POINT ( 'NONE',  ( 0.1733418428536109834, 1478.369830831500167, 182.1644135495710088 ) ) ;
#50428 = EDGE_LOOP ( 'NONE', ( #82547, #13193 ) ) ;
#50427 = DIRECTION ( 'NONE',  ( 0.000000000000000000, 0.7071067811865475727, 0.7071067811865475727 ) ) ;
#50429 = CARTESIAN_POINT ( 'NONE',  ( -20.77846844200000120, 1444.740067931809790, 176.2781434906979996 ) ) ;
#50430 = CARTESIAN_POINT ( 'NONE',  ( 0.000000000000000000, 1526.382868172863937, 209.1218459616979999 ) ) ;
#50431 = DIRECTION ( 'NONE',  ( 0.000000000000000000, -1.000000000000000000, 0.000000000000000000 ) ) ;
#50432 = CARTESIAN_POINT ( 'NONE',  ( -40.01221335562710379, 1438.828034966029918, 134.0999999981109738 ) ) ;
#50433 = CARTESIAN_POINT ( 'NONE',  ( -109.1646014829999984, 1384.895722584660007, 297.1326616210590146 ) ) ;
#50434 = EDGE_LOOP ( 'NONE', ( #102637, #3330, #14895, #68124 ) ) ;
#50435 = DIRECTION ( 'NONE',  ( 1.000000000000000000, 0.000000000000000000, 0.000000000000000000 ) ) ;
#50436 = CARTESIAN_POINT ( 'NONE',  ( 3.348647037815641436, 1523.530870145310701, 176.1572109406605193 ) ) ;
#50437 = CARTESIAN_POINT ( 'NONE',  ( -103.5985846424588601, 1379.901892699559312, 304.5993904023399068 ) ) ;
#50438 = CARTESIAN_POINT ( 'NONE',  ( 17.12499568933700189, 1499.118982824430077, 222.9618237066810025 ) ) ;
#50439 = CARTESIAN_POINT ( 'NONE',  ( -8.200787980966151025, 1436.145857994200242, 211.9570384925519875 ) ) ;
#50440 = DIRECTION ( 'NONE',  ( -0.000000000000000000, 1.000000000000000000, -0.000000000000000000 ) ) ;
#50441 = CARTESIAN_POINT ( 'NONE',  ( -4.145978979534980458E-15, 1375.413060387289988, 209.1218459572589836 ) ) ;
#50442 = CARTESIAN_POINT ( 'NONE',  ( 7.369537115729440480, 1409.170410294239900, 222.1470682314269993 ) ) ;
#50443 = DIRECTION ( 'NONE',  ( 0.000000000000000000, 0.000000000000000000, 1.000000000000000000 ) ) ;
#50444 = CARTESIAN_POINT ( 'NONE',  ( -84.36119002024280178, 1385.173936778570123, 288.1322194500510250 ) ) ;
#50445 = EDGE_CURVE ( 'NONE', #53780, #1895, #89475, .T. ) ;
#50446 = CARTESIAN_POINT ( 'NONE',  ( -10.88252683822419975, 1391.913060387289988, 212.7915775323999981 ) ) ;
#50447 = CARTESIAN_POINT ( 'NONE',  ( 11.63682296995209953, 1421.992969092299973, 209.6317927274760109 ) ) ;
#50448 = LINE ( 'NONE', #100809, #46819 ) ;
#50449 = CARTESIAN_POINT ( 'NONE',  ( -15.73561791997630088, 1409.462558364120014, 225.3904801341000166 ) ) ;
#50451 = ORIENTED_EDGE ( 'NONE', *, *, #78695, .T. ) ;
#50450 = FACE_BOUND ( 'NONE', #103632, .T. ) ;
#50452 = CARTESIAN_POINT ( 'NONE',  ( 2.227690093140000105, 1473.333206620189912, 219.1070348612290104 ) ) ;
#50453 = EDGE_CURVE ( 'NONE', #12155, #87976, #59121, .T. ) ;
#50454 = CARTESIAN_POINT ( 'NONE',  ( -20.71343476517554905, 1522.382868172863937, 179.9059455038197086 ) ) ;
#50455 = CARTESIAN_POINT ( 'NONE',  ( -8.622403150232841540, 1362.632156860344139, 210.6218459616987957 ) ) ;
#50456 = CARTESIAN_POINT ( 'NONE',  ( -10.20231950299999824, 1492.893084484690235, 203.6441250547690061 ) ) ;
#50457 = CARTESIAN_POINT ( 'NONE',  ( 41.27403068698424704, 1446.758019147874620, 269.6337390305045005 ) ) ;
#50458 = DIRECTION ( 'NONE',  ( 0.000000000000000000, 0.000000000000000000, 1.000000000000000000 ) ) ;
#50459 = CARTESIAN_POINT ( 'NONE',  ( 18.39211149378427379, 1435.897264093365948, 214.5601621755202757 ) ) ;
#50460 = CARTESIAN_POINT ( 'NONE',  ( 1.552710838619999922, 1417.100030409630108, 233.1250354766980024 ) ) ;
#50461 = CARTESIAN_POINT ( 'NONE',  ( -2.862715468142697617, 1516.551704408386058, 201.3093830337851387 ) ) ;
#50462 = CARTESIAN_POINT ( 'NONE',  ( -21.57334207099999901, 1507.349712068389863, 210.4840098404890227 ) ) ;
#50463 = CARTESIAN_POINT ( 'NONE',  ( 6.531167973260561865, 1517.051704408389924, 201.5366623270788295 ) ) ;
#50464 = CARTESIAN_POINT ( 'NONE',  ( -3.021161635200000362, 1455.772982809590076, 200.1537592901690061 ) ) ;
#50465 = CARTESIAN_POINT ( 'NONE',  ( 2.284199363404999961, 1516.940296199220029, 205.8526610237369994 ) ) ;
#50466 = CARTESIAN_POINT ( 'NONE',  ( 2.500000000000000000, 1448.210448412299911, 170.5244215879980061 ) ) ;
#50467 = ORIENTED_EDGE ( 'NONE', *, *, #33938, .F. ) ;
#50468 = CARTESIAN_POINT ( 'NONE',  ( 32.28466283162151029, 1522.382868172863937, 199.0684425896244250 ) ) ;
#50469 = CARTESIAN_POINT ( 'NONE',  ( 32.44714059009999829, 1466.431271693930057, 269.3248281139979667 ) ) ;
#50471 = VERTEX_POINT ( 'NONE', #106155 ) ;
#50470 = CARTESIAN_POINT ( 'NONE',  ( -68.58336172453009283, 1379.747483509290078, 280.1906536643289769 ) ) ;
#50472 = CARTESIAN_POINT ( 'NONE',  ( -17.53307272543440121, 1417.831573838860095, 206.8262974944190091 ) ) ;
#50473 = ORIENTED_EDGE ( 'NONE', *, *, #3285, .F. ) ;
#50474 = CARTESIAN_POINT ( 'NONE',  ( -16.25130726159467542, 1514.566425925963586, 223.9165014063416379 ) ) ;
#50475 = CARTESIAN_POINT ( 'NONE',  ( -23.51192877400000114, 1410.913812961229951, 206.4143556372079615 ) ) ;
#50477 = CARTESIAN_POINT ( 'NONE',  ( 15.80609125907960255, 1409.490806506669969, 192.6604916703820152 ) ) ;
#50476 = CARTESIAN_POINT ( 'NONE',  ( -11.16073650870000122, 1426.886991639529924, 102.3049941106980043 ) ) ;
#50478 = CARTESIAN_POINT ( 'NONE',  ( -3.445201526505000000, 1516.743010792419909, 210.8372070624770060 ) ) ;
#50479 = CARTESIAN_POINT ( 'NONE',  ( 36.86583086841639556, 1437.713619129489871, 136.5403217841159744 ) ) ;
#50480 = VECTOR ( 'NONE', #75493, 1000.000000000000000 ) ;
#50481 = DIRECTION ( 'NONE',  ( 0.4436356471204865315, 1.250495761681361773E-32, 0.8962072375315807138 ) ) ;
#50482 = CARTESIAN_POINT ( 'NONE',  ( -39.71667698230000099, 1438.440173584909871, 259.0958797427979903 ) ) ;
#50483 = CARTESIAN_POINT ( 'NONE',  ( -0.1339064907639219981, 1508.974573961829947, 179.3682901727229932 ) ) ;
#50484 = CARTESIAN_POINT ( 'NONE',  ( 12.60056023386209922, 1500.993407397960027, 210.8144105449839856 ) ) ;
#50485 = CONTEXT_DEPENDENT_SHAPE_REPRESENTATION ( #62815, #4437 ) ;
#50486 = CARTESIAN_POINT ( 'NONE',  ( 38.54572101799519857, 1450.058425145439969, 134.0999999982749955 ) ) ;
#50487 = CARTESIAN_POINT ( 'NONE',  ( -39.17232000345539689, 1439.963336824750058, 136.7246149087999925 ) ) ;
#50488 = ORIENTED_EDGE ( 'NONE', *, *, #23300, .F. ) ;
#50489 = DIRECTION ( 'NONE',  ( 0.000000000000000000, 1.000000000000000000, 0.000000000000000000 ) ) ;
#50490 = DIRECTION ( 'NONE',  ( 0.9455185755993178454, 0.000000000000000000, -0.3255681544571539243 ) ) ;
#50491 = ORIENTED_EDGE ( 'NONE', *, *, #7663, .F. ) ;
#50492 = VERTEX_POINT ( 'NONE', #11548 ) ;
#50493 = CARTESIAN_POINT ( 'NONE',  ( -1.413982343730000091, 1425.233086417520099, 191.1415897097990069 ) ) ;
#50494 = CARTESIAN_POINT ( 'NONE',  ( 17.83486663330506872, 1523.678648413191695, 237.8759530894958800 ) ) ;
#50495 = CARTESIAN_POINT ( 'NONE',  ( -14.13953454557050016, 1379.986141950590081, 211.1479330773270249 ) ) ;
#50496 = CARTESIAN_POINT ( 'NONE',  ( -13.02765491641741846, 1417.056304985424049, 200.8910991843737008 ) ) ;
#50498 = CARTESIAN_POINT ( 'NONE',  ( 4.287909922120000772, 1515.369373403189911, 209.8550833674839851 ) ) ;
#50497 = AXIS2_PLACEMENT_3D ( 'NONE', #101039, #8091, #92649 ) ;
#50499 = CARTESIAN_POINT ( 'NONE',  ( -6.272372246000269769, 1454.211692497139893, 202.1362065909700050 ) ) ;
#50500 = CARTESIAN_POINT ( 'NONE',  ( -15.10371725490000117, 1409.440493816029857, 225.2902966875980155 ) ) ;
#50501 = CARTESIAN_POINT ( 'NONE',  ( -19.71644462915288187, 1485.715905243316456, 215.2741460507342310 ) ) ;
#50502 = CARTESIAN_POINT ( 'NONE',  ( 30.11977250498251379, 1524.538768545234007, 222.3783518056995945 ) ) ;
#50503 = CARTESIAN_POINT ( 'NONE',  ( -12.41968314810000074, 1391.384630209019861, 211.0556431170890050 ) ) ;
#50504 = CARTESIAN_POINT ( 'NONE',  ( -89.28715904204869958, 1384.835856820089930, 292.1171647776239979 ) ) ;
#50505 = VERTEX_POINT ( 'NONE', #71497 ) ;
#50506 = CARTESIAN_POINT ( 'NONE',  ( 0.7396922377450010355, 1517.135701590510052, 201.7845486201169933 ) ) ;
#50507 = CARTESIAN_POINT ( 'NONE',  ( 5.011551368014999674, 1517.080322339569875, 209.8587501411369942 ) ) ;
#50508 = VERTEX_POINT ( 'NONE', #70380 ) ;
#50509 = CARTESIAN_POINT ( 'NONE',  ( 11.80796784730199889, 1428.630476879899788, 148.5709776132119657 ) ) ;
#50510 = CARTESIAN_POINT ( 'NONE',  ( 3.836782192165181904, 1511.512562116162371, 217.2653043727980560 ) ) ;
#50511 = EDGE_LOOP ( 'NONE', ( #27466, #80734, #60864, #95726 ) ) ;
#50512 = CARTESIAN_POINT ( 'NONE',  ( 14.59277107062129986, 1436.244837967300100, 149.8707660814949918 ) ) ;
#50513 = CARTESIAN_POINT ( 'NONE',  ( -16.68498601116327151, 1442.773887286369018, 162.0933193695679222 ) ) ;
#50514 = CARTESIAN_POINT ( 'NONE',  ( -4.170038484254391165, 1432.161950885697252, 216.4833537471189402 ) ) ;
#50515 = CARTESIAN_POINT ( 'NONE',  ( -10.57410958284499891, 1462.298602691789938, 208.7181287738039828 ) ) ;
#50516 = CARTESIAN_POINT ( 'NONE',  ( 21.24774881647060099, 1409.658413723660033, 206.3980491481210038 ) ) ;
#50517 = CARTESIAN_POINT ( 'NONE',  ( 10.12605604320560104, 1469.432876218259935, 207.3487825585040127 ) ) ;
#50518 = CARTESIAN_POINT ( 'NONE',  ( -9.237108298879999069, 1474.172111518589873, 204.4935998512690105 ) ) ;
#50519 = CARTESIAN_POINT ( 'NONE',  ( -9.123972348892126050, 1410.606870705112215, 188.1126544915522913 ) ) ;
#50520 = CARTESIAN_POINT ( 'NONE',  ( -58.01117002480000195, 1379.721643371590289, 257.2111322587590507 ) ) ;
#50521 = CARTESIAN_POINT ( 'NONE',  ( -15.43453510460000011, 1462.585142083830078, 223.2687737027980006 ) ) ;
#50523 = CARTESIAN_POINT ( 'NONE',  ( 8.543286749999769114, 1468.346214803730163, 201.8597651585060078 ) ) ;
#50522 = CARTESIAN_POINT ( 'NONE',  ( -20.64498752849999974, 1505.794066315190094, 209.1536330714720009 ) ) ;
#50524 = DIRECTION ( 'NONE',  ( 0.1677289028140550031, 0.3720281548064550137, -0.9129414368907229349 ) ) ;
#50525 = CARTESIAN_POINT ( 'NONE',  ( -5.437469379731239449, 1506.424482793976722, 187.8301161205860410 ) ) ;
#50526 = ORIENTED_EDGE ( 'NONE', *, *, #94458, .F. ) ;
#50527 = DIRECTION ( 'NONE',  ( 9.156846217086110244E-47, -1.000000000000000000, 1.836970198721029688E-16 ) ) ;
#50528 = CARTESIAN_POINT ( 'NONE',  ( 0.4290910254045180450, 1516.809856563741278, 216.8380932758135771 ) ) ;
#50529 = CARTESIAN_POINT ( 'NONE',  ( 1.132949076425000090, 1516.693851263360102, 214.1195642086070166 ) ) ;
#50530 = CARTESIAN_POINT ( 'NONE',  ( -2.947166520632872988, 1485.291949360874924, 182.9808020193160587 ) ) ;
#50531 = CARTESIAN_POINT ( 'NONE',  ( -1.766059939614330165, 1483.862676877220110, 198.5882530496979825 ) ) ;
#50533 = ORIENTED_EDGE ( 'NONE', *, *, #9714, .T. ) ;
#50532 = CARTESIAN_POINT ( 'NONE',  ( -11.55143878132009938, 1501.163903211799834, 211.2289541138460152 ) ) ;
#50534 = CARTESIAN_POINT ( 'NONE',  ( 1.331830187880000071, 1453.151875979030137, 188.5601980120979988 ) ) ;
#50535 = CARTESIAN_POINT ( 'NONE',  ( -0.4021349000140009844, 1508.551704408389924, 220.0610460832990043 ) ) ;
#50536 = CARTESIAN_POINT ( 'NONE',  ( -10.91072510809999940, 1428.225676817730118, 150.5333655099979921 ) ) ;
#50537 = DIRECTION ( 'NONE',  ( 0.2302114497549279104, -0.7071067811868634312, 0.6685825965438282337 ) ) ;
#50538 = CYLINDRICAL_SURFACE ( 'NONE', #88496, 26.99999999999999289 ) ;
#50539 = CARTESIAN_POINT ( 'NONE',  ( 4.760896992130000172, 1449.971761959190189, 190.6385172635989704 ) ) ;
#50540 = CARTESIAN_POINT ( 'NONE',  ( 20.49831092009999978, 1496.178973653789853, 204.1013708937389879 ) ) ;
#50541 = CARTESIAN_POINT ( 'NONE',  ( 1.113400974650000208, 1478.239378551490063, 201.5788049939389737 ) ) ;
#50543 = CARTESIAN_POINT ( 'NONE',  ( -10.68990730692100044, 1481.192710571149973, 208.4620442137509997 ) ) ;
#50542 = CARTESIAN_POINT ( 'NONE',  ( -19.52587859339999810, 1470.090240710929947, 227.0208896569980084 ) ) ;
#50544 = CARTESIAN_POINT ( 'NONE',  ( -8.929044350759999915, 1464.245425498190116, 227.2010804325990136 ) ) ;
#50545 = ORIENTED_EDGE ( 'NONE', *, *, #21926, .T. ) ;
#50546 = CARTESIAN_POINT ( 'NONE',  ( -0.01328397755539850039, 1516.939580991450157, 205.8601936452070049 ) ) ;
#50547 = CARTESIAN_POINT ( 'NONE',  ( 26.68674721769999891, 1413.099522324730060, 269.4193621475980081 ) ) ;
#50548 = CARTESIAN_POINT ( 'NONE',  ( 22.89198443360000113, 1435.442148801120084, 140.5684033940979987 ) ) ;
#50549 = CARTESIAN_POINT ( 'NONE',  ( 19.05265570330000102, 1449.733526242509924, 192.0691012804980176 ) ) ;
#50550 = ADVANCED_FACE ( 'NONE', ( #53011 ), #78749, .T. ) ;
#50551 = CARTESIAN_POINT ( 'NONE',  ( 20.01203290568441773, 1426.583398916021451, 221.2898012671467143 ) ) ;
#50552 = CARTESIAN_POINT ( 'NONE',  ( -8.082394523001108055, 1387.362642507876217, 218.5730659734533390 ) ) ;
#50553 = CARTESIAN_POINT ( 'NONE',  ( 11.87823649874709986, 1433.207008023099888, 147.6493504979379736 ) ) ;
#50554 = CARTESIAN_POINT ( 'NONE',  ( 2.500000000000000000, 1439.615672362369878, 176.6480837420980095 ) ) ;
#50555 = CARTESIAN_POINT ( 'NONE',  ( -15.84994825389999740, 1416.551565560330118, 207.9043296938389744 ) ) ;
#50556 = CARTESIAN_POINT ( 'NONE',  ( -13.30879681040000051, 1445.197123204520040, 187.8034403054980146 ) ) ;
#50557 = EDGE_CURVE ( 'NONE', #1077, #103300, #19931, .T. ) ;
#50558 = CARTESIAN_POINT ( 'NONE',  ( -16.66821264700000071, 1497.713060387329961, 224.4060481835979886 ) ) ;
#50559 = CARTESIAN_POINT ( 'NONE',  ( -16.63648012991517433, 1419.612236357899292, 209.0575818519019720 ) ) ;
#50560 = CARTESIAN_POINT ( 'NONE',  ( -4.795131425830000182, 1497.578645253790000, 220.1696405719989968 ) ) ;
#50561 = CARTESIAN_POINT ( 'NONE',  ( 0.1832230673610020233, 1471.246529402990063, 189.0482111049990124 ) ) ;
#50562 = CARTESIAN_POINT ( 'NONE',  ( -18.39258007780000170, 1441.405133176690015, 212.6808529323389791 ) ) ;
#50563 = CARTESIAN_POINT ( 'NONE',  ( -11.65979349303169954, 1507.853111589269929, 207.9005118103889913 ) ) ;
#50564 = CARTESIAN_POINT ( 'NONE',  ( -4.882950377119058771, 1421.798896365259225, 193.0164691839993907 ) ) ;
#50565 = CARTESIAN_POINT ( 'NONE',  ( -12.63400943340000104, 1474.287538769530101, 269.2355652850980050 ) ) ;
#50566 = CARTESIAN_POINT ( 'NONE',  ( -30.30249668296272958, 1524.678872986481338, 196.4365537040479239 ) ) ;
#50567 = CARTESIAN_POINT ( 'NONE',  ( -15.09731539277014001, 1514.821745470009319, 193.1064629479987502 ) ) ;
#50568 = DIRECTION ( 'NONE',  ( 0.8090169943749422332, 0.000000000000000000, -0.5877852522924802425 ) ) ;
#50569 = CARTESIAN_POINT ( 'NONE',  ( -51.99793925633279912, 1384.730550586590198, 265.8323962730830203 ) ) ;
#50570 = CARTESIAN_POINT ( 'NONE',  ( 19.03110457515579768, 1457.047041246000163, 226.1578386336209974 ) ) ;
#50571 = CARTESIAN_POINT ( 'NONE',  ( -5.773159728049999117E-15, 1442.756953654919926, 155.7628527808980152 ) ) ;
#50572 = CARTESIAN_POINT ( 'NONE',  ( -107.4538559780000071, 1379.578066771490057, 299.0810615966589694 ) ) ;
#50573 = CARTESIAN_POINT ( 'NONE',  ( -16.55108609117688445, 1524.760046179776054, 237.4542795853993482 ) ) ;
#50574 = DIRECTION ( 'NONE',  ( -1.000000000000000000, -1.267952440776734034E-09, 6.874604651021009972E-10 ) ) ;
#50575 = CARTESIAN_POINT ( 'NONE',  ( -22.94994330970000362, 1410.635878578629899, 204.6714796687680007 ) ) ;
#50576 = CARTESIAN_POINT ( 'NONE',  ( -9.803547299931144821, 1380.487226564378943, 201.5547637714570328 ) ) ;
#50577 = CARTESIAN_POINT ( 'NONE',  ( 4.722118042039999963, 1485.526134326590181, 218.7852782599590000 ) ) ;
#50578 = CARTESIAN_POINT ( 'NONE',  ( 10.17866008307600012, 1479.588344398260006, 206.0280708825729903 ) ) ;
#50579 = CARTESIAN_POINT ( 'NONE',  ( -18.31485190103290250, 1445.278724020879963, 204.5307765124340165 ) ) ;
#50580 = CARTESIAN_POINT ( 'NONE',  ( -19.31924249874780131, 1445.911422301539915, 199.9640984727790283 ) ) ;
#50581 = CARTESIAN_POINT ( 'NONE',  ( 16.48400364722103362, 1525.790286462515496, 181.7637252794370397 ) ) ;
#50582 = CARTESIAN_POINT ( 'NONE',  ( -16.76045707751869784, 1417.322363310820037, 208.1402530697109796 ) ) ;
#50583 = CARTESIAN_POINT ( 'NONE',  ( 11.70423387253950054, 1426.717280763200051, 141.8225260926249973 ) ) ;
#50584 = CARTESIAN_POINT ( 'NONE',  ( 16.49871591221882738, 1525.320827368860819, 237.0413499740942029 ) ) ;
#50585 = CARTESIAN_POINT ( 'NONE',  ( -10.44087869485973030, 1522.051704408389924, 205.3524051900861593 ) ) ;
#50586 = CARTESIAN_POINT ( 'NONE',  ( 7.722580314274734903, 1517.051704408389924, 211.3043090471990126 ) ) ;
#50587 = CARTESIAN_POINT ( 'NONE',  ( 11.60004869885203860, 1428.965959225140750, 137.0999999980979851 ) ) ;
#50588 = CARTESIAN_POINT ( 'NONE',  ( -1.710004586925000236, 1516.557392317769882, 202.5758445815369839 ) ) ;
#50589 = CARTESIAN_POINT ( 'NONE',  ( -11.73357813035489983, 1488.009932409569956, 191.9067504558449855 ) ) ;
#50590 = CARTESIAN_POINT ( 'NONE',  ( -11.80537760282536119, 1398.263100982790093, 203.6771685272100001 ) ) ;
#50591 = DIRECTION ( 'NONE',  ( 0.4794255386042036160, 0.000000000000000000, 0.8775825618903725367 ) ) ;
#50592 = FACE_BOUND ( 'NONE', #102322, .T. ) ;
#50593 = CARTESIAN_POINT ( 'NONE',  ( -7.463281564165999526, 1379.014324719059914, 211.6703187352700013 ) ) ;
#50594 = CARTESIAN_POINT ( 'NONE',  ( 22.38660642171149817, 1509.694817746930084, 228.2841629394400229 ) ) ;
#50596 = EDGE_LOOP ( 'NONE', ( #7243, #46947, #11187, #43984, #107879 ) ) ;
#50595 = CARTESIAN_POINT ( 'NONE',  ( -40.60195937901799823, 1379.651450217159891, 229.3176569930949995 ) ) ;
#50597 = ORIENTED_EDGE ( 'NONE', *, *, #34451, .F. ) ;
#50598 = CARTESIAN_POINT ( 'NONE',  ( 11.97738863534810072, 1433.633111691630120, 150.0666321391890392 ) ) ;
#50599 = CARTESIAN_POINT ( 'NONE',  ( -2.393224162990000181, 1395.996633616729923, 220.4495428705980089 ) ) ;
#50600 = ORIENTED_EDGE ( 'NONE', *, *, #25098, .T. ) ;
#50601 = CARTESIAN_POINT ( 'NONE',  ( -0.0002584699284550677598, 1396.263918536362098, 221.2551011699866024 ) ) ;
#50602 = CARTESIAN_POINT ( 'NONE',  ( -10.34253148339749906, 1448.363770563499884, 208.2854772084710078 ) ) ;
#50603 = CARTESIAN_POINT ( 'NONE',  ( 4.324121584285009590, 1515.222544093250008, 206.1650180736299944 ) ) ;
#50605 = CARTESIAN_POINT ( 'NONE',  ( 17.43533191579999908, 1424.302130621530068, 226.6671662756980083 ) ) ;
#50604 = CARTESIAN_POINT ( 'NONE',  ( 2.370970874524634286, 1427.002265528474027, 134.0999999980979851 ) ) ;
#50606 = CARTESIAN_POINT ( 'NONE',  ( 17.77010835247230247, 1498.112583753600120, 230.1664113477359876 ) ) ;
#50607 = CARTESIAN_POINT ( 'NONE',  ( 0.8908956287060000312, 1468.708728676529972, 182.6671616012979769 ) ) ;
#50608 = CARTESIAN_POINT ( 'NONE',  ( 1.047166550769999871, 1468.609441862589847, 219.1136373509289967 ) ) ;
#50609 = CARTESIAN_POINT ( 'NONE',  ( -0.3062940834119980416, 1423.431708106900032, 191.1679817776989694 ) ) ;
#50610 = SURFACE_STYLE_USAGE ( .BOTH. , #59022 ) ;
#50611 = CARTESIAN_POINT ( 'NONE',  ( 2.211127611826209982, 1395.990274664960225, 198.3288829735440117 ) ) ;
#50612 = CARTESIAN_POINT ( 'NONE',  ( 1.316362887779999991, 1415.041103189330215, 191.5323437754979921 ) ) ;
#50613 = CARTESIAN_POINT ( 'NONE',  ( 10.96882372829999852, 1432.300972684430008, 151.7702498152980297 ) ) ;
#50614 = CARTESIAN_POINT ( 'NONE',  ( 6.390054448255000352, 1513.333000339840055, 201.6257627613769614 ) ) ;
#50615 = ORIENTED_EDGE ( 'NONE', *, *, #48204, .T. ) ;
#50616 = CARTESIAN_POINT ( 'NONE',  ( 13.39145132700120122, 1435.009615361580018, 149.5108276884409975 ) ) ;
#50617 = VERTEX_POINT ( 'NONE', #97193 ) ;
#50618 = ORIENTED_EDGE ( 'NONE', *, *, #24333, .T. ) ;
#50619 = CARTESIAN_POINT ( 'NONE',  ( 13.22577696261745039, 1444.679985164650816, 169.3877355158035698 ) ) ;
#50620 = CARTESIAN_POINT ( 'NONE',  ( -4.909144810329999942, 1464.788387721129993, 235.1559025205980049 ) ) ;
#50621 = CARTESIAN_POINT ( 'NONE',  ( -8.690454074780983973, 1474.493355088299722, 203.6172070775714928 ) ) ;
#50622 = CARTESIAN_POINT ( 'NONE',  ( -3.259729335964999919, 1517.119374999550018, 216.4589997383470177 ) ) ;
#50623 = CARTESIAN_POINT ( 'NONE',  ( -8.133931657293652862, 1511.520884441827775, 212.9284830860449631 ) ) ;
#50624 = CARTESIAN_POINT ( 'NONE',  ( 11.19148775935109974, 1422.145533233709784, 210.4506149377330075 ) ) ;
#50625 = LINE ( 'NONE', #101003, #21454 ) ;
#50626 = CARTESIAN_POINT ( 'NONE',  ( 2.285812126927549962E-14, 1380.413060387289988, 208.3364477938620212 ) ) ;
#50627 = EDGE_CURVE ( 'NONE', #46100, #19958, #108087, .T. ) ;
#50628 = B_SPLINE_CURVE_WITH_KNOTS ( 'NONE', 3,
 ( #30398, #80817, #72431, #100364, #21968, #56160, #106563, #89758, #64589, #90854, #47216, #6306, #82469, #74628, #47762, #5203, #64036, #57295, #98152, #14141, #21426, #107666, #81343, #48330, #4656, #30952, #91958, #65127, #99240, #40451, #22515, #5767, #74080, #108209, #23087, #91422, #14697, #48886, #108763, #46686, #32055, #23650, #68853, #94563, #66790, #52040, #43082, #18952, #15235 ),
 .UNSPECIFIED., .F., .F.,
 ( 4, 3, 3, 3, 3, 3, 3, 3, 3, 3, 3, 3, 3, 3, 3, 3, 4 ),
 ( 0.000000000000000000, 0.1298111464596899967, 0.2614081304872279965, 0.3961310922636709919, 0.5284374970052909681, 0.6643687372991460283, 0.7931396734179789743, 0.8002999775929999782, 1.059465424392620037, 1.309520818660049990, 1.559475944711749884, 1.808681423173479796, 2.056514135787280040, 2.301333315630279763, 2.543978965925790092, 2.783061379017449877, 2.873623551990000191 ),
 .UNSPECIFIED. ) ;
#50629 = ORIENTED_EDGE ( 'NONE', *, *, #89820, .F. ) ;
#50630 = CARTESIAN_POINT ( 'NONE',  ( 1.118903270415000151, 1517.003078582959688, 206.2405205581369785 ) ) ;
#50631 = ORIENTED_EDGE ( 'NONE', *, *, #18286, .T. ) ;
#50632 = CARTESIAN_POINT ( 'NONE',  ( -105.5086933517860075, 1378.552678757879903, 304.0434870558410125 ) ) ;
#50633 = CARTESIAN_POINT ( 'NONE',  ( -2.309262712062270850, 1512.187213306747481, 217.7723287588028995 ) ) ;
#50634 = ADVANCED_FACE ( 'NONE', ( #105616 ), #52547, .T. ) ;
#50636 = ADVANCED_FACE ( 'NONE', ( #52459 ), #79399, .T. ) ;
#50635 = CARTESIAN_POINT ( 'NONE',  ( -4.163739766079999960, 1409.058461383930080, 188.2538941213980195 ) ) ;
#50637 = CARTESIAN_POINT ( 'NONE',  ( 7.649034400464999273, 1514.243099272629934, 214.7715657207469917 ) ) ;
#50639 = ORIENTED_EDGE ( 'NONE', *, *, #80351, .F. ) ;
#50638 = CARTESIAN_POINT ( 'NONE',  ( -0.2679975439270000370, 1416.543503932829935, 227.4610302084980162 ) ) ;
#50640 = CARTESIAN_POINT ( 'NONE',  ( 24.57285633690000282, 1439.622216053659940, 213.1838506830980009 ) ) ;
#50641 = CARTESIAN_POINT ( 'NONE',  ( 17.78284146230000218, 1432.724246433989947, 213.5810953123289835 ) ) ;
#50642 = B_SPLINE_CURVE_WITH_KNOTS ( 'NONE', 3,
 ( #40663, #66445, #87079, #27724, #27177, #63031 ),
 .UNSPECIFIED., .F., .F.,
 ( 4, 2, 4 ),
 ( 0.000000000000000000, 0.5000000000000000000, 1.000000000000000000 ),
 .UNSPECIFIED. ) ;
#50643 = CARTESIAN_POINT ( 'NONE',  ( -109.2093473777249955, 1385.425682697149796, 295.1563182021879470 ) ) ;
#50644 = DIRECTION ( 'NONE',  ( -5.980589973904019347E-17, 1.000000000000000000, -1.736889445713099699E-16 ) ) ;
#50645 = CARTESIAN_POINT ( 'NONE',  ( -1.541850711665649963E-13, 1515.064792882589927, 213.4512947377390049 ) ) ;
#50646 = CARTESIAN_POINT ( 'NONE',  ( 1.134357970594999987, 1516.744381837270112, 213.1504571913470159 ) ) ;
#50647 = CARTESIAN_POINT ( 'NONE',  ( -3.215255062656879659, 1428.800608840759878, 200.3254522118909904 ) ) ;
#50648 = CARTESIAN_POINT ( 'NONE',  ( -21.86920309050000100, 1509.656483798930140, 190.1619192503980003 ) ) ;
#50649 = CARTESIAN_POINT ( 'NONE',  ( 6.455425405871869415, 1508.551704612109916, 215.9494989760289911 ) ) ;
#50650 = CARTESIAN_POINT ( 'NONE',  ( 7.338411959395000572, 1517.170512887980067, 211.6064236274570192 ) ) ;
#50651 = CARTESIAN_POINT ( 'NONE',  ( 9.574980784980720472, 1434.721929005479979, 207.0935444517720043 ) ) ;
#50652 = CARTESIAN_POINT ( 'NONE',  ( 14.30200421219999996, 1410.347835407430239, 191.4195238701979633 ) ) ;
#50653 = CARTESIAN_POINT ( 'NONE',  ( -11.54861356885641044, 1486.021746504592329, 184.4896162731949687 ) ) ;
#50655 = ORIENTED_EDGE ( 'NONE', *, *, #79634, .F. ) ;
#50654 = CARTESIAN_POINT ( 'NONE',  ( -47.49417614000000043, 1386.750003725609986, 256.2226892774589828 ) ) ;
#50656 = CARTESIAN_POINT ( 'NONE',  ( -59.28183620200640291, 1385.069713019159963, 279.7253289016610438 ) ) ;
#50657 = CARTESIAN_POINT ( 'NONE',  ( 33.93600685300000208, 1457.486634655030002, 259.3468319324980484 ) ) ;
#50658 = CARTESIAN_POINT ( 'NONE',  ( -8.515581525576479294, 1522.051704408389924, 226.9159523030141372 ) ) ;
#50659 = LINE ( 'NONE', #91557, #86130 ) ;
#50660 = CARTESIAN_POINT ( 'NONE',  ( -23.95803383590000379, 1445.274057039780018, 213.2142028417179915 ) ) ;
#50661 = CARTESIAN_POINT ( 'NONE',  ( 0.6079674380864850125, 1452.959918024070021, 183.3081617366339913 ) ) ;
#50663 = CARTESIAN_POINT ( 'NONE',  ( -8.580842993890000159, 1384.881883552430054, 218.6695867492290120 ) ) ;
#50662 = CARTESIAN_POINT ( 'NONE',  ( -2.500000000000000000, 1425.929641636930000, 178.2078840400980084 ) ) ;
#50664 = DIRECTION ( 'NONE',  ( 1.836970198721029688E-16, 1.000000000000000000, -2.953460612019999929E-19 ) ) ;
#50665 = CARTESIAN_POINT ( 'NONE',  ( -107.6465574917919952, 1382.804371864389850, 310.6282975730970293 ) ) ;
#50666 = VERTEX_POINT ( 'NONE', #94296 ) ;
#50667 = CARTESIAN_POINT ( 'NONE',  ( -2.487103457664999961, 1516.577434278289957, 202.5755431900869894 ) ) ;
#50668 = CARTESIAN_POINT ( 'NONE',  ( -0.2726096272919999453, 1487.204355548130025, 230.5507616997979881 ) ) ;
#50669 = CARTESIAN_POINT ( 'NONE',  ( 24.62744524829999904, 1442.406980887019927, 212.8172870668879852 ) ) ;
#50670 = CARTESIAN_POINT ( 'NONE',  ( -31.50799703744276670, 1526.382868172863709, 216.4233194664831785 ) ) ;
#50671 = CARTESIAN_POINT ( 'NONE',  ( -7.515458858486791627, 1461.908370352513202, 202.9557135729516517 ) ) ;
#50672 = CARTESIAN_POINT ( 'NONE',  ( 26.02899615147670076, 1450.772943025348695, 136.7241299949539552 ) ) ;
#50673 = CARTESIAN_POINT ( 'NONE',  ( 10.73431074182437328, 1418.150870888782492, 229.8889230194085656 ) ) ;
#50674 = CARTESIAN_POINT ( 'NONE',  ( 32.03035082978020398, 1436.091942216389953, 136.3581855157840153 ) ) ;
#50675 = CARTESIAN_POINT ( 'NONE',  ( 39.75685596340139938, 1446.397812216890088, 136.7371007338339837 ) ) ;
#50676 = CARTESIAN_POINT ( 'NONE',  ( 8.410267065803780360E-17, 1471.436294031830130, 269.3346704751489824 ) ) ;
#50677 = CARTESIAN_POINT ( 'NONE',  ( -2.670661672390000074, 1430.456431923590117, 201.2104187199990122 ) ) ;
#50678 = ADVANCED_FACE ( 'NONE', ( #6995 ), #35540, .T. ) ;
#50679 = CARTESIAN_POINT ( 'NONE',  ( 8.482872683409999226, 1508.704761105730086, 182.5447718006980153 ) ) ;
#50680 = CARTESIAN_POINT ( 'NONE',  ( -21.08703188482416380, 1525.317359687841190, 184.4717570622386518 ) ) ;
#50681 = CYLINDRICAL_SURFACE ( 'NONE', #72549, 1.000000000000000888 ) ;
#50682 = EDGE_LOOP ( 'NONE', ( #97682, #2644, #18657, #108818, #42080 ) ) ;
#50683 = CARTESIAN_POINT ( 'NONE',  ( 9.717824533310780666, 1463.678478211699939, 210.3770741684630252 ) ) ;
#50684 = CARTESIAN_POINT ( 'NONE',  ( 13.27700334932523951, 1506.366982238135279, 191.6232499193883427 ) ) ;
#50685 = CIRCLE ( 'NONE', #27679, 1.999999999999999556 ) ;
#50686 = CARTESIAN_POINT ( 'NONE',  ( -4.679794233794990710, 1508.610718263850003, 212.9834969940540077 ) ) ;
#50687 = FACE_OUTER_BOUND ( 'NONE', #91326, .T. ) ;
#50688 = CARTESIAN_POINT ( 'NONE',  ( -0.4966801320660000352, 1415.438062173830076, 233.3911217857980205 ) ) ;
#50689 = CARTESIAN_POINT ( 'NONE',  ( 11.47508409600000157, 1501.971768102289843, 208.9761436802440073 ) ) ;
#50690 = CARTESIAN_POINT ( 'NONE',  ( -29.27919551730000336, 1509.872435209829746, 208.8759114952370055 ) ) ;
#50691 = CARTESIAN_POINT ( 'NONE',  ( 8.191473432960000522, 1428.034249043490036, 212.8209790924290132 ) ) ;
#50692 = CARTESIAN_POINT ( 'NONE',  ( -4.259777698987590178, 1515.374151778960140, 212.0586637247320141 ) ) ;
#50693 = CARTESIAN_POINT ( 'NONE',  ( -11.19695579387275863, 1418.593385094034375, 229.3149266084969895 ) ) ;
#50694 = CARTESIAN_POINT ( 'NONE',  ( -7.821557675210984328, 1451.395427275060001, 152.9976685588227951 ) ) ;
#50695 = CARTESIAN_POINT ( 'NONE',  ( -5.345845988899998957, 1483.903125241190082, 199.7205319149290119 ) ) ;
#50696 = CARTESIAN_POINT ( 'NONE',  ( 25.06611318670000088, 1436.294882506480008, 137.6250933127980147 ) ) ;
#50697 =( BOUNDED_CURVE ( )  B_SPLINE_CURVE ( 3, ( #78101, #9791, #36112, #35543 ),
 .UNSPECIFIED., .F., .F. ) 
 B_SPLINE_CURVE_WITH_KNOTS ( ( 4, 4 ),
 ( 4.177675728947532363, 5.247004315084660142 ),
 .UNSPECIFIED. ) 
 CURVE ( )  GEOMETRIC_REPRESENTATION_ITEM ( )  RATIONAL_B_SPLINE_CURVE ( ( 1.000000000000000000, 0.9069598253110926489, 0.9069598253110926489, 1.000000000000000000 ) ) 
 REPRESENTATION_ITEM ( '' )  );
#50698 = CARTESIAN_POINT ( 'NONE',  ( 35.07315792529999499, 1444.191445724089817, 137.2843330345980064 ) ) ;
#50699 = ORIENTED_EDGE ( 'NONE', *, *, #88465, .F. ) ;
#50700 = CARTESIAN_POINT ( 'NONE',  ( 0.3266950887905089584, 1415.429375168339902, 191.4648083493140120 ) ) ;
#50701 = CARTESIAN_POINT ( 'NONE',  ( -13.12553473323018416, 1379.406084055735619, 211.7521813457520636 ) ) ;
#50702 = ORIENTED_EDGE ( 'NONE', *, *, #9075, .F. ) ;
#50703 = VERTEX_POINT ( 'NONE', #24338 ) ;
#50704 = FACE_OUTER_BOUND ( 'NONE', #57493, .T. ) ;
#50705 = CARTESIAN_POINT ( 'NONE',  ( 7.364872175426726564, 1516.579711047741739, 207.6756468922182819 ) ) ;
#50707 = CARTESIAN_POINT ( 'NONE',  ( -19.87540907819999703, 1452.861698873429987, 216.4112603940479858 ) ) ;
#50706 = FACE_OUTER_BOUND ( 'NONE', #20573, .T. ) ;
#50708 = CARTESIAN_POINT ( 'NONE',  ( -1.693092261709999935, 1443.235800066189995, 218.9922124666489935 ) ) ;
#50709 = CARTESIAN_POINT ( 'NONE',  ( 4.169165030684239603, 1424.160883088660057, 184.4444951202710001 ) ) ;
#50710 = EDGE_CURVE ( 'NONE', #53402, #65447, #101038, .T. ) ;
#50711 = CARTESIAN_POINT ( 'NONE',  ( -12.29845482411220026, 1378.332941950110126, 209.9703957929920080 ) ) ;
#50712 = CARTESIAN_POINT ( 'NONE',  ( -2.498700678426172939, 1421.135883849067341, 185.0048294103856676 ) ) ;
#50713 = CARTESIAN_POINT ( 'NONE',  ( -2.397475438392928204, 1525.713797967456912, 243.2249543484664116 ) ) ;
#50714 = CARTESIAN_POINT ( 'NONE',  ( -24.19213419669999610, 1438.598800249630131, 211.7608300950280125 ) ) ;
#50715 = CARTESIAN_POINT ( 'NONE',  ( -3.644092503733519894, 1454.098320749749973, 199.2979021310670191 ) ) ;
#50716 = CARTESIAN_POINT ( 'NONE',  ( 1.528898867239999904, 1450.858514550550126, 182.5684021596979960 ) ) ;
#50717 = CARTESIAN_POINT ( 'NONE',  ( 9.622136349630000751, 1363.684386430210225, 207.6218459616989946 ) ) ;
#50718 = CARTESIAN_POINT ( 'NONE',  ( -27.56847755513489062, 1509.987811263605408, 197.2905327719515185 ) ) ;
#50720 = ORIENTED_EDGE ( 'NONE', *, *, #26674, .T. ) ;
#50719 = CARTESIAN_POINT ( 'NONE',  ( -2.804568549241229620E-09, 1414.830288601209986, 244.9882278679610010 ) ) ;
#50721 = ORIENTED_EDGE ( 'NONE', *, *, #77606, .F. ) ;
#50722 = CARTESIAN_POINT ( 'NONE',  ( -2.188078410709979771, 1508.020976590390092, 220.9453026643990086 ) ) ;
#50723 = CARTESIAN_POINT ( 'NONE',  ( -19.88052731184480137, 1484.560536701516867, 191.1415595291306602 ) ) ;
#50724 = CARTESIAN_POINT ( 'NONE',  ( -3.472352184000000008, 1472.519747990830183, 270.3710077336979793 ) ) ;
#50725 = CARTESIAN_POINT ( 'NONE',  ( -110.0628831554700042, 1384.910109443090050, 296.9513044379630173 ) ) ;
#50726 = CARTESIAN_POINT ( 'NONE',  ( -118.8461440515248171, 1348.229899472569514, 301.2466039018639208 ) ) ;
#50727 = LINE ( 'NONE', #57502, #1790 ) ;
#50728 = CARTESIAN_POINT ( 'NONE',  ( 2.096969080950850106, 1476.217590029780013, 197.8222115087120017 ) ) ;
#50729 = CARTESIAN_POINT ( 'NONE',  ( -22.91663120903140083, 1507.606285602550088, 207.6071078552859888 ) ) ;
#50730 = CARTESIAN_POINT ( 'NONE',  ( 9.369782510132241171, 1366.497526915279877, 210.6218459616991936 ) ) ;
#50731 = CARTESIAN_POINT ( 'NONE',  ( -10.04889086637309958, 1447.057712588790082, 211.5131067902999860 ) ) ;
#50732 = CARTESIAN_POINT ( 'NONE',  ( -23.80723810840019894, 1411.676400612559974, 269.4670551916460113 ) ) ;
#50733 = CARTESIAN_POINT ( 'NONE',  ( -14.56157998151809885, 1435.986635814069814, 149.8060811127620013 ) ) ;
#50734 = ORIENTED_EDGE ( 'NONE', *, *, #32346, .F. ) ;
#50735 = CARTESIAN_POINT ( 'NONE',  ( -4.328283507529860685, 1515.109292691759947, 210.1175503365320196 ) ) ;
#50736 = CARTESIAN_POINT ( 'NONE',  ( 13.43628448359999972, 1443.378768469500073, 188.3384116640980039 ) ) ;
#50737 = ORIENTED_EDGE ( 'NONE', *, *, #74658, .T. ) ;
#50738 = ORIENTED_EDGE ( 'NONE', *, *, #102468, .T. ) ;
#50739 = CARTESIAN_POINT ( 'NONE',  ( 5.026278901445378366, 1423.016945676001569, 184.4099619136632953 ) ) ;
#50740 = CARTESIAN_POINT ( 'NONE',  ( 9.475492894836309077, 1425.388351994820141, 195.3726508077949688 ) ) ;
#50741 = CARTESIAN_POINT ( 'NONE',  ( 2.877113070465000089, 1516.697242742309982, 214.1184881303969973 ) ) ;
#50742 = CARTESIAN_POINT ( 'NONE',  ( -19.28103481819999843, 1485.491211888429916, 189.7669585599980167 ) ) ;
#50743 = CYLINDRICAL_SURFACE ( 'NONE', #10801, 2.000000000000003553 ) ;
#50744 = ORIENTED_EDGE ( 'NONE', *, *, #49995, .T. ) ;
#50745 = CARTESIAN_POINT ( 'NONE',  ( -109.5441724430000079, 1374.437034645689891, 303.4364478832590066 ) ) ;
#50746 = ADVANCED_FACE ( 'NONE', ( #92648 ), #89256, .F. ) ;
#50747 = EDGE_CURVE ( 'NONE', #60042, #23187, #26551, .T. ) ;
#50748 = EDGE_CURVE ( 'NONE', #78107, #97433, #85476, .T. ) ;
#50749 = CARTESIAN_POINT ( 'NONE',  ( -1.709358701255000001, 1516.542957540330008, 202.1882582765869927 ) ) ;
#50750 = CARTESIAN_POINT ( 'NONE',  ( -26.92695807870000380, 1508.008395488129963, 203.1594552079080245 ) ) ;
#50751 = ADVANCED_FACE ( 'NONE', ( #38261 ), #90312, .F. ) ;
#50752 = DIRECTION ( 'NONE',  ( 0.000000000000000000, 0.000000000000000000, 1.000000000000000000 ) ) ;
#50753 = EDGE_CURVE ( 'NONE', #53407, #48957, #10845, .T. ) ;
#50754 = CARTESIAN_POINT ( 'NONE',  ( -35.92330893652459878, 1384.571147577790043, 209.4208511670099995 ) ) ;
#50755 = CARTESIAN_POINT ( 'NONE',  ( -6.688849051720000105, 1408.965348141229924, 196.7627783315979855 ) ) ;
#50756 = DIRECTION ( 'NONE',  ( 1.755985294532464991E-16, -1.000000000000000000, 1.338183447452830017E-16 ) ) ;
#50758 = ORIENTED_EDGE ( 'NONE', *, *, #83572, .F. ) ;
#50757 = CARTESIAN_POINT ( 'NONE',  ( 31.26701538686466719, 1523.919934424249959, 196.3491293340342736 ) ) ;
#50759 = CARTESIAN_POINT ( 'NONE',  ( -25.19786267552049708, 1449.936431062559905, 210.5275732939500131 ) ) ;
#50760 = CARTESIAN_POINT ( 'NONE',  ( 26.66930585240000084, 1508.126733773130127, 215.8812207616579997 ) ) ;
#50761 = AXIS2_PLACEMENT_3D ( 'NONE', #80632, #35881, #71726 ) ;
#50762 = CARTESIAN_POINT ( 'NONE',  ( -68.39223289816457907, 1379.747175533331301, 280.0421571237133094 ) ) ;
#50763 = EDGE_CURVE ( 'NONE', #80101, #23359, #62528, .T. ) ;
#50764 = CARTESIAN_POINT ( 'NONE',  ( 10.73980232230699983, 1460.418891470940025, 207.1303042227569904 ) ) ;
#50765 = CARTESIAN_POINT ( 'NONE',  ( -24.69200176050000195, 1435.857451379459917, 137.7788013625980170 ) ) ;
#50766 = CARTESIAN_POINT ( 'NONE',  ( 4.043990307595000111, 1516.983612918759945, 211.6010928179370012 ) ) ;
#50767 = CARTESIAN_POINT ( 'NONE',  ( -68.75005492889998493, 1379.747908384619905, 280.1011935185590005 ) ) ;
#50768 = CIRCLE ( 'NONE', #29342, 7.842199003069996621 ) ;
#50769 = CARTESIAN_POINT ( 'NONE',  ( -18.53032035940000100, 1445.072917693090176, 205.4274489127490142 ) ) ;
#50770 = CARTESIAN_POINT ( 'NONE',  ( -18.02257621027557377, 1526.382868172863937, 235.3484976865589147 ) ) ;
#50771 = CARTESIAN_POINT ( 'NONE',  ( 1.704170714124999986, 1516.927039499179955, 208.3639196453299860 ) ) ;
#50772 = VERTEX_POINT ( 'NONE', #80828 ) ;
#50773 = CARTESIAN_POINT ( 'NONE',  ( -40.71747596959829707, 1448.637563236699862, 134.4203405313490123 ) ) ;
#50775 = EDGE_CURVE ( 'NONE', #79540, #33227, #26582, .T. ) ;
#50774 = CARTESIAN_POINT ( 'NONE',  ( -1.912834366250000029, 1412.842211185330143, 232.9360292305979954 ) ) ;
#50776 = CARTESIAN_POINT ( 'NONE',  ( -19.68132502244943893, 1456.948574072194788, 225.7511772315920950 ) ) ;
#50777 = ORIENTED_EDGE ( 'NONE', *, *, #95243, .F. ) ;
#50778 = CARTESIAN_POINT ( 'NONE',  ( -2.738357492517908387, 1525.795403621571040, 240.9366226831509437 ) ) ;
#50779 = CARTESIAN_POINT ( 'NONE',  ( 12.94392783832900129, 1435.642753611090029, 150.6515099629039867 ) ) ;
#50780 = B_SPLINE_SURFACE_WITH_KNOTS ( 'NONE', 5, 1, ( 
 ( #105065, #51341 ),
 ( #85475, #8774 ),
 ( #77116, #9349 ),
 ( #34540, #97756 ),
 ( #80420, #13176 ),
 ( #55231, #3733 ) ),
 .UNSPECIFIED., .F., .F., .F.,
 ( 6, 6 ),
 ( 2, 2 ),
 ( -2.070056070795430156E-05, 17.51321923676070114 ),
 ( 0.000000000000000000, 14.00002070056070025 ),
 .UNSPECIFIED. ) ;
#50781 = CARTESIAN_POINT ( 'NONE',  ( 15.19613196592609938, 1459.303298073210044, 229.7660246535220097 ) ) ;
#50782 = EDGE_CURVE ( 'NONE', #17951, #26163, #48412, .T. ) ;
#50783 = CARTESIAN_POINT ( 'NONE',  ( -12.32280451139999933, 1415.506406008910062, 208.1838605997770060 ) ) ;
#50784 = CARTESIAN_POINT ( 'NONE',  ( 26.85712173870000186, 1451.975206518229925, 134.9164576279979997 ) ) ;
#50785 = CARTESIAN_POINT ( 'NONE',  ( 5.547280765580000050, 1487.873461314389942, 198.4571336758990014 ) ) ;
#50786 = ADVANCED_FACE ( 'NONE', ( #29315 ), #65691, .T. ) ;
#50787 = CARTESIAN_POINT ( 'NONE',  ( 13.15726448907880020, 1416.913057013679918, 198.3331256186419864 ) ) ;
#50788 = DIRECTION ( 'NONE',  ( -0.000000000000000000, 1.000000000000000000, -0.000000000000000000 ) ) ;
#50790 = CARTESIAN_POINT ( 'NONE',  ( -7.777329619812174855, 1449.162765272808201, 191.3840481915840144 ) ) ;
#50789 = CARTESIAN_POINT ( 'NONE',  ( -3.449777353855000062, 1516.974592746400049, 214.1332139170270068 ) ) ;
#50791 = CARTESIAN_POINT ( 'NONE',  ( 20.81411617090000021, 1509.690291770430122, 187.8298652661979986 ) ) ;
#50792 = CARTESIAN_POINT ( 'NONE',  ( 0.1595995995380000143, 1486.508831850330125, 181.8147405652979671 ) ) ;
#50793 = EDGE_LOOP ( 'NONE', ( #91039, #47138, #89653, #66733 ) ) ;
#50794 = CARTESIAN_POINT ( 'NONE',  ( 2.283436972078669822E-15, 1391.413060387289988, 209.1218459572589836 ) ) ;
#50795 = B_SPLINE_SURFACE_WITH_KNOTS ( 'NONE', 5, 5, ( 
 ( #36014, #70206, #104312, #27603, #95911, #42753 ),
 ( #53378, #104864, #87524, #10814, #44983, #28152 ),
 ( #62342, #79681, #90247, #20288, #21373, #72384 ),
 ( #12450, #98101, #29257, #54494, #97567, #30346 ),
 ( #5150, #46634, #3533, #39305, #4076, #71863 ),
 ( #89161, #107062, #28711, #20839, #99190, #88082 ) ),
 .UNSPECIFIED., .F., .F., .F.,
 ( 6, 6 ),
 ( 6, 6 ),
 ( 15.04009677950000068, 20.59615426749999756 ),
 ( 0.000000000000000000, 2.000000000000000000 ),
 .UNSPECIFIED. ) ;
#50796 = CARTESIAN_POINT ( 'NONE',  ( -17.01683863309999722, 1420.343045529830079, 203.4497032551290090 ) ) ;
#50797 = ORIENTED_EDGE ( 'NONE', *, *, #16575, .F. ) ;
#50798 = ADVANCED_FACE ( 'NONE', ( #63513 ), #73938, .F. ) ;
#50799 = CARTESIAN_POINT ( 'NONE',  ( 0.3035066335680000060, 1419.252317566729971, 184.6483442805979962 ) ) ;
#50800 = B_SPLINE_CURVE_WITH_KNOTS ( 'NONE', 5,
 ( #55446, #11240, #89573, #79003, #29124, #30209, #70609, #28575, #2306 ),
 .UNSPECIFIED., .F., .F.,
 ( 6, 3, 6 ),
 ( -14.37983903770000005, -7.189919518870000026, -1.776356839400250465E-15 ),
 .UNSPECIFIED. ) ;
#50801 = CARTESIAN_POINT ( 'NONE',  ( 3.062931151456462775, 1525.320827368860137, 176.8367908461840443 ) ) ;
#50802 = CARTESIAN_POINT ( 'NONE',  ( 9829.078716723830439, 2833.596074015639715, -1083.720023828199828 ) ) ;
#50803 = CARTESIAN_POINT ( 'NONE',  ( -11.16643434163729864, 1471.372555858320084, 206.7508257846899937 ) ) ;
#50804 = CARTESIAN_POINT ( 'NONE',  ( -4.309330992969162999, 1508.176589348497373, 220.5992834243717766 ) ) ;
#50805 = CARTESIAN_POINT ( 'NONE',  ( 18.94485037129999583, 1416.547221147930031, 210.4653698564179933 ) ) ;
#50806 = CARTESIAN_POINT ( 'NONE',  ( 14.88455792500072228, 1507.555497567031580, 232.3243931051981406 ) ) ;
#50807 = CARTESIAN_POINT ( 'NONE',  ( 9.146295267174979315, 1461.861888617270097, 205.8341477717290218 ) ) ;
#50808 = CARTESIAN_POINT ( 'NONE',  ( -12.00000000000000000, 1443.913060387330006, 147.5878346084980137 ) ) ;
#50809 = CARTESIAN_POINT ( 'NONE',  ( 26.04901694399470102, 1446.564900598870054, 138.1454005870479875 ) ) ;
#50811 = CARTESIAN_POINT ( 'NONE',  ( 26.19952982486130111, 1509.827968087110094, 209.0871425590960087 ) ) ;
#50810 = CARTESIAN_POINT ( 'NONE',  ( -13.79952627106220042, 1418.844960651139900, 200.3911282168379842 ) ) ;
#50812 = CARTESIAN_POINT ( 'NONE',  ( 13.09590858069999975, 1426.025605857829987, 222.2823526253980049 ) ) ;
#50813 = ORIENTED_EDGE ( 'NONE', *, *, #83912, .F. ) ;
#50814 = ORIENTED_EDGE ( 'NONE', *, *, #75300, .T. ) ;
#50815 = CARTESIAN_POINT ( 'NONE',  ( -12.48995958582669985, 1501.883328869510024, 211.6213070116990025 ) ) ;
#50816 = CARTESIAN_POINT ( 'NONE',  ( -19.74447868890439040, 1485.088289844508154, 190.4769327812108202 ) ) ;
#50817 = CARTESIAN_POINT ( 'NONE',  ( -28.29497435070000222, 1509.672356513830209, 211.0137316004380068 ) ) ;
#50818 = CARTESIAN_POINT ( 'NONE',  ( 3.457627847960712320, 1410.410824016061724, 185.8561312258957514 ) ) ;
#50819 = CARTESIAN_POINT ( 'NONE',  ( -3.421145496696929023, 1426.005600530342690, 185.8301723314418155 ) ) ;
#50820 = B_SPLINE_SURFACE_WITH_KNOTS ( 'NONE', 5, 1, ( 
 ( #45132, #42475 ),
 ( #50890, #110228 ),
 ( #104457, #79274 ),
 ( #85020, #61943 ),
 ( #19330, #16152 ),
 ( #8314, #93423 ),
 ( #33502, #67703 ),
 ( #25105, #76632 ),
 ( #25659, #70900 ) ),
 .UNSPECIFIED., .F., .F., .F.,
 ( 6, 3, 6 ),
 ( 2, 2 ),
 ( 0.000000000000000000, 7.208900216690000029, 14.43479085090000069 ),
 ( 0.000000000000000000, 14.00000000000000000 ),
 .UNSPECIFIED. ) ;
#50821 = CARTESIAN_POINT ( 'NONE',  ( 9.379603162543640238, 1422.628403586280001, 212.8485163645989928 ) ) ;
#50822 = EDGE_CURVE ( 'NONE', #58393, #47709, #42131, .T. ) ;
#50823 = CARTESIAN_POINT ( 'NONE',  ( -4.635897072777390271, 1377.991090176196622, 203.9911396117953188 ) ) ;
#50824 = CARTESIAN_POINT ( 'NONE',  ( 10.75633390746000018, 1451.138030594549946, 190.3409186702180023 ) ) ;
#50825 = CARTESIAN_POINT ( 'NONE',  ( -63.13574013807390628, 1383.792676540780121, 285.6932720343630194 ) ) ;
#50826 = DIRECTION ( 'NONE',  ( -1.295211781927295682E-16, 1.000000000000000000, 0.000000000000000000 ) ) ;
#50827 = EDGE_CURVE ( 'NONE', #8084, #29796, #8506, .T. ) ;
#50828 = CARTESIAN_POINT ( 'NONE',  ( -5.219699508016872436, 1391.908825959211299, 214.5074746467423950 ) ) ;
#50829 = DIRECTION ( 'NONE',  ( 0.000000000000000000, -1.000000000000000000, 0.000000000000000000 ) ) ;
#50831 = ORIENTED_EDGE ( 'NONE', *, *, #103398, .T. ) ;
#50830 = CARTESIAN_POINT ( 'NONE',  ( -1.107012941800000094, 1455.995237770089943, 218.5495680003989776 ) ) ;
#50832 = CARTESIAN_POINT ( 'NONE',  ( -0.5133638609672289688, 1410.311096993930050, 233.1717005261690190 ) ) ;
#50833 = CARTESIAN_POINT ( 'NONE',  ( -38.64161925439999834, 1383.830331748989920, 239.2263113910589993 ) ) ;
#50834 = CARTESIAN_POINT ( 'NONE',  ( 4.865329319716050094, 1508.551704408389924, 205.8589166638820132 ) ) ;
#50835 = ORIENTED_EDGE ( 'NONE', *, *, #77392, .F. ) ;
#50836 = VERTEX_POINT ( 'NONE', #101449 ) ;
#50837 = CARTESIAN_POINT ( 'NONE',  ( 18.11450235977809697, 1507.710540422290023, 230.4427282681980103 ) ) ;
#50838 = CARTESIAN_POINT ( 'NONE',  ( -15.90990259576500065, 1513.492015765619954, 220.0820010595669771 ) ) ;
#50839 = CARTESIAN_POINT ( 'NONE',  ( 38.12415249455629862, 1438.740481096789836, 136.6172136615510055 ) ) ;
#50841 = CARTESIAN_POINT ( 'NONE',  ( -2.407253779970412566, 1523.313115944345554, 243.1783812783781116 ) ) ;
#50840 = CARTESIAN_POINT ( 'NONE',  ( -11.87227031139999944, 1435.412617320299887, 147.6610825172980128 ) ) ;
#50842 = CIRCLE ( 'NONE', #100855, 2.000000000000001776 ) ;
#50843 = CARTESIAN_POINT ( 'NONE',  ( -7.773290426329999114, 1463.683257113590116, 201.8013873513490068 ) ) ;
#50844 = CARTESIAN_POINT ( 'NONE',  ( -109.5297118039999873, 1383.965857270459992, 297.1689209028589858 ) ) ;
#50845 = ADVANCED_FACE ( 'NONE', ( #7418 ), #71402, .T. ) ;
#50846 = CARTESIAN_POINT ( 'NONE',  ( -109.1656546792999904, 1384.956445601399992, 297.1328575267269798 ) ) ;
#50847 = CARTESIAN_POINT ( 'NONE',  ( -0.4725090652239359867, 1450.961208915834504, 181.9239884145632118 ) ) ;
#50848 = CARTESIAN_POINT ( 'NONE',  ( -11.08276793864819965, 1508.551704408389924, 217.7591383316709823 ) ) ;
#50849 = CARTESIAN_POINT ( 'NONE',  ( 4.486565162759999836, 1409.573462333729822, 186.4102199717980284 ) ) ;
#50850 = CARTESIAN_POINT ( 'NONE',  ( 4.087244338739999705, 1424.194161142730081, 184.7150739516980025 ) ) ;
#50851 = CARTESIAN_POINT ( 'NONE',  ( -1.772523594583782724, 1468.998700552058153, 218.9957837055941638 ) ) ;
#50852 = CARTESIAN_POINT ( 'NONE',  ( -2.500000000000000000, 1439.245488529090153, 159.3585436906180348 ) ) ;
#50853 = CIRCLE ( 'NONE', #27593, 1.999999999999998668 ) ;
#50854 = CARTESIAN_POINT ( 'NONE',  ( -2.951770618412270064, 1451.103496634380008, 184.7382020502219859 ) ) ;
#50855 = CARTESIAN_POINT ( 'NONE',  ( 0.4196953096899999625, 1466.017965088330129, 235.8216877134980223 ) ) ;
#50856 = EDGE_LOOP ( 'NONE', ( #58201, #47712, #12689, #67063 ) ) ;
#50857 = CARTESIAN_POINT ( 'NONE',  ( 11.14734945969999913, 1480.282866945889964, 229.7914729789989963 ) ) ;
#50858 = CARTESIAN_POINT ( 'NONE',  ( -2.424063131930000115, 1427.257651041929876, 147.9020499575979954 ) ) ;
#50859 = CARTESIAN_POINT ( 'NONE',  ( 11.78238356083980065, 1440.882651838439870, 188.1224447589279976 ) ) ;
#50860 = CARTESIAN_POINT ( 'NONE',  ( 22.28696231330000188, 1506.798305107829947, 209.3970118511340104 ) ) ;
#50861 = CARTESIAN_POINT ( 'NONE',  ( -14.20118038929999926, 1469.193620957790017, 194.7233937116990035 ) ) ;
#50862 = EDGE_CURVE ( 'NONE', #67358, #61077, #16342, .T. ) ;
#50863 = CARTESIAN_POINT ( 'NONE',  ( -1.299075913466369845E-09, 1471.155365519019824, 256.9781891023540652 ) ) ;
#50864 = CARTESIAN_POINT ( 'NONE',  ( 28.27139721233048419, 1526.382868172863937, 219.5606225550385489 ) ) ;
#50865 = CARTESIAN_POINT ( 'NONE',  ( -12.38301933081382877, 1507.638490212013721, 208.9814132965477427 ) ) ;
#50866 = CARTESIAN_POINT ( 'NONE',  ( -0.8945944849849999381, 1417.298095640030169, 235.8147265461980169 ) ) ;
#50867 = CARTESIAN_POINT ( 'NONE',  ( -2.199814249270000133, 1475.434091217589867, 198.2859427615989887 ) ) ;
#50868 = CARTESIAN_POINT ( 'NONE',  ( -107.9182817679999857, 1387.176265556199951, 310.5436438242589929 ) ) ;
#50869 = CARTESIAN_POINT ( 'NONE',  ( -0.04668112204882676752, 1486.220989728969016, 181.8154795728657405 ) ) ;
#50870 = CARTESIAN_POINT ( 'NONE',  ( 0.06074730888943565693, 1359.389611325063242, 207.6218459616987673 ) ) ;
#50871 = CARTESIAN_POINT ( 'NONE',  ( -46.19910792603680250, 1438.826958754830002, 267.5922038166469292 ) ) ;
#50872 = CARTESIAN_POINT ( 'NONE',  ( 13.94394020758319819, 1509.346948278499895, 234.4482500451630074 ) ) ;
#50873 = EDGE_CURVE ( 'NONE', #40166, #103332, #12740, .T. ) ;
#50874 = CARTESIAN_POINT ( 'NONE',  ( -8.089559954360000305, 1425.642170091349954, 208.1666042629669846 ) ) ;
#50875 = ORIENTED_EDGE ( 'NONE', *, *, #90513, .F. ) ;
#50876 = CARTESIAN_POINT ( 'NONE',  ( -0.7533003905399979772, 1516.992029636990083, 208.3816250717139837 ) ) ;
#50877 = CARTESIAN_POINT ( 'NONE',  ( -12.85016526419999927, 1389.184315283510159, 203.6059765727289914 ) ) ;
#50878 = CARTESIAN_POINT ( 'NONE',  ( -8.938145041388430911, 1471.651254853389446, 214.0140567895946901 ) ) ;
#50879 = CARTESIAN_POINT ( 'NONE',  ( 7.311343960930040353, 1426.407259653950177, 212.7706406922160056 ) ) ;
#50880 = CARTESIAN_POINT ( 'NONE',  ( -25.27414439665539803, 1452.025395757659908, 135.5207945563980161 ) ) ;
#50881 = ORIENTED_EDGE ( 'NONE', *, *, #11868, .T. ) ;
#50882 = CARTESIAN_POINT ( 'NONE',  ( 21.83685800909999841, 1429.816530635930121, 221.4941967423980032 ) ) ;
#50884 = CARTESIAN_POINT ( 'NONE',  ( -15.30266652055029830, 1512.633419863009976, 222.5280214136559778 ) ) ;
#50883 = CARTESIAN_POINT ( 'NONE',  ( -10.93326214739339974, 1492.840634310439782, 207.3500978010279994 ) ) ;
#50885 = EDGE_CURVE ( 'NONE', #76758, #28705, #17233, .T. ) ;
#50886 = CIRCLE ( 'NONE', #79764, 2.000000000000023537 ) ;
#50887 = CARTESIAN_POINT ( 'NONE',  ( -2.115949517696979587, 1419.508337143739709, 185.9017425962819914 ) ) ;
#50889 = CARTESIAN_POINT ( 'NONE',  ( -24.40164416920000079, 1439.300524262840099, 211.9534758538480332 ) ) ;
#50888 = B_SPLINE_CURVE_WITH_KNOTS ( 'NONE', 3,
 ( #71195, #30243, #62810, #3982, #50385, #5612, #15624, #100219, #25139, #23499, #67184, #40857, #91806, #73925, #83960, #108054, #49830, #32996, #57137, #66092, #75033, #76121, #48732, #91265, #101285, #24580, #84513, #7260, #41423, #48176, #92352, #57691, #109184, #99641 ),
 .UNSPECIFIED., .F., .F.,
 ( 4, 3, 3, 3, 3, 3, 3, 3, 3, 3, 3, 4 ),
 ( -2.000000000000000000, -1.859445973531549834, -1.676484109249690047, -1.491267025722599948, -1.304875122534860044, -1.117035657520179859, -0.9287884496328548956, -0.7405969126087090793, -0.5529186171893840651, -0.3669390813415169816, -0.1825462010525040757, 0.000000000000000000 ),
 .UNSPECIFIED. ) ;
#50890 = CARTESIAN_POINT ( 'NONE',  ( 4.975825873569999835, 1424.099705961009931, 208.5330668394979909 ) ) ;
#50891 = ADVANCED_FACE ( 'NONE', ( #15780 ), #84665, .F. ) ;
#50892 = CARTESIAN_POINT ( 'NONE',  ( -14.27715603315103543, 1416.818673810148084, 221.7183468844290530 ) ) ;
#50893 = CARTESIAN_POINT ( 'NONE',  ( -18.79647803339999967, 1416.822694190429729, 208.4084638389329882 ) ) ;
#50894 = ORIENTED_EDGE ( 'NONE', *, *, #52970, .T. ) ;
#50895 = CARTESIAN_POINT ( 'NONE',  ( -1.243032230405529903, 1408.244502896100130, 270.3924218761350176 ) ) ;
#50896 = CARTESIAN_POINT ( 'NONE',  ( 12.34120302092700072, 1420.636070528880055, 230.5426365944759937 ) ) ;
#50897 = CARTESIAN_POINT ( 'NONE',  ( 8.980818830724000890, 1434.681779501059964, 206.5340080207419931 ) ) ;
#50898 = EDGE_LOOP ( 'NONE', ( #53980, #45000, #15929, #90528 ) ) ;
#50899 = ORIENTED_EDGE ( 'NONE', *, *, #10863, .F. ) ;
#50900 = CARTESIAN_POINT ( 'NONE',  ( -23.01060016338059810, 1409.833637653050118, 209.8936558164379846 ) ) ;
#50901 = CARTESIAN_POINT ( 'NONE',  ( -7.649034438594999763, 1514.243099272629934, 203.4721261815869866 ) ) ;
#50902 = CARTESIAN_POINT ( 'NONE',  ( -103.5905391456900020, 1377.418846546390114, 309.5807788459990206 ) ) ;
#50903 = CARTESIAN_POINT ( 'NONE',  ( -2.329729395510000245, 1427.373795049630189, 123.0297916884979941 ) ) ;
#50904 = ADVANCED_FACE ( 'NONE', ( #93068 ), #80685, .T. ) ;
#50905 = CARTESIAN_POINT ( 'NONE',  ( -19.14510341657199888, 1447.481386810810136, 194.0904547693720019 ) ) ;
#50906 = EDGE_CURVE ( 'NONE', #29671, #89283, #102010, .T. ) ;
#50907 = CARTESIAN_POINT ( 'NONE',  ( -18.60329415920000073, 1410.876893835729788, 223.7172180216979882 ) ) ;
#50908 = CARTESIAN_POINT ( 'NONE',  ( 32.63392384532819790, 1464.921899099569828, 269.3041819200249734 ) ) ;
#50909 = CARTESIAN_POINT ( 'NONE',  ( -3.958629232097630180, 1508.551704408389924, 204.1347648892599977 ) ) ;
#50910 = CARTESIAN_POINT ( 'NONE',  ( -16.47782421224261995, 1421.308645812501709, 226.9890287628209649 ) ) ;
#50911 = CARTESIAN_POINT ( 'NONE',  ( 1.702405985064999960, 1516.999105586269934, 205.8518611507970206 ) ) ;
#50912 = EDGE_LOOP ( 'NONE', ( #70894, #28562, #88986, #53053 ) ) ;
#50913 = CARTESIAN_POINT ( 'NONE',  ( -11.93562773578777048, 1433.536277773312577, 150.1881492786055219 ) ) ;
#50914 = CARTESIAN_POINT ( 'NONE',  ( 15.29008551986609987, 1513.004579589629884, 195.2250800361269967 ) ) ;
#50915 = CARTESIAN_POINT ( 'NONE',  ( 8.036006549726169013, 1434.089066884029990, 225.8500050052630002 ) ) ;
#50916 = VERTEX_POINT ( 'NONE', #77389 ) ;
#50917 = CARTESIAN_POINT ( 'NONE',  ( 4.987078446123650366, 1508.551704408389924, 206.6339246584809928 ) ) ;
#50918 = CARTESIAN_POINT ( 'NONE',  ( 27.02694966472599702, 1451.203421905880077, 136.2754127003069868 ) ) ;
#50919 = CARTESIAN_POINT ( 'NONE',  ( -4.913312227335970839, 1508.551704408389924, 212.2183601949549825 ) ) ;
#50920 = CARTESIAN_POINT ( 'NONE',  ( -13.62888597016050163, 1517.051704413129983, 226.2994540733420195 ) ) ;
#50921 = CARTESIAN_POINT ( 'NONE',  ( 7.439417113980000273, 1422.547532122410075, 195.6475770543989938 ) ) ;
#50922 = EDGE_CURVE ( 'NONE', #70769, #1585, #100344, .T. ) ;
#50924 = B_SPLINE_SURFACE_WITH_KNOTS ( 'NONE', 5, 5, ( 
 ( #9884, #51333, #68715, #10999, #27793, #104500 ),
 ( #35634, #102820, #44611, #17142, #2068, #9341 ),
 ( #95547, #96095, #10439, #42948, #27243, #44052 ),
 ( #53015, #86043, #61980, #415, #1503, #70383 ),
 ( #59755, #43503, #2622, #17699, #19371, #95001 ),
 ( #69828, #18269, #53574, #36199, #18820, #26676 ) ),
 .UNSPECIFIED., .F., .F., .F.,
 ( 6, 6 ),
 ( 6, 6 ),
 ( 5.220737937810000062, 7.751661675270000273 ),
 ( 0.000000000000000000, 2.000000000000000000 ),
 .UNSPECIFIED. ) ;
#50923 = CARTESIAN_POINT ( 'NONE',  ( -2.787430966700440216, 1433.043516581739823, 218.2512527028169984 ) ) ;
#50925 = CARTESIAN_POINT ( 'NONE',  ( -4.075622605530000442, 1495.353897722689908, 197.4859375650989932 ) ) ;
#50926 = AXIS2_PLACEMENT_3D ( 'NONE', #94985, #43490, #104485 ) ;
#50927 = CARTESIAN_POINT ( 'NONE',  ( 5.734105306875630248, 1409.113299756970036, 188.1906873671159985 ) ) ;
#50929 = DIRECTION ( 'NONE',  ( 0.000000000000000000, 1.000000000000000000, 0.000000000000000000 ) ) ;
#50928 = FACE_OUTER_BOUND ( 'NONE', #78281, .T. ) ;
#50930 = LINE ( 'NONE', #102413, #43302 ) ;
#50931 = FACE_OUTER_BOUND ( 'NONE', #13958, .T. ) ;
#50933 = EDGE_CURVE ( 'NONE', #100321, #24499, #44060, .T. ) ;
#50932 = CIRCLE ( 'NONE', #79554, 32.13701971169416538 ) ;
#50934 = CARTESIAN_POINT ( 'NONE',  ( 16.90814665888983015, 1423.564526555951034, 229.0298210386986852 ) ) ;
#50935 = ORIENTED_EDGE ( 'NONE', *, *, #46138, .T. ) ;
#50936 = FACE_OUTER_BOUND ( 'NONE', #55619, .T. ) ;
#50937 = VECTOR ( 'NONE', #36224, 1000.000000000000227 ) ;
#50938 = CARTESIAN_POINT ( 'NONE',  ( 11.35815110745130063, 1432.342270311610037, 151.4015260409140069 ) ) ;
#50940 = CARTESIAN_POINT ( 'NONE',  ( -106.4480417398009848, 1384.930840067430154, 311.2385799845050087 ) ) ;
#50939 = B_SPLINE_CURVE_WITH_KNOTS ( 'NONE', 3,
 ( #92190, #48557, #81036, #82693, #65363, #108444, #66472, #38476, #57514, #49106, #83240, #40685, #74858, #30069, #64260, #81570, #47992, #100580, #30635, #23862, #64822, #13806, #82130, #94377, #16549, #17657, #7085, #35037, #50739, #84874, #93286, #101121, #67013, #50212, #41241, #75413, #101667, #32824, #24418, #9294, #75942, #103325, #110095, #34492, #8722, #68126, #51289, #85423, #8170, #42339, #368, #109552 ),
 .UNSPECIFIED., .F., .F.,
 ( 4, 2, 2, 1, 1, 1, 2, 2, 2, 2, 1, 2, 2, 2, 2, 2, 2, 2, 2, 2, 1, 2, 2, 2, 2, 1, 2, 2, 4 ),
 ( 0.000000000000000000, 0.06249999999999765465, 0.09375000000000460743, 0.1093750000000183881, 0.1171874999999746036, 0.1210937499998826355, 0.1230468749998226835, 0.1249999999997627453, 0.1874999999982030763, 0.2187499999974809872, 0.2343749999971287690, 0.2421874999970357045, 0.2499999999969426123, 0.3124999999965559216, 0.3437499999963705699, 0.3749999999961852182, 0.4999999999961076136, 0.5624999999960688113, 0.6249999999960300645, 0.6874999999959913177, 0.7187499999960752506, 0.7343749999961173280, 0.7499999999961594055, 0.8124999999965581976, 0.8437499999968343101, 0.8593749999969143571, 0.8671874999970149434, 0.8749999999971155296, 1.000000000000000000 ),
 .UNSPECIFIED. ) ;
#50941 = B_SPLINE_SURFACE_WITH_KNOTS ( 'NONE', 5, 1, ( 
 ( #110172, #68207 ),
 ( #9372, #95032 ),
 ( #26712, #17175 ),
 ( #42981, #35119 ),
 ( #77140, #16627 ),
 ( #60906, #102310 ),
 ( #42414, #69301 ),
 ( #1537, #43535 ),
 ( #77680, #26149 ),
 ( #60338, #93362 ),
 ( #35671, #992 ),
 ( #103977, #51366 ),
 ( #84954, #68751 ),
 ( #102854, #27272 ),
 ( #61456, #95582 ),
 ( #18850, #53047 ),
 ( #50824, #33444 ),
 ( #8246, #67644 ),
 ( #101753, #3761 ),
 ( #62012, #96132 ),
 ( #19410, #45761 ),
 ( #12681, #55260 ),
 ( #89392, #37895 ),
 ( #104535, #105658 ),
 ( #80448, #46319 ),
 ( #37340, #106191 ),
 ( #70415, #27831 ),
 ( #72077, #11585 ),
 ( #20505, #97233 ),
 ( #46861, #38424 ),
 ( #53612, #71537 ),
 ( #2656, #11036 ),
 ( #79344, #63665 ),
 ( #28943, #29473 ),
 ( #97779, #105091 ),
 ( #72599, #12126 ),
 ( #54714, #45203 ),
 ( #55814, #62583 ),
 ( #106728, #30018 ),
 ( #88841, #89931 ),
 ( #21055, #21609 ),
 ( #13208, #80991 ),
 ( #19971, #4297 ),
 ( #64209, #87754 ),
 ( #98332, #78788 ),
 ( #2102, #63132 ),
 ( #36230, #36783 ),
 ( #70976, #28381 ),
 ( #96700, #54165 ),
 ( #88290, #79898 ),
 ( #3211, #22700 ) ),
 .UNSPECIFIED., .F., .F., .F.,
 ( 6, 3, 3, 3, 3, 3, 3, 3, 3, 3, 3, 3, 3, 3, 3, 3, 6 ),
 ( 2, 2 ),
 ( 0.000000000000000000, 28.69702819429999963, 61.04778752440000034, 93.62768910810000023, 123.7336603250000024, 156.1762685979999787, 187.3272846180000215, 220.4669312460000015, 237.3878297990000021, 254.2938300590000154, 289.2398204710000300, 325.3030936050000150, 360.8626869010000178, 395.8828220460000011, 432.6128460950000090, 468.8934854820000169, 502.1482307969999965 ),
 ( -8.108887887879349314E-05, 2.001700839520000219 ),
 .UNSPECIFIED. ) ;
#50942 = CARTESIAN_POINT ( 'NONE',  ( -10.10234689610000203, 1389.151301037549956, 201.8686386834390305 ) ) ;
#50943 = CARTESIAN_POINT ( 'NONE',  ( -16.36456115631862929, 1517.151704408390060, 220.0929384032941698 ) ) ;
#50944 = CARTESIAN_POINT ( 'NONE',  ( 1.632599499710808422, 1421.481676329297898, 193.8011752862853712 ) ) ;
#50945 = DIRECTION ( 'NONE',  ( -0.7071067811865475727, 0.000000000000000000, 0.7071067811865475727 ) ) ;
#50946 = CARTESIAN_POINT ( 'NONE',  ( -33.42844755917204225, 1501.977400791986611, 196.1165140606796058 ) ) ;
#50947 = CARTESIAN_POINT ( 'NONE',  ( -8.874427328269188564, 1384.581418649760053, 218.6695361999740044 ) ) ;
#50948 = CARTESIAN_POINT ( 'NONE',  ( 11.87901658470000044, 1433.117702068830113, 149.9761015577979890 ) ) ;
#50949 = CARTESIAN_POINT ( 'NONE',  ( 3.330669073880000148E-16, 1453.913060387330006, 209.1218459616979999 ) ) ;
#50950 = B_SPLINE_SURFACE_WITH_KNOTS ( 'NONE', 5, 5, ( 
 ( #110281, #77255, #94029, #24596, #34679, #68867, #76684, #15103, #23516 ),
 ( #67203, #67752, #49294, #50404, #49425, #57708, #6718, #49846, #40874 ),
 ( #59360, #101862, #25707, #101302, #17293, #58789, #7818, #41988, #75051 ),
 ( #25156, #92928, #93468, #100760, #51488, #76137, #24051, #58245, #68317 ),
 ( #92367, #83976, #85071, #102425, #7276, #85619, #41441, #75606, #109736 ),
 ( #88399, #2767, #27942, #2220, #105206, #35792, #28494, #69976, #87300 ),
 ( #45865, #52052, #36334, #9479, #86187, #18407, #45318, #96250, #17850 ),
 ( #79457, #96810, #3322, #43643, #19524, #36887, #79998, #62123, #26835 ),
 ( #18964, #61563, #37447, #53730, #26268, #1656, #95147, #102970, #69421 ),
 ( #104645, #60458, #10033, #11158, #103534, #44203, #10593, #53159, #104092 ),
 ( #87868, #70528, #27384, #35233, #71081, #61023, #95697, #94575, #62686 ),
 ( #86741, #77796, #52605, #1105, #44763, #78915, #78347, #20080, #54274 ) ),
 .UNSPECIFIED., .F., .F., .F.,
 ( 6, 3, 3, 6 ),
 ( 6, 3, 6 ),
 ( 0.000000000000000000, 17.84603210599999912, 40.51038747020000130, 67.03953034199999195 ),
 ( 84.36360870500000431, 126.5454130579999941, 168.7272174100000086 ),
 .UNSPECIFIED. ) ;
#50951 = CARTESIAN_POINT ( 'NONE',  ( -11.04008170774799957, 1462.385341758290224, 208.9869242049449838 ) ) ;
#50952 = CARTESIAN_POINT ( 'NONE',  ( -16.95945306273139863, 1420.347400483130059, 203.7374467786609955 ) ) ;
#50953 = CARTESIAN_POINT ( 'NONE',  ( 12.67647370521179973, 1426.478948021449924, 202.7078733498550207 ) ) ;
#50954 = CARTESIAN_POINT ( 'NONE',  ( -15.06279948716559680, 1422.388304403035136, 229.4662111949969301 ) ) ;
#50955 = PLANE ( 'NONE',  #28136 ) ;
#50956 = CARTESIAN_POINT ( 'NONE',  ( -14.16989796120989986, 1420.440730658529901, 227.4201728071160176 ) ) ;
#50957 = CARTESIAN_POINT ( 'NONE',  ( -29.87022976070419844, 1509.969119424489918, 208.7889112562570233 ) ) ;
#50958 = CARTESIAN_POINT ( 'NONE',  ( 24.30946323610000093, 1430.356462477430114, 212.0522589108380203 ) ) ;
#50959 = CARTESIAN_POINT ( 'NONE',  ( -0.7008159675984454440, 1477.501393641809045, 198.7433666631080769 ) ) ;
#50960 = CARTESIAN_POINT ( 'NONE',  ( -8.991592997889998884, 1509.227053733729917, 237.0094774837980083 ) ) ;
#50961 = CARTESIAN_POINT ( 'NONE',  ( 3.353036578218081321, 1508.146033441647660, 220.1520117934527150 ) ) ;
#50962 = CARTESIAN_POINT ( 'NONE',  ( 31.41104781486823327, 1512.187213306747481, 215.9140555522422460 ) ) ;
#50963 = CARTESIAN_POINT ( 'NONE',  ( -4.354856832958300394, 1481.954697149059939, 231.1149924593809999 ) ) ;
#50964 = CARTESIAN_POINT ( 'NONE',  ( 0.7568986996720019622, 1516.805675336850072, 213.1530147380969993 ) ) ;
#50965 = CARTESIAN_POINT ( 'NONE',  ( -14.57368822342009906, 1420.954711568789889, 207.9848542621210186 ) ) ;
#50966 = CARTESIAN_POINT ( 'NONE',  ( 0.1784803411008450136, 1475.371066012589836, 182.2932093119499939 ) ) ;
#50968 = EDGE_LOOP ( 'NONE', ( #39569, #95234, #14660, #101662, #11399, #14999 ) ) ;
#50967 = CARTESIAN_POINT ( 'NONE',  ( -5.680073728562159197, 1408.055878260910049, 221.5454655010989882 ) ) ;
#50969 = CARTESIAN_POINT ( 'NONE',  ( -20.82705473220000059, 1444.994950788469851, 176.6587301488980017 ) ) ;
#50970 = CARTESIAN_POINT ( 'NONE',  ( -38.13546499650039578, 1444.994950788468714, 136.8609531837178963 ) ) ;
#50971 = CARTESIAN_POINT ( 'NONE',  ( 11.87502393270000134, 1433.007271228389982, 149.9804723947979994 ) ) ;
#50972 = CARTESIAN_POINT ( 'NONE',  ( -39.48448845344529445, 1449.205409213619987, 134.0999999980729740 ) ) ;
#50973 = CARTESIAN_POINT ( 'NONE',  ( -110.0630399400000101, 1384.905426682000098, 296.9512818274590131 ) ) ;
#50974 = ORIENTED_EDGE ( 'NONE', *, *, #76076, .T. ) ;
#50975 = CARTESIAN_POINT ( 'NONE',  ( -13.15726448929999925, 1416.913060387330006, 219.9105610086979823 ) ) ;
#50976 = AXIS2_PLACEMENT_3D ( 'NONE', #70773, #10262, #36575 ) ;
#50977 = DIRECTION ( 'NONE',  ( 0.000000000000000000, 0.000000000000000000, 1.000000000000000000 ) ) ;
#50978 = CARTESIAN_POINT ( 'NONE',  ( -15.65413333740000112, 1416.520322351130062, 219.1909222911980066 ) ) ;
#50979 = DIRECTION ( 'NONE',  ( 0.01594118961724027769, -0.9969860201949399814, 0.07592597717146752634 ) ) ;
#50980 = B_SPLINE_CURVE_WITH_KNOTS ( 'NONE', 3,
 ( #76787, #68966, #103641, #85176, #86284, #44302, #70623, #44866, #85726, #79017, #70079, #95241, #69521, #61665, #103068, #95789, #26369, #43741, #52151 ),
 .UNSPECIFIED., .F., .F.,
 ( 4, 2, 2, 2, 1, 1, 1, 2, 2, 2, 4 ),
 ( 0.000000000000000000, 0.2500000000076687545, 0.3750000000115031318, 0.4375000000133325018, 0.4687500000142481582, 0.4843750000146268553, 0.4921875000148150936, 0.4960937500148319690, 0.5000000000148488999, 0.7500000000074245055, 1.000000000000000000 ),
 .UNSPECIFIED. ) ;
#50981 = CARTESIAN_POINT ( 'NONE',  ( -4.782325726783580144, 1433.817978782009959, 216.6757878527850210 ) ) ;
#50982 = CARTESIAN_POINT ( 'NONE',  ( -108.4664300161794586, 1381.328991949513011, 310.3998206309821057 ) ) ;
#50983 = CARTESIAN_POINT ( 'NONE',  ( -15.64027221210000107, 1419.286982173109891, 210.8948112567390183 ) ) ;
#50984 = LINE ( 'NONE', #103576, #16366 ) ;
#50985 = CARTESIAN_POINT ( 'NONE',  ( -11.90322536250000063, 1391.913060490810039, 209.2366397656629999 ) ) ;
#50986 = CARTESIAN_POINT ( 'NONE',  ( -77.18387175459460536, 1385.145919355859860, 279.0577792721099968 ) ) ;
#50987 = CARTESIAN_POINT ( 'NONE',  ( -11.13475278476130015, 1391.913060387289988, 212.1805052186929856 ) ) ;
#50988 = CARTESIAN_POINT ( 'NONE',  ( 10.78765558695330107, 1422.957222186570107, 207.1808645241220290 ) ) ;
#50989 = VERTEX_POINT ( 'NONE', #70677 ) ;
#50990 = CARTESIAN_POINT ( 'NONE',  ( -32.05911371000000543, 1451.793557196030179, 134.7701858639979946 ) ) ;
#50991 = CARTESIAN_POINT ( 'NONE',  ( -15.70046566381129871, 1410.429479579480130, 226.6601106372359880 ) ) ;
#50993 = ORIENTED_EDGE ( 'NONE', *, *, #17536, .F. ) ;
#50992 = CARTESIAN_POINT ( 'NONE',  ( 3.005276066430000448, 1369.205039411269809, 210.6218459616989946 ) ) ;
#50994 = CARTESIAN_POINT ( 'NONE',  ( 1.742415919699999982, 1474.343050966390138, 219.6228429884990305 ) ) ;
#50995 = CARTESIAN_POINT ( 'NONE',  ( 27.04494143110000337, 1509.634156398229834, 216.9800077211579890 ) ) ;
#50996 = CARTESIAN_POINT ( 'NONE',  ( -8.082564370853681623, 1362.241991287382007, 210.6218459616987957 ) ) ;
#50997 = CARTESIAN_POINT ( 'NONE',  ( -7.648516765129999229, 1495.666136353089996, 200.8684719025990262 ) ) ;
#50998 = CARTESIAN_POINT ( 'NONE',  ( -5.389719915088219793, 1440.971386074470047, 154.8246291213590098 ) ) ;
#50999 = DIRECTION ( 'NONE',  ( -0.9942586961433751425, 0.000000000000000000, 0.1070030146457376097 ) ) ;
#51000 = CARTESIAN_POINT ( 'NONE',  ( 14.92518454057932331, 1430.567503116120179, 220.1855779226771404 ) ) ;
#51001 = CARTESIAN_POINT ( 'NONE',  ( -7.012921688925192854, 1508.551704408389696, 215.5137845987784146 ) ) ;
#51002 = CARTESIAN_POINT ( 'NONE',  ( 8.347715551000000289, 1448.434209623990000, 205.2198596814789937 ) ) ;
#51003 = CARTESIAN_POINT ( 'NONE',  ( -120.4392612185272213, 1309.112692017090239, 300.3762800269232116 ) ) ;
#51004 = CARTESIAN_POINT ( 'NONE',  ( -4.780260440829766644, 1370.125810961987781, 210.6218459617030021 ) ) ;
#51005 = CARTESIAN_POINT ( 'NONE',  ( -3.201474586160000246, 1454.788669850390079, 199.8827619061390237 ) ) ;
#51006 = CARTESIAN_POINT ( 'NONE',  ( 0.7353365397730019515, 1516.995911393979895, 206.2425275143270085 ) ) ;
#51007 = CARTESIAN_POINT ( 'NONE',  ( 3.133278283570000156, 1446.922686756950043, 159.4826872549980123 ) ) ;
#51008 = CARTESIAN_POINT ( 'NONE',  ( -31.99468309217327189, 1524.860077346005255, 216.1184527756807370 ) ) ;
#51009 = CARTESIAN_POINT ( 'NONE',  ( -1.966612674429999652, 1496.552542902290043, 197.6618318493989932 ) ) ;
#51011 = ORIENTED_EDGE ( 'NONE', *, *, #88612, .T. ) ;
#51010 = FACE_OUTER_BOUND ( 'NONE', #40717, .T. ) ;
#51012 = DIRECTION ( 'NONE',  ( 0.000000000000000000, 0.000000000000000000, 1.000000000000000000 ) ) ;
#51013 = EDGE_LOOP ( 'NONE', ( #25033, #92826, #53093, #9298 ) ) ;
#51014 = CARTESIAN_POINT ( 'NONE',  ( -16.25466705341527529, 1514.562529184129517, 223.9116621936409217 ) ) ;
#51015 = CARTESIAN_POINT ( 'NONE',  ( -19.39159332910000089, 1430.347784943829993, 195.6539361813979951 ) ) ;
#51018 = CARTESIAN_POINT ( 'NONE',  ( 16.57071976326540153, 1410.582081926380170, 191.7433702585070137 ) ) ;
#51017 = AXIS2_PLACEMENT_3D ( 'NONE', #81954, #99852, #49486 ) ;
#51016 = CARTESIAN_POINT ( 'NONE',  ( -11.19642886898100009, 1425.622699824140227, 127.8389159192909972 ) ) ;
#51019 = CARTESIAN_POINT ( 'NONE',  ( 7.338753830235000386, 1517.184383877180153, 211.4127322367170052 ) ) ;
#51020 = CARTESIAN_POINT ( 'NONE',  ( 27.92935577517391721, 1510.000134406965572, 220.0760090323809379 ) ) ;
#51021 = CARTESIAN_POINT ( 'NONE',  ( 2.030980132853136944, 1450.182268141366194, 181.9754583269210855 ) ) ;
#51022 = CARTESIAN_POINT ( 'NONE',  ( 19.25251418436180018, 1509.610172285510089, 231.6560777679470107 ) ) ;
#51024 = ADVANCED_FACE ( 'NONE', ( #692 ), #1980, .F. ) ;
#51023 = CARTESIAN_POINT ( 'NONE',  ( 8.013639455417655100, 1465.494642556247300, 233.0458548789991937 ) ) ;
#51025 = CARTESIAN_POINT ( 'NONE',  ( 4.174962612117290028, 1508.551704408389924, 213.4548848115649946 ) ) ;
#51026 = CARTESIAN_POINT ( 'NONE',  ( -36.55889210262929367, 1437.673941850749770, 136.5464336263889891 ) ) ;
#51027 = ORIENTED_EDGE ( 'NONE', *, *, #6667, .F. ) ;
#51028 = CARTESIAN_POINT ( 'NONE',  ( 6.881122077359999700, 1396.213462846930042, 198.7274638095979924 ) ) ;
#51029 = CARTESIAN_POINT ( 'NONE',  ( 9.778911541403340735, 1461.615419081409982, 207.8750183380009844 ) ) ;
#51030 = EDGE_CURVE ( 'NONE', #35724, #47452, #32404, .T. ) ;
#51031 = CARTESIAN_POINT ( 'NONE',  ( -16.13006593319999737, 1459.079424064530031, 230.3616556409980092 ) ) ;
#51032 = ORIENTED_EDGE ( 'NONE', *, *, #78217, .F. ) ;
#51033 = VERTEX_POINT ( 'NONE', #61713 ) ;
#51034 = CARTESIAN_POINT ( 'NONE',  ( -1.090665124220995930, 1370.067406900570404, 211.2860174477949613 ) ) ;
#51035 = CARTESIAN_POINT ( 'NONE',  ( 14.79248454883459907, 1496.752653259379940, 226.0610261129200182 ) ) ;
#51036 = EDGE_CURVE ( 'NONE', #17035, #66323, #104239, .T. ) ;
#51037 = LINE ( 'NONE', #60001, #22315 ) ;
#51038 = B_SPLINE_CURVE_WITH_KNOTS ( 'NONE', 5,
 ( #89892, #96657, #79859, #97744, #89348, #71495, #11546, #46278, #28898 ),
 .UNSPECIFIED., .F., .F.,
 ( 6, 3, 6 ),
 ( 0.000000000000000000, 0.4258971877630836622, 1.000000000000000000 ),
 .UNSPECIFIED. ) ;
#51039 = CARTESIAN_POINT ( 'NONE',  ( -10.84387077669929589, 1417.968182827059536, 198.1845410755198600 ) ) ;
#51040 = CARTESIAN_POINT ( 'NONE',  ( 2.330134122034449806, 1515.551704408389924, 205.2922258479440245 ) ) ;
#51041 = CARTESIAN_POINT ( 'NONE',  ( -6.092591263813240232, 1454.342283619849923, 201.9713694523269965 ) ) ;
#51042 = ADVANCED_FACE ( 'NONE', ( #1805 ), #105717, .F. ) ;
#51043 = CARTESIAN_POINT ( 'NONE',  ( -15.88507158550000042, 1470.477701853530107, 228.8906323047980038 ) ) ;
#51044 = CARTESIAN_POINT ( 'NONE',  ( -9.123736379228210680, 1384.508619151900120, 199.9712811155520171 ) ) ;
#51045 = AXIS2_PLACEMENT_3D ( 'NONE', #43526, #95021, #94443 ) ;
#51046 = CARTESIAN_POINT ( 'NONE',  ( -12.27558643790000126, 1391.355947405540064, 211.6931146936589982 ) ) ;
#51047 = CARTESIAN_POINT ( 'NONE',  ( -93.07309726766789026, 1384.850428360820160, 294.1733350510500031 ) ) ;
#51048 = VERTEX_POINT ( 'NONE', #35377 ) ;
#51049 =( BOUNDED_CURVE ( )  B_SPLINE_CURVE ( 3, ( #20648, #70561, #104678, #54850 ),
 .UNSPECIFIED., .F., .T. ) 
 B_SPLINE_CURVE_WITH_KNOTS ( ( 4, 4 ),
 ( 6.150868878552831376, 6.164145497763507286 ),
 .UNSPECIFIED. ) 
 CURVE ( )  GEOMETRIC_REPRESENTATION_ITEM ( )  RATIONAL_B_SPLINE_CURVE ( ( 1.000000000000000000, 0.9999853110024699010, 0.9999853110024699010, 1.000000000000000000 ) ) 
 REPRESENTATION_ITEM ( '' )  );
#51050 = CARTESIAN_POINT ( 'NONE',  ( 7.716252052974999387, 1516.810037859429940, 202.1795012402670011 ) ) ;
#51051 = CARTESIAN_POINT ( 'NONE',  ( 2.292217010694999946, 1516.941178807709775, 209.1086494233340147 ) ) ;
#51052 = VERTEX_POINT ( 'NONE', #51636 ) ;
#51053 = CARTESIAN_POINT ( 'NONE',  ( 11.73709356406289928, 1426.695943121369965, 144.1748013758129900 ) ) ;
#51054 = B_SPLINE_CURVE_WITH_KNOTS ( 'NONE', 3,
 ( #1544, #44093, #9922, #51939, #85508, #52499, #77146, #86083, #53617, #93914, #61461, #9377, #8805, #53052, #18856, #77685, #60911, #78231, #87190, #450, #70422, #42987, #68756, #998, #95039, #25602, #59794, #2109 ),
 .UNSPECIFIED., .F., .F.,
 ( 4, 3, 3, 3, 3, 3, 3, 3, 3, 4 ),
 ( -7.293785117949999730, -7.169388331878350229, -6.566796097046200487, -5.839807076142389697, -5.147073161146510145, -4.739076892086050208, -4.240156153919569348, -3.759358294541570000, -3.363905596364519912, -3.000356897310000548 ),
 .UNSPECIFIED. ) ;
#51055 = CARTESIAN_POINT ( 'NONE',  ( 19.13278187119999885, 1487.527101359029984, 228.6867874049980003 ) ) ;
#51056 = EDGE_LOOP ( 'NONE', ( #69511, #33128, #16406, #30776, #43085 ) ) ;
#51057 = CARTESIAN_POINT ( 'NONE',  ( -13.58235846979999906, 1416.828040475229955, 221.9087530951979659 ) ) ;
#51058 = CARTESIAN_POINT ( 'NONE',  ( 5.009886284249999377, 1430.069699660889910, 217.1776678749689893 ) ) ;
#51059 = CARTESIAN_POINT ( 'NONE',  ( -18.74729292449999818, 1442.199705176290081, 209.1218459616989946 ) ) ;
#51060 = AXIS2_PLACEMENT_3D ( 'NONE', #66216, #101968, #25254 ) ;
#51061 = CARTESIAN_POINT ( 'NONE',  ( -3.701332510601603953, 1488.791807424273657, 219.3688952161021746 ) ) ;
#51062 = CARTESIAN_POINT ( 'NONE',  ( -4.747361959010000021, 1423.750432747230207, 185.1131762002980281 ) ) ;
#51063 = CARTESIAN_POINT ( 'NONE',  ( -7.842556662604346585, 1446.693600393765337, 154.0804530413156215 ) ) ;
#51064 = CARTESIAN_POINT ( 'NONE',  ( -0.1613635196969999963, 1507.107001830130002, 180.9028739243980226 ) ) ;
#51065 = CARTESIAN_POINT ( 'NONE',  ( 6.291724964230139605, 1441.035272546479973, 154.5485623116409784 ) ) ;
#51066 = CARTESIAN_POINT ( 'NONE',  ( -51.76145802239999938, 1379.744278086280019, 243.7243931585590246 ) ) ;
#51067 = CARTESIAN_POINT ( 'NONE',  ( -7.012921583605000286, 1509.051704408389924, 209.1218459511669892 ) ) ;
#51069 = CARTESIAN_POINT ( 'NONE',  ( 8.358086347145718520, 1468.256939908329969, 201.6625126024160295 ) ) ;
#51068 = CARTESIAN_POINT ( 'NONE',  ( -3.644795242719999884, 1497.323677685689972, 198.4600586451990125 ) ) ;
#51070 = CARTESIAN_POINT ( 'NONE',  ( -5.027042350745985821, 1422.871757580189978, 184.8364420396860339 ) ) ;
#51071 = B_SPLINE_SURFACE_WITH_KNOTS ( 'NONE', 5, 1, ( 
 ( #4077, #103764 ),
 ( #44423, #27066 ),
 ( #61251, #45542 ),
 ( #44984, #78565 ),
 ( #1881, #62917 ),
 ( #53379, #28153 ) ),
 .UNSPECIFIED., .F., .F., .F.,
 ( 6, 6 ),
 ( 2, 2 ),
 ( -1.032047596522180116E-05, 16.54785843137600310 ),
 ( 0.000000000000000000, 14.00001032047599914 ),
 .UNSPECIFIED. ) ;
#51073 = EDGE_CURVE ( 'NONE', #68277, #68290, #16225, .T. ) ;
#51072 = EDGE_CURVE ( 'NONE', #84410, #76626, #88013, .T. ) ;
#51074 = CARTESIAN_POINT ( 'NONE',  ( -7.910413875049510324, 1499.455618961650089, 212.0002310091700224 ) ) ;
#51075 = ORIENTED_EDGE ( 'NONE', *, *, #83599, .T. ) ;
#51076 = CARTESIAN_POINT ( 'NONE',  ( 12.39573405564623165, 1522.051704408389924, 218.5685989363918225 ) ) ;
#51077 = CARTESIAN_POINT ( 'NONE',  ( -21.26059330700258343, 1525.055427061272212, 233.8824087493117929 ) ) ;
#51078 = CARTESIAN_POINT ( 'NONE',  ( -2.899134383046004348, 1484.388260718141055, 183.3068692522237200 ) ) ;
#51079 = ADVANCED_FACE ( 'NONE', ( #105345 ), #18007, .F. ) ;
#51080 = CARTESIAN_POINT ( 'NONE',  ( -14.30113686340000179, 1415.739699861750069, 214.3509892272290074 ) ) ;
#51082 = ORIENTED_EDGE ( 'NONE', *, *, #28345, .F. ) ;
#51081 = CARTESIAN_POINT ( 'NONE',  ( 4.802232110086869454, 1508.551704408389924, 213.5516190689590132 ) ) ;
#51083 = CARTESIAN_POINT ( 'NONE',  ( 1.546867496849999801, 1416.839692139930094, 190.2222514364979986 ) ) ;
#51084 = CYLINDRICAL_SURFACE ( 'NONE', #29847, 1.999999999999995781 ) ;
#51085 = CARTESIAN_POINT ( 'NONE',  ( -11.19300148449999988, 1425.653304015530011, 147.1770035940979824 ) ) ;
#51086 = CARTESIAN_POINT ( 'NONE',  ( 4.026786250540000722, 1415.442497638829991, 163.1427597075980032 ) ) ;
#51087 = B_SPLINE_CURVE_WITH_KNOTS ( 'NONE', 5,
 ( #91908, #90808, #98658, #82962, #15185, #24134 ),
 .UNSPECIFIED., .F., .F.,
 ( 6, 6 ),
 ( 0.000000000000000000, 1.000000000000000000 ),
 .UNSPECIFIED. ) ;
#51088 = CARTESIAN_POINT ( 'NONE',  ( -7.352292206439999589, 1441.815725582649975, 185.3605977109980074 ) ) ;
#51089 = DIRECTION ( 'NONE',  ( -0.9455185755993178454, 0.000000000000000000, 0.3255681544571539243 ) ) ;
#51090 = CARTESIAN_POINT ( 'NONE',  ( 21.13068363900000080, 1496.786787671390130, 208.1084808827089887 ) ) ;
#51091 = FACE_OUTER_BOUND ( 'NONE', #29666, .T. ) ;
#51093 = CARTESIAN_POINT ( 'NONE',  ( -9.366078551730000257, 1478.880934751289942, 214.2941079828090096 ) ) ;
#51092 = CARTESIAN_POINT ( 'NONE',  ( -21.82073367870000169, 1482.726029602730023, 224.2880922674980013 ) ) ;
#51094 = CARTESIAN_POINT ( 'NONE',  ( -2.472529913803022783, 1523.678648413191695, 242.8674788698241400 ) ) ;
#51095 = ORIENTED_EDGE ( 'NONE', *, *, #50256, .T. ) ;
#51096 = CARTESIAN_POINT ( 'NONE',  ( 2.865588684285000021, 1516.890356958860139, 205.8536102114670143 ) ) ;
#51097 = CARTESIAN_POINT ( 'NONE',  ( 23.62346383279999884, 1410.898849078630064, 268.8227235180979733 ) ) ;
#51098 = CARTESIAN_POINT ( 'NONE',  ( -19.37374569213905318, 1526.382868172863937, 234.3668155954421479 ) ) ;
#51099 = CARTESIAN_POINT ( 'NONE',  ( 20.08216459950000043, 1449.729590668439869, 193.7700040052980057 ) ) ;
#51100 = CARTESIAN_POINT ( 'NONE',  ( 10.70848634212536865, 1506.855035729306792, 228.7236287190453936 ) ) ;
#51101 = AXIS2_PLACEMENT_3D ( 'NONE', #5282, #58455, #100979 ) ;
#51102 = CARTESIAN_POINT ( 'NONE',  ( 1.439473459159019919, 1454.776503338229986, 218.4216800315260230 ) ) ;
#51103 = CARTESIAN_POINT ( 'NONE',  ( -41.53485087296149914, 1442.119024217849983, 135.5124738229289960 ) ) ;
#51104 = CARTESIAN_POINT ( 'NONE',  ( 12.63038619288439968, 1428.207532477410041, 223.9332333053530135 ) ) ;
#51105 = CARTESIAN_POINT ( 'NONE',  ( -14.50510915870000161, 1416.687742578199959, 203.9073860009089856 ) ) ;
#51106 = CARTESIAN_POINT ( 'NONE',  ( -14.16826824910000049, 1443.187051346489852, 188.6845770635979704 ) ) ;
#51107 = CARTESIAN_POINT ( 'NONE',  ( -4.159019969402780070, 1485.181217399250045, 197.9706610134819869 ) ) ;
#51108 = B_SPLINE_SURFACE_WITH_KNOTS ( 'NONE', 5, 1, ( 
 ( #29110, #36947 ),
 ( #71145, #63296 ),
 ( #21776, #81157 ),
 ( #29652, #88471 ),
 ( #30195, #79525 ),
 ( #98508, #63839 ),
 ( #97951, #54881 ),
 ( #3935, #11755 ),
 ( #80061, #96875 ) ),
 .UNSPECIFIED., .F., .F., .F.,
 ( 6, 3, 6 ),
 ( 2, 2 ),
 ( -3.570158630500980045E-05, 8.847362025080000691, 17.72538832238630135 ),
 ( 0.000000000000000000, 14.00003570158630062 ),
 .UNSPECIFIED. ) ;
#51109 = CARTESIAN_POINT ( 'NONE',  ( -16.09212348995429664, 1419.771771290114657, 210.1905430961424486 ) ) ;
#51110 = CARTESIAN_POINT ( 'NONE',  ( -9.930122423809999432, 1499.782504084789934, 217.2571562510489969 ) ) ;
#51111 = ORIENTED_EDGE ( 'NONE', *, *, #44567, .F. ) ;
#51112 = CARTESIAN_POINT ( 'NONE',  ( 1.451959685182149906, 1503.840107181440089, 181.2560994760340236 ) ) ;
#51113 = CARTESIAN_POINT ( 'NONE',  ( -13.81911144855440021, 1409.395634392820057, 214.7971903334679951 ) ) ;
#51114 = CARTESIAN_POINT ( 'NONE',  ( 10.56762249884929972, 1481.680206704629882, 209.7477003755120109 ) ) ;
#51115 = CARTESIAN_POINT ( 'NONE',  ( -12.08843586217701827, 1377.632273357547774, 211.4485156452657861 ) ) ;
#51116 = CARTESIAN_POINT ( 'NONE',  ( -12.73087921850000015, 1474.751530140129944, 268.4159631503979995 ) ) ;
#51117 = CARTESIAN_POINT ( 'NONE',  ( -7.359379718520192348, 1516.577810474467015, 210.5819051629668195 ) ) ;
#51118 = CARTESIAN_POINT ( 'NONE',  ( -13.95544062720738054, 1513.969077476929442, 192.4617105174407072 ) ) ;
#51119 = DIRECTION ( 'NONE',  ( 0.9149707217702551798, 0.000000000000000000, -0.4035202328300510621 ) ) ;
#51120 = CARTESIAN_POINT ( 'NONE',  ( -72.47816579847129503, 1384.655904266999869, 297.6885493325589778 ) ) ;
#51121 = CYLINDRICAL_SURFACE ( 'NONE', #69698, 1.999999999999913181 ) ;
#51122 = CARTESIAN_POINT ( 'NONE',  ( 12.11709951209460101, 1416.029511585410091, 223.4307279390160090 ) ) ;
#51123 = FACE_OUTER_BOUND ( 'NONE', #50898, .T. ) ;
#51124 = CARTESIAN_POINT ( 'NONE',  ( -15.46337563405010052, 1415.677402202039957, 209.5778891453549875 ) ) ;
#51125 = CIRCLE ( 'NONE', #2858, 3.000000000000002665 ) ;
#51126 = CARTESIAN_POINT ( 'NONE',  ( -23.56691185029999858, 1411.096426580230172, 206.5756125875680027 ) ) ;
#51127 = CARTESIAN_POINT ( 'NONE',  ( -10.29023455615431537, 1379.884657259707410, 202.2562532116602085 ) ) ;
#51128 = CARTESIAN_POINT ( 'NONE',  ( 4.957343604469999221, 1484.564563689889837, 219.0507238675290012 ) ) ;
#51129 = CARTESIAN_POINT ( 'NONE',  ( 3.855903970259999980, 1423.712488786839913, 193.3614856424989910 ) ) ;
#51130 = CARTESIAN_POINT ( 'NONE',  ( -4.367411321880000158E-15, 1433.447543843880112, 150.4377610267980003 ) ) ;
#51131 = CARTESIAN_POINT ( 'NONE',  ( -19.86496342331569664, 1441.826159015929989, 212.7408786141659789 ) ) ;
#51132 = FACE_OUTER_BOUND ( 'NONE', #106089, .T. ) ;
#51133 = AXIS2_PLACEMENT_3D ( 'NONE', #8763, #61976, #42944 ) ;
#51134 = CARTESIAN_POINT ( 'NONE',  ( -18.92738905877370215, 1503.346139544750031, 222.1981867165029882 ) ) ;
#51136 = CARTESIAN_POINT ( 'NONE',  ( -11.00370989719999848, 1381.644652005500120, 201.9116486243489987 ) ) ;
#51135 = CARTESIAN_POINT ( 'NONE',  ( -16.60706435110729728, 1417.159713941199925, 208.4134677303929948 ) ) ;
#51137 = CARTESIAN_POINT ( 'NONE',  ( 11.73572286974009948, 1426.696804897310130, 144.0764963122049949 ) ) ;
#51138 = DIRECTION ( 'NONE',  ( -0.6736849260863837507, 0.000000000000000000, 0.7390186874254154326 ) ) ;
#51139 = CARTESIAN_POINT ( 'NONE',  ( -19.15298488520000220, 1464.559837765089924, 213.8319524061190009 ) ) ;
#51140 = CARTESIAN_POINT ( 'NONE',  ( 4.850088428599620194, 1447.195166418000099, 200.1568079554039912 ) ) ;
#51141 = CARTESIAN_POINT ( 'NONE',  ( 3.007752987394139908E-09, 1406.911841295280055, 222.1218459617980159 ) ) ;
#51142 = CARTESIAN_POINT ( 'NONE',  ( 6.937965660314999283, 1516.732530461250008, 204.1161457306970135 ) ) ;
#51143 = CARTESIAN_POINT ( 'NONE',  ( -8.235420378752696280, 1398.157615904283375, 219.1813604885521727 ) ) ;
#51144 = CARTESIAN_POINT ( 'NONE',  ( 14.72577131403500061, 1514.214451716350140, 194.1036979393670094 ) ) ;
#51145 = FACE_BOUND ( 'NONE', #87153, .T. ) ;
#51146 = CARTESIAN_POINT ( 'NONE',  ( 10.51435689538379847, 1503.261304779379998, 214.3454426394149834 ) ) ;
#51148 = VERTEX_POINT ( 'NONE', #19102 ) ;
#51147 = CARTESIAN_POINT ( 'NONE',  ( -56.86315681117869758, 1379.712756814529939, 259.5172876196859875 ) ) ;
#51149 = ORIENTED_EDGE ( 'NONE', *, *, #87176, .F. ) ;
#51150 = CARTESIAN_POINT ( 'NONE',  ( 12.01841008247880005, 1433.726417607980011, 149.8316427203229750 ) ) ;
#51151 = CARTESIAN_POINT ( 'NONE',  ( 21.46337646344914774, 1524.972613296804866, 183.7396512953049807 ) ) ;
#51152 = EDGE_LOOP ( 'NONE', ( #33509, #110372, #90621 ) ) ;
#51153 = CARTESIAN_POINT ( 'NONE',  ( -107.0879710039999964, 1379.224539023319949, 308.6385636590589456 ) ) ;
#51154 = CARTESIAN_POINT ( 'NONE',  ( -10.25711658408749827, 1448.721523702089826, 207.5095412171060332 ) ) ;
#51155 = CARTESIAN_POINT ( 'NONE',  ( 2.936816566051839938, 1515.374151772610048, 204.8620682733370018 ) ) ;
#51157 = FACE_OUTER_BOUND ( 'NONE', #99246, .T. ) ;
#51156 = CARTESIAN_POINT ( 'NONE',  ( -0.9161538208349989665, 1443.103178644890022, 200.2678594588790020 ) ) ;
#51158 = CARTESIAN_POINT ( 'NONE',  ( 17.62013664171889715, 1498.112312558009990, 230.2633706911829847 ) ) ;
#51159 = CARTESIAN_POINT ( 'NONE',  ( 0.3783643747870000240, 1468.710133949630062, 182.5713305459979949 ) ) ;
#51160 = CARTESIAN_POINT ( 'NONE',  ( 0.8760155196429990632, 1467.778340247989945, 219.4697915747989896 ) ) ;
#51161 = CARTESIAN_POINT ( 'NONE',  ( 15.14118775829999919, 1409.441802315629957, 226.2727750917980245 ) ) ;
#51162 = CARTESIAN_POINT ( 'NONE',  ( 0.1334653011508349918, 1395.917721098340053, 198.1212205003539850 ) ) ;
#51163 = CARTESIAN_POINT ( 'NONE',  ( 14.06293010156799994, 1415.542389211330146, 197.2558749039930035 ) ) ;
#51164 = CARTESIAN_POINT ( 'NONE',  ( 10.96395513279999889, 1431.947606384360142, 151.7599316184980296 ) ) ;
#51165 = CARTESIAN_POINT ( 'NONE',  ( 5.277460848200000498, 1426.742654866309977, 191.8370381630989812 ) ) ;
#51166 = ORIENTED_EDGE ( 'NONE', *, *, #48707, .T. ) ;
#51167 = CARTESIAN_POINT ( 'NONE',  ( 14.13823592991809974, 1436.109943510260109, 150.1180615443350064 ) ) ;
#51168 = EDGE_LOOP ( 'NONE', ( #103636, #34338, #70198, #25013 ) ) ;
#51169 = ORIENTED_EDGE ( 'NONE', *, *, #95112, .F. ) ;
#51170 = CARTESIAN_POINT ( 'NONE',  ( 13.51610093808350221, 1443.927065517340907, 169.3501091255430424 ) ) ;
#51171 = CARTESIAN_POINT ( 'NONE',  ( -12.81329301000000065, 1461.300013870830071, 232.2698450468980127 ) ) ;
#51172 = DIRECTION ( 'NONE',  ( -0.02616798426500960631, 0.9993150019883682011, 0.02616798426500960631 ) ) ;
#51173 = CARTESIAN_POINT ( 'NONE',  ( 3.260378255074999565, 1516.582197289609894, 216.8321318079170226 ) ) ;
#51174 = CARTESIAN_POINT ( 'NONE',  ( -8.501621014552872779, 1511.397679221962107, 214.0579325126637968 ) ) ;
#51175 = CARTESIAN_POINT ( 'NONE',  ( -19.08186866826044437, 1442.067311600292442, 210.3913232654338969 ) ) ;
#51176 = DIRECTION ( 'NONE',  ( 0.9900965937346509760, 0.1403878024439500216, 3.790652827686680047E-16 ) ) ;
#51177 = CARTESIAN_POINT ( 'NONE',  ( -1.906499580428539872E-08, 1517.051704408389924, 216.8444262845069943 ) ) ;
#51178 = TOROIDAL_SURFACE ( 'NONE', #72600, 30.13701971169416538, 3.000000000000000000 ) ;
#51179 = EDGE_CURVE ( 'NONE', #27764, #45161, #22589, .T. ) ;
#51180 = CARTESIAN_POINT ( 'NONE',  ( -6.950214971414999887, 1517.129577905929864, 206.2502655435069983 ) ) ;
#51181 = EDGE_LOOP ( 'NONE', ( #103379, #19086, #28725, #86049, #17052, #77500 ) ) ;
#51182 = CARTESIAN_POINT ( 'NONE',  ( -105.5653050470969987, 1378.245869374329914, 304.5467815922049795 ) ) ;
#51183 = CARTESIAN_POINT ( 'NONE',  ( -19.06709057720000189, 1507.978133441429918, 229.6728830551980138 ) ) ;
#51184 = EDGE_CURVE ( 'NONE', #5789, #72142, #94991, .T. ) ;
#51185 = CARTESIAN_POINT ( 'NONE',  ( -7.275747108760000081, 1410.543472109730146, 187.4914510093980198 ) ) ;
#51186 = CARTESIAN_POINT ( 'NONE',  ( 7.496083170734999968, 1513.333000339860064, 215.5119004184770120 ) ) ;
#51188 = VERTEX_POINT ( 'NONE', #17438 ) ;
#51187 = CARTESIAN_POINT ( 'NONE',  ( -0.4068402809140000409, 1415.948532225030021, 227.3221874807980214 ) ) ;
#51189 = CARTESIAN_POINT ( 'NONE',  ( 24.21908197320000156, 1436.980893512170269, 213.8801751562779998 ) ) ;
#51190 = CARTESIAN_POINT ( 'NONE',  ( -16.61699100185279931, 1508.551704408389924, 210.3875922597520116 ) ) ;
#51191 = CARTESIAN_POINT ( 'NONE',  ( -4.038582018629999659, 1515.598601288590089, 209.1218459616989946 ) ) ;
#51192 = PLANE ( 'NONE',  #110664 ) ;
#51193 = CARTESIAN_POINT ( 'NONE',  ( 19.63708787179688287, 1526.382868172863937, 183.4208852702759316 ) ) ;
#51194 = CARTESIAN_POINT ( 'NONE',  ( -3.255967424474999650, 1516.989560013210166, 214.1335248082570217 ) ) ;
#51195 = CARTESIAN_POINT ( 'NONE',  ( -3.162210773369679817, 1428.830388020579903, 200.3057258517670220 ) ) ;
#51196 = AXIS2_PLACEMENT_3D ( 'NONE', #1654, #61019, #10031 ) ;
#51197 = CARTESIAN_POINT ( 'NONE',  ( 22.99941590693347138, 1409.742488441884007, 209.3674371477623595 ) ) ;
#51198 = CARTESIAN_POINT ( 'NONE',  ( 5.513258753594000083, 1508.551704615640119, 216.1343122516159951 ) ) ;
#51199 = CARTESIAN_POINT ( 'NONE',  ( -3.445685115514999897, 1516.778761582560037, 211.6139765934069885 ) ) ;
#51200 = CARTESIAN_POINT ( 'NONE',  ( -11.72713760778269965, 1482.434255557160213, 207.0899337349270013 ) ) ;
#51201 = EDGE_CURVE ( 'NONE', #36699, #108462, #52200, .T. ) ;
#51202 = CARTESIAN_POINT ( 'NONE',  ( 29.75841426814800528, 1525.320827368874461, 222.0114972872726469 ) ) ;
#51204 = ORIENTED_EDGE ( 'NONE', *, *, #23577, .F. ) ;
#51203 = CARTESIAN_POINT ( 'NONE',  ( -67.88104421250000087, 1388.175118100200052, 291.5606887542589902 ) ) ;
#51205 = CARTESIAN_POINT ( 'NONE',  ( -72.06849244676079991, 1385.017144407860087, 297.2881297217280121 ) ) ;
#51206 = CARTESIAN_POINT ( 'NONE',  ( -8.446261695729999662E-10, 1468.737548875729999, 250.5651368549980305 ) ) ;
#51207 = CARTESIAN_POINT ( 'NONE',  ( 10.85948193710989962, 1490.658306709410226, 210.7204932393690058 ) ) ;
#51208 = CARTESIAN_POINT ( 'NONE',  ( 20.70484064406403846, 1525.907212628473644, 233.2025904124105580 ) ) ;
#51209 = CARTESIAN_POINT ( 'NONE',  ( -2.864170848000150205, 1509.034024718710043, 238.6060105441289920 ) ) ;
#51210 = CARTESIAN_POINT ( 'NONE',  ( 10.86975233959999976, 1425.686310118649772, 206.4629375099989943 ) ) ;
#51211 = CARTESIAN_POINT ( 'NONE',  ( 1.174449684515169956, 1452.839884179820046, 183.4104027199379914 ) ) ;
#51213 = DIRECTION ( 'NONE',  ( 0.8775825618903720926, 0.000000000000000000, 0.4794255386042039491 ) ) ;
#51212 = DIRECTION ( 'NONE',  ( 0.04361938736533144123, 0.9990482215818579093, 0.000000000000000000 ) ) ;
#51214 = FACE_OUTER_BOUND ( 'NONE', #104204, .T. ) ;
#51215 = CARTESIAN_POINT ( 'NONE',  ( -109.4369740319060185, 1383.303469659739903, 311.1345803559980254 ) ) ;
#51216 = VERTEX_POINT ( 'NONE', #43783 ) ;
#51217 = CARTESIAN_POINT ( 'NONE',  ( -7.331812124104999384, 1516.906641539930206, 202.5676945058570197 ) ) ;
#51218 = CARTESIAN_POINT ( 'NONE',  ( -11.57853339036000051, 1508.440951728300206, 218.0096696868039885 ) ) ;
#51219 = CARTESIAN_POINT ( 'NONE',  ( 32.02808312589922224, 1512.187213306747481, 220.9649204700462235 ) ) ;
#51220 = CARTESIAN_POINT ( 'NONE',  ( 24.58439919890000169, 1442.301074160069902, 213.1549993496080333 ) ) ;
#51221 = DIRECTION ( 'NONE',  ( 0.000000000000000000, -1.000000000000000000, 0.000000000000000000 ) ) ;
#51222 = CARTESIAN_POINT ( 'NONE',  ( 4.025649270539999769, 1466.171376325889923, 219.4115622680990043 ) ) ;
#51223 = CARTESIAN_POINT ( 'NONE',  ( -0.3665735836847974771, 1469.467114346855169, 219.1664881883607165 ) ) ;
#51224 = CARTESIAN_POINT ( 'NONE',  ( 28.39358856799220021, 1435.964832128500120, 136.4714687674249944 ) ) ;
#51225 = CARTESIAN_POINT ( 'NONE',  ( 40.21456421019439631, 1444.725599080220036, 137.0098365210060081 ) ) ;
#51226 = CARTESIAN_POINT ( 'NONE',  ( -2.907264515414449857, 1451.960119877520128, 184.7556101994359778 ) ) ;
#51227 = CARTESIAN_POINT ( 'NONE',  ( -109.1483069509999950, 1386.118696371760052, 297.2762669758590164 ) ) ;
#51228 = CARTESIAN_POINT ( 'NONE',  ( 13.73944485519999859, 1508.116386186929958, 185.6413942156979999 ) ) ;
#51229 = CARTESIAN_POINT ( 'NONE',  ( 11.75435543447689923, 1479.754058704430008, 210.0662386466290172 ) ) ;
#51230 = CARTESIAN_POINT ( 'NONE',  ( -21.83181799873807805, 1524.739563915922190, 184.6224812385471523 ) ) ;
#51231 = CARTESIAN_POINT ( 'NONE',  ( -40.82827697499264730, 1448.469058903514906, 269.6248674872855418 ) ) ;
#51232 = ORIENTED_EDGE ( 'NONE', *, *, #45484, .T. ) ;
#51233 = CARTESIAN_POINT ( 'NONE',  ( 1.633469776390000128, 1432.353341358199941, 150.3624711946980028 ) ) ;
#51234 = CARTESIAN_POINT ( 'NONE',  ( 12.40452786870000068, 1434.419866698830219, 146.5969156002979901 ) ) ;
#51235 = CARTESIAN_POINT ( 'NONE',  ( -3.487587080698910214, 1508.884219106000046, 213.6131341098150074 ) ) ;
#51236 = DIRECTION ( 'NONE',  ( 0.9956776678953921378, -0.09285416003634892890, 0.002021538606455937359 ) ) ;
#51237 = CARTESIAN_POINT ( 'NONE',  ( 11.39112423001730789, 1425.664172111152993, 138.8630547727001670 ) ) ;
#51239 = CARTESIAN_POINT ( 'NONE',  ( -17.11714618750000128, 1444.740067931809790, 162.7561046190980107 ) ) ;
#51238 = CARTESIAN_POINT ( 'NONE',  ( -33.23571934791680604, 1512.187213306747481, 198.7594255952499793 ) ) ;
#51240 = CARTESIAN_POINT ( 'NONE',  ( 24.63043001767085727, 1451.910743108596080, 137.3284549923116629 ) ) ;
#51241 = CARTESIAN_POINT ( 'NONE',  ( 9.217029512000001645, 1427.824332272489983, 211.8044453694090237 ) ) ;
#51242 = CARTESIAN_POINT ( 'NONE',  ( -2.956826570601670312, 1515.222544082249897, 213.4459675328979813 ) ) ;
#51243 = PRODUCT_DEFINITION_FORMATION_WITH_SPECIFIED_SOURCE ( 'ANY', '', #22290, .NOT_KNOWN. ) ;
#51244 = CARTESIAN_POINT ( 'NONE',  ( -12.30704544771305997, 1419.221384995674498, 228.6548432408881126 ) ) ;
#51245 = CARTESIAN_POINT ( 'NONE',  ( -5.352781315208301471, 1451.479376706958192, 153.6005146435509516 ) ) ;
#51246 = CARTESIAN_POINT ( 'NONE',  ( -17.50151672410429882, 1415.426561690370136, 209.2157686050819905 ) ) ;
#51247 = CARTESIAN_POINT ( 'NONE',  ( 25.04098008639999762, 1435.655091878980102, 136.8337871717980079 ) ) ;
#51248 = CARTESIAN_POINT ( 'NONE',  ( -10.07831585545570086, 1396.265002934200083, 204.5499906845170131 ) ) ;
#51249 = EDGE_LOOP ( 'NONE', ( #75627, #85552, #89157, #87609 ) ) ;
#51250 = CARTESIAN_POINT ( 'NONE',  ( 0.2241001114877609890, 1414.913060387399810, 193.0224632409980074 ) ) ;
#51251 = CARTESIAN_POINT ( 'NONE',  ( -5.505226529499999799, 1409.105307133929955, 230.1454130303979753 ) ) ;
#51252 = ORIENTED_EDGE ( 'NONE', *, *, #80295, .T. ) ;
#51253 = ORIENTED_EDGE ( 'NONE', *, *, #29546, .F. ) ;
#51254 = CARTESIAN_POINT ( 'NONE',  ( -11.48424209289999887, 1501.246870413989882, 210.7154051127189973 ) ) ;
#51255 = CARTESIAN_POINT ( 'NONE',  ( -15.30458060377867646, 1416.034819603857841, 206.6266340747784227 ) ) ;
#51257 = CARTESIAN_POINT ( 'NONE',  ( -9.966727850805121136, 1439.480327375449860, 208.4309914983489875 ) ) ;
#51256 = CARTESIAN_POINT ( 'NONE',  ( 11.01695271670000054, 1426.937849641930143, 91.93091727569790805 ) ) ;
#51258 = CARTESIAN_POINT ( 'NONE',  ( 24.06753648839999826, 1410.675710978030111, 209.6250578378659668 ) ) ;
#51259 = CARTESIAN_POINT ( 'NONE',  ( -0.1652168328899510097, 1507.119555385590047, 237.3426446390569993 ) ) ;
#51260 = CARTESIAN_POINT ( 'NONE',  ( -12.30432296583530061, 1378.363065960840231, 209.8932745738640051 ) ) ;
#51261 = CARTESIAN_POINT ( 'NONE',  ( -2.497969711800415382, 1421.148623978353953, 184.9753524319759492 ) ) ;
#51262 = CARTESIAN_POINT ( 'NONE',  ( 7.004917722090000076, 1424.454089082370047, 213.1672744739490213 ) ) ;
#51263 = CARTESIAN_POINT ( 'NONE',  ( -18.29179384260000063, 1466.060301038189891, 217.7541513960790098 ) ) ;
#51264 = CARTESIAN_POINT ( 'NONE',  ( -24.08426305480000451, 1411.115211393229856, 208.6111285346999864 ) ) ;
#51265 = CARTESIAN_POINT ( 'NONE',  ( -105.6883471066019951, 1379.461008901829928, 304.2217744859839854 ) ) ;
#51266 = CARTESIAN_POINT ( 'NONE',  ( 9.093835586129998205, 1363.023136422000107, 207.6218459616989946 ) ) ;
#51267 = CARTESIAN_POINT ( 'NONE',  ( -23.59273067950500291, 1509.852083508271107, 190.5178204038475656 ) ) ;
#51268 =( GEOMETRIC_REPRESENTATION_CONTEXT ( 3 ) GLOBAL_UNCERTAINTY_ASSIGNED_CONTEXT ( ( #88268 ) ) GLOBAL_UNIT_ASSIGNED_CONTEXT ( ( #2428, #77452, #53367 ) ) REPRESENTATION_CONTEXT ( 'NONE', 'WORKASPACE' ) );
#51270 = ORIENTED_EDGE ( 'NONE', *, *, #19407, .F. ) ;
#51269 = CARTESIAN_POINT ( 'NONE',  ( 19.32263322520000060, 1455.378559704889767, 209.1218459616989946 ) ) ;
#51271 = ORIENTED_EDGE ( 'NONE', *, *, #79881, .T. ) ;
#51272 = CARTESIAN_POINT ( 'NONE',  ( -11.85531524228330014, 1431.584718363120146, 149.9327016396569832 ) ) ;
#51273 = CARTESIAN_POINT ( 'NONE',  ( 7.465999341866490724, 1510.821818219470515, 202.9578065124467230 ) ) ;
#51274 = CARTESIAN_POINT ( 'NONE',  ( -2.339369569539999638, 1474.134115800729887, 270.1366117264980176 ) ) ;
#51275 = CARTESIAN_POINT ( 'NONE',  ( 13.31848378016444734, 1434.903344954230306, 146.7688399487844606 ) ) ;
#51276 = CARTESIAN_POINT ( 'NONE',  ( -121.5779650366722535, 1311.832804576488343, 299.7542032958708091 ) ) ;
#51277 = CARTESIAN_POINT ( 'NONE',  ( 19.76034656259999878, 1519.913060387329779, 196.6657374964980249 ) ) ;
#51278 = CARTESIAN_POINT ( 'NONE',  ( -9.123736304069998582, 1384.508619150859886, 199.9712811105490289 ) ) ;
#51279 = CARTESIAN_POINT ( 'NONE',  ( 38.64678288495740333, 1443.959461509469975, 137.1848747843469880 ) ) ;
#51280 = CARTESIAN_POINT ( 'NONE',  ( 8.904389930515678842, 1368.484676233528489, 210.6218459617030021 ) ) ;
#51281 = CARTESIAN_POINT ( 'NONE',  ( -9.735300322427688613, 1447.426970202749999, 210.9824412164790317 ) ) ;
#51282 = CARTESIAN_POINT ( 'NONE',  ( -15.53177320253059968, 1407.736001233250136, 267.4358752646630251 ) ) ;
#51283 = CARTESIAN_POINT ( 'NONE',  ( -14.50855428415770021, 1436.251820910509878, 149.9260813992850103 ) ) ;
#51284 = EDGE_LOOP ( 'NONE', ( #88743, #93353, #92131, #107090 ) ) ;
#51285 = DIRECTION ( 'NONE',  ( -1.000000000000000000, 0.000000000000000000, 0.000000000000000000 ) ) ;
#51286 = CARTESIAN_POINT ( 'NONE',  ( 13.64985700350000108, 1444.557014110619775, 188.8602261534980187 ) ) ;
#51287 = ORIENTED_EDGE ( 'NONE', *, *, #35739, .F. ) ;
#51288 = EDGE_LOOP ( 'NONE', ( #57385, #107559, #76583, #20645, #38757, #52097, #81186, #66067 ) ) ;
#51289 = CARTESIAN_POINT ( 'NONE',  ( 4.664360135691749676, 1422.142640414709604, 184.1192042709404291 ) ) ;
#51290 = CARTESIAN_POINT ( 'NONE',  ( 6.435621394989889943, 1424.539923079149958, 193.7524916796629952 ) ) ;
#51291 = CARTESIAN_POINT ( 'NONE',  ( -6.936398393775000670, 1516.667393516340098, 213.1585948090369698 ) ) ;
#51292 = CARTESIAN_POINT ( 'NONE',  ( -18.13447789030000123, 1470.472875412729991, 189.7357867468980146 ) ) ;
#51293 = DIRECTION ( 'NONE',  ( 0.3363363969979658030, 0.9417419115949056119, 0.000000000000000000 ) ) ;
#51294 = ORIENTED_EDGE ( 'NONE', *, *, #27771, .F. ) ;
#51295 = CARTESIAN_POINT ( 'NONE',  ( -8.881784197000000993E-16, 1391.913060387289988, 209.1218459616989946 ) ) ;
#51296 = CARTESIAN_POINT ( 'NONE',  ( -3.458526536014999930, 1516.742629295279812, 204.1242721449069961 ) ) ;
#51297 = CARTESIAN_POINT ( 'NONE',  ( -28.19408351100000232, 1508.123162623830012, 208.4952225986349958 ) ) ;
#51298 = CARTESIAN_POINT ( 'NONE',  ( 3.947090874974254149, 1427.113278099589934, 134.0999999980980704 ) ) ;
#51299 = CARTESIAN_POINT ( 'NONE',  ( -30.86955864515919856, 1384.558263882109941, 206.0685599762870197 ) ) ;
#51300 = CARTESIAN_POINT ( 'NONE',  ( -1.284214933530000158, 1407.590765156830003, 196.0582559783980230 ) ) ;
#51301 = CARTESIAN_POINT ( 'NONE',  ( -13.85929445400000048, 1410.325638502529955, 227.0940372023979990 ) ) ;
#51303 = VERTEX_POINT ( 'NONE', #69566 ) ;
#51302 = DIRECTION ( 'NONE',  ( -0.9980844203940560933, -0.06184550950400349856, -0.001619481661280090237 ) ) ;
#51304 = CARTESIAN_POINT ( 'NONE',  ( -26.50580188063009857, 1469.329502110289923, 209.9352390060020070 ) ) ;
#51305 = CARTESIAN_POINT ( 'NONE',  ( 27.42581371220000008, 1488.692458006830066, 209.3595745165729909 ) ) ;
#51306 = CARTESIAN_POINT ( 'NONE',  ( -33.52629754523064065, 1379.638293383748078, 221.4617334473517190 ) ) ;
#51307 = CARTESIAN_POINT ( 'NONE',  ( 19.07029180426959769, 1456.930551391809786, 225.1474799417119925 ) ) ;
#51308 = CARTESIAN_POINT ( 'NONE',  ( -23.80235451360000098, 1435.328707481769925, 136.9030858810979794 ) ) ;
#51309 =( REPRESENTATION_RELATIONSHIP ('NONE','NONE', #14372, #45156 ) REPRESENTATION_RELATIONSHIP_WITH_TRANSFORMATION ( #94668 )SHAPE_REPRESENTATION_RELATIONSHIP( ) );
#51310 = CARTESIAN_POINT ( 'NONE',  ( -4.609064341505000328, 1516.723920667490120, 211.9995909164769898 ) ) ;
#51311 = CARTESIAN_POINT ( 'NONE',  ( -68.70865610920000677, 1379.748126065489942, 280.0489821606589658 ) ) ;
#51312 = AXIS2_PLACEMENT_3D ( 'NONE', #50962, #74520, #49861 ) ;
#51313 = CARTESIAN_POINT ( 'NONE',  ( 8.594280337688530835, 1437.591337424159974, 210.1983079730889870 ) ) ;
#51314 = CARTESIAN_POINT ( 'NONE',  ( -16.66936639845609491, 1523.382868172864164, 237.7608804993221838 ) ) ;
#51315 = CARTESIAN_POINT ( 'NONE',  ( -3.269025173884999802, 1517.026534522949987, 208.0024068424170025 ) ) ;
#51316 = ORIENTED_EDGE ( 'NONE', *, *, #16619, .F. ) ;
#51317 = CARTESIAN_POINT ( 'NONE',  ( -2.068751723726309777, 1451.946575739190166, 184.4429135660199961 ) ) ;
#51318 = CARTESIAN_POINT ( 'NONE',  ( -0.5133635713019999436, 1410.311096974030079, 233.1717008067979862 ) ) ;
#51319 = CARTESIAN_POINT ( 'NONE',  ( -3.078458293570000226, 1385.048553955020225, 218.5738910584090036 ) ) ;
#51320 = ORIENTED_EDGE ( 'NONE', *, *, #40299, .T. ) ;
#51321 = CARTESIAN_POINT ( 'NONE',  ( -13.02322703936409987, 1416.825784014559986, 196.6108461303639672 ) ) ;
#51322 = CARTESIAN_POINT ( 'NONE',  ( -10.60846321666980074, 1492.499096768809977, 202.9143931177430034 ) ) ;
#51323 = CARTESIAN_POINT ( 'NONE',  ( 11.83454512112139945, 1434.825470695330068, 151.1770841828369782 ) ) ;
#51324 = CARTESIAN_POINT ( 'NONE',  ( -4.138348461501534459, 1441.507286901806310, 184.0825983021243815 ) ) ;
#51325 = B_SPLINE_CURVE_WITH_KNOTS ( 'NONE', 3,
 ( #65504, #22897, #57106, #15595, #49799, #1061, #25112, #17248, #51441, #94529 ),
 .UNSPECIFIED., .F., .F.,
 ( 4, 2, 2, 2, 4 ),
 ( 0.000000000000000000, 0.2500000000000000000, 0.5000000000000000000, 0.7500000000000000000, 1.000000000000000000 ),
 .UNSPECIFIED. ) ;
#51326 = CARTESIAN_POINT ( 'NONE',  ( -22.04195665738010135, 1508.943562127990162, 226.5634866290460252 ) ) ;
#51327 = CARTESIAN_POINT ( 'NONE',  ( -16.52275697106984609, 1525.042337199239910, 237.2696949994484328 ) ) ;
#51328 = DIRECTION ( 'NONE',  ( 1.006446316953035876E-09, 1.000000000000000000, -9.896731379374899561E-10 ) ) ;
#51329 = CARTESIAN_POINT ( 'NONE',  ( 15.69795926888880189, 1517.051704408389924, 222.7678737654429995 ) ) ;
#51330 = DIRECTION ( 'NONE',  ( -0.000000000000000000, 1.000000000000000000, -0.000000000000000000 ) ) ;
#51331 = EDGE_CURVE ( 'NONE', #10158, #25299, #105549, .T. ) ;
#51333 = CARTESIAN_POINT ( 'NONE',  ( -2.466766482289999729, 1421.294048410029973, 184.8150638888980097 ) ) ;
#51332 = CARTESIAN_POINT ( 'NONE',  ( 6.945490048805000427, 1516.932669162149978, 214.9002185338470099 ) ) ;
#51334 = CARTESIAN_POINT ( 'NONE',  ( 21.21436153039999795, 1509.702916644130028, 188.2361191047979787 ) ) ;
#51335 = CARTESIAN_POINT ( 'NONE',  ( 5.004442038985000174, 1516.690345681169902, 216.8349637732169697 ) ) ;
#51336 = AXIS2_PLACEMENT_3D ( 'NONE', #109993, #42239, #110536 ) ;
#51337 = ORIENTED_EDGE ( 'NONE', *, *, #61681, .T. ) ;
#51338 = CARTESIAN_POINT ( 'NONE',  ( -12.58190538649999901, 1415.948532224930204, 195.9645815321979967 ) ) ;
#51339 = CARTESIAN_POINT ( 'NONE',  ( -16.64876402000000155, 1420.540327547920015, 203.2475213236290017 ) ) ;
#51340 = ORIENTED_EDGE ( 'NONE', *, *, #45919, .F. ) ;
#51341 = CARTESIAN_POINT ( 'NONE',  ( 20.41260875014629761, 1494.156740513740033, 204.1224910194729887 ) ) ;
#51342 =( BOUNDED_CURVE ( )  B_SPLINE_CURVE ( 3, ( #1532, #25593, #34563, #43532 ),
 .UNSPECIFIED., .F., .F. ) 
 B_SPLINE_CURVE_WITH_KNOTS ( ( 4, 4 ),
 ( 0.9863028871718200197, 2.155290151626870099 ),
 .UNSPECIFIED. ) 
 CURVE ( )  GEOMETRIC_REPRESENTATION_ITEM ( )  RATIONAL_B_SPLINE_CURVE ( ( 1.000000000000000000, 0.8893277299739500430, 0.8893277299739500430, 1.000000000000000000 ) ) 
 REPRESENTATION_ITEM ( '' )  );
#51343 = CARTESIAN_POINT ( 'NONE',  ( -12.96940454689999989, 1511.061367290189992, 209.8579693186340194 ) ) ;
#51344 = CARTESIAN_POINT ( 'NONE',  ( 2.472529913803020563, 1523.678648413191695, 175.3762130535718597 ) ) ;
#51345 = PRODUCT_DEFINITION_CONTEXT ( 'detailed design', #14836, 'design' ) ;
#51346 = CARTESIAN_POINT ( 'NONE',  ( 0.3061100630284139812, 1423.569528417510128, 191.1866024191019733 ) ) ;
#51347 = CARTESIAN_POINT ( 'NONE',  ( -11.34294724864570014, 1471.070521140359915, 207.8607066046959915 ) ) ;
#51348 = CARTESIAN_POINT ( 'NONE',  ( -6.379498533362892410, 1508.334156579840510, 219.9884138064801959 ) ) ;
#51349 = CARTESIAN_POINT ( 'NONE',  ( 17.50215275067818865, 1422.936145674484123, 226.4538908241968045 ) ) ;
#51350 = DIRECTION ( 'NONE',  ( -0.6736849260863841948, 0.000000000000000000, 0.7390186874254148774 ) ) ;
#51351 = CARTESIAN_POINT ( 'NONE',  ( 8.782444512891389721, 1461.515893433170049, 204.8665823944039914 ) ) ;
#51352 = CARTESIAN_POINT ( 'NONE',  ( -11.91321771470000002, 1435.943783413959864, 147.6429393588979906 ) ) ;
#51353 = CARTESIAN_POINT ( 'NONE',  ( 26.80104177516750141, 1446.506287311350206, 137.4021340779750062 ) ) ;
#51355 = DIRECTION ( 'NONE',  ( 0.7059182309095664021, 0.02465121832729061380, -0.7078642304174497246 ) ) ;
#51354 = CARTESIAN_POINT ( 'NONE',  ( -12.91642173549690042, 1417.638397378020045, 200.6455995762629811 ) ) ;
#51356 = CARTESIAN_POINT ( 'NONE',  ( 11.23256922559021653, 1433.984535818029144, 151.5862715624802490 ) ) ;
#51357 = ORIENTED_EDGE ( 'NONE', *, *, #96051, .F. ) ;
#51358 = CARTESIAN_POINT ( 'NONE',  ( -11.17096468969999812, 1500.478073591689963, 215.5530715242690007 ) ) ;
#51359 = CARTESIAN_POINT ( 'NONE',  ( 18.82859584293606758, 1461.935129172100915, 190.8088398609367857 ) ) ;
#51360 = AXIS2_PLACEMENT_3D ( 'NONE', #49413, #76808, #84093 ) ;
#51361 = CARTESIAN_POINT ( 'NONE',  ( -4.633397089669999858, 1377.913060387289988, 209.1218459563329759 ) ) ;
#51362 = LINE ( 'NONE', #12119, #25646 ) ;
#51363 = CARTESIAN_POINT ( 'NONE',  ( -10.51130365114040011, 1479.967629185039868, 209.1301374756710061 ) ) ;
#51364 = CARTESIAN_POINT ( 'NONE',  ( 2.923521462801879967, 1410.394928839790055, 231.6309329194170061 ) ) ;
#51365 = DIRECTION ( 'NONE',  ( -0.1070030146457375958, 0.000000000000000000, -0.9942586961433750314 ) ) ;
#51366 = CARTESIAN_POINT ( 'NONE',  ( -17.51440555739999994, 1442.103933559090137, 219.2287671671990097 ) ) ;
#51367 = CARTESIAN_POINT ( 'NONE',  ( -54.11663967002189679, 1383.805289491930125, 269.6990428264840034 ) ) ;
#51368 = EDGE_CURVE ( 'NONE', #84088, #109192, #78761, .T. ) ;
#51369 = EDGE_CURVE ( 'NONE', #36236, #15891, #37314, .T. ) ;
#51370 = CARTESIAN_POINT ( 'NONE',  ( 22.73270563069999994, 1451.307588288230136, 142.3779184700979954 ) ) ;
#51371 = B_SPLINE_CURVE_WITH_KNOTS ( 'NONE', 3,
 ( #72350, #81812, #23001, #46598, #72887, #108119, #31413, #57205, #48241, #82384, #80733, #99155, #107027, #64502, #38169, #48801, #56084, #82924, #106479, #6215, #90210, #98619, #47684, #5114, #39270 ),
 .UNSPECIFIED., .F., .F.,
 ( 4, 3, 3, 3, 3, 3, 3, 3, 4 ),
 ( -41.86545604797390041, -41.27964960583160092, -39.51168084002180336, -37.86278309458619873, -36.27358298899350331, -34.76523579414600107, -33.29895478326900360, -31.86861058327169971, -30.44048980260000548 ),
 .UNSPECIFIED. ) ;
#51372 = PLANE ( 'NONE',  #53620 ) ;
#51373 = CARTESIAN_POINT ( 'NONE',  ( 13.86092937120069912, 1410.765486813650114, 191.1266627561969926 ) ) ;
#51374 = EDGE_CURVE ( 'NONE', #75187, #69928, #43120, .T. ) ;
#51376 = ORIENTED_EDGE ( 'NONE', *, *, #24045, .F. ) ;
#51375 = CARTESIAN_POINT ( 'NONE',  ( 23.57642905779999865, 1509.468438641930106, 193.4040834977980126 ) ) ;
#51377 = CARTESIAN_POINT ( 'NONE',  ( -18.15370184069965731, 1459.449025707702049, 227.9319138183309974 ) ) ;
#51378 = CARTESIAN_POINT ( 'NONE',  ( -36.68365415889999781, 1382.326063136570156, 235.1111881889589768 ) ) ;
#51379 = EDGE_CURVE ( 'NONE', #55526, #34578, #31933, .T. ) ;
#51380 = CARTESIAN_POINT ( 'NONE',  ( 4.973792553537950134, 1508.551704408389924, 206.3628108551109790 ) ) ;
#51381 = ORIENTED_EDGE ( 'NONE', *, *, #67201, .F. ) ;
#51382 = ORIENTED_EDGE ( 'NONE', *, *, #32431, .T. ) ;
#51383 = ADVANCED_FACE ( 'NONE', ( #21297 ), #101033, .T. ) ;
#51384 = CARTESIAN_POINT ( 'NONE',  ( 19.85686604346530260, 1508.846387636299823, 229.4817185467019840 ) ) ;
#51385 = LINE ( 'NONE', #85517, #24214 ) ;
#51386 = CARTESIAN_POINT ( 'NONE',  ( 39.38156440427009386, 1440.303727024390128, 136.7574120630100083 ) ) ;
#51388 = CYLINDRICAL_SURFACE ( 'NONE', #17176, 2.000000000000003553 ) ;
#51387 = DIRECTION ( 'NONE',  ( -0.9965074780644831431, -0.004098122787124980695, 0.08340294689748870005 ) ) ;
#51389 = B_SPLINE_CURVE_WITH_KNOTS ( 'NONE', 5,
 ( #43572, #77721, #1034, #35157, #69900, #104016 ),
 .UNSPECIFIED., .F., .F.,
 ( 6, 6 ),
 ( 362.7063815370000270, 367.7284095229999821 ),
 .UNSPECIFIED. ) ;
#51390 = CARTESIAN_POINT ( 'NONE',  ( 11.75160532048070117, 1479.729357405969949, 209.9771243583440139 ) ) ;
#51391 = CARTESIAN_POINT ( 'NONE',  ( -108.5373427389999961, 1383.177762179680030, 297.5067995922590285 ) ) ;
#51392 = CARTESIAN_POINT ( 'NONE',  ( -12.81719096786032352, 1435.925157283035560, 150.8223353154213839 ) ) ;
#51393 = CARTESIAN_POINT ( 'NONE',  ( 21.38516915557965703, 1522.382868172863937, 180.3939891059721106 ) ) ;
#51394 = CARTESIAN_POINT ( 'NONE',  ( 3.277154590789999933, 1409.963920169630228, 185.8200990145979858 ) ) ;
#51395 = CARTESIAN_POINT ( 'NONE',  ( 0.6879128371797639252, 1508.983932488360097, 179.4145436916340088 ) ) ;
#51396 = CARTESIAN_POINT ( 'NONE',  ( 40.27278867766426629, 1443.694772336818687, 137.1246062732301141 ) ) ;
#51397 = CARTESIAN_POINT ( 'NONE',  ( 8.062593549087260669, 1436.235959150659937, 206.1283030154239952 ) ) ;
#51398 = CARTESIAN_POINT ( 'NONE',  ( -4.284965797313190272, 1440.956314292269781, 155.9224932556410010 ) ) ;
#51399 = CIRCLE ( 'NONE', #97830, 30.13701971169416183 ) ;
#51400 = CARTESIAN_POINT ( 'NONE',  ( -3.793561831505700255, 1450.899630787780097, 184.9307162316310098 ) ) ;
#51401 = CARTESIAN_POINT ( 'NONE',  ( 1.119830458929999883, 1465.309628979130139, 236.0546564598980126 ) ) ;
#51402 = ORIENTED_EDGE ( 'NONE', *, *, #66618, .T. ) ;
#51403 = CARTESIAN_POINT ( 'NONE',  ( 4.749348430879999583, 1472.167733319789932, 187.6580953298989982 ) ) ;
#51405 = ADVANCED_FACE ( 'NONE', ( #26131 ), #977, .F. ) ;
#51404 = CARTESIAN_POINT ( 'NONE',  ( -41.09355243439999583, 1449.585181137809968, 270.0512738362979803 ) ) ;
#51406 = DIRECTION ( 'NONE',  ( 0.000000000000000000, 0.000000000000000000, -1.000000000000000000 ) ) ;
#51407 = CARTESIAN_POINT ( 'NONE',  ( -1.906563618092599921E-08, 1509.038615934239942, 213.6090957241370063 ) ) ;
#51408 = CARTESIAN_POINT ( 'NONE',  ( 17.55838294249999976, 1488.199839363530145, 189.1289626450980279 ) ) ;
#51409 = CARTESIAN_POINT ( 'NONE',  ( 2.330134126628495839, 1515.551704408385831, 213.1059277140580548 ) ) ;
#51410 = CARTESIAN_POINT ( 'NONE',  ( 9.170465408922220618, 1461.406018709129967, 205.9602291374590095 ) ) ;
#51411 = CARTESIAN_POINT ( 'NONE',  ( -1.547930050009999947, 1416.311719782429918, 227.9539241407980228 ) ) ;
#51412 = CARTESIAN_POINT ( 'NONE',  ( -4.139355080849999702, 1416.968741244730154, 232.7076405003979858 ) ) ;
#51413 = CARTESIAN_POINT ( 'NONE',  ( -2.245641459690000286, 1475.226982416989813, 197.8915804961989693 ) ) ;
#51414 = CARTESIAN_POINT ( 'NONE',  ( -104.9846310909999971, 1389.412964589189869, 307.6627679757589817 ) ) ;
#51415 = EDGE_CURVE ( 'NONE', #48402, #55385, #9901, .T. ) ;
#51416 = CARTESIAN_POINT ( 'NONE',  ( 0.08971693578977467387, 1486.409952364518176, 181.8122316423428799 ) ) ;
#51417 = CARTESIAN_POINT ( 'NONE',  ( 6.892224678239999847, 1361.632554499750086, 207.6218459616989946 ) ) ;
#51418 = CARTESIAN_POINT ( 'NONE',  ( -46.14657524832199442, 1438.245561584440111, 267.5940402666269620 ) ) ;
#51419 = CARTESIAN_POINT ( 'NONE',  ( 13.72406976976210125, 1509.120045271949948, 233.9463300173069911 ) ) ;
#51420 = CARTESIAN_POINT ( 'NONE',  ( -7.973575425169999953, 1425.245987008030170, 205.1887793146490253 ) ) ;
#51421 = ADVANCED_FACE ( 'NONE', ( #1520 ), #93345, .F. ) ;
#51422 = ORIENTED_EDGE ( 'NONE', *, *, #48851, .F. ) ;
#51423 = CARTESIAN_POINT ( 'NONE',  ( 6.944466742375000834, 1516.939530130779985, 209.1105810159089913 ) ) ;
#51424 = CARTESIAN_POINT ( 'NONE',  ( -5.439681134809999818, 1437.306888242379955, 154.7134157797979981 ) ) ;
#51425 = AXIS2_PLACEMENT_3D ( 'NONE', #67917, #33177, #109362 ) ;
#51426 = CARTESIAN_POINT ( 'NONE',  ( 19.26518044636202731, 1456.127854578388451, 225.0603431000050421 ) ) ;
#51427 = CARTESIAN_POINT ( 'NONE',  ( 7.527129073409500215, 1425.476184744899911, 212.1957883662609845 ) ) ;
#51428 = CARTESIAN_POINT ( 'NONE',  ( -25.94056929255189914, 1451.122515486970087, 136.6312467053010096 ) ) ;
#51429 = ORIENTED_EDGE ( 'NONE', *, *, #80934, .T. ) ;
#51430 = CARTESIAN_POINT ( 'NONE',  ( 4.385438019169999535, 1418.241830526729927, 231.9989422736980202 ) ) ;
#51432 = CARTESIAN_POINT ( 'NONE',  ( -14.72577118585429901, 1514.214451951579804, 224.1399941292770279 ) ) ;
#51431 = CARTESIAN_POINT ( 'NONE',  ( -10.96112826740149870, 1492.491747564250090, 207.2364351939560265 ) ) ;
#51433 = CARTESIAN_POINT ( 'NONE',  ( 11.60004869885203682, 1423.633685391621384, 135.8154921816039007 ) ) ;
#51434 = CARTESIAN_POINT ( 'NONE',  ( -23.51884061320912878, 1448.078341978384287, 217.4024159428893199 ) ) ;
#51435 = CARTESIAN_POINT ( 'NONE',  ( 7.892648486029999688, 1424.312437875390060, 211.9575832887890101 ) ) ;
#51436 = DIRECTION ( 'NONE',  ( -0.000000000000000000, -1.000000000000000000, -0.000000000000000000 ) ) ;
#51437 = CARTESIAN_POINT ( 'NONE',  ( -18.90690578109999720, 1416.819760216030090, 208.2173865545289857 ) ) ;
#51438 = VERTEX_POINT ( 'NONE', #60320 ) ;
#51439 = CARTESIAN_POINT ( 'NONE',  ( -8.718177347727909421, 1408.261084764490079, 270.1210383458869728 ) ) ;
#51440 = CARTESIAN_POINT ( 'NONE',  ( 4.075906014412360001, 1417.644700588070236, 232.4454855814549887 ) ) ;
#51441 = CARTESIAN_POINT ( 'NONE',  ( -2.500000810785663052, 1448.904868584106680, 183.3442529213150181 ) ) ;
#51443 = EDGE_LOOP ( 'NONE', ( #31723, #70220 ) ) ;
#51442 = CARTESIAN_POINT ( 'NONE',  ( -2.500000000000000000, 1439.615921247279857, 167.6891699144290158 ) ) ;
#51444 = ORIENTED_EDGE ( 'NONE', *, *, #64539, .T. ) ;
#51445 = CARTESIAN_POINT ( 'NONE',  ( -23.63499367410939911, 1410.853431111550208, 210.3632786977680098 ) ) ;
#51446 = CARTESIAN_POINT ( 'NONE',  ( 0.03284348760489309849, 1410.296499662470069, 185.0199513014300123 ) ) ;
#51447 = DIRECTION ( 'NONE',  ( -0.7628756745748126455, -0.04363816677874606670, -0.6450708608689551538 ) ) ;
#51448 = CARTESIAN_POINT ( 'NONE',  ( -9.253402716490001012, 1428.330636036430178, 123.0297916884979941 ) ) ;
#51449 = CARTESIAN_POINT ( 'NONE',  ( -20.15668535170019737, 1479.813499036020175, 193.0638610647490054 ) ) ;
#51450 = CARTESIAN_POINT ( 'NONE',  ( -22.46702269440000421, 1420.825031629329715, 215.0041689658179962 ) ) ;
#51451 = ORIENTED_EDGE ( 'NONE', *, *, #52348, .T. ) ;
#51452 = CARTESIAN_POINT ( 'NONE',  ( 28.47708477731459809, 1468.479349472730064, 266.9011526386389619 ) ) ;
#51453 = CARTESIAN_POINT ( 'NONE',  ( -2.941982104803258835, 1466.821624837357149, 235.0423269388574852 ) ) ;
#51454 = CARTESIAN_POINT ( 'NONE',  ( -3.824657317049999783, 1429.713551374290091, 201.7356719887889938 ) ) ;
#51455 = CARTESIAN_POINT ( 'NONE',  ( -6.561995998525000040, 1517.083030555940013, 205.8633713531569924 ) ) ;
#51456 = VERTEX_POINT ( 'NONE', #51919 ) ;
#51457 = CARTESIAN_POINT ( 'NONE',  ( 18.92306020057025862, 1457.652989641058639, 226.8765308104140956 ) ) ;
#51458 = CARTESIAN_POINT ( 'NONE',  ( 15.26851439840219982, 1512.495155157840145, 195.9338870901020186 ) ) ;
#51459 = CARTESIAN_POINT ( 'NONE',  ( 4.500000000000000000, 1448.210448412289907, 182.3842140122979743 ) ) ;
#51460 = EDGE_LOOP ( 'NONE', ( #43541, #102918, #8612, #67544 ) ) ;
#51461 = CARTESIAN_POINT ( 'NONE',  ( -3.304926829299330709E-16, 1420.443991414029824, 172.2701767054979882 ) ) ;
#51462 = CARTESIAN_POINT ( 'NONE',  ( 26.72825992618109936, 1451.963087292549972, 135.1721373074829842 ) ) ;
#51463 = CARTESIAN_POINT ( 'NONE',  ( -2.640559407880699982, 1508.551704408389924, 214.1054286845740080 ) ) ;
#51464 = CARTESIAN_POINT ( 'NONE',  ( -109.9840560936046927, 1378.913060387289988, 302.1406618644074342 ) ) ;
#51465 = CARTESIAN_POINT ( 'NONE',  ( 7.481687810619999546, 1422.866741622099880, 195.6598841224989940 ) ) ;
#51466 = CARTESIAN_POINT ( 'NONE',  ( 17.02706952559999820, 1409.507658761130187, 193.7554158992979865 ) ) ;
#51467 = CARTESIAN_POINT ( 'NONE',  ( 13.35741048202589809, 1443.913060387329324, 164.9741927960640453 ) ) ;
#51468 = CARTESIAN_POINT ( 'NONE',  ( 0.3812827203925389652, 1408.926375073290046, 186.5173452701070005 ) ) ;
#51470 = DIRECTION ( 'NONE',  ( 0.000000000000000000, -0.7071067811865474617, -0.7071067811865474617 ) ) ;
#51469 = CARTESIAN_POINT ( 'NONE',  ( 1.220192692170000148, 1416.035373678829956, 233.0189416646979907 ) ) ;
#51471 = CIRCLE ( 'NONE', #13878, 26.99999999999999645 ) ;
#51472 = CARTESIAN_POINT ( 'NONE',  ( 11.95779796459999922, 1409.330635893630188, 227.4564908493979942 ) ) ;
#51473 = EDGE_CURVE ( 'NONE', #77609, #43125, #97388, .T. ) ;
#51474 = CARTESIAN_POINT ( 'NONE',  ( -1.906499846882070084E-08, 1516.051704408390151, 209.1218459511669892 ) ) ;
#51475 = CARTESIAN_POINT ( 'NONE',  ( -11.46268780760000006, 1379.176763712969887, 214.2011949338190107 ) ) ;
#51476 = EDGE_CURVE ( 'NONE', #94471, #50492, #29367, .T. ) ;
#51477 = CARTESIAN_POINT ( 'NONE',  ( 5.007662633622221193, 1418.086932660744651, 233.9718093764707305 ) ) ;
#51478 = ORIENTED_EDGE ( 'NONE', *, *, #96141, .T. ) ;
#51479 = CARTESIAN_POINT ( 'NONE',  ( 12.70695307632060000, 1416.230844595159851, 222.1275921544260257 ) ) ;
#51480 = CARTESIAN_POINT ( 'NONE',  ( 11.86176262958469962, 1432.335962564359988, 150.1420606180239758 ) ) ;
#51481 = VECTOR ( 'NONE', #85852, 1000.000000000000000 ) ;
#51482 = CARTESIAN_POINT ( 'NONE',  ( -10.22150738884329968, 1483.444541873599974, 203.0139270434760022 ) ) ;
#51483 = AXIS2_PLACEMENT_3D ( 'NONE', #62481, #10941, #105559 ) ;
#51484 = CARTESIAN_POINT ( 'NONE',  ( -13.85278479829999831, 1390.202287805009973, 206.8926036963289903 ) ) ;
#51485 = CARTESIAN_POINT ( 'NONE',  ( 9.270085536629588674, 1427.204361394170064, 210.8459614755520022 ) ) ;
#51486 = CARTESIAN_POINT ( 'NONE',  ( 1.547169282253892053, 1421.459440452008039, 193.7923915457423902 ) ) ;
#51487 = CARTESIAN_POINT ( 'NONE',  ( -11.02391225866199953, 1462.506727572930004, 208.4595876642919734 ) ) ;
#51488 = CARTESIAN_POINT ( 'NONE',  ( -26.42894385079999964, 1460.505561531929970, 262.6648722463980334 ) ) ;
#51489 = ADVANCED_FACE ( 'NONE', ( #33997 ), #85354, .F. ) ;
#51490 = CARTESIAN_POINT ( 'NONE',  ( -10.24091433091644809, 1479.068389395743679, 211.4585749931201235 ) ) ;
#51491 = CARTESIAN_POINT ( 'NONE',  ( 11.18950481729999957, 1433.539833593499907, 151.6108599932980212 ) ) ;
#51492 = CARTESIAN_POINT ( 'NONE',  ( 26.42714721250000309, 1443.942861156509935, 243.9198229606980135 ) ) ;
#51493 = CARTESIAN_POINT ( 'NONE',  ( -9.686238329417539816, 1461.028144820860007, 208.9774245188330042 ) ) ;
#51494 = CARTESIAN_POINT ( 'NONE',  ( 2.645368138919999890, 1426.526422906339803, 188.7496620777990017 ) ) ;
#51495 = CARTESIAN_POINT ( 'NONE',  ( 11.32501011340429997, 1425.466614524120132, 201.3329890293439917 ) ) ;
#51496 = CARTESIAN_POINT ( 'NONE',  ( 5.378706850333720091, 1465.763327832039977, 218.3327295566870134 ) ) ;
#51497 = CARTESIAN_POINT ( 'NONE',  ( -13.63663271600000115, 1486.121807553629878, 185.3134443986979818 ) ) ;
#51498 = CARTESIAN_POINT ( 'NONE',  ( 11.90436745871180690, 1398.266016359466903, 214.3454593262396202 ) ) ;
#51499 = CARTESIAN_POINT ( 'NONE',  ( -25.72757591410449862, 1509.824537483000086, 193.1381027855750006 ) ) ;
#51500 = AXIS2_PLACEMENT_3D ( 'NONE', #60480, #69441, #36909 ) ;
#51501 = CARTESIAN_POINT ( 'NONE',  ( 22.35979953500000050, 1410.906900721630109, 215.2033244915180035 ) ) ;
#51502 = CARTESIAN_POINT ( 'NONE',  ( 0.6427929286027795897, 1477.829905493179695, 198.7252071007316090 ) ) ;
#51503 = CARTESIAN_POINT ( 'NONE',  ( 26.08009213506066715, 1436.684477317271103, 136.9230107608492233 ) ) ;
#51504 = CARTESIAN_POINT ( 'NONE',  ( -1.485593186740000071, 1515.527915486090023, 205.0761616848290032 ) ) ;
#51505 = CARTESIAN_POINT ( 'NONE',  ( 5.826428076080000906, 1473.811884028689974, 218.9454251420289950 ) ) ;
#51506 = ADVANCED_FACE ( 'NONE', ( #11015 ), #46369, .F. ) ;
#51507 = CARTESIAN_POINT ( 'NONE',  ( -19.73707540517630221, 1467.795348456740157, 204.3773263242620146 ) ) ;
#51508 = CARTESIAN_POINT ( 'NONE',  ( 3.266349474065000091, 1516.797038924770050, 213.1501537103870021 ) ) ;
#51509 = CARTESIAN_POINT ( 'NONE',  ( -11.35287584023299878, 1423.238978238550089, 204.2096404009320167 ) ) ;
#51510 = CARTESIAN_POINT ( 'NONE',  ( 0.1727113076434980132, 1478.739035586289901, 182.1485550913949965 ) ) ;
#51511 = EDGE_CURVE ( 'NONE', #69033, #1227, #86031, .T. ) ;
#51513 = ORIENTED_EDGE ( 'NONE', *, *, #89125, .T. ) ;
#51512 = CARTESIAN_POINT ( 'NONE',  ( 4.010802518989999399, 1440.993092037090037, 217.7599617541789883 ) ) ;
#51514 = CARTESIAN_POINT ( 'NONE',  ( -13.51610093809999924, 1443.913060387330006, 169.3501091259980171 ) ) ;
#51515 = CARTESIAN_POINT ( 'NONE',  ( -38.71377205869448801, 1444.324653571827866, 136.9322096537518973 ) ) ;
#51516 = CARTESIAN_POINT ( 'NONE',  ( 3.250000000000000000, 1524.051704408389924, 209.1218459616989946 ) ) ;
#51517 = CARTESIAN_POINT ( 'NONE',  ( -31.92299894892000722, 1524.776010967693992, 216.6640755986756517 ) ) ;
#51518 = CARTESIAN_POINT ( 'NONE',  ( -109.1649475050000007, 1384.884072125880039, 297.1327577457590223 ) ) ;
#51519 = ORIENTED_EDGE ( 'NONE', *, *, #101280, .F. ) ;
#51520 = CARTESIAN_POINT ( 'NONE',  ( -10.96582334520000046, 1470.988105993590125, 208.9883436308459750 ) ) ;
#51521 = CARTESIAN_POINT ( 'NONE',  ( -12.24215919237970063, 1392.317484695480061, 210.7023522567849909 ) ) ;
#51522 = CARTESIAN_POINT ( 'NONE',  ( -17.16585533279999964, 1415.931391677329884, 214.4037704070680093 ) ) ;
#51523 = CARTESIAN_POINT ( 'NONE',  ( -16.71509328323223187, 1526.382868172864391, 183.8816066442305726 ) ) ;
#51525 = EDGE_CURVE ( 'NONE', #10141, #77824, #94828, .T. ) ;
#51524 = CARTESIAN_POINT ( 'NONE',  ( -9.198895294782719390, 1437.332964060710310, 212.8805274561509862 ) ) ;
#51526 = AXIS2_PLACEMENT_3D ( 'NONE', #28560, #46487, #21220 ) ;
#51527 = CARTESIAN_POINT ( 'NONE',  ( -107.6245944317399506, 1380.278007003908897, 309.5812188244966023 ) ) ;
#51528 = CARTESIAN_POINT ( 'NONE',  ( -10.35182684444420076, 1472.068470821749997, 207.0629838042650022 ) ) ;
#51529 = CARTESIAN_POINT ( 'NONE',  ( -12.47575469030000050, 1379.153285202859934, 210.8825669665690157 ) ) ;
#51530 = CARTESIAN_POINT ( 'NONE',  ( -12.55604107059999919, 1391.387401865550146, 208.6966032511679714 ) ) ;
#51531 = CARTESIAN_POINT ( 'NONE',  ( -72.30449149428240219, 1385.123662558519982, 270.5213631660990359 ) ) ;
#51532 = CARTESIAN_POINT ( 'NONE',  ( -11.54851213157500212, 1391.913060387289988, 210.7248915062780270 ) ) ;
#51533 = CARTESIAN_POINT ( 'NONE',  ( 10.91486453896849973, 1422.290287042430009, 209.5939553138669851 ) ) ;
#51534 = ORIENTED_EDGE ( 'NONE', *, *, #19407, .T. ) ;
#51535 = EDGE_CURVE ( 'NONE', #52413, #43913, #45475, .T. ) ;
#51536 = CARTESIAN_POINT ( 'NONE',  ( 17.22623662315568893, 1443.501467202830781, 162.9225832754749490 ) ) ;
#51538 = ORIENTED_EDGE ( 'NONE', *, *, #76021, .F. ) ;
#51537 = CARTESIAN_POINT ( 'NONE',  ( 17.71193101166619854, 1519.551704408389924, 196.6727161458730109 ) ) ;
#51539 = CARTESIAN_POINT ( 'NONE',  ( 4.650852508730000778, 1472.634552772589814, 218.1962482253990174 ) ) ;
#51540 = VERTEX_POINT ( 'NONE', #89913 ) ;
#51541 = CARTESIAN_POINT ( 'NONE',  ( 18.72979941119999836, 1454.437773883689943, 204.5413093961989830 ) ) ;
#51542 = CARTESIAN_POINT ( 'NONE',  ( -8.910387285859998840, 1362.858511851210096, 207.6218459616989946 ) ) ;
#51543 = DIRECTION ( 'NONE',  ( 0.03006000153037601333, -0.4884709562387480331, 0.8720622232496927362 ) ) ;
#51544 = CARTESIAN_POINT ( 'NONE',  ( 38.90834013964843052, 1452.449200603389727, 269.5913925115327743 ) ) ;
#51545 = CARTESIAN_POINT ( 'NONE',  ( -1.906499758064230099E-08, 1516.051704408390151, 209.1218459511669892 ) ) ;
#51546 = CARTESIAN_POINT ( 'NONE',  ( 16.18610113297054198, 1432.064054184273346, 218.4257206746670192 ) ) ;
#51547 = CARTESIAN_POINT ( 'NONE',  ( 2.961376673209999755, 1417.751980673930120, 234.4067280231980135 ) ) ;
#51548 = CARTESIAN_POINT ( 'NONE',  ( 5.134328406469999884, 1447.265806521789955, 200.6829430861090202 ) ) ;
#51549 = CARTESIAN_POINT ( 'NONE',  ( -117.4166280489782253, 1306.483669372789336, 297.4506287831988516 ) ) ;
#51550 = B_SPLINE_CURVE_WITH_KNOTS ( 'NONE', 5,
 ( #25450, #93754, #17031, #51794, #8657, #36640, #3617, #61872, #54574, #97647, #19823, #20917 ),
 .UNSPECIFIED., .F., .F.,
 ( 6, 3, 3, 6 ),
 ( 0.000000000000000000, 0.4064120419304899090, 0.8128240838611042740, 1.000000000000000000 ),
 .UNSPECIFIED. ) ;
#51551 = CARTESIAN_POINT ( 'NONE',  ( -8.774197885167456690, 1368.328613538127001, 207.6218459616987673 ) ) ;
#51552 = EDGE_CURVE ( 'NONE', #18384, #62647, #44, .T. ) ;
#51553 = CARTESIAN_POINT ( 'NONE',  ( -2.455032153949999962, 1454.699340087689961, 198.9067334848990072 ) ) ;
#51554 = CARTESIAN_POINT ( 'NONE',  ( -3.461360131404999763, 1516.874084700499907, 205.8683838714370040 ) ) ;
#51555 = VECTOR ( 'NONE', #63266, 1000.000000000000114 ) ;
#51556 = FACE_OUTER_BOUND ( 'NONE', #91673, .T. ) ;
#51557 = EDGE_CURVE ( 'NONE', #34085, #60010, #73408, .T. ) ;
#51558 = CARTESIAN_POINT ( 'NONE',  ( -31.79838993233234490, 1525.159177407156449, 216.1507442378014332 ) ) ;
#51559 = CARTESIAN_POINT ( 'NONE',  ( -3.394304438509999855, 1495.766742855890016, 197.6817022580989942 ) ) ;
#51562 = ORIENTED_EDGE ( 'NONE', *, *, #30684, .T. ) ;
#51561 = CARTESIAN_POINT ( 'NONE',  ( -68.77190087506669158, 1379.747925807530009, 280.3125204381590265 ) ) ;
#51560 = CIRCLE ( 'NONE', #62305, 1.000000000000001554 ) ;
#51563 = B_SPLINE_CURVE_WITH_KNOTS ( 'NONE', 5,
 ( #72819, #21262, #20186, #3424, #54384, #63878, #30794, #3976, #4511, #63339, #73365, #106410 ),
 .UNSPECIFIED., .F., .F.,
 ( 6, 3, 3, 6 ),
 ( 39.80009975441029724, 56.26732510819999789, 56.97897492249999374, 58.84485018950000068 ),
 .UNSPECIFIED. ) ;
#51564 = CARTESIAN_POINT ( 'NONE',  ( 15.68557540059999766, 1410.853897593529837, 191.5168599455980143 ) ) ;
#51565 = ORIENTED_EDGE ( 'NONE', *, *, #90567, .F. ) ;
#51566 = CIRCLE ( 'NONE', #33632, 2.000000000000003553 ) ;
#51567 = CARTESIAN_POINT ( 'NONE',  ( -8.881784197000000993E-16, 1391.913060387289988, 209.1218459616989946 ) ) ;
#51568 = CARTESIAN_POINT ( 'NONE',  ( -24.57539793409999973, 1430.358747824730244, 207.2090478296979938 ) ) ;
#51570 = CARTESIAN_POINT ( 'NONE',  ( 16.57550902493450096, 1410.866907009090028, 191.7134341172800021 ) ) ;
#51569 = CARTESIAN_POINT ( 'NONE',  ( -11.24026918932699992, 1425.602988694570058, 130.8057374633750101 ) ) ;
#51571 = CARTESIAN_POINT ( 'NONE',  ( 7.338411959395000572, 1517.170512887980067, 211.6064236274570192 ) ) ;
#51572 = CARTESIAN_POINT ( 'NONE',  ( 19.80907117253899585, 1509.722913433488202, 186.5213986624754909 ) ) ;
#51573 = VECTOR ( 'NONE', #12176, 1000.000000000000227 ) ;
#51574 = CARTESIAN_POINT ( 'NONE',  ( 1.630002283467431701, 1450.546079252429763, 181.7385653295009149 ) ) ;
#51575 = CARTESIAN_POINT ( 'NONE',  ( -45.67177475829999622, 1440.913060392909983, 266.1885948849979968 ) ) ;
#51576 = CARTESIAN_POINT ( 'NONE',  ( 17.88484985822620033, 1509.549773635790189, 232.6392117127710151 ) ) ;
#51577 = CARTESIAN_POINT ( 'NONE',  ( 17.35588498053416018, 1460.101161736126869, 228.4988312450949195 ) ) ;
#51578 = APPLICATION_PROTOCOL_DEFINITION ( 'draft international standard', 'automotive_design', 1998, #26278 ) ;
#51579 = CARTESIAN_POINT ( 'NONE',  ( 4.850704082057680111, 1508.551704408389924, 212.4235637436360093 ) ) ;
#51580 = CARTESIAN_POINT ( 'NONE',  ( -37.50393792736510079, 1438.236878684590010, 136.5796126580320049 ) ) ;
#51581 = ORIENTED_EDGE ( 'NONE', *, *, #21692, .T. ) ;
#51582 = CARTESIAN_POINT ( 'NONE',  ( 10.77364935086789899, 1398.232638417850012, 200.3335059216469745 ) ) ;
#51583 = CARTESIAN_POINT ( 'NONE',  ( 9.669214496953919991, 1462.615592212159982, 207.8321519686910221 ) ) ;
#51584 = CARTESIAN_POINT ( 'NONE',  ( -17.27928175550000134, 1460.220522733030066, 228.2633105307979804 ) ) ;
#51585 = EDGE_LOOP ( 'NONE', ( #28857, #92506, #11663, #82280 ) ) ;
#51586 = ORIENTED_EDGE ( 'NONE', *, *, #78500, .F. ) ;
#51587 = CARTESIAN_POINT ( 'NONE',  ( 9.837801962708470072, 1453.205870278119846, 211.6882699933420042 ) ) ;
#51588 = CARTESIAN_POINT ( 'NONE',  ( 1.143529715360000064E-14, 1421.542806690330053, 144.1893924737979944 ) ) ;
#51589 = CARTESIAN_POINT ( 'NONE',  ( -14.24503472313680064, 1380.268785586849845, 210.4293653685249978 ) ) ;
#51590 = AXIS2_PLACEMENT_3D ( 'NONE', #61797, #27072, #61256 ) ;
#51591 = CARTESIAN_POINT ( 'NONE',  ( -14.16402923184379858, 1508.451126306549895, 209.7829216516819884 ) ) ;
#51592 = CARTESIAN_POINT ( 'NONE',  ( -1.260434061590582910, 1444.023716841911892, 199.8554606798724365 ) ) ;
#51593 = CARTESIAN_POINT ( 'NONE',  ( 12.51045652733512981, 1414.677402202029953, 211.4999743317719663 ) ) ;
#51594 = CARTESIAN_POINT ( 'NONE',  ( -9.862951377749247683, 1519.551704408389924, 228.3939896778649654 ) ) ;
#51595 = CARTESIAN_POINT ( 'NONE',  ( 9.224564342578489118, 1450.690345550029861, 209.5619459605489965 ) ) ;
#51596 = CARTESIAN_POINT ( 'NONE',  ( 33.79495575609362845, 1443.086052842850904, 154.8158086860452158 ) ) ;
#51597 = CARTESIAN_POINT ( 'NONE',  ( -86.96400225606849688, 1384.826294148989973, 290.4385014204809750 ) ) ;
#51598 = ORIENTED_EDGE ( 'NONE', *, *, #52715, .F. ) ;
#51599 = CARTESIAN_POINT ( 'NONE',  ( -3.456007423304999993, 1516.647534046129977, 202.5739645571870255 ) ) ;
#51600 = CARTESIAN_POINT ( 'NONE',  ( 0.7468175155120010400, 1517.006509894990131, 209.1147170949500094 ) ) ;
#51601 = ORIENTED_EDGE ( 'NONE', *, *, #95406, .F. ) ;
#51602 = CARTESIAN_POINT ( 'NONE',  ( 11.74262852945270019, 1426.700939307690078, 144.5631990736900150 ) ) ;
#51603 = B_SPLINE_CURVE_WITH_KNOTS ( 'NONE', 5,
 ( #14702, #41575, #33699, #83554, #84656, #75186 ),
 .UNSPECIFIED., .F., .F.,
 ( 6, 6 ),
 ( 0.000000000000000000, 1.000000000000000000 ),
 .UNSPECIFIED. ) ;
#51604 = CARTESIAN_POINT ( 'NONE',  ( 4.330052502347664145, 1511.419866573372474, 217.4238689493611787 ) ) ;
#51605 = ORIENTED_EDGE ( 'NONE', *, *, #68016, .T. ) ;
#51606 = CARTESIAN_POINT ( 'NONE',  ( -13.57909981250000087, 1416.568813547830132, 221.8977233994979770 ) ) ;
#51607 = CARTESIAN_POINT ( 'NONE',  ( -15.95383389570000077, 1506.798305147730161, 224.6865364803979901 ) ) ;
#51608 = CARTESIAN_POINT ( 'NONE',  ( 7.009648883750000614, 1508.650232072529889, 235.9040373969980067 ) ) ;
#51609 = CARTESIAN_POINT ( 'NONE',  ( -7.318182648980661398, 1489.884714771882273, 217.2580560210730027 ) ) ;
#51610 = CARTESIAN_POINT ( 'NONE',  ( -5.982287179200000082, 1424.434878864929942, 186.5640619623980001 ) ) ;
#51611 = CARTESIAN_POINT ( 'NONE',  ( -0.4382461997867930226, 1517.051704408389924, 216.6878286752280189 ) ) ;
#51613 = B_SPLINE_CURVE_WITH_KNOTS ( 'NONE', 5,
 ( #61895, #54052, #88178, #20391, #46191, #104415 ),
 .UNSPECIFIED., .F., .F.,
 ( 6, 6 ),
 ( -2.000000000000000000, 0.000000000000000000 ),
 .UNSPECIFIED. ) ;
#51612 = LINE ( 'NONE', #83539, #13752 ) ;
#51614 = CARTESIAN_POINT ( 'NONE',  ( 5.400236726889999339, 1493.509547987889846, 218.8212158057690147 ) ) ;
#51615 = CARTESIAN_POINT ( 'NONE',  ( -25.98205113330000060, 1379.634954421569773, 211.5700168387090230 ) ) ;
#51616 = CARTESIAN_POINT ( 'NONE',  ( 25.28594636015140296, 1472.590752081330038, 206.2214039951899736 ) ) ;
#51618 = CARTESIAN_POINT ( 'NONE',  ( 8.892135936816799813, 1468.525511668620084, 202.2742229671289920 ) ) ;
#51617 = CARTESIAN_POINT ( 'NONE',  ( 17.53810613550000141, 1458.155921961129934, 230.1375793178980302 ) ) ;
#51619 = CARTESIAN_POINT ( 'NONE',  ( 15.45814005882069786, 1507.562498016489826, 226.0579763435260077 ) ) ;
#51620 = EDGE_CURVE ( 'NONE', #65987, #69312, #108263, .T. ) ;
#51621 = CARTESIAN_POINT ( 'NONE',  ( -2.499955718113179959, 1419.779050710960064, 121.7745100861179992 ) ) ;
#51622 = ORIENTED_EDGE ( 'NONE', *, *, #52796, .F. ) ;
#51623 = CARTESIAN_POINT ( 'NONE',  ( 18.42577555256999844, 1424.509265906519886, 223.4215472205989954 ) ) ;
#51624 = CARTESIAN_POINT ( 'NONE',  ( -20.72500064278883158, 1525.697947650517563, 233.5887215935848644 ) ) ;
#51625 = CARTESIAN_POINT ( 'NONE',  ( -2.938567406957015127, 1485.191830619298344, 183.0435406588377703 ) ) ;
#51626 = CARTESIAN_POINT ( 'NONE',  ( -17.52110315343864855, 1410.887420241879909, 192.7668757445707115 ) ) ;
#51628 = ORIENTED_EDGE ( 'NONE', *, *, #22691, .F. ) ;
#51627 = CARTESIAN_POINT ( 'NONE',  ( 0.04897144338186310009, 1515.158513834189989, 204.7948513551449992 ) ) ;
#51629 = CARTESIAN_POINT ( 'NONE',  ( 1.532287138359999856, 1453.154034701829914, 188.6110597941980132 ) ) ;
#51630 = DIRECTION ( 'NONE',  ( -0.8672669759446596238, 0.000000000000000000, 0.4978433412588795792 ) ) ;
#51631 = ADVANCED_FACE ( 'NONE', ( #67500 ), #77541, .T. ) ;
#51632 = CARTESIAN_POINT ( 'NONE',  ( -11.51579808750000034, 1427.983711584930006, 149.6431119016979778 ) ) ;
#51633 = CARTESIAN_POINT ( 'NONE',  ( -10.87386229588725861, 1426.225512375807057, 148.5386954957300247 ) ) ;
#51634 = CARTESIAN_POINT ( 'NONE',  ( -4.039629965989999683, 1440.883721145919935, 185.1940559541980065 ) ) ;
#51635 = CARTESIAN_POINT ( 'NONE',  ( -12.51034970659999956, 1378.851356593469973, 207.9031378000489951 ) ) ;
#51636 = CARTESIAN_POINT ( 'NONE',  ( -10.85852385830536448, 1424.794007418652882, 138.1924915167475660 ) ) ;
#51637 = CARTESIAN_POINT ( 'NONE',  ( -15.16677556006500005, 1513.509764667529907, 223.5894014746669995 ) ) ;
#51638 = CARTESIAN_POINT ( 'NONE',  ( -2.493947715939999643, 1442.756953654919926, 150.6345094620980092 ) ) ;
#51640 = CARTESIAN_POINT ( 'NONE',  ( 10.52837420263239920, 1481.199010226290284, 208.2608686310830137 ) ) ;
#51639 = CARTESIAN_POINT ( 'NONE',  ( -110.0662890209999887, 1385.104992454720104, 296.9550740769589652 ) ) ;
#51641 = CARTESIAN_POINT ( 'NONE',  ( -17.15173707733800157, 1460.896355352879937, 228.2717902142180151 ) ) ;
#51642 = VERTEX_POINT ( 'NONE', #101604 ) ;
#51644 = VECTOR ( 'NONE', #99874, 1000.000000000000000 ) ;
#51643 = CARTESIAN_POINT ( 'NONE',  ( -2.299014068865000038, 1516.811292230880099, 206.2578025137869986 ) ) ;
#51645 = CARTESIAN_POINT ( 'NONE',  ( 27.10793701029999880, 1412.310179361130167, 268.1710502007979926 ) ) ;
#51646 = CARTESIAN_POINT ( 'NONE',  ( -4.363122647530000009, 1409.354802298930053, 121.6099336315979969 ) ) ;
#51647 = CIRCLE ( 'NONE', #94538, 8.000000000000007105 ) ;
#51648 = CARTESIAN_POINT ( 'NONE',  ( 19.16352043740000255, 1449.733021707809939, 192.2423658547980097 ) ) ;
#51649 = CARTESIAN_POINT ( 'NONE',  ( -0.2658531787139999936, 1507.120040072329857, 237.3289624399980084 ) ) ;
#51650 = CARTESIAN_POINT ( 'NONE',  ( 10.81507089421240053, 1424.921187596799882, 144.1620444706739761 ) ) ;
#51651 = CARTESIAN_POINT ( 'NONE',  ( 21.32617020629999871, 1509.431680019330088, 227.8426433468980292 ) ) ;
#51652 = CARTESIAN_POINT ( 'NONE',  ( -32.30068554584597962, 1526.382868172863937, 220.2363794648147746 ) ) ;
#51653 = CARTESIAN_POINT ( 'NONE',  ( -15.06253099230000103, 1415.635739491490085, 205.8115256829090072 ) ) ;
#51654 = CARTESIAN_POINT ( 'NONE',  ( -13.42598331690000002, 1444.386710359030076, 186.9377794141980189 ) ) ;
#51655 = EDGE_CURVE ( 'NONE', #51991, #7508, #20048, .T. ) ;
#51656 = CARTESIAN_POINT ( 'NONE',  ( -5.167079976729559654, 1484.950571581749955, 198.3957337195609796 ) ) ;
#51657 = CARTESIAN_POINT ( 'NONE',  ( -15.94781981578667995, 1419.817486795263449, 210.5094882503032352 ) ) ;
#51658 = CARTESIAN_POINT ( 'NONE',  ( -3.810473913917186373, 1457.645299305861499, 229.1842260504324997 ) ) ;
#51659 = ORIENTED_EDGE ( 'NONE', *, *, #15076, .F. ) ;
#51660 = EDGE_CURVE ( 'NONE', #107071, #48164, #18162, .T. ) ;
#51661 = CARTESIAN_POINT ( 'NONE',  ( -3.432975322854999956, 1511.645462744430006, 201.1048498743170114 ) ) ;
#51662 = CARTESIAN_POINT ( 'NONE',  ( -14.75167259043490020, 1409.428200145470100, 206.7901764737640065 ) ) ;
#51664 = EDGE_CURVE ( 'NONE', #33692, #81968, #41174, .T. ) ;
#51663 = CARTESIAN_POINT ( 'NONE',  ( 11.44928335637692918, 1425.357787524876585, 138.1871431916367499 ) ) ;
#51665 = CARTESIAN_POINT ( 'NONE',  ( -14.75797208140014938, 1418.752374206816057, 201.0754936769993151 ) ) ;
#51666 = CARTESIAN_POINT ( 'NONE',  ( -23.62453004620000030, 1470.926794567029901, 268.8227032888980261 ) ) ;
#51668 = AXIS2_PLACEMENT_3D ( 'NONE', #21665, #55872, #82142 ) ;
#51667 = CARTESIAN_POINT ( 'NONE',  ( -31.32995031131208918, 1523.678648413191695, 196.3423562208917588 ) ) ;
#51669 = CARTESIAN_POINT ( 'NONE',  ( -14.24695065547103034, 1514.160659596399228, 192.5687003935095731 ) ) ;
#51670 = CARTESIAN_POINT ( 'NONE',  ( -24.33268552243512062, 1444.628224150390679, 211.2399863042838888 ) ) ;
#51671 = CARTESIAN_POINT ( 'NONE',  ( -63.30236682719129959, 1384.683505265780013, 286.2651546391219881 ) ) ;
#51672 = CARTESIAN_POINT ( 'NONE',  ( -9.094129269030000629, 1384.954944735329946, 199.9429221374590213 ) ) ;
#51673 = CARTESIAN_POINT ( 'NONE',  ( 18.09890889826640148, 1424.873618492820015, 225.7493724871799827 ) ) ;
#51674 = CARTESIAN_POINT ( 'NONE',  ( 12.18885905831090177, 1416.259629946529913, 223.5006617761420102 ) ) ;
#51675 = EDGE_CURVE ( 'NONE', #44415, #50505, #84809, .T. ) ;
#51676 = CARTESIAN_POINT ( 'NONE',  ( -8.194496425724276278, 1495.378119627901697, 201.4616218148407256 ) ) ;
#51677 = CARTESIAN_POINT ( 'NONE',  ( 33.23571934791667104, 1511.187213306747708, 198.7594255952494962 ) ) ;
#51678 = FACE_OUTER_BOUND ( 'NONE', #72130, .T. ) ;
#51679 = CARTESIAN_POINT ( 'NONE',  ( -23.66755926680000144, 1411.100008216330025, 206.9440434488080029 ) ) ;
#51680 = CARTESIAN_POINT ( 'NONE',  ( 14.45747078059999957, 1416.828040557830036, 196.8519857451980215 ) ) ;
#51681 = CARTESIAN_POINT ( 'NONE',  ( -22.08622291482368283, 1512.187213306747481, 184.4183880513178337 ) ) ;
#51682 = CARTESIAN_POINT ( 'NONE',  ( 11.16961893628350033, 1479.160307786130033, 207.2818337165830087 ) ) ;
#51683 = CARTESIAN_POINT ( 'NONE',  ( -4.046039468759740743, 1455.103744561050235, 203.6879517955759979 ) ) ;
#51684 = CARTESIAN_POINT ( 'NONE',  ( 4.955072371518870256, 1436.062886099170100, 228.7521548814630137 ) ) ;
#51685 = CARTESIAN_POINT ( 'NONE',  ( 17.29393938232457728, 1523.621879633028811, 180.8572348224458324 ) ) ;
#51686 = CARTESIAN_POINT ( 'NONE',  ( -0.03314732912356650046, 1502.038625534309858, 233.2541157079660081 ) ) ;
#51688 = CARTESIAN_POINT ( 'NONE',  ( -9.528525097359999307, 1381.369362415970045, 201.1489852242889924 ) ) ;
#51687 = CARTESIAN_POINT ( 'NONE',  ( 17.17241001986506888, 1518.913060387330006, 238.6251415217915337 ) ) ;
#51689 = CARTESIAN_POINT ( 'NONE',  ( 11.72625744468970055, 1426.702793517190003, 143.3981854150229935 ) ) ;
#51690 = CARTESIAN_POINT ( 'NONE',  ( 11.75869035672759999, 1519.551704408389924, 227.2994842695800060 ) ) ;
#51691 = CARTESIAN_POINT ( 'NONE',  ( -11.38785606999999978, 1490.657837854590070, 209.9657568313180036 ) ) ;
#51692 = CARTESIAN_POINT ( 'NONE',  ( 7.361562866177969511, 1448.713196798179979, 201.9147366591519983 ) ) ;
#51693 = CARTESIAN_POINT ( 'NONE',  ( -17.25022837948109711, 1507.614846716840020, 224.2951197320900008 ) ) ;
#51694 = CARTESIAN_POINT ( 'NONE',  ( 1.706797785944999868, 1517.164987839469859, 203.3324512698969784 ) ) ;
#51695 = CARTESIAN_POINT ( 'NONE',  ( -10.57136850119649374, 1398.226370804211456, 216.7217188148681544 ) ) ;
#51696 = CARTESIAN_POINT ( 'NONE',  ( -4.045957869977510057, 1440.951247040982707, 156.1595413419819920 ) ) ;
#51697 = FACE_BOUND ( 'NONE', #63264, .T. ) ;
#51698 = CARTESIAN_POINT ( 'NONE',  ( 1.430007510489999856, 1507.678536141130053, 236.8162301602979767 ) ) ;
#51699 = ADVANCED_FACE ( 'NONE', ( #68055 ), #41722, .F. ) ;
#51700 = SURFACE_SIDE_STYLE ('',( #86390 ) ) ;
#51701 = CIRCLE ( 'NONE', #53475, 28.41070217520000440 ) ;
#51702 = CARTESIAN_POINT ( 'NONE',  ( -9.927720267860891568, 1422.647037618466356, 210.6683186352579185 ) ) ;
#51704 = ORIENTED_EDGE ( 'NONE', *, *, #109148, .T. ) ;
#51703 = CARTESIAN_POINT ( 'NONE',  ( -65.35806189339839989, 1379.740364976560159, 275.4909032779769973 ) ) ;
#51705 = ORIENTED_EDGE ( 'NONE', *, *, #19215, .T. ) ;
#51706 = CARTESIAN_POINT ( 'NONE',  ( 11.96561352722999949, 1433.598104579079973, 150.0754075377500101 ) ) ;
#51707 = CARTESIAN_POINT ( 'NONE',  ( 27.04486969230000071, 1509.634167057629838, 216.9802351812680001 ) ) ;
#51708 = ORIENTED_EDGE ( 'NONE', *, *, #38008, .F. ) ;
#51709 = CARTESIAN_POINT ( 'NONE',  ( -3.641325192198154870, 1462.848003559786548, 199.9870330951486324 ) ) ;
#51710 = CARTESIAN_POINT ( 'NONE',  ( -23.82022599419999764, 1509.070378065730210, 195.5050499778980111 ) ) ;
#51711 = CARTESIAN_POINT ( 'NONE',  ( -7.785551154210000213, 1385.415854725780036, 218.8883729281390060 ) ) ;
#51714 = EDGE_CURVE ( 'NONE', #74194, #75452, #52903, .T. ) ;
#51713 = CARTESIAN_POINT ( 'NONE',  ( 9.110233712619999480, 1428.462521060929930, 112.4493539157979995 ) ) ;
#51712 = CARTESIAN_POINT ( 'NONE',  ( -1.333619433810000254, 1444.154719577489914, 199.5606630350989974 ) ) ;
#51715 = CARTESIAN_POINT ( 'NONE',  ( 19.64145264752830045, 1498.117040017750014, 228.8701979158510085 ) ) ;
#51716 =( BOUNDED_SURFACE ( )  B_SPLINE_SURFACE ( 3, 2, ( 
 ( #10301, #19803, #87010 ),
 ( #80280, #36614, #36074 ),
 ( #70259, #104367, #28212 ),
 ( #98163, #89222, #45596 ),
 ( #104927, #97084, #12517 ),
 ( #27663, #79738, #3046 ) ),
 .UNSPECIFIED., .F., .F., .T. ) 
 B_SPLINE_SURFACE_WITH_KNOTS ( ( 4, 2, 4 ),
 ( 3, 3 ),
 ( -2.103352214621878602E-17, 0.001312027981647337967, 0.002624055963294697185 ),
 ( 0.000000000000000000, 1.000000000000000000 ),
 .UNSPECIFIED. ) 
 GEOMETRIC_REPRESENTATION_ITEM ( )  RATIONAL_B_SPLINE_SURFACE ( (
 ( 1.000000000000000000, 0.9376006582765896713, 1.000000000000000000),
 ( 1.000000000000000000, 0.9569320108030433536, 1.000000000000000000),
 ( 1.000000000000000000, 0.9725743441608392104, 1.000000000000000000),
 ( 1.000000000000000000, 0.9942095667146111371, 1.000000000000000000),
 ( 1.000000000000000000, 1.000043666449921265, 1.000000000000000000),
 ( 1.000000000000000000, 1.000000000000000000, 1.000000000000000000) ) ) 
 REPRESENTATION_ITEM ( '' )  SURFACE ( )  );
#51717 = CIRCLE ( 'NONE', #110676, 2.000000000000001776 ) ;
#51718 = CARTESIAN_POINT ( 'NONE',  ( 4.365873002549999882, 1507.637804422629870, 181.7436736497979837 ) ) ;
#51719 = COLOUR_RGB ( '', 0.72549020, 0.75294118, 0.79215686) ;
#51720 = CARTESIAN_POINT ( 'NONE',  ( 3.172882057879999884, 1467.373998898590116, 218.6974008828489673 ) ) ;
#51721 = CARTESIAN_POINT ( 'NONE',  ( 16.17522453369999980, 1409.477911658830180, 225.6432838665979830 ) ) ;
#51722 = SURFACE_STYLE_FILL_AREA ( #50068 ) ;
#51723 = B_SPLINE_SURFACE_WITH_KNOTS ( 'NONE', 5, 5, ( 
 ( #97992, #12334, #46525, #73363, #5042, #106408 ),
 ( #80659, #82307, #81734, #22364, #30235, #30792 ),
 ( #5605, #107500, #64971, #45966, #106949, #21259 ),
 ( #64426, #56565, #39756, #108046, #65527, #75025 ),
 ( #100208, #49824, #109176, #16177, #110255, #76115 ),
 ( #83953, #57684, #31897, #101277, #24574, #58765 ),
 ( #67731, #59336, #92345, #93446, #82850, #110810 ),
 ( #15617, #58220, #66082, #23492, #15075, #6140 ),
 ( #14536, #7254, #91798, #92903, #8338, #33529 ) ),
 .UNSPECIFIED., .F., .F., .F.,
 ( 6, 3, 6 ),
 ( 6, 6 ),
 ( 3.132904301029519889, 5.380600720280000360, 7.628289045712770111 ),
 ( -0.0004171348989584099847, 2.000000000000000000 ),
 .UNSPECIFIED. ) ;
#51724 = CARTESIAN_POINT ( 'NONE',  ( 2.881222757585000238, 1516.891731298979948, 211.5992195760969707 ) ) ;
#51725 = CARTESIAN_POINT ( 'NONE',  ( 13.46591420274270057, 1415.020374543940079, 197.8571796951229942 ) ) ;
#51726 = CARTESIAN_POINT ( 'NONE',  ( 11.57593930269999838, 1432.295998248850083, 151.1968184610979620 ) ) ;
#51727 = CARTESIAN_POINT ( 'NONE',  ( 8.080850430355001279, 1512.335510084610178, 202.5241399173669947 ) ) ;
#51728 = ORIENTED_EDGE ( 'NONE', *, *, #13834, .T. ) ;
#51729 = CARTESIAN_POINT ( 'NONE',  ( 13.76712058163199970, 1435.795625921070041, 150.2004772032130120 ) ) ;
#51730 = ORIENTED_EDGE ( 'NONE', *, *, #1511, .T. ) ;
#51731 = ORIENTED_EDGE ( 'NONE', *, *, #67624, .F. ) ;
#51732 = CARTESIAN_POINT ( 'NONE',  ( 12.99399919968730011, 1444.879491996346360, 169.4223100370116981 ) ) ;
#51733 = CARTESIAN_POINT ( 'NONE',  ( -1.085166694420000022, 1466.317866144730033, 235.5238959666980065 ) ) ;
#51734 = CARTESIAN_POINT ( 'NONE',  ( -8.305592643558565413, 1474.704246973548607, 203.0641412134559403 ) ) ;
#51735 = CARTESIAN_POINT ( 'NONE',  ( -7.329303116114999739, 1516.857992118400034, 216.4524001036569985 ) ) ;
#51736 = CARTESIAN_POINT ( 'NONE',  ( -8.147601308547534060, 1511.509050022407564, 212.9717243131179316 ) ) ;
#51737 = B_SPLINE_SURFACE_WITH_KNOTS ( 'NONE', 5, 5, ( 
 ( #5882, #55758, #23213, #57951, #38908, #65797, #92084, #39482, #108886 ),
 ( #107784, #32730, #99361, #48453, #6432, #14816, #89876, #31069, #98274 ),
 ( #57413, #82018, #47330, #64710, #81459, #4764, #65250, #73090, #41127 ),
 ( #56842, #90974, #5323, #108336, #100482, #74206, #107230, #31619, #99918 ),
 ( #98828, #49003, #22088, #56285, #23764, #49551, #90415, #6973, #75307 ),
 ( #68563, #110539, #94278, #15901, #33272, #58498, #8617, #24854, #50101 ) ),
 .UNSPECIFIED., .F., .F., .F.,
 ( 6, 6 ),
 ( 6, 3, 6 ),
 ( 1.365479238354990077, 2.643755244583379849 ),
 ( 0.000000000000000000, 1.000000000000000000, 2.000011373467919906 ),
 .UNSPECIFIED. ) ;
#51738 = VECTOR ( 'NONE', #67191, 1000.000000000000114 ) ;
#51739 = CARTESIAN_POINT ( 'NONE',  ( 12.39400990049870011, 1421.652661456120086, 207.6978078727499906 ) ) ;
#51740 = CARTESIAN_POINT ( 'NONE',  ( -35.62143398542752237, 1379.642029864801543, 218.5761008737005398 ) ) ;
#51741 = CARTESIAN_POINT ( 'NONE',  ( -3.771520288500000539, 1375.389610323599982, 208.3364477064349956 ) ) ;
#51742 = CIRCLE ( 'NONE', #3468, 1.999999999999999556 ) ;
#51743 = ORIENTED_EDGE ( 'NONE', *, *, #19250, .T. ) ;
#51744 = CARTESIAN_POINT ( 'NONE',  ( 4.609064303374999838, 1516.723920667490120, 206.2441009858569885 ) ) ;
#51745 = ORIENTED_EDGE ( 'NONE', *, *, #79451, .F. ) ;
#51746 = CARTESIAN_POINT ( 'NONE',  ( 22.91311234439279687, 1440.913060387330006, 231.3965099084779808 ) ) ;
#51747 = CARTESIAN_POINT ( 'NONE',  ( -19.01903537849999992, 1509.560719700929894, 231.2847914768979933 ) ) ;
#51748 = ORIENTED_EDGE ( 'NONE', *, *, #24232, .T. ) ;
#51749 = CARTESIAN_POINT ( 'NONE',  ( -5.751971152109999430, 1409.281467972630026, 187.6758683908980174 ) ) ;
#51750 = CARTESIAN_POINT ( 'NONE',  ( 7.692900448525000101, 1514.487275757750012, 214.9404204251670194 ) ) ;
#51752 = VERTEX_POINT ( 'NONE', #54572 ) ;
#51751 = CARTESIAN_POINT ( 'NONE',  ( -11.36018337610000195, 1414.996442546130083, 195.9645814914979951 ) ) ;
#51753 = CARTESIAN_POINT ( 'NONE',  ( 22.56647849180000165, 1431.126951193569994, 217.0164414152080212 ) ) ;
#51754 = CARTESIAN_POINT ( 'NONE',  ( -16.17659802858249662, 1508.551704408389924, 210.3807973950520136 ) ) ;
#51755 = CARTESIAN_POINT ( 'NONE',  ( -106.4197298790000019, 1384.588767362379940, 311.3121942672589739 ) ) ;
#51756 = CARTESIAN_POINT ( 'NONE',  ( 8.225616979109998894, 1452.226705206789802, 213.5360760307489727 ) ) ;
#51757 = DIRECTION ( 'NONE',  ( -0.6736849260863839728, 0.000000000000000000, 0.7390186874254150995 ) ) ;
#51758 = CIRCLE ( 'NONE', #76751, 7.500000000000000000 ) ;
#51759 = B_SPLINE_SURFACE_WITH_KNOTS ( 'NONE', 5, 5, ( 
 ( #38049, #28545, #45371, #78399, #96863, #72226 ),
 ( #104146, #19011, #53212, #87353, #10649, #44816 ),
 ( #78970, #2275, #62175, #96301, #19581, #79511 ),
 ( #71131, #22866, #39128, #107442, #56513, #12835 ),
 ( #30177, #40244, #47015, #55961, #13367, #108553 ),
 ( #74426, #23437, #66028, #109123, #4983, #73307 ),
 ( #82796, #81139, #57072, #100151, #89544, #47556 ),
 ( #48672, #106888, #4455, #83345, #57631, #38582 ),
 ( #81677, #72761, #91199, #31843, #64369, #31290 ),
 ( #82248, #91745, #99583, #30739, #22310, #90640 ),
 ( #98491, #99033, #15021, #21760, #40797, #6642 ),
 ( #32403, #49219, #13921, #100689, #23972, #74975 ) ),
 .UNSPECIFIED., .F., .F., .F.,
 ( 6, 3, 3, 6 ),
 ( 6, 6 ),
 ( 5.135474514900000287, 7.195071677909999686, 11.31426600390000026, 15.30658226960000157 ),
 ( 0.000000000000000000, 2.031188710939999975 ),
 .UNSPECIFIED. ) ;
#51760 = CARTESIAN_POINT ( 'NONE',  ( 4.037378256055000669, 1516.688761843659904, 215.6706679112870120 ) ) ;
#51761 = CARTESIAN_POINT ( 'NONE',  ( 1.946290797379999882, 1468.809136692889979, 216.1326187760289770 ) ) ;
#51762 = CARTESIAN_POINT ( 'NONE',  ( -21.25831203310000106, 1509.376731495729928, 190.0552735725980256 ) ) ;
#51763 = CARTESIAN_POINT ( 'NONE',  ( 21.91520783698931751, 1524.538768545234007, 184.5727256433340244 ) ) ;
#51764 = CARTESIAN_POINT ( 'NONE',  ( 1.717432448265000078, 1516.836638729160086, 211.4041475482669910 ) ) ;
#51765 = CARTESIAN_POINT ( 'NONE',  ( -11.79975722151939976, 1482.296391875749805, 207.6022922335340297 ) ) ;
#51766 = CARTESIAN_POINT ( 'NONE',  ( -15.48152669746104060, 1486.079334726010075, 186.6356546698670513 ) ) ;
#51768 = EDGE_LOOP ( 'NONE', ( #52138, #57230, #22463, #62228 ) ) ;
#51767 = CARTESIAN_POINT ( 'NONE',  ( -85.78494180500000255, 1386.745275533519816, 289.7710778616590233 ) ) ;
#51769 = CARTESIAN_POINT ( 'NONE',  ( -63.98031756861389852, 1385.047684693189922, 287.2751599999480163 ) ) ;
#51770 = CARTESIAN_POINT ( 'NONE',  ( 33.60183515439999979, 1440.913060383429865, 248.0844435622979915 ) ) ;
#51771 = CARTESIAN_POINT ( 'NONE',  ( 2.851403222469678145, 1451.784497409910728, 183.8440006949768701 ) ) ;
#51772 = CARTESIAN_POINT ( 'NONE',  ( 3.272667022753707577, 1522.051704408389924, 229.2073556998901438 ) ) ;
#51773 = CARTESIAN_POINT ( 'NONE',  ( -5.272191020579219511, 1507.500514379029937, 236.2607515669679970 ) ) ;
#51774 = B_SPLINE_CURVE_WITH_KNOTS ( 'NONE', 3,
 ( #39416, #48387, #108823, #50035, #7464, #109933, #33211, #98765, #22027, #82530, #5826, #108272, #31558, #93116, #51135, #44400, #26461, #50582, #86931, #67400, #16386, #16933 ),
 .UNSPECIFIED., .F., .F.,
 ( 4, 3, 3, 3, 3, 3, 3, 4 ),
 ( 10.65476131940000037, 12.10693589158530159, 12.77474861870000034, 14.28402943510999989, 15.71731362297010115, 16.21876727693750198, 17.58349865633480036, 18.78936860560000000 ),
 .UNSPECIFIED. ) ;
#51775 = CARTESIAN_POINT ( 'NONE',  ( -18.15654714260000091, 1466.352650648189865, 200.0994765531190183 ) ) ;
#51777 = CARTESIAN_POINT ( 'NONE',  ( 19.74853702200000427, 1455.472137956930283, 226.4474092902979976 ) ) ;
#51776 = CARTESIAN_POINT ( 'NONE',  ( -10.41132050640263174, 1522.051704408389924, 189.4661702785461728 ) ) ;
#51778 = LINE ( 'NONE', #59083, #71091 ) ;
#51779 = CARTESIAN_POINT ( 'NONE',  ( -106.9567297613849917, 1382.281980269420046, 310.2341151030279320 ) ) ;
#51780 = ORIENTED_EDGE ( 'NONE', *, *, #60395, .T. ) ;
#51781 = CARTESIAN_POINT ( 'NONE',  ( -1.711311266675000109, 1516.591755933730155, 203.3510257909670145 ) ) ;
#51782 = CARTESIAN_POINT ( 'NONE',  ( -10.71865670083870192, 1508.438609848949909, 218.4505424401079949 ) ) ;
#51783 = CARTESIAN_POINT ( 'NONE',  ( 27.68253990799999897, 1507.989615297430191, 207.6661388674179989 ) ) ;
#51784 = CIRCLE ( 'NONE', #82134, 33.13701971169416538 ) ;
#51785 = CARTESIAN_POINT ( 'NONE',  ( 24.57684147700000210, 1440.965848065480031, 212.8359072196480213 ) ) ;
#51786 = CARTESIAN_POINT ( 'NONE',  ( -9.234134023826198856, 1461.205490114660051, 206.1827678865119822 ) ) ;
#51787 = CARTESIAN_POINT ( 'NONE',  ( 3.313200396079999610, 1466.616402805890175, 219.2512007924990201 ) ) ;
#51788 = DIRECTION ( 'NONE',  ( 0.000000000000000000, 0.000000000000000000, 1.000000000000000000 ) ) ;
#51789 = CARTESIAN_POINT ( 'NONE',  ( 30.84776965385309921, 1436.903798512589901, 136.6563984318939902 ) ) ;
#51790 = CARTESIAN_POINT ( 'NONE',  ( -26.03280816719999891, 1448.977735834329906, 137.1485333417979859 ) ) ;
#51791 = CARTESIAN_POINT ( 'NONE',  ( -12.27023110815660090, 1416.839692126590080, 194.6640136892829958 ) ) ;
#51792 = CARTESIAN_POINT ( 'NONE',  ( -2.348673686699999763, 1430.656302287590051, 201.0926571014589967 ) ) ;
#51793 = EDGE_CURVE ( 'NONE', #29992, #12956, #2514, .T. ) ;
#51794 = CARTESIAN_POINT ( 'NONE',  ( 6.937425782160731025, 1464.940099892885883, 217.7535805317997131 ) ) ;
#51795 = CARTESIAN_POINT ( 'NONE',  ( -9.244895511235538876, 1448.612347789799969, 209.9869602076240085 ) ) ;
#51796 = ORIENTED_EDGE ( 'NONE', *, *, #91968, .F. ) ;
#51797 = AXIS2_PLACEMENT_3D ( 'NONE', #13397, #5015, #6671 ) ;
#51798 = CARTESIAN_POINT ( 'NONE',  ( -39.47393889809999479, 1426.323565199129916, 271.1218459616979999 ) ) ;
#51799 = CARTESIAN_POINT ( 'NONE',  ( 1.953870304974810068, 1456.496003654670176, 219.5623012099979690 ) ) ;
#51800 = CARTESIAN_POINT ( 'NONE',  ( -4.833437661688551046, 1508.551704408389924, 213.0319860769199920 ) ) ;
#51801 = PLANE ( 'NONE',  #16676 ) ;
#51802 = CARTESIAN_POINT ( 'NONE',  ( 10.93642306640074224, 1424.903169850106678, 138.2808805187167707 ) ) ;
#51804 = DIRECTION ( 'NONE',  ( 0.000000000000000000, -1.000000000000000000, 6.123233995736769734E-17 ) ) ;
#51803 = CARTESIAN_POINT ( 'NONE',  ( 11.45577218270000053, 1502.286415152389964, 208.3140800519860250 ) ) ;
#51805 = CARTESIAN_POINT ( 'NONE',  ( -12.93281143504288089, 1444.916649965908391, 186.1917424862305381 ) ) ;
#51806 = CARTESIAN_POINT ( 'NONE',  ( 7.919198134229999297, 1428.084552926790138, 213.0326556074190307 ) ) ;
#51807 = CARTESIAN_POINT ( 'NONE',  ( -12.99960798169789911, 1384.882413778849923, 219.0844187336040250 ) ) ;
#51808 = TOROIDAL_SURFACE ( 'NONE', #103671, 7.016581249619999738, 2.000000000000000000 ) ;
#51809 = CARTESIAN_POINT ( 'NONE',  ( -13.70524990486647887, 1420.114476090270955, 227.7448751836718372 ) ) ;
#51811 = EDGE_CURVE ( 'NONE', #41235, #49802, #49426, .T. ) ;
#51810 = CARTESIAN_POINT ( 'NONE',  ( -7.686253120226395730, 1451.400019608767252, 153.0367187530530941 ) ) ;
#51812 = CARTESIAN_POINT ( 'NONE',  ( -18.06717587838990013, 1416.826860677879949, 209.3441468771879954 ) ) ;
#51813 = CARTESIAN_POINT ( 'NONE',  ( 25.09552600510000175, 1436.154465690999814, 137.4570931897980017 ) ) ;
#51814 = CARTESIAN_POINT ( 'NONE',  ( -6.458058201505220808, 1396.138580749159928, 200.1630282699710222 ) ) ;
#51816 = ORIENTED_EDGE ( 'NONE', *, *, #53466, .T. ) ;
#51815 = B_SPLINE_CURVE_WITH_KNOTS ( 'NONE', 5,
 ( #78155, #55059, #5174, #95513, #36166, #44019, #103911, #30922, #89186, #12478, #61392, #18783 ),
 .UNSPECIFIED., .F., .F.,
 ( 6, 3, 3, 6 ),
 ( -8.927001670169998349, -7.815970586829999789, -6.076675143260000134, -3.686514310899999813 ),
 .UNSPECIFIED. ) ;
#51817 = CARTESIAN_POINT ( 'NONE',  ( -17.12363160903159809, 1410.143831958050214, 225.8068293093689931 ) ) ;
#51818 = CARTESIAN_POINT ( 'NONE',  ( -13.40902085879850070, 1483.658216990520032, 225.6646531694549935 ) ) ;
#51819 = EDGE_CURVE ( 'NONE', #79854, #53940, #78861, .T. ) ;
#51820 = VERTEX_POINT ( 'NONE', #10322 ) ;
#51821 = ORIENTED_EDGE ( 'NONE', *, *, #40774, .T. ) ;
#51822 = DIRECTION ( 'NONE',  ( -1.987380029059999976E-13, 6.832419524060000430E-15, 1.000000000000000000 ) ) ;
#51823 = CARTESIAN_POINT ( 'NONE',  ( -14.82486707557663586, 1416.127778529439411, 204.8631623252366580 ) ) ;
#51825 = CARTESIAN_POINT ( 'NONE',  ( -2.676030461421510243, 1457.817666378469767, 219.4510933441680152 ) ) ;
#51824 = CARTESIAN_POINT ( 'NONE',  ( 10.70864553689999887, 1425.696178928829795, 94.99429751269789790 ) ) ;
#51826 = B_SPLINE_CURVE_WITH_KNOTS ( 'NONE', 3,
 ( #73462, #107593, #4595, #38729 ),
 .UNSPECIFIED., .F., .F.,
 ( 4, 4 ),
 ( 0.000000000000000000, 0.0002960034161023842431 ),
 .UNSPECIFIED. ) ;
#51827 = CARTESIAN_POINT ( 'NONE',  ( -11.87502380990000006, 1433.007271236840097, 149.9804568709980117 ) ) ;
#51828 = CIRCLE ( 'NONE', #44726, 1.999999999999998668 ) ;
#51829 = CARTESIAN_POINT ( 'NONE',  ( -109.9698195215979979, 1384.452562162210143, 311.4357956501490321 ) ) ;
#51830 = CARTESIAN_POINT ( 'NONE',  ( -2.582675909241389345, 1526.178928173327677, 242.3428666835333445 ) ) ;
#51831 = CARTESIAN_POINT ( 'NONE',  ( -20.36853080839999919, 1464.956632876090225, 210.9458194778790130 ) ) ;
#51832 = CARTESIAN_POINT ( 'NONE',  ( 7.865891863719999932, 1508.177616610530094, 182.6824962180979810 ) ) ;
#51833 = CARTESIAN_POINT ( 'NONE',  ( 2.493346804579999798, 1449.100684543890111, 182.3308732938979801 ) ) ;
#51834 = CARTESIAN_POINT ( 'NONE',  ( 8.000294350727555681, 1364.913589071355318, 209.6218459617148824 ) ) ;
#51836 = ORIENTED_EDGE ( 'NONE', *, *, #74750, .F. ) ;
#51835 = CARTESIAN_POINT ( 'NONE',  ( 5.183480683570000025, 1454.129157349589832, 216.9717332163589845 ) ) ;
#51837 = ORIENTED_EDGE ( 'NONE', *, *, #3615, .T. ) ;
#51838 = DIRECTION ( 'NONE',  ( 1.000000000000000000, 0.000000000000000000, 0.000000000000000000 ) ) ;
#51839 = CARTESIAN_POINT ( 'NONE',  ( -21.61356760059999971, 1507.917715158790088, 209.5243360325540039 ) ) ;
#51840 = CARTESIAN_POINT ( 'NONE',  ( -1.438086367899999773, 1472.604997560230004, 270.3713140929979772 ) ) ;
#51841 = CARTESIAN_POINT ( 'NONE',  ( 12.60016312909735881, 1434.521797930790854, 147.2295963768206661 ) ) ;
#51843 = EDGE_CURVE ( 'NONE', #60672, #91618, #52680, .T. ) ;
#51842 = CARTESIAN_POINT ( 'NONE',  ( -3.476453357950000100, 1485.977928129130078, 182.2504961336979932 ) ) ;
#51844 = CARTESIAN_POINT ( 'NONE',  ( -32.32093690483954163, 1524.075000532257718, 202.1437793362934485 ) ) ;
#51845 = CARTESIAN_POINT ( 'NONE',  ( 1.953691794509409663, 1476.191320038690037, 197.7993456081649981 ) ) ;
#51846 = CARTESIAN_POINT ( 'NONE',  ( -35.15227308153860264, 1451.683551734719913, 135.1171324062460144 ) ) ;
#51847 = FACE_OUTER_BOUND ( 'NONE', #87118, .T. ) ;
#51848 = CARTESIAN_POINT ( 'NONE',  ( -16.48401273470000206, 1408.913060387329779, 201.9064470506779685 ) ) ;
#51849 = CARTESIAN_POINT ( 'NONE',  ( 8.402703615647871160, 1368.786815462734921, 210.6218459617030021 ) ) ;
#51850 = FACE_OUTER_BOUND ( 'NONE', #61167, .T. ) ;
#51851 = CARTESIAN_POINT ( 'NONE',  ( -18.60991398711139766, 1409.400608050520077, 269.3767701890689636 ) ) ;
#51852 = CARTESIAN_POINT ( 'NONE',  ( -14.07097133599449990, 1435.229630904430223, 149.3999849555079891 ) ) ;
#51853 = ORIENTED_EDGE ( 'NONE', *, *, #93471, .F. ) ;
#51854 = CARTESIAN_POINT ( 'NONE',  ( -11.76883255979999987, 1432.286228545659924, 150.8119424982980092 ) ) ;
#51855 = CARTESIAN_POINT ( 'NONE',  ( 13.12953739719999824, 1444.897984030819998, 187.7977427021979793 ) ) ;
#51856 = B_SPLINE_SURFACE_WITH_KNOTS ( 'NONE', 5, 5, ( 
 ( #84994, #32940, #43573, #92852, #41911, #8289 ),
 ( #67129, #35158, #25081, #68792, #58717, #50334 ),
 ( #51411, #85542, #84460, #76065, #95074, #1035 ),
 ( #34606, #8839, #59284, #17772, #93402, #42451 ),
 ( #76611, #102892, #110763, #94500, #34053, #483 ),
 ( #102353, #25636, #77180, #26191, #60379, #55713 ),
 ( #36266, #1579, #27870, #56796, #70455, #5280 ),
 ( #98782, #89834, #38322, #47839, #64665, #38868 ),
 ( #65206, #81972, #39436, #4724, #13106, #87225 ) ),
 .UNSPECIFIED., .F., .F., .F.,
 ( 6, 3, 6 ),
 ( 6, 6 ),
 ( 0.7655572723410000169, 2.316155491850000026, 3.835724788409999864 ),
 ( 0.000000000000000000, 1.000000000000000000 ),
 .UNSPECIFIED. ) ;
#51857 = ORIENTED_EDGE ( 'NONE', *, *, #98653, .F. ) ;
#51858 = EDGE_LOOP ( 'NONE', ( #60971, #39718 ) ) ;
#51859 = CARTESIAN_POINT ( 'NONE',  ( 13.92686551478569967, 1517.051704405520013, 192.0624604828410043 ) ) ;
#51860 = CARTESIAN_POINT ( 'NONE',  ( -6.376409808257103684, 1368.420764496007678, 207.6218459616990231 ) ) ;
#51861 = CARTESIAN_POINT ( 'NONE',  ( -2.285487619494999567, 1517.001127920769704, 213.1661676502270097 ) ) ;
#51862 = CARTESIAN_POINT ( 'NONE',  ( -14.01202549919999996, 1470.465034534930055, 187.2960763698980031 ) ) ;
#51863 = ORIENTED_EDGE ( 'NONE', *, *, #93209, .T. ) ;
#51864 = DIRECTION ( 'NONE',  ( -0.9942586961433749204, 0.000000000000000000, 0.1070030146457375819 ) ) ;
#51865 = CARTESIAN_POINT ( 'NONE',  ( 9.382531478650001588, 1414.913060387329779, 223.2369444284979920 ) ) ;
#51866 = CARTESIAN_POINT ( 'NONE',  ( -7.334328310795000583, 1517.005755693489846, 204.1179978101270081 ) ) ;
#51867 = CIRCLE ( 'NONE', #12536, 1.999999999999994227 ) ;
#51868 = CARTESIAN_POINT ( 'NONE',  ( -26.99539266469999887, 1509.166234529530129, 202.5158776357180272 ) ) ;
#51869 = B_SPLINE_SURFACE_WITH_KNOTS ( 'NONE', 5, 5, ( 
 ( #24211, #88271, #32081, #45740, #109356, #30424, #99263, #57855, #3191, #5793, #15259, #90321, #32636, #73557, #81924, #107691, #30974, #99820, #56743, #14167, #48352, #82492, #74103, #39935, #31519, #7427, #68462 ),
 ( #69576, #60061, #18016, #159, #85224, #85785, #77941, #101463, #59504, #109893, #9622, #86336, #84128, #41593, #67913, #75748, #103122, #43791, #42140, #93077, #33172, #102566, #69017, #34282, #1248, #43250, #24749 ),
 ( #35388, #84674, #103694, #26423, #94178, #25859, #60617, #102020, #94738, #25304, #42691, #51099, #58398, #67362, #17449, #58947, #16352, #7973, #701, #51648, #50549, #76290, #34831, #52211, #92523, #110440, #9084 ),
 ( #15791, #33720, #49992, #93615, #16894, #8516, #77399, #76849, #2375, #36491, #95301, #35951, #44923, #71232, #27540, #97500, #29194, #20768, #54428, #61722, #61183, #70137, #78503, #88561, #18561, #104249, #95844 ),
 ( #19112, #70688, #38137, #80146, #1814, #96962, #86889, #37594, #3466, #104800, #45474, #105355, #71796, #53315, #54968, #52756, #28646, #87458, #11844, #62849, #89095, #2921, #10752, #79070, #46017, #28088, #62275 ),
 ( #105914, #19681, #96405, #10184, #20227, #44358, #63384, #53886, #88022, #11306, #79617, #37038, #12382, #46568, #80703, #4012, #72319, #26994, #73406, #57721, #55511, #5080, #108647, #107544, #91839, #89640, #39231 ) ),
 .UNSPECIFIED., .F., .F., .F.,
 ( 6, 6 ),
 ( 6, 3, 3, 3, 3, 3, 3, 3, 6 ),
 ( 2.177958220529999878, 99.41336299639999652 ),
 ( 27.66640414800000158, 34.17054740399999702, 36.60181165779999901, 37.81744378469999646, 38.42525984819999962, 39.03307591160000101, 39.44347959870000153, 39.85388328589999674, 40.67469066009999779 ),
 .UNSPECIFIED. ) ;
#51870 = CARTESIAN_POINT ( 'NONE',  ( -3.034964906435000387, 1517.051704408389924, 217.3038049130670117 ) ) ;
#51871 = CARTESIAN_POINT ( 'NONE',  ( -31.92565964530000144, 1384.834792386509889, 206.3014967088990090 ) ) ;
#51872 = CARTESIAN_POINT ( 'NONE',  ( -63.95720680553800008, 1384.698108589110234, 252.7292494320779781 ) ) ;
#51873 = CARTESIAN_POINT ( 'NONE',  ( -5.805073486770000457, 1409.115778020430298, 195.2388944971980038 ) ) ;
#51874 = DIRECTION ( 'NONE',  ( 0.9455185755993178454, 0.000000000000000000, -0.3255681544571537578 ) ) ;
#51875 = AXIS2_PLACEMENT_3D ( 'NONE', #20143, #46486, #96314 ) ;
#51877 = VERTEX_POINT ( 'NONE', #11986 ) ;
#51876 = CARTESIAN_POINT ( 'NONE',  ( -9.042061235680000308, 1445.734082586790009, 185.2473999953979842 ) ) ;
#51878 = CARTESIAN_POINT ( 'NONE',  ( -31.23437356469455040, 1511.187213306747708, 197.3468678195118287 ) ) ;
#51879 = CARTESIAN_POINT ( 'NONE',  ( 27.33420534990000306, 1488.691127165830039, 209.8949700443229744 ) ) ;
#51880 = CARTESIAN_POINT ( 'NONE',  ( 20.10214423559910202, 1487.444758163989945, 225.8674582954020025 ) ) ;
#51881 = CARTESIAN_POINT ( 'NONE',  ( -25.54454699020000064, 1436.325264848330107, 137.1090852991980285 ) ) ;
#51883 = CARTESIAN_POINT ( 'NONE',  ( -4.027697264044999947, 1516.766397346390022, 212.0005392193770035 ) ) ;
#51882 = AXIS2_PLACEMENT_3D ( 'NONE', #94636, #93525, #604 ) ;
#51884 = CARTESIAN_POINT ( 'NONE',  ( -68.44345568869999852, 1379.747786969579920, 279.4410717829589430 ) ) ;
#51885 = CARTESIAN_POINT ( 'NONE',  ( -13.93822302919999956, 1413.184296187929931, 227.1928256324979998 ) ) ;
#51886 = CARTESIAN_POINT ( 'NONE',  ( -29.75840146891882654, 1525.320849883639312, 222.0114828297162717 ) ) ;
#51887 = CARTESIAN_POINT ( 'NONE',  ( -3.460866208815000178, 1517.020847257979995, 208.3861469975149987 ) ) ;
#51888 = VERTEX_POINT ( 'NONE', #103838 ) ;
#51889 = CARTESIAN_POINT ( 'NONE',  ( -1.772459524117049989, 1451.934256328719812, 184.2034882996969998 ) ) ;
#51890 = CARTESIAN_POINT ( 'NONE',  ( -4.148108818479999904, 1412.836893066629955, 232.2745409437980015 ) ) ;
#51891 = CARTESIAN_POINT ( 'NONE',  ( -17.47467951480000181, 1385.286067972039973, 219.9356668727590147 ) ) ;
#51892 = ORIENTED_EDGE ( 'NONE', *, *, #84946, .T. ) ;
#51893 = CARTESIAN_POINT ( 'NONE',  ( -16.22920744153299921, 1385.290408393959979, 219.6908716482870148 ) ) ;
#51894 = CARTESIAN_POINT ( 'NONE',  ( -9.023097092110859307, 1493.387773720369978, 200.7584573620279969 ) ) ;
#51895 = CARTESIAN_POINT ( 'NONE',  ( 12.67555790997639953, 1434.596121652720058, 149.5884656837649800 ) ) ;
#51896 = CARTESIAN_POINT ( 'NONE',  ( 15.62608574728940170, 1459.304094441330108, 229.5211440070559945 ) ) ;
#51897 = CARTESIAN_POINT ( 'NONE',  ( -21.67692661982870206, 1509.608767922699826, 228.6318993757969906 ) ) ;
#51898 = CARTESIAN_POINT ( 'NONE',  ( -1.498828828049999951, 1408.965400643329986, 187.6521917822979901 ) ) ;
#51899 = CARTESIAN_POINT ( 'NONE',  ( 0.4382461657092809881, 1517.051704408389924, 201.5558633854139998 ) ) ;
#51900 = CARTESIAN_POINT ( 'NONE',  ( 4.229538064822990329, 1441.537955797840141, 165.0787593380850069 ) ) ;
#51901 = VECTOR ( 'NONE', #40488, 1000.000000000000000 ) ;
#51903 = CARTESIAN_POINT ( 'NONE',  ( 15.91624037646960055, 1491.015088416080062, 194.0444298851370206 ) ) ;
#51902 = CARTESIAN_POINT ( 'NONE',  ( -5.000083865865000199, 1516.858456333729919, 214.1306941701269864 ) ) ;
#51904 = CARTESIAN_POINT ( 'NONE',  ( 20.20853917690000401, 1508.359852710729911, 189.3077113257979818 ) ) ;
#51905 = CARTESIAN_POINT ( 'NONE',  ( -2.485205687335000135, 1517.181921232829836, 216.8478361320569832 ) ) ;
#51906 = EDGE_LOOP ( 'NONE', ( #109338, #2172, #32597, #96357, #39658 ) ) ;
#51907 = CARTESIAN_POINT ( 'NONE',  ( -12.72965190870000107, 1416.819760216229952, 195.1130952921980111 ) ) ;
#51908 = DIRECTION ( 'NONE',  ( -1.755985294532469921E-16, 1.000000000000000000, -1.338183447452831989E-16 ) ) ;
#51909 = ORIENTED_EDGE ( 'NONE', *, *, #92101, .F. ) ;
#51911 = CARTESIAN_POINT ( 'NONE',  ( 1.533058233270000015, 1417.373139556630122, 235.5867829536979912 ) ) ;
#51910 = ADVANCED_BREP_SHAPE_REPRESENTATION ( '', ( #11085, #21632 ), #78983 ) ;
#51912 = CARTESIAN_POINT ( 'NONE',  ( 8.313287170068500487, 1507.316777277299934, 183.0869016502879845 ) ) ;
#51913 = DIRECTION ( 'NONE',  ( -0.2360473468807729458, 0.3679196751255739417, -0.8993980001567938309 ) ) ;
#51914 = CARTESIAN_POINT ( 'NONE',  ( -31.95643112690961019, 1526.329757971584968, 201.5629546934959251 ) ) ;
#51915 = CARTESIAN_POINT ( 'NONE',  ( -21.80961351509205670, 1523.919943579690425, 234.9115559964644149 ) ) ;
#51916 = AXIS2_PLACEMENT_3D ( 'NONE', #11751, #26904, #78411 ) ;
#51917 = CARTESIAN_POINT ( 'NONE',  ( 13.36997651309999924, 1416.851343894929869, 196.3340833727979771 ) ) ;
#51918 = CARTESIAN_POINT ( 'NONE',  ( 1.959285284397550120, 1474.800623515119923, 220.3715842348549927 ) ) ;
#51919 = CARTESIAN_POINT ( 'NONE',  ( 16.36456115949343371, 1522.051704408389924, 198.1507535207238391 ) ) ;
#51920 = CARTESIAN_POINT ( 'NONE',  ( 8821.345249565620179, 5182.654794667094393, -2585.374449305243161 ) ) ;
#51921 = CARTESIAN_POINT ( 'NONE',  ( 41.45644848187150444, 1440.913060354650042, 261.2593951003379971 ) ) ;
#51923 = CARTESIAN_POINT ( 'NONE',  ( 4.329294185584050325, 1515.070696454110021, 207.5527501733459985 ) ) ;
#51922 = CARTESIAN_POINT ( 'NONE',  ( -14.79231131374850072, 1418.341681852919919, 202.2100798908639945 ) ) ;
#51924 = CARTESIAN_POINT ( 'NONE',  ( 11.14671379024469999, 1434.019377051509991, 151.6529839732360188 ) ) ;
#51925 = ORIENTED_EDGE ( 'NONE', *, *, #51664, .T. ) ;
#51926 = CARTESIAN_POINT ( 'NONE',  ( -7.672264733570000494, 1508.551704439589912, 219.1253561400989724 ) ) ;
#51927 = CARTESIAN_POINT ( 'NONE',  ( 24.27272702730000020, 1449.843846490510032, 206.2143647668480071 ) ) ;
#51928 = CARTESIAN_POINT ( 'NONE',  ( -2.385019621457261874, 1526.073429442291854, 177.7124997907143040 ) ) ;
#51929 = CARTESIAN_POINT ( 'NONE',  ( 4.286107831027711867, 1410.438896930658757, 186.1261285953802087 ) ) ;
#51930 = CARTESIAN_POINT ( 'NONE',  ( -10.48474110849999974, 1480.275079708390194, 208.2232256045050178 ) ) ;
#51931 = CARTESIAN_POINT ( 'NONE',  ( 28.97303002314154696, 1526.186458717542791, 220.8123550170068654 ) ) ;
#51932 = DIRECTION ( 'NONE',  ( 5.980589973904019347E-17, -1.000000000000000000, 1.736889445713099699E-16 ) ) ;
#51933 = CARTESIAN_POINT ( 'NONE',  ( -4.636604420221742906, 1378.026799461571272, 203.9259778311827063 ) ) ;
#51934 = CARTESIAN_POINT ( 'NONE',  ( 13.17906415938499975, 1414.913527275050001, 198.1030012665459878 ) ) ;
#51936 = EDGE_CURVE ( 'NONE', #28587, #106610, #94589, .T. ) ;
#51935 = CARTESIAN_POINT ( 'NONE',  ( -56.13545839238830126, 1383.802202486730039, 273.6217168716430024 ) ) ;
#51937 = CARTESIAN_POINT ( 'NONE',  ( -107.5501839752090234, 1379.272371746452563, 299.1643430017058449 ) ) ;
#51938 = CARTESIAN_POINT ( 'NONE',  ( -1.633027085391620004, 1516.553531807389845, 201.4123107264900057 ) ) ;
#51940 = ORIENTED_EDGE ( 'NONE', *, *, #2873, .T. ) ;
#51939 = CARTESIAN_POINT ( 'NONE',  ( 10.36440324736019925, 1451.671856551549809, 207.3348124021030117 ) ) ;
#51941 = CARTESIAN_POINT ( 'NONE',  ( -17.64542808779836491, 1460.260031838558461, 228.1847870265016525 ) ) ;
#51942 = AXIS2_PLACEMENT_3D ( 'NONE', #45850, #36871, #71065 ) ;
#51943 = CARTESIAN_POINT ( 'NONE',  ( -73.20427770220000241, 1380.595915926100133, 278.0678802370590006 ) ) ;
#51944 = DIRECTION ( 'NONE',  ( -1.000000000000000000, 1.836970198721029688E-16, 0.000000000000000000 ) ) ;
#51945 = EDGE_CURVE ( 'NONE', #80494, #87520, #69924, .T. ) ;
#51946 = VERTEX_POINT ( 'NONE', #79208 ) ;
#51947 = ORIENTED_EDGE ( 'NONE', *, *, #45039, .T. ) ;
#51948 = CARTESIAN_POINT ( 'NONE',  ( 3.118627138969999990, 1507.020746158230168, 237.9289388427980043 ) ) ;
#51949 = CARTESIAN_POINT ( 'NONE',  ( -3.737543590866930110, 1457.196795654610014, 214.7727701001950038 ) ) ;
#51950 = CARTESIAN_POINT ( 'NONE',  ( 40.26153007682929541, 1443.187744381950097, 137.0666827882720042 ) ) ;
#51952 = CARTESIAN_POINT ( 'NONE',  ( -19.16279666149999983, 1470.534631754830116, 262.3396919526979900 ) ) ;
#51951 = CARTESIAN_POINT ( 'NONE',  ( 22.09833645820000214, 1506.806593688229896, 209.1697492017360105 ) ) ;
#51953 = TOROIDAL_SURFACE ( 'NONE', #55316, 6.500000000000000000, 1.000000000000000000 ) ;
#51954 = CARTESIAN_POINT ( 'NONE',  ( 8.750084289021121009, 1436.836525569339756, 209.7700227241190021 ) ) ;
#51955 = CARTESIAN_POINT ( 'NONE',  ( -110.0634902310000030, 1384.899971913130003, 296.9512050679589947 ) ) ;
#51956 = CARTESIAN_POINT ( 'NONE',  ( -12.82658623871375347, 1435.929109846025995, 150.8182851086763208 ) ) ;
#51957 = CARTESIAN_POINT ( 'NONE',  ( -20.53890917329999866, 1486.102232517730044, 191.0326899443980153 ) ) ;
#51958 = CARTESIAN_POINT ( 'NONE',  ( 3.773835479270000182, 1410.421536211630155, 185.9548053891980146 ) ) ;
#51959 = CARTESIAN_POINT ( 'NONE',  ( 3.116401324629539893, 1487.019696768639960, 197.5841379987910216 ) ) ;
#51960 = CARTESIAN_POINT ( 'NONE',  ( -7.981991148520000579, 1441.362204533440035, 154.1152758918979941 ) ) ;
#51961 = CARTESIAN_POINT ( 'NONE',  ( -9.198164182857258453, 1450.369964096400054, 208.5037453834269741 ) ) ;
#51962 = CARTESIAN_POINT ( 'NONE',  ( -8.535066471915349950, 1424.913453952659893, 204.9008513312109869 ) ) ;
#51963 = AXIS2_PLACEMENT_3D ( 'NONE', #74315, #107339, #31175 ) ;
#51964 = CARTESIAN_POINT ( 'NONE',  ( -23.90685205709999650, 1451.267540530529914, 140.4958681723980192 ) ) ;
#51965 = CARTESIAN_POINT ( 'NONE',  ( 1.420259601960000229, 1466.712985171129958, 235.0376566307980113 ) ) ;
#51966 = ORIENTED_EDGE ( 'NONE', *, *, #74064, .F. ) ;
#51967 = CARTESIAN_POINT ( 'NONE',  ( -12.35793136629999900, 1506.116535470989902, 208.8889582108720049 ) ) ;
#51968 = CARTESIAN_POINT ( 'NONE',  ( 22.27437808960000254, 1476.550945564490121, 209.6594615055550150 ) ) ;
#51969 = CARTESIAN_POINT ( 'NONE',  ( -42.06231866970000510, 1440.913089571779892, 269.6487540859979504 ) ) ;
#51970 = CARTESIAN_POINT ( 'NONE',  ( 2.038847259689231084, 1501.977400791986611, 173.3106345060153046 ) ) ;
#51971 = CARTESIAN_POINT ( 'NONE',  ( 17.60627587029999930, 1410.895669429430200, 224.1775087542980032 ) ) ;
#51972 = CARTESIAN_POINT ( 'NONE',  ( -3.227261282950000254, 1476.559864218489793, 202.2993187396990038 ) ) ;
#51973 = CARTESIAN_POINT ( 'NONE',  ( 2.330134126090000368, 1515.064792882589927, 213.4512947377390049 ) ) ;
#51974 = CARTESIAN_POINT ( 'NONE',  ( 2.760778564396810353, 1409.009468899150079, 230.1977509304229841 ) ) ;
#51975 = CARTESIAN_POINT ( 'NONE',  ( -2.039114686836970058, 1421.064113876339889, 193.7872318451859712 ) ) ;
#51976 = CARTESIAN_POINT ( 'NONE',  ( -10.37900483499999993, 1419.722126144429922, 232.2032976616980022 ) ) ;
#51977 = CARTESIAN_POINT ( 'NONE',  ( -106.7877995600000105, 1387.660326901150029, 310.1072176132589675 ) ) ;
#51978 = VECTOR ( 'NONE', #106616, 1000.000000000000114 ) ;
#51979 = LINE ( 'NONE', #35160, #16205 ) ;
#51980 = CARTESIAN_POINT ( 'NONE',  ( -0.7618909056700008398, 1360.403425203260213, 207.6218459616989946 ) ) ;
#51981 = CARTESIAN_POINT ( 'NONE',  ( -45.44490940612519125, 1437.744605196359998, 268.9801658155380437 ) ) ;
#51982 = FACE_OUTER_BOUND ( 'NONE', #55728, .T. ) ;
#51983 = CARTESIAN_POINT ( 'NONE',  ( -8.110586521360000134, 1425.115383700800066, 209.5285450949000108 ) ) ;
#51984 = ORIENTED_EDGE ( 'NONE', *, *, #48641, .F. ) ;
#51985 = CARTESIAN_POINT ( 'NONE',  ( -7.719640941135000212, 1516.939452820819952, 209.1319487995289705 ) ) ;
#51986 = AXIS2_PLACEMENT_3D ( 'NONE', #54808, #10590, #86738 ) ;
#51987 = DIRECTION ( 'NONE',  ( -0.000000000000000000, 1.000000000000000000, 0.000000000000000000 ) ) ;
#51988 = FACE_OUTER_BOUND ( 'NONE', #84873, .T. ) ;
#51989 = CARTESIAN_POINT ( 'NONE',  ( 7.499492845059839929, 1425.981480573469753, 212.3193081490009888 ) ) ;
#51990 = CARTESIAN_POINT ( 'NONE',  ( -25.23019512061160086, 1452.032085083439824, 135.4492350236539835 ) ) ;
#51991 = VERTEX_POINT ( 'NONE', #29328 ) ;
#51992 = CARTESIAN_POINT ( 'NONE',  ( -16.35911259859972233, 1409.492701125528583, 225.1152623397985337 ) ) ;
#51994 = CARTESIAN_POINT ( 'NONE',  ( 14.13297884659999859, 1452.811554597230042, 195.2238856287980013 ) ) ;
#51993 = CARTESIAN_POINT ( 'NONE',  ( -2.485146179491022345, 1524.547395018738143, 175.7094276205802146 ) ) ;
#51995 = CARTESIAN_POINT ( 'NONE',  ( 1.797565579689999860, 1415.903556134529936, 232.4419632246980143 ) ) ;
#51996 = CIRCLE ( 'NONE', #3738, 1.999999999999999556 ) ;
#51997 = DIRECTION ( 'NONE',  ( 0.000000000000000000, -0.07593562622321022026, -0.9971127221483482295 ) ) ;
#51998 = CARTESIAN_POINT ( 'NONE',  ( -0.07708582513870239350, 1460.859163483989960, 228.7412678487989979 ) ) ;
#51999 = CARTESIAN_POINT ( 'NONE',  ( -18.64588645199999917, 1416.828044802730119, 208.5593772625580016 ) ) ;
#52000 = ORIENTED_EDGE ( 'NONE', *, *, #56916, .F. ) ;
#52001 = CARTESIAN_POINT ( 'NONE',  ( -3.129454527291580135, 1407.723237535949920, 270.1357211735799524 ) ) ;
#52002 = CARTESIAN_POINT ( 'NONE',  ( -0.7559395363919990674, 1516.972341476009888, 207.9998125401569951 ) ) ;
#52003 = CARTESIAN_POINT ( 'NONE',  ( 8.734601244239950546, 1418.821511342440090, 231.3068792023239837 ) ) ;
#52004 = DIRECTION ( 'NONE',  ( -0.02616798426450828510, 0.9993150019883944024, 0.02616798426450818449 ) ) ;
#52006 = ORIENTED_EDGE ( 'NONE', *, *, #59298, .T. ) ;
#52005 = CARTESIAN_POINT ( 'NONE',  ( -7.760077312028009544, 1365.297824701876380, 209.6218459617148824 ) ) ;
#52007 = VERTEX_POINT ( 'NONE', #37194 ) ;
#52008 = CARTESIAN_POINT ( 'NONE',  ( -23.64670054153389955, 1410.982901525189845, 210.3775373128219996 ) ) ;
#52009 = CARTESIAN_POINT ( 'NONE',  ( -4.086401651919999267, 1424.208576867429883, 185.4429785608980126 ) ) ;
#52010 = CARTESIAN_POINT ( 'NONE',  ( -101.7585531180999965, 1320.102705746890251, 310.5815973742389815 ) ) ;
#52011 = CARTESIAN_POINT ( 'NONE',  ( -4.823778297959999684, 1426.859560269130043, 144.1938086916980239 ) ) ;
#52012 = CARTESIAN_POINT ( 'NONE',  ( -19.76012964183019704, 1467.135250698569962, 193.4660110028719942 ) ) ;
#52013 = CARTESIAN_POINT ( 'NONE',  ( -22.29148574759999946, 1425.804551132829829, 216.5767124936379844 ) ) ;
#52014 = CARTESIAN_POINT ( 'NONE',  ( 28.58215788712900007, 1468.635916194609990, 268.1351379920200202 ) ) ;
#52015 = ADVANCED_FACE ( 'NONE', ( #27138 ), #98492, .T. ) ;
#52016 = CARTESIAN_POINT ( 'NONE',  ( -10.22810209145352900, 1464.519780891043638, 232.1939053660614718 ) ) ;
#52017 = CARTESIAN_POINT ( 'NONE',  ( -4.820692999790000322, 1427.981916302389891, 201.4689414325489736 ) ) ;
#52018 =( BOUNDED_CURVE ( )  B_SPLINE_CURVE ( 3, ( #83475, #22446, #82395, #47693 ),
 .UNSPECIFIED., .F., .F. ) 
 B_SPLINE_CURVE_WITH_KNOTS ( ( 4, 4 ),
 ( 3.142823553869715347, 3.152136943596000052 ),
 .UNSPECIFIED. ) 
 CURVE ( )  GEOMETRIC_REPRESENTATION_ITEM ( )  RATIONAL_B_SPLINE_CURVE ( ( 1.000000000000000000, 0.9999927717440458830, 0.9999927717440458830, 1.000000000000000000 ) ) 
 REPRESENTATION_ITEM ( '' )  );
#52019 = CARTESIAN_POINT ( 'NONE',  ( 2.864972116015000125, 1516.859514182039902, 206.2412530031170093 ) ) ;
#52020 = ORIENTED_EDGE ( 'NONE', *, *, #93906, .T. ) ;
#52021 = LINE ( 'NONE', #2741, #746 ) ;
#52022 = CARTESIAN_POINT ( 'NONE',  ( 1.510002137662999955, 1461.120581648620146, 183.1207398647079856 ) ) ;
#52023 = CARTESIAN_POINT ( 'NONE',  ( 22.91483027350000157, 1409.739594360729825, 208.7501026320239816 ) ) ;
#52024 = EDGE_LOOP ( 'NONE', ( #49322, #54683, #14513, #73488 ) ) ;
#52026 = B_SPLINE_CURVE_WITH_KNOTS ( 'NONE', 3,
 ( #64177, #96663, #46827, #54680 ),
 .UNSPECIFIED., .F., .F.,
 ( 4, 4 ),
 ( 0.000000000000000000, 1.000000000000000000 ),
 .UNSPECIFIED. ) ;
#52025 = CARTESIAN_POINT ( 'NONE',  ( 4.240940644616750355, 1509.032041130069956, 205.3774179143429990 ) ) ;
#52027 = ADVANCED_FACE ( 'NONE', ( #52359 ), #33100, .F. ) ;
#52028 = CARTESIAN_POINT ( 'NONE',  ( 25.97075925569999910, 1451.764531650130039, 135.9704145892980023 ) ) ;
#52029 = B_SPLINE_SURFACE_WITH_KNOTS ( 'NONE', 5, 5, ( 
 ( #71188, #77362, #35910, #26953, #25821, #19071, #104207, #79031, #1773 ),
 ( #43755, #2332, #60020, #62234, #94140, #53841, #87979, #52168, #1213 ),
 ( #77906, #17972, #61680, #11267, #51608, #60578, #10144, #27493, #43212 ),
 ( #663, #95803, #34794, #95258, #53275, #86299, #79573, #18519, #86851 ),
 ( #68981, #94698, #69535, #61144, #87414, #2875, #45429, #30237, #55472 ),
 ( #12891, #47612, #96919, #72278, #5044, #47069, #89599, #81193, #38100 ) ),
 .UNSPECIFIED., .F., .F., .F.,
 ( 6, 6 ),
 ( 6, 3, 6 ),
 ( 11.16857693960000120, 24.00668087930000283 ),
 ( 0.000000000000000000, 1.000000000000000000, 2.000000000000000000 ),
 .UNSPECIFIED. ) ;
#52030 = ADVANCED_FACE ( 'NONE', ( #31529, #57323 ), #72460, .T. ) ;
#52031 = CARTESIAN_POINT ( 'NONE',  ( 2.487935123032368967, 1508.603735228351297, 204.3914617891122703 ) ) ;
#52032 = CARTESIAN_POINT ( 'NONE',  ( -8.757904425059999554, 1386.987225607769915, 218.3429050645090115 ) ) ;
#52033 = CARTESIAN_POINT ( 'NONE',  ( 7.535268056249999624, 1422.940929649649888, 195.7043803497990098 ) ) ;
#52034 = CARTESIAN_POINT ( 'NONE',  ( 18.42637209560000144, 1409.556523480330043, 196.3080071043980013 ) ) ;
#52035 = CARTESIAN_POINT ( 'NONE',  ( 27.48389906189999721, 1443.913060387330006, 168.8435737885979790 ) ) ;
#52036 = CARTESIAN_POINT ( 'NONE',  ( 3.421791868836843165, 1439.691577471224718, 184.4543791659172314 ) ) ;
#52038 = CARTESIAN_POINT ( 'NONE',  ( -23.47750638058768757, 1434.817782033998583, 212.9234740453307779 ) ) ;
#52037 = CARTESIAN_POINT ( 'NONE',  ( 31.25789155968564970, 1523.954914175594922, 196.3501112485169813 ) ) ;
#52039 = CARTESIAN_POINT ( 'NONE',  ( 11.03217570710000039, 1409.298312452229993, 227.8647431501979952 ) ) ;
#52040 = CARTESIAN_POINT ( 'NONE',  ( -0.007173723813013069966, 1508.946327270009988, 179.4591247994410139 ) ) ;
#52041 = CARTESIAN_POINT ( 'NONE',  ( -8.401610822820000379, 1382.692138962740046, 218.3897665777690236 ) ) ;
#52042 = LINE ( 'NONE', #26826, #98149 ) ;
#52043 = ORIENTED_EDGE ( 'NONE', *, *, #1905, .F. ) ;
#52044 = CARTESIAN_POINT ( 'NONE',  ( 11.01105141466669934, 1414.913060387399810, 221.0326450546259878 ) ) ;
#52045 = AXIS2_PLACEMENT_3D ( 'NONE', #46904, #75403, #15452 ) ;
#52046 = CARTESIAN_POINT ( 'NONE',  ( 11.13648443495080009, 1432.345323076100158, 151.6342730693140197 ) ) ;
#52047 = CARTESIAN_POINT ( 'NONE',  ( -7.853014526819640295, 1484.259593461030136, 200.1697423039280181 ) ) ;
#52048 = CARTESIAN_POINT ( 'NONE',  ( -13.97245352320000045, 1390.368340403819957, 209.8294132315500349 ) ) ;
#52049 = CARTESIAN_POINT ( 'NONE',  ( -1.599049516947889105, 1420.649782495757108, 193.7985443746896124 ) ) ;
#52050 = CIRCLE ( 'NONE', #77066, 1.999999999999999556 ) ;
#52051 = CARTESIAN_POINT ( 'NONE',  ( -4.328404850859190134, 1515.104658776890119, 208.0669027827329955 ) ) ;
#52052 = CARTESIAN_POINT ( 'NONE',  ( -4.290289618250000103, 1461.407663418029870, 243.9198229205979942 ) ) ;
#52053 = CARTESIAN_POINT ( 'NONE',  ( -8.921303631935559864, 1384.360432746769902, 218.6413268481589967 ) ) ;
#52054 = CARTESIAN_POINT ( 'NONE',  ( 11.80976821910000041, 1433.247602250280124, 150.6126538827979857 ) ) ;
#52055 = CARTESIAN_POINT ( 'NONE',  ( 9.562842983910000427, 1454.397736359230066, 219.6133833293980047 ) ) ;
#52056 = CARTESIAN_POINT ( 'NONE',  ( 11.61527099316350231, 1414.971349104640012, 197.1579164385690035 ) ) ;
#52057 = EDGE_CURVE ( 'NONE', #108598, #44333, #70662, .T. ) ;
#52058 = CIRCLE ( 'NONE', #48470, 1.999999999999999556 ) ;
#52059 = CARTESIAN_POINT ( 'NONE',  ( -13.97983274584369973, 1420.196076808720136, 195.9955686830610091 ) ) ;
#52060 = CARTESIAN_POINT ( 'NONE',  ( 11.64982809710589962, 1421.677256869899793, 203.4368870229210131 ) ) ;
#52061 = CARTESIAN_POINT ( 'NONE',  ( 10.52578744093320040, 1462.363382362089851, 212.2902631912189975 ) ) ;
#52062 = CARTESIAN_POINT ( 'NONE',  ( 1.448679645196929933, 1507.129709964000085, 181.1126013477120011 ) ) ;
#52063 = AXIS2_PLACEMENT_3D ( 'NONE', #65004, #22961, #6727 ) ;
#52064 = CARTESIAN_POINT ( 'NONE',  ( 13.01603395294319476, 1398.298686285902704, 209.4299075615936374 ) ) ;
#52065 = CARTESIAN_POINT ( 'NONE',  ( 0.04734028010245310697, 1508.924978232730155, 238.6962546503989984 ) ) ;
#52066 = CARTESIAN_POINT ( 'NONE',  ( -8.116894974276100072, 1425.431424825695331, 208.6843198518954523 ) ) ;
#52067 = CARTESIAN_POINT ( 'NONE',  ( 12.78654151607593015, 1416.818673880716915, 223.0773805434268127 ) ) ;
#52068 = CARTESIAN_POINT ( 'NONE',  ( 26.50108598912411750, 1436.729172686955735, 136.8088966875825179 ) ) ;
#52069 = CARTESIAN_POINT ( 'NONE',  ( -10.89134688618890046, 1383.862286347570034, 218.6605473698739956 ) ) ;
#52070 = CARTESIAN_POINT ( 'NONE',  ( 4.803837556235689199, 1471.771475080379787, 187.6888395172460093 ) ) ;
#52071 = CARTESIAN_POINT ( 'NONE',  ( 6.560742225334999844, 1517.028034847769959, 213.1554992345569701 ) ) ;
#52072 = CARTESIAN_POINT ( 'NONE',  ( -13.75591821840509965, 1421.742616532689908, 205.2219009381699948 ) ) ;
#52073 = CARTESIAN_POINT ( 'NONE',  ( 9.181100887863649973, 1450.964097471789955, 210.1935140534000084 ) ) ;
#52075 = ORIENTED_EDGE ( 'NONE', *, *, #42568, .F. ) ;
#52074 = CARTESIAN_POINT ( 'NONE',  ( 3.899014136759999971, 1442.684943332589910, 217.1061286285590199 ) ) ;
#52076 = CARTESIAN_POINT ( 'NONE',  ( -0.7130142951239999416, 1416.844618638430120, 227.9191939111979934 ) ) ;
#52077 = VECTOR ( 'NONE', #44348, 999.9999999999998863 ) ;
#52078 = CARTESIAN_POINT ( 'NONE',  ( 2.500000000000000000, 1443.913060387330006, 150.6726614421979775 ) ) ;
#52079 = CARTESIAN_POINT ( 'NONE',  ( 12.40402065109999974, 1434.420118205629933, 149.6993386520979925 ) ) ;
#52080 = ADVANCED_FACE ( 'NONE', ( #49457 ), #20382, .T. ) ;
#52081 = CARTESIAN_POINT ( 'NONE',  ( -37.66742087365959435, 1450.649596001770078, 134.0999999985879754 ) ) ;
#52082 = CARTESIAN_POINT ( 'NONE',  ( -17.11734631873629908, 1420.830859248140086, 201.6585988287660030 ) ) ;
#52083 = ORIENTED_EDGE ( 'NONE', *, *, #80068, .F. ) ;
#52084 = CARTESIAN_POINT ( 'NONE',  ( -10.14857146029999946, 1472.086425142190137, 209.7191475309859925 ) ) ;
#52085 = AXIS2_PLACEMENT_3D ( 'NONE', #43109, #34692, #24609 ) ;
#52086 = CARTESIAN_POINT ( 'NONE',  ( -13.62718107187109950, 1390.427313303139954, 210.7651432677700143 ) ) ;
#52087 = CARTESIAN_POINT ( 'NONE',  ( -14.44608864360000133, 1416.522662137629823, 221.3854392607979946 ) ) ;
#52088 = CARTESIAN_POINT ( 'NONE',  ( -6.227663043015771116, 1509.133838473635024, 237.8782978115028470 ) ) ;
#52089 = CARTESIAN_POINT ( 'NONE',  ( -2.895732582093412333, 1368.219138801509644, 210.2516770323846629 ) ) ;
#52090 = CARTESIAN_POINT ( 'NONE',  ( 45.63712937690380755, 1440.913060387330006, 268.9747523971630017 ) ) ;
#52091 = DIRECTION ( 'NONE',  ( 0.000000000000000000, -6.123233995736769734E-17, -1.000000000000000000 ) ) ;
#52092 = DIRECTION ( 'NONE',  ( -0.9455185755993178454, 0.000000000000000000, 0.3255681544571537578 ) ) ;
#52093 = CARTESIAN_POINT ( 'NONE',  ( -10.25368835369999942, 1391.913060387289988, 204.2726076338790051 ) ) ;
#52094 = CARTESIAN_POINT ( 'NONE',  ( -81.68439207092418997, 1385.164090965520018, 285.2251458109799955 ) ) ;
#52095 = CARTESIAN_POINT ( 'NONE',  ( -16.69507587579999708, 1411.915237329530100, 191.7082158511979912 ) ) ;
#52096 = CARTESIAN_POINT ( 'NONE',  ( 9.490563787272430218, 1424.812203410370103, 209.0803129943540171 ) ) ;
#52097 = ORIENTED_EDGE ( 'NONE', *, *, #17134, .T. ) ;
#52098 = CIRCLE ( 'NONE', #19941, 0.9999999999999952260 ) ;
#52099 = CARTESIAN_POINT ( 'NONE',  ( -15.77423603240969996, 1409.463753444150143, 225.3878024414169943 ) ) ;
#52101 = ORIENTED_EDGE ( 'NONE', *, *, #45319, .F. ) ;
#52100 = CARTESIAN_POINT ( 'NONE',  ( -0.7910245917146945249, 1426.918876941764893, 134.0999999980979851 ) ) ;
#52102 = CARTESIAN_POINT ( 'NONE',  ( -19.67625207089999861, 1467.566588935489790, 206.2108820087490244 ) ) ;
#52103 = ORIENTED_EDGE ( 'NONE', *, *, #75552, .T. ) ;
#52104 = CARTESIAN_POINT ( 'NONE',  ( 27.59578647829999909, 1509.876726487329734, 217.1913344172780000 ) ) ;
#52105 = CARTESIAN_POINT ( 'NONE',  ( -7.042317098485010973, 1363.957259258367230, 209.6218459617148824 ) ) ;
#52106 = DIRECTION ( 'NONE',  ( 0.000000000000000000, -0.8724564897876576630, -0.4886917979948086077 ) ) ;
#52107 = CARTESIAN_POINT ( 'NONE',  ( 39.37269659054818050, 1451.600413132400945, 269.5993111650432752 ) ) ;
#52108 = CARTESIAN_POINT ( 'NONE',  ( -4.329791528864999961, 1515.051704408389924, 205.7917117663469924 ) ) ;
#52109 = CARTESIAN_POINT ( 'NONE',  ( 18.48763279861755748, 1436.139455391317370, 214.3615573111846118 ) ) ;
#52110 = CARTESIAN_POINT ( 'NONE',  ( -7302.760118613915438, 5181.793945261120825, -10646.37847981480263 ) ) ;
#52111 = CARTESIAN_POINT ( 'NONE',  ( -4.588057595808531453, 1516.952111086027799, 215.0815035125188501 ) ) ;
#52112 = CARTESIAN_POINT ( 'NONE',  ( -16.68599179819999989, 1461.099982565929849, 230.2790296985980092 ) ) ;
#52113 = CARTESIAN_POINT ( 'NONE',  ( -8.395212705517364427, 1368.789864683679070, 210.6218459617030021 ) ) ;
#52114 = CARTESIAN_POINT ( 'NONE',  ( 1.102161665280000147, 1456.373626168390047, 198.9794195941990154 ) ) ;
#52115 = EDGE_CURVE ( 'NONE', #109511, #95178, #44907, .T. ) ;
#52116 = CARTESIAN_POINT ( 'NONE',  ( 3.445407533985000104, 1516.764084769670262, 206.8237970085970119 ) ) ;
#52118 = EDGE_CURVE ( 'NONE', #2574, #31132, #50250, .T. ) ;
#52117 = DIRECTION ( 'NONE',  ( -0.6736849260863841948, 0.000000000000000000, 0.7390186874254148774 ) ) ;
#52119 = CARTESIAN_POINT ( 'NONE',  ( -31.29224604902359985, 1525.661275128775969, 216.2849134033308758 ) ) ;
#52120 = CARTESIAN_POINT ( 'NONE',  ( -3.617573937850000032, 1497.333809982789944, 198.4503636364990200 ) ) ;
#52122 = VERTEX_POINT ( 'NONE', #45482 ) ;
#52121 = CARTESIAN_POINT ( 'NONE',  ( -3.619841760469999947, 1497.142537370389846, 220.5541520919989864 ) ) ;
#52123 = B_SPLINE_CURVE_WITH_KNOTS ( 'NONE', 3,
 ( #30880, #55020, #74009, #108141, #99174, #56656, #90790, #14072, #48261, #82405, #31433, #65615 ),
 .UNSPECIFIED., .F., .F.,
 ( 4, 2, 2, 2, 2, 4 ),
 ( -0.08222331866850060567, -0.06445908733047370220, -0.04475466563503439910, -0.02302985374697249371, 0.000000000000000000, 0.0003446917825884465714 ),
 .UNSPECIFIED. ) ;
#52124 = DIRECTION ( 'NONE',  ( 0.4794255386041986200, 0.000000000000000000, 0.8775825618903752012 ) ) ;
#52125 = ORIENTED_EDGE ( 'NONE', *, *, #105425, .T. ) ;
#52126 = CARTESIAN_POINT ( 'NONE',  ( 3.021259845790000085E-08, 1408.296884782030020, 262.4989465150980550 ) ) ;
#52127 = CARTESIAN_POINT ( 'NONE',  ( -24.49050335060000094, 1430.357935323129823, 206.8695671012879984 ) ) ;
#52129 = CARTESIAN_POINT ( 'NONE',  ( 16.55649716813289984, 1410.443606432929982, 191.7825502688590120 ) ) ;
#52128 = CARTESIAN_POINT ( 'NONE',  ( -10.60244528208989934, 1425.057211382899823, 130.8090886194080156 ) ) ;
#52130 = CARTESIAN_POINT ( 'NONE',  ( -1.118104767724999782, 1516.965971551240045, 211.4215139361070044 ) ) ;
#52131 = TOROIDAL_SURFACE ( 'NONE', #62886, 2.030931026690000252, 0.5000000000000000000 ) ;
#52132 = CARTESIAN_POINT ( 'NONE',  ( 26.18610560624165018, 1509.940572648346006, 194.3908627882991311 ) ) ;
#52133 = CARTESIAN_POINT ( 'NONE',  ( -18.79734767819999774, 1416.844618642430078, 208.4088319194450207 ) ) ;
#52134 = CARTESIAN_POINT ( 'NONE',  ( -12.42519068387639969, 1378.686196775090139, 209.1401553900249723 ) ) ;
#52135 = CARTESIAN_POINT ( 'NONE',  ( 43.37195119983255864, 1452.013340143054393, 269.7132330850898256 ) ) ;
#52136 = CARTESIAN_POINT ( 'NONE',  ( -4.992622102040000343, 1391.631309831290082, 214.6079342942889809 ) ) ;
#52137 = CARTESIAN_POINT ( 'NONE',  ( -35.45835282683830769, 1437.253800090359846, 136.5355674391020102 ) ) ;
#52138 = ORIENTED_EDGE ( 'NONE', *, *, #5288, .T. ) ;
#52139 = CARTESIAN_POINT ( 'NONE',  ( 13.97474060794100126, 1398.020587696859820, 206.9428454895969764 ) ) ;
#52140 = CARTESIAN_POINT ( 'NONE',  ( 9.597484669293001147, 1461.985966042660266, 207.5232997255220084 ) ) ;
#52141 = CARTESIAN_POINT ( 'NONE',  ( -16.71362360910000078, 1459.161552659730205, 228.9915664566980240 ) ) ;
#52142 = ORIENTED_EDGE ( 'NONE', *, *, #57877, .T. ) ;
#52143 = VERTEX_POINT ( 'NONE', #44365 ) ;
#52144 = FACE_OUTER_BOUND ( 'NONE', #87665, .T. ) ;
#52145 = VERTEX_POINT ( 'NONE', #53894 ) ;
#52146 = VECTOR ( 'NONE', #65719, 1000.000000000000000 ) ;
#52147 = DIRECTION ( 'NONE',  ( 0.8090169943749465631, 0.000000000000000000, -0.5877852522924742473 ) ) ;
#52148 = CARTESIAN_POINT ( 'NONE',  ( -9.534864884007895114, 1418.422607348942392, 197.0272821719209730 ) ) ;
#52149 = ADVANCED_FACE ( 'NONE', ( #19119 ), #84058, .T. ) ;
#52150 = CARTESIAN_POINT ( 'NONE',  ( -19.59053950279439960, 1486.265866315750145, 189.8955481462990065 ) ) ;
#52151 = CARTESIAN_POINT ( 'NONE',  ( 28.77729953137099983, 1509.917985831029910, 206.0039978706130057 ) ) ;
#52152 = CARTESIAN_POINT ( 'NONE',  ( 30.25425994617009096, 1526.382868172863937, 218.9520509131588994 ) ) ;
#52153 = EDGE_CURVE ( 'NONE', #23737, #83466, #18085, .T. ) ;
#52154 = CARTESIAN_POINT ( 'NONE',  ( 10.12302436080650025, 1452.223079970169920, 209.0282544715680046 ) ) ;
#52155 = DIRECTION ( 'NONE',  ( -0.9125304618753966590, 0.000000000000000000, 0.4090087482554319309 ) ) ;
#52156 = CARTESIAN_POINT ( 'NONE',  ( -91.57517030605119146, 1384.844808691319940, 293.4524694912760197 ) ) ;
#52157 = EDGE_LOOP ( 'NONE', ( #6709, #85317, #69656, #63817 ) ) ;
#52158 = CARTESIAN_POINT ( 'NONE',  ( -7.718763544034999313, 1516.905946377369901, 202.1794916586869988 ) ) ;
#52159 = CARTESIAN_POINT ( 'NONE',  ( -5.786847777804999815, 1517.104497701820037, 208.3841784293060186 ) ) ;
#52160 = ORIENTED_EDGE ( 'NONE', *, *, #16760, .T. ) ;
#52162 = EDGE_CURVE ( 'NONE', #29251, #50772, #49213, .T. ) ;
#52161 = CARTESIAN_POINT ( 'NONE',  ( 11.81926599889289875, 1429.255342282230004, 149.0484304434379794 ) ) ;
#52163 = VECTOR ( 'NONE', #82608, 1000.000000000000227 ) ;
#52164 = CARTESIAN_POINT ( 'NONE',  ( 3.059233499280463064, 1511.948749218694957, 217.0319409951804062 ) ) ;
#52165 = VERTEX_POINT ( 'NONE', #48776 ) ;
#52166 = CARTESIAN_POINT ( 'NONE',  ( 3.487592431261229642, 1509.038615938009798, 213.6090957240379851 ) ) ;
#52167 = CARTESIAN_POINT ( 'NONE',  ( -13.51610093809999924, 1443.501467202829872, 169.3501091259980171 ) ) ;
#52168 = CARTESIAN_POINT ( 'NONE',  ( 4.908323279449999355, 1507.487947428030111, 235.7295937283979868 ) ) ;
#52169 =( BOUNDED_SURFACE ( )  B_SPLINE_SURFACE ( 3, 2, ( 
 ( #38676, #30827, #63913 ),
 ( #3460, #98029, #39226 ),
 ( #105909, #55505, #89634 ),
 ( #65003, #81773, #12921 ),
 ( #54962, #108082, #31377 ),
 ( #37587, #63379, #47101 ),
 ( #89089, #97495, #20763 ),
 ( #90732, #57168, #56598 ),
 ( #81227, #30274, #12376 ),
 ( #4007, #38132, #4542 ) ),
 .UNSPECIFIED., .F., .F., .F. ) 
 B_SPLINE_SURFACE_WITH_KNOTS ( ( 4, 2, 2, 2, 4 ),
 ( 3, 3 ),
 ( 0.000000000000000000, 0.3926990816987241395, 0.7853981633974482790, 1.178097245096172418, 1.570796326794896558 ),
 ( 0.000000000000000000, 1.000000000000000000 ),
 .UNSPECIFIED. ) 
 GEOMETRIC_REPRESENTATION_ITEM ( )  RATIONAL_B_SPLINE_SURFACE ( (
 ( 1.000000000000000000, 0.7763623250684332788, 1.000000000000000000),
 ( 1.000000000000000000, 0.7763684247032729413, 1.000000000000000000),
 ( 1.000000000000000000, 0.7746454561800525385, 1.000000000000000000),
 ( 1.000000000000000000, 0.7679730451969956073, 1.000000000000000000),
 ( 1.000000000000000000, 0.7630177051944824207, 1.000000000000000000),
 ( 1.000000000000000000, 0.7504512394530151731, 1.000000000000000000),
 ( 1.000000000000000000, 0.7428408967932995655, 1.000000000000000000),
 ( 1.000000000000000000, 0.7259222650904413321, 1.000000000000000000),
 ( 1.000000000000000000, 0.7166207884824116192, 1.000000000000000000),
 ( 1.000000000000000000, 0.7071067811865867636, 1.000000000000000000) ) ) 
 REPRESENTATION_ITEM ( '' )  SURFACE ( )  );
#52170 = CARTESIAN_POINT ( 'NONE',  ( -1.748905610829809998, 1488.269106374019884, 219.8524659745219765 ) ) ;
#52171 = CARTESIAN_POINT ( 'NONE',  ( -5.099269457000000116, 1423.012593427629781, 185.1299087936980072 ) ) ;
#52172 = CARTESIAN_POINT ( 'NONE',  ( 4.146667765623250013, 1409.925191843709854, 270.0721511231989780 ) ) ;
#52173 = CARTESIAN_POINT ( 'NONE',  ( 9.207192151108898770, 1450.833480228639928, 209.8877954179420158 ) ) ;
#52174 = CARTESIAN_POINT ( 'NONE',  ( -12.64341534048310045, 1502.151632001139888, 210.8278707494170021 ) ) ;
#52175 = CARTESIAN_POINT ( 'NONE',  ( 7.220783133089999417, 1493.964658354389940, 218.1716920474590040 ) ) ;
#52176 = CARTESIAN_POINT ( 'NONE',  ( -14.15052379810000005, 1379.587026329759965, 207.9895299807990057 ) ) ;
#52177 = CARTESIAN_POINT ( 'NONE',  ( 0.02188712286643353447, 1410.253115378247912, 233.2197962875069379 ) ) ;
#52178 = EDGE_CURVE ( 'NONE', #85990, #81697, #106703, .T. ) ;
#52180 = CARTESIAN_POINT ( 'NONE',  ( 16.71340900559999909, 1489.468502498129965, 194.5581736820979870 ) ) ;
#52179 = CARTESIAN_POINT ( 'NONE',  ( -3.699130484579999933, 1497.303414919790157, 198.4797053902989887 ) ) ;
#52181 = CARTESIAN_POINT ( 'NONE',  ( -4.400896008966714845, 1423.841311741514801, 184.2785382031196377 ) ) ;
#52182 = CARTESIAN_POINT ( 'NONE',  ( 17.99786997119990062, 1423.579729440439905, 225.1773348763740046 ) ) ;
#52183 = FACE_OUTER_BOUND ( 'NONE', #72739, .T. ) ;
#52184 = VERTEX_POINT ( 'NONE', #21860 ) ;
#52185 = CIRCLE ( 'NONE', #77194, 29.84605316733869174 ) ;
#52186 = ADVANCED_FACE ( 'NONE', ( #105923 ), #4019, .F. ) ;
#52187 = CARTESIAN_POINT ( 'NONE',  ( 38.63621011600843502, 1450.019461304174456, 134.8312852903657415 ) ) ;
#52188 = CARTESIAN_POINT ( 'NONE',  ( -2.971677051434508776, 1485.527647794828226, 182.7973173799614131 ) ) ;
#52189 = CARTESIAN_POINT ( 'NONE',  ( -14.80222597220000047, 1415.865102022439942, 213.2039056074190171 ) ) ;
#52190 = EDGE_CURVE ( 'NONE', #46077, #73174, #7736, .T. ) ;
#52192 = ORIENTED_EDGE ( 'NONE', *, *, #35830, .T. ) ;
#52191 = CARTESIAN_POINT ( 'NONE',  ( 1.130521170281699961, 1515.098624608320051, 204.7932831006150138 ) ) ;
#52193 = CARTESIAN_POINT ( 'NONE',  ( 17.33645362950000290, 1414.996442546130083, 210.3925741896480304 ) ) ;
#52194 = DIRECTION ( 'NONE',  ( 0.4978433412588811335, 0.000000000000000000, 0.8672669759446587356 ) ) ;
#52195 = CARTESIAN_POINT ( 'NONE',  ( -11.26505527650000005, 1429.630426659629848, 150.9929481330979968 ) ) ;
#52196 = CARTESIAN_POINT ( 'NONE',  ( 19.33960037451650038, 1456.940524333479971, 224.5990868967689948 ) ) ;
#52197 = CARTESIAN_POINT ( 'NONE',  ( -10.95020795142180070, 1462.043827289809997, 210.3303817636600002 ) ) ;
#52198 = EDGE_CURVE ( 'NONE', #43546, #80530, #73198, .T. ) ;
#52199 = CARTESIAN_POINT ( 'NONE',  ( 3.909710721586100224, 1517.051704408389924, 220.4764703678949900 ) ) ;
#52200 = LINE ( 'NONE', #85773, #9154 ) ;
#52201 = CARTESIAN_POINT ( 'NONE',  ( -16.42424932566499862, 1513.961173499609913, 223.7109085266669979 ) ) ;
#52202 = EDGE_CURVE ( 'NONE', #90117, #71856, #37765, .T. ) ;
#52203 = CARTESIAN_POINT ( 'NONE',  ( 16.35241204879999799, 1473.763677363790066, 196.1841466627989803 ) ) ;
#52204 = CARTESIAN_POINT ( 'NONE',  ( -9.562019153030000496, 1479.258837048789928, 214.5473981509090038 ) ) ;
#52205 = CARTESIAN_POINT ( 'NONE',  ( -16.67053790319999962, 1460.330596138029932, 228.3373634785979789 ) ) ;
#52206 = CARTESIAN_POINT ( 'NONE',  ( 2.476733476015000157, 1516.858326417339867, 206.6281461634669938 ) ) ;
#52207 = CARTESIAN_POINT ( 'NONE',  ( 30.12542694869999593, 1414.418184686029917, 268.6829023064980220 ) ) ;
#52208 = AXIS2_PLACEMENT_3D ( 'NONE', #38753, #40405, #74582 ) ;
#52209 = CARTESIAN_POINT ( 'NONE',  ( 23.55466122310000188, 1435.319754623780000, 138.4646105849980131 ) ) ;
#52210 = EDGE_CURVE ( 'NONE', #43597, #9501, #29170, .T. ) ;
#52211 = CARTESIAN_POINT ( 'NONE',  ( 18.66630351470000093, 1449.735460805310140, 191.4766007327979764 ) ) ;
#52212 = CARTESIAN_POINT ( 'NONE',  ( -21.59755472069999982, 1429.927022223929953, 220.3212187975979930 ) ) ;
#52213 = FACE_OUTER_BOUND ( 'NONE', #17965, .T. ) ;
#52214 = CARTESIAN_POINT ( 'NONE',  ( 17.22845782853287488, 1525.848196786131211, 236.4819750992561467 ) ) ;
#52215 = CARTESIAN_POINT ( 'NONE',  ( 6.674324621289978055, 1480.055983087696859, 228.4398896743051068 ) ) ;
#52216 = CARTESIAN_POINT ( 'NONE',  ( -13.85929445549190042, 1410.325638904459993, 227.0940372234059907 ) ) ;
#52217 = CARTESIAN_POINT ( 'NONE',  ( -16.90152335259999816, 1414.971339025629959, 205.6657720955479931 ) ) ;
#52218 = CARTESIAN_POINT ( 'NONE',  ( -12.23547426050000020, 1441.747762228240163, 187.6912675146980121 ) ) ;
#52219 = CARTESIAN_POINT ( 'NONE',  ( -2.519506328514930171, 1485.538153147889943, 197.4903980647760022 ) ) ;
#52220 = CARTESIAN_POINT ( 'NONE',  ( -33.52368713759999963, 1436.996791544049984, 136.5733088107979825 ) ) ;
#52221 = CARTESIAN_POINT ( 'NONE',  ( -4.922266137120000273, 1497.746000166390104, 220.5680551797990177 ) ) ;
#52222 = ORIENTED_EDGE ( 'NONE', *, *, #30892, .F. ) ;
#52223 = CARTESIAN_POINT ( 'NONE',  ( -2.325731141814999958, 1511.751588929339960, 201.5380540260670159 ) ) ;
#52224 = CARTESIAN_POINT ( 'NONE',  ( -14.56057633080500047, 1409.421526917029951, 205.7954462250399956 ) ) ;
#52225 = CARTESIAN_POINT ( 'NONE',  ( 11.26238334597741719, 1425.491802413522009, 138.6337954581835845 ) ) ;
#52226 = CARTESIAN_POINT ( 'NONE',  ( -5.327792725146696995, 1422.321596787008048, 138.7601748833760666 ) ) ;
#52227 = CARTESIAN_POINT ( 'NONE',  ( -21.97983258780000071, 1471.906657365530009, 268.2775703267980134 ) ) ;
#52228 = B_SPLINE_CURVE_WITH_KNOTS ( 'NONE', 5,
 ( #9626, #36498, #52760, #86896, #44363, #78508, #52215, #77947, #1818 ),
 .UNSPECIFIED., .F., .F.,
 ( 6, 3, 6 ),
 ( 0.000000000000000000, 0.7707393916760963970, 1.000000000000000000 ),
 .UNSPECIFIED. ) ;
#52229 = CARTESIAN_POINT ( 'NONE',  ( -30.29139560038384360, 1523.843271061948826, 195.7510757303778064 ) ) ;
#52230 = CARTESIAN_POINT ( 'NONE',  ( 32.86802468386284914, 1523.481610426287716, 201.0396662540042030 ) ) ;
#52231 = CARTESIAN_POINT ( 'NONE',  ( -24.42065677639604004, 1444.677908474019205, 211.1079349083759098 ) ) ;
#52232 = CARTESIAN_POINT ( 'NONE',  ( -64.65996261591139671, 1384.678844644059836, 288.2602538484970296 ) ) ;
#52233 = CARTESIAN_POINT ( 'NONE',  ( 19.02704169900689735, 1456.915441405320053, 225.6706379604710264 ) ) ;
#52234 = CARTESIAN_POINT ( 'NONE',  ( -0.4151546846821903003, 1522.382868172863937, 242.9330574173806951 ) ) ;
#52235 = CARTESIAN_POINT ( 'NONE',  ( 14.57172186319999874, 1416.216739748630062, 219.6692783647980036 ) ) ;
#52236 = CARTESIAN_POINT ( 'NONE',  ( 11.70773956419579953, 1415.348334734299897, 223.0287674909799875 ) ) ;
#52237 = ADVANCED_FACE ( 'NONE', ( #34155 ), #94858, .F. ) ;
#52238 = FACE_OUTER_BOUND ( 'NONE', #84411, .T. ) ;
#52239 = CARTESIAN_POINT ( 'NONE',  ( -7.545064063707340729, 1384.907232462019920, 219.0876311385090105 ) ) ;
#52240 = DIRECTION ( 'NONE',  ( -0.9536973892116009655, 0.1200132912778490019, -0.2757863298418440356 ) ) ;
#52241 = CARTESIAN_POINT ( 'NONE',  ( -23.69628899429999791, 1410.235927737129941, 207.8525723050880174 ) ) ;
#52242 = EDGE_CURVE ( 'NONE', #75187, #105162, #96838, .T. ) ;
#52243 = CARTESIAN_POINT ( 'NONE',  ( -156.6846457583342840, 1524.382868172863937, 340.9912860285748479 ) ) ;
#52244 = CIRCLE ( 'NONE', #12885, 6.771217174059998456 ) ;
#52245 = CARTESIAN_POINT ( 'NONE',  ( 3.842540062219999886, 1485.442838166189858, 219.2998310712989962 ) ) ;
#52246 = CARTESIAN_POINT ( 'NONE',  ( 5.057113137720000040, 1424.030137378339987, 193.7146021066990045 ) ) ;
#52247 = B_SPLINE_CURVE_WITH_KNOTS ( 'NONE', 3,
 ( #40444, #72965, #81337, #108755, #81891, #32047, #66236, #100355, #21418, #107658, #23643, #57825, #72425, #91951, #29844, #13024, #60029, #51616, #41563, #84097, #672, #102537, #24177, #93047, #94706, #83541, #85197, #17982, #58365, #8484, #58916, #75718, #6834, #75173, #94147, #109864, #16320, #76812, #34251, #128 ),
 .UNSPECIFIED., .F., .F.,
 ( 4, 3, 3, 3, 3, 3, 3, 3, 3, 3, 3, 3, 3, 4 ),
 ( -168.1723202510000021, -162.2888149943200062, -153.5620393927819975, -144.4833429881919926, -135.1231727132679907, -125.1025808913170039, -114.4147035693629988, -102.6255519937520120, -87.74092214761390096, -72.67910686651640617, -60.92308613310270005, -50.23111378371720548, -40.21016113735100816, -30.67014438050000535 ),
 .UNSPECIFIED. ) ;
#52248 = CARTESIAN_POINT ( 'NONE',  ( 0.8327748425420000711, 1442.756953654829886, 150.7628527808980152 ) ) ;
#52249 = CARTESIAN_POINT ( 'NONE',  ( 18.90935262129999828, 1456.544091939490045, 200.1670491895490045 ) ) ;
#52250 = CARTESIAN_POINT ( 'NONE',  ( -3.892696961574322323, 1515.551704300027950, 210.6723164294263029 ) ) ;
#52251 = CARTESIAN_POINT ( 'NONE',  ( -37.65047686723229958, 1442.773887284729881, 137.1096749952629921 ) ) ;
#52253 = CARTESIAN_POINT ( 'NONE',  ( -8.029416465979998918, 1383.927159441839876, 199.5752583396389923 ) ) ;
#52252 = CARTESIAN_POINT ( 'NONE',  ( -22.16158675810000034, 1409.686960050029938, 210.4767810254680001 ) ) ;
#52254 = CARTESIAN_POINT ( 'NONE',  ( 1.075780832630000017, 1414.392608856630204, 233.0977785888980236 ) ) ;
#52255 = CARTESIAN_POINT ( 'NONE',  ( 9.691987769041398693, 1436.253413666279812, 210.7989517529429975 ) ) ;
#52256 = CARTESIAN_POINT ( 'NONE',  ( -10.95999825190000010, 1490.767389346189930, 211.0929827415589841 ) ) ;
#52257 = CARTESIAN_POINT ( 'NONE',  ( 3.728847569731689848, 1446.583145393379937, 199.6841023494010017 ) ) ;
#52258 = CARTESIAN_POINT ( 'NONE',  ( -1.775961533719359942, 1421.047340809089974, 184.1901329777589922 ) ) ;
#52259 = EDGE_CURVE ( 'NONE', #76760, #86613, #95507, .T. ) ;
#52260 = CARTESIAN_POINT ( 'NONE',  ( 2.870951667784999994, 1517.111322026010157, 202.5592101095969895 ) ) ;
#52261 = CARTESIAN_POINT ( 'NONE',  ( -4.254615091958411810, 1398.039996049444881, 221.4059216359357265 ) ) ;
#52262 = CARTESIAN_POINT ( 'NONE',  ( -3.119330264448041845, 1440.523299896550043, 157.1480219251303367 ) ) ;
#52263 = CARTESIAN_POINT ( 'NONE',  ( 14.02295695628119887, 1432.459693560080041, 221.0332480332689897 ) ) ;
#52264 = CARTESIAN_POINT ( 'NONE',  ( 1.443907308950000079, 1507.678956818529741, 236.8026632909979980 ) ) ;
#52265 = AXIS2_PLACEMENT_3D ( 'NONE', #50259, #18267, #59209 ) ;
#52266 = CARTESIAN_POINT ( 'NONE',  ( 5.662322984621799726, 1504.894625891569831, 220.5557319434630017 ) ) ;
#52267 = CARTESIAN_POINT ( 'NONE',  ( 40.21518593132410047, 1445.085294981540073, 136.9476663967080015 ) ) ;
#52269 = VERTEX_POINT ( 'NONE', #52628 ) ;
#52268 = CARTESIAN_POINT ( 'NONE',  ( -66.42203761300000053, 1379.747445253800151, 277.0326445461590197 ) ) ;
#52270 = ORIENTED_EDGE ( 'NONE', *, *, #11395, .T. ) ;
#52271 = CARTESIAN_POINT ( 'NONE',  ( 11.15310914653060159, 1434.045385467309870, 151.6482511736529943 ) ) ;
#52272 = CARTESIAN_POINT ( 'NONE',  ( 27.56163678460000099, 1509.624398677929776, 215.4636615634079817 ) ) ;
#52273 = ORIENTED_EDGE ( 'NONE', *, *, #34350, .T. ) ;
#52274 = CARTESIAN_POINT ( 'NONE',  ( -106.6765851849999933, 1378.991158695870126, 307.6173790219590387 ) ) ;
#52275 = CARTESIAN_POINT ( 'NONE',  ( -10.34166276688940123, 1447.760272548699959, 209.7025959161350102 ) ) ;
#52276 = CARTESIAN_POINT ( 'NONE',  ( -2.500000000000000000, 1432.413060387330006, 146.1721969590979882 ) ) ;
#52278 = CARTESIAN_POINT ( 'NONE',  ( 11.16223122930000144, 1428.970455832429934, 101.8807690336980016 ) ) ;
#52277 = CARTESIAN_POINT ( 'NONE',  ( 3.827327205999999649, 1424.046157813729906, 177.8294128217980017 ) ) ;
#52279 = CARTESIAN_POINT ( 'NONE',  ( 18.08978621609999848, 1507.814340215129732, 230.4555789890980009 ) ) ;
#52280 = ADVANCED_FACE ( 'NONE', ( #17879 ), #101946, .F. ) ;
#52281 = DIRECTION ( 'NONE',  ( 0.000000000000000000, 0.000000000000000000, 1.000000000000000000 ) ) ;
#52282 = CARTESIAN_POINT ( 'NONE',  ( -2.576993086239999897, 1414.913060387329779, 192.9504896103979945 ) ) ;
#52283 = CARTESIAN_POINT ( 'NONE',  ( 15.88129808800000120, 1409.969386305029957, 226.7471413913980030 ) ) ;
#52284 = CARTESIAN_POINT ( 'NONE',  ( 3.268859396054999866, 1516.922519270759949, 211.5998327024669834 ) ) ;
#52285 = CARTESIAN_POINT ( 'NONE',  ( 13.73229811442000248, 1415.184612914949867, 197.5903291147609764 ) ) ;
#52286 = CARTESIAN_POINT ( 'NONE',  ( -4.761835946750000659, 1382.817942133689940, 214.6047291967390152 ) ) ;
#52287 = CARTESIAN_POINT ( 'NONE',  ( 7.072298189685000125, 1512.974587999910000, 201.9513001534670309 ) ) ;
#52288 = EDGE_LOOP ( 'NONE', ( #92458, #84615, #107518, #20167 ) ) ;
#52289 = CARTESIAN_POINT ( 'NONE',  ( 13.90221499949599959, 1436.238194080860012, 150.2928919302390227 ) ) ;
#52290 = EDGE_CURVE ( 'NONE', #44146, #104880, #102090, .T. ) ;
#52291 = CARTESIAN_POINT ( 'NONE',  ( -1.005805788909989840, 1431.851947266499792, 200.7719531180060244 ) ) ;
#52292 = ORIENTED_EDGE ( 'NONE', *, *, #58614, .T. ) ;
#52293 = ORIENTED_EDGE ( 'NONE', *, *, #37818, .T. ) ;
#52294 = CARTESIAN_POINT ( 'NONE',  ( 12.70061752951238887, 1445.015675426939197, 169.4597949495606883 ) ) ;
#52295 = CARTESIAN_POINT ( 'NONE',  ( 16.37694613928643150, 1512.916366990907363, 197.5610450319645679 ) ) ;
#52296 = CARTESIAN_POINT ( 'NONE',  ( -11.36959371680000075, 1503.847165134090119, 207.0750569533189775 ) ) ;
#52297 = CARTESIAN_POINT ( 'NONE',  ( -4.616899872884999922, 1517.050041317280147, 216.8443827349270236 ) ) ;
#52299 = CARTESIAN_POINT ( 'NONE',  ( -1.636057583032799911, 1465.068318594939910, 198.2397572230070182 ) ) ;
#52298 = B_SPLINE_CURVE_WITH_KNOTS ( 'NONE', 5,
 ( #54161, #105653, #2653, #70972, #98880, #79895, #55257, #13204, #106726 ),
 .UNSPECIFIED., .F., .F.,
 ( 6, 3, 6 ),
 ( 21.34408555294309906, 21.90163172499999789, 30.14216317859590077 ),
 .UNSPECIFIED. ) ;
#52300 = CARTESIAN_POINT ( 'NONE',  ( -19.07368456369233556, 1442.271103625454771, 210.5520796240281811 ) ) ;
#52301 = CARTESIAN_POINT ( 'NONE',  ( -24.68953382638999372, 1379.615025458047285, 210.8754759576296181 ) ) ;
#52302 = CARTESIAN_POINT ( 'NONE',  ( 4.244840198528499364, 1446.426887755389998, 161.9784992303009972 ) ) ;
#52303 = EDGE_CURVE ( 'NONE', #109826, #77569, #62830, .T. ) ;
#52304 = CARTESIAN_POINT ( 'NONE',  ( 0.4675733539479999812, 1508.925830125129778, 238.6310950794979817 ) ) ;
#52305 = ORIENTED_EDGE ( 'NONE', *, *, #100694, .T. ) ;
#52306 = CARTESIAN_POINT ( 'NONE',  ( 2.282915183265000092, 1516.876240617270014, 206.6278256496669883 ) ) ;
#52307 = EDGE_LOOP ( 'NONE', ( #83288, #17387, #73380, #65203 ) ) ;
#52308 = CARTESIAN_POINT ( 'NONE',  ( 21.38805416096829859, 1440.913060387330006, 224.3727411978530029 ) ) ;
#52309 = CARTESIAN_POINT ( 'NONE',  ( -19.59880086690000311, 1507.802454088529885, 229.4381582326980151 ) ) ;
#52310 = EDGE_CURVE ( 'NONE', #43776, #72498, #96839, .T. ) ;
#52311 = VERTEX_POINT ( 'NONE', #2248 ) ;
#52312 = CARTESIAN_POINT ( 'NONE',  ( -7.012473013355389639, 1508.551704609589933, 203.6085845825829779 ) ) ;
#52313 = CARTESIAN_POINT ( 'NONE',  ( -14.70465958249999971, 1409.593213617929905, 191.2178800344979948 ) ) ;
#52314 = CARTESIAN_POINT ( 'NONE',  ( -24.34654694089999794, 1442.312289605810065, 211.4248143116180358 ) ) ;
#52316 = ORIENTED_EDGE ( 'NONE', *, *, #83741, .T. ) ;
#52315 = CARTESIAN_POINT ( 'NONE',  ( 4.905383437976600369, 1424.139022048180095, 193.2146529292390085 ) ) ;
#52317 = CARTESIAN_POINT ( 'NONE',  ( -5.925858265440809625, 1511.532396045849964, 201.1754967935600007 ) ) ;
#52318 = CARTESIAN_POINT ( 'NONE',  ( -2.407253779970412566, 1523.313115944345554, 175.0653106450178882 ) ) ;
#52319 = DIRECTION ( 'NONE',  ( 1.755985294532469921E-16, -1.000000000000000000, 1.338183447452831989E-16 ) ) ;
#52320 = DIRECTION ( 'NONE',  ( 1.224646799147350002E-16, -1.836970198721029688E-16, -1.000000000000000000 ) ) ;
#52321 = EDGE_CURVE ( 'NONE', #82812, #103332, #43119, .T. ) ;
#52323 = DIRECTION ( 'NONE',  ( -1.000000000000000000, 0.000000000000000000, 0.000000000000000000 ) ) ;
#52322 = CARTESIAN_POINT ( 'NONE',  ( 21.38516915557964282, 1522.382868172863937, 180.3939891059721106 ) ) ;
#52324 = CARTESIAN_POINT ( 'NONE',  ( 6.945490048805000427, 1516.932669162149978, 214.9002185338470099 ) ) ;
#52325 = ADVANCED_FACE ( 'NONE', ( #60482 ), #36465, .T. ) ;
#52326 = CARTESIAN_POINT ( 'NONE',  ( -2.863667357675800496, 1428.996785130359967, 200.2011281577639750 ) ) ;
#52327 = CARTESIAN_POINT ( 'NONE',  ( -20.84948682980000001, 1508.934641637929872, 190.2319761415980111 ) ) ;
#52328 = CARTESIAN_POINT ( 'NONE',  ( 28.66654218860000114, 1509.598009363130132, 207.9792368166280028 ) ) ;
#52329 = CARTESIAN_POINT ( 'NONE',  ( 2.299656316094999653, 1516.843453247299749, 211.5982966343670171 ) ) ;
#52330 = CARTESIAN_POINT ( 'NONE',  ( 14.44229455070000157, 1409.585625628630169, 192.0310987722980087 ) ) ;
#52331 = CARTESIAN_POINT ( 'NONE',  ( -17.60921851184225417, 1486.151197990332548, 188.1605117022275522 ) ) ;
#52333 = VERTEX_POINT ( 'NONE', #41874 ) ;
#52332 = CARTESIAN_POINT ( 'NONE',  ( -81.69295930340000211, 1388.108283263359908, 304.1383302712590080 ) ) ;
#52334 = CARTESIAN_POINT ( 'NONE',  ( 33.33289073369999755, 1445.199364519750134, 248.0947902374979890 ) ) ;
#52335 = CARTESIAN_POINT ( 'NONE',  ( 10.52331109828659983, 1491.075809623180021, 212.3133573343550040 ) ) ;
#52336 = CARTESIAN_POINT ( 'NONE',  ( -28.50728667541919847, 1509.908556774140152, 216.1167956888880042 ) ) ;
#52337 = B_SPLINE_CURVE_WITH_KNOTS ( 'NONE', 3,
 ( #62831, #53299, #104785, #61169 ),
 .UNSPECIFIED., .F., .F.,
 ( 4, 4 ),
 ( 0.000000000000000000, 1.000000000000000000 ),
 .UNSPECIFIED. ) ;
#52338 = CARTESIAN_POINT ( 'NONE',  ( -8.364995774877499457, 1509.202158754189895, 236.9158755863900012 ) ) ;
#52339 = ADVANCED_FACE ( 'NONE', ( #7715 ), #25048, .F. ) ;
#52340 = CARTESIAN_POINT ( 'NONE',  ( -21.73553347590000229, 1452.603807136129944, 221.7739260095980001 ) ) ;
#52342 = CARTESIAN_POINT ( 'NONE',  ( 19.01828621289999788, 1456.631844032529898, 226.0087226235980040 ) ) ;
#52341 = CARTESIAN_POINT ( 'NONE',  ( -3995.587774573430124, 778.1435722443549139, 210.2209376587489942 ) ) ;
#52343 = CARTESIAN_POINT ( 'NONE',  ( -8.301987938657498844, 1519.913060387329779, 185.0111222839169898 ) ) ;
#52344 = CARTESIAN_POINT ( 'NONE',  ( -108.0278876277179876, 1382.536111722130045, 310.5170612373680115 ) ) ;
#52345 = VERTEX_POINT ( 'NONE', #110179 ) ;
#52346 = CARTESIAN_POINT ( 'NONE',  ( 3.255967386345000047, 1516.989560013210166, 204.1101670940770134 ) ) ;
#52347 = CARTESIAN_POINT ( 'NONE',  ( 0.3357109459749999525, 1406.507447809929999, 269.4986534845979236 ) ) ;
#52348 = EDGE_CURVE ( 'NONE', #36440, #18252, #100663, .T. ) ;
#52349 = AXIS2_PLACEMENT_3D ( 'NONE', #6596, #91700, #15522 ) ;
#52350 = CARTESIAN_POINT ( 'NONE',  ( 28.62254820377552278, 1526.345556099435726, 198.0531334975491973 ) ) ;
#52351 = B_SPLINE_CURVE_WITH_KNOTS ( 'NONE', 5,
 ( #29400, #63603, #52981, #36167, #35601, #19898, #55195, #70351, #46249, #89321, #54100, #103912 ),
 .UNSPECIFIED., .F., .F.,
 ( 6, 3, 3, 6 ),
 ( 0.000000000000000000, 0.2428673809476307177, 0.7286021428483020479, 1.000000000000000000 ),
 .UNSPECIFIED. ) ;
#52352 = CARTESIAN_POINT ( 'NONE',  ( 13.09755946009999938, 1428.691652272130113, 223.5005393930979949 ) ) ;
#52353 =( BOUNDED_CURVE ( )  B_SPLINE_CURVE ( 3, ( #4793, #37864, #55790, #71509 ),
 .UNSPECIFIED., .F., .F. ) 
 B_SPLINE_CURVE_WITH_KNOTS ( ( 4, 4 ),
 ( 4.712388980384758952, 7.353981633974552068 ),
 .UNSPECIFIED. ) 
 CURVE ( )  GEOMETRIC_REPRESENTATION_ITEM ( )  RATIONAL_B_SPLINE_CURVE ( ( 1.000000000000000000, 0.4982693061696819581, 0.4982693061696819581, 1.000000000000000000 ) ) 
 REPRESENTATION_ITEM ( '' )  );
#52354 = CARTESIAN_POINT ( 'NONE',  ( 22.75273496409577945, 1518.913060387330006, 183.6728937936772184 ) ) ;
#52355 = CARTESIAN_POINT ( 'NONE',  ( -40.11829264410000206, 1445.561899567880118, 136.8687421407979912 ) ) ;
#52356 = CARTESIAN_POINT ( 'NONE',  ( 6.039845038650000220, 1450.200509660590114, 208.6657063127539971 ) ) ;
#52357 = CARTESIAN_POINT ( 'NONE',  ( -40.53150014929950373, 1440.913060405800024, 260.0257716865519910 ) ) ;
#52358 = CARTESIAN_POINT ( 'NONE',  ( 37.23777575920910721, 1449.393681520200289, 136.3086112982300335 ) ) ;
#52359 = FACE_OUTER_BOUND ( 'NONE', #79400, .T. ) ;
#52360 = FACE_OUTER_BOUND ( 'NONE', #66611, .T. ) ;
#52361 = CARTESIAN_POINT ( 'NONE',  ( 10.57326081867249989, 1481.032691398090037, 210.7950195358730241 ) ) ;
#52362 = CARTESIAN_POINT ( 'NONE',  ( -0.5682668705760020034, 1506.801775235190007, 221.9434713837989932 ) ) ;
#52363 = CARTESIAN_POINT ( 'NONE',  ( -8.254331781353046793, 1448.308236332938350, 213.1040624623483950 ) ) ;
#52364 = ORIENTED_EDGE ( 'NONE', *, *, #43925, .T. ) ;
#52365 = CARTESIAN_POINT ( 'NONE',  ( 2.424063131930000115, 1427.257651041929876, 147.9020499575979954 ) ) ;
#52366 = CARTESIAN_POINT ( 'NONE',  ( 3.392304019253070013, 1456.149158459580121, 219.1891682523919940 ) ) ;
#52367 = CARTESIAN_POINT ( 'NONE',  ( 2.645773951119999801, 1485.597577325490192, 198.6813594259990055 ) ) ;
#52368 = CARTESIAN_POINT ( 'NONE',  ( 16.26863210207389798, 1486.460469297460122, 188.7573094889239940 ) ) ;
#52369 = CARTESIAN_POINT ( 'NONE',  ( 11.43347548804394620, 1425.764712714644475, 138.9807451318896483 ) ) ;
#52370 = CARTESIAN_POINT ( 'NONE',  ( 11.49924241569999950, 1502.518364560089822, 209.1346295538230038 ) ) ;
#52371 = CARTESIAN_POINT ( 'NONE',  ( -33.82780500856058836, 1523.429859730330463, 197.6825146852533237 ) ) ;
#52372 = CARTESIAN_POINT ( 'NONE',  ( 19.77969251879999746, 1507.818093401829856, 229.2755605921979907 ) ) ;
#52373 = CARTESIAN_POINT ( 'NONE',  ( -19.06115223335860165, 1384.865189719420187, 220.5788536041530108 ) ) ;
#52374 = CARTESIAN_POINT ( 'NONE',  ( -31.23437356469425907, 1512.187213306747481, 222.8968241038848248 ) ) ;
#52375 = CARTESIAN_POINT ( 'NONE',  ( -17.36801834869999794, 1414.983773852829927, 207.7378529790379957 ) ) ;
#52376 = CARTESIAN_POINT ( 'NONE',  ( 3.829620154741123716, 1515.551704408389696, 212.3304832152426229 ) ) ;
#52377 = CARTESIAN_POINT ( 'NONE',  ( 25.03889118680000081, 1435.391010761600000, 136.0112995284980002 ) ) ;
#52378 = B_SPLINE_CURVE_WITH_KNOTS ( 'NONE', 5,
 ( #88183, #55697, #46196, #79790, #47275, #13090 ),
 .UNSPECIFIED., .F., .F.,
 ( 6, 6 ),
 ( 16.38547747492637896, 26.49451346759999737 ),
 .UNSPECIFIED. ) ;
#52379 = CARTESIAN_POINT ( 'NONE',  ( -6.241370329288110419, 1396.131013841920094, 200.0124121438620080 ) ) ;
#52380 = ORIENTED_EDGE ( 'NONE', *, *, #9651, .F. ) ;
#52381 =( BOUNDED_SURFACE ( )  B_SPLINE_SURFACE ( 3, 2, ( 
 ( #72807, #45951, #97445 ),
 ( #98534, #71741, #89033 ),
 ( #106396, #64959, #21245 ),
 ( #12323, #46512, #89586 ),
 ( #106935, #108033, #22352 ),
 ( #90682, #30223, #21802 ) ),
 .UNSPECIFIED., .F., .F., .T. ) 
 B_SPLINE_SURFACE_WITH_KNOTS ( ( 4, 2, 4 ),
 ( 3, 3 ),
 ( -6.440160904563896338E-17, 0.001312027981647337100, 0.002624055963294738385 ),
 ( 0.000000000000000000, 1.000000000000000000 ),
 .UNSPECIFIED. ) 
 GEOMETRIC_REPRESENTATION_ITEM ( )  RATIONAL_B_SPLINE_SURFACE ( (
 ( 1.000000000000000000, 0.9376006582765872288, 1.000000000000000000),
 ( 1.000000000000000000, 0.9569320108031740268, 1.000000000000000000),
 ( 1.000000000000000000, 0.9725743441606660156, 1.000000000000000000),
 ( 1.000000000000000000, 0.9942095667147807792, 1.000000000000000000),
 ( 1.000000000000000000, 1.000043666449794921, 1.000000000000000000),
 ( 1.000000000000000000, 1.000000000000000000, 1.000000000000000000) ) ) 
 REPRESENTATION_ITEM ( '' )  SURFACE ( )  );
#52382 = CARTESIAN_POINT ( 'NONE',  ( 30.31940284292409515, 1523.382868172864164, 195.7503880523414352 ) ) ;
#52383 = CARTESIAN_POINT ( 'NONE',  ( -6.817824598025731042, 1490.769479965739720, 213.3956848422870110 ) ) ;
#52384 = ORIENTED_EDGE ( 'NONE', *, *, #17773, .F. ) ;
#52385 = VERTEX_POINT ( 'NONE', #50832 ) ;
#52386 = CARTESIAN_POINT ( 'NONE',  ( -11.33475729309999913, 1500.341569084289858, 210.4138247025489932 ) ) ;
#52387 = CARTESIAN_POINT ( 'NONE',  ( 7.156843037479131198, 1516.545712885865214, 206.8754839868354907 ) ) ;
#52389 = CARTESIAN_POINT ( 'NONE',  ( -9.972525074869899697, 1439.148125713659965, 209.2054671327859694 ) ) ;
#52388 = CARTESIAN_POINT ( 'NONE',  ( 11.00536806779999921, 1426.523248317530033, 91.15359103569791444 ) ) ;
#52390 = CARTESIAN_POINT ( 'NONE',  ( 2.041884302589999756, 1451.400483888490044, 190.0484128324990252 ) ) ;
#52391 = CARTESIAN_POINT ( 'NONE',  ( 4.148789385605260449, 1424.601256096389989, 184.9569090508520048 ) ) ;
#52392 = CARTESIAN_POINT ( 'NONE',  ( -2.861850767359648273, 1419.693532390741893, 186.1800267117334897 ) ) ;
#52393 = CARTESIAN_POINT ( 'NONE',  ( 7.535581150919999693, 1424.790543398920136, 212.1876082168290054 ) ) ;
#52394 = CARTESIAN_POINT ( 'NONE',  ( 20.75865325819999896, 1455.056399776190119, 207.3304373729289978 ) ) ;
#52395 = FACE_OUTER_BOUND ( 'NONE', #50793, .T. ) ;
#52396 = CARTESIAN_POINT ( 'NONE',  ( -105.6009733815480018, 1377.068166733269891, 306.8927961940029832 ) ) ;
#52397 = CARTESIAN_POINT ( 'NONE',  ( 8.731338020832811964, 1365.274321608607124, 210.6218459617142003 ) ) ;
#52399 = ORIENTED_EDGE ( 'NONE', *, *, #81097, .F. ) ;
#52398 = CARTESIAN_POINT ( 'NONE',  ( -5.513435596820279727, 1509.038615934079871, 216.6345961782780023 ) ) ;
#52400 = VERTEX_POINT ( 'NONE', #57602 ) ;
#52401 = CARTESIAN_POINT ( 'NONE',  ( 19.53786426059039982, 1512.187213306747481, 236.7197124308265188 ) ) ;
#52402 = CARTESIAN_POINT ( 'NONE',  ( 7.550614469730767553, 1510.484595326600129, 203.5546347261997937 ) ) ;
#52403 = CARTESIAN_POINT ( 'NONE',  ( -2.654130549429999957E-10, 1472.045055685429816, 270.0713874941980066 ) ) ;
#52404 = CARTESIAN_POINT ( 'NONE',  ( 12.53132851702783945, 1434.462080285801449, 147.2718985355009238 ) ) ;
#52405 = CARTESIAN_POINT ( 'NONE',  ( -2.052286426879999848, 1486.111609172430008, 181.8527502747979838 ) ) ;
#52406 = CARTESIAN_POINT ( 'NONE',  ( -0.03257067699863269716, 1475.780217561950167, 197.6613938121659828 ) ) ;
#52407 = CARTESIAN_POINT ( 'NONE',  ( -49.24962907673571522, 1524.382868172863937, 407.9033880519289710 ) ) ;
#52408 = CARTESIAN_POINT ( 'NONE',  ( -2.500000000000000000, 1448.532394040329791, 160.1065257882549986 ) ) ;
#52409 = CARTESIAN_POINT ( 'NONE',  ( 9.389216481230956646, 1368.118150840410408, 210.6218459617030021 ) ) ;
#52410 = CARTESIAN_POINT ( 'NONE',  ( 13.45819569170899932, 1408.065586298919925, 204.5788124947870017 ) ) ;
#52411 = CARTESIAN_POINT ( 'NONE',  ( -8.399633448627239929, 1406.327446574869782, 268.4546571330000120 ) ) ;
#52412 = CARTESIAN_POINT ( 'NONE',  ( -13.94839511594039827, 1435.086904260040001, 149.1659738623210103 ) ) ;
#52413 = VERTEX_POINT ( 'NONE', #6618 ) ;
#52414 = CARTESIAN_POINT ( 'NONE',  ( 3.289090359600000291, 1441.224765589789968, 218.4797294130789851 ) ) ;
#52415 = CARTESIAN_POINT ( 'NONE',  ( 13.55140343089999888, 1443.942093640929897, 188.2793544314979783 ) ) ;
#52416 = ORIENTED_EDGE ( 'NONE', *, *, #110594, .F. ) ;
#52417 = ORIENTED_EDGE ( 'NONE', *, *, #20601, .T. ) ;
#52418 = CARTESIAN_POINT ( 'NONE',  ( -22.75273496409559826, 1512.187213306747481, 234.5707981297189235 ) ) ;
#52419 = CARTESIAN_POINT ( 'NONE',  ( -8.910387285859998840, 1362.858511851210096, 207.6218459616989946 ) ) ;
#52420 = CARTESIAN_POINT ( 'NONE',  ( -0.7365612166329978949, 1517.066898074209803, 213.7457380308570123 ) ) ;
#52421 = CARTESIAN_POINT ( 'NONE',  ( 4.461625796074999428, 1510.696675236759802, 216.6780121820170280 ) ) ;
#52422 = B_SPLINE_SURFACE_WITH_KNOTS ( 'NONE', 5, 5, ( 
 ( #47834, #38317, #5274, #71975, #89281, #73041 ),
 ( #54610, #30472, #3658, #63566, #39430, #97681 ),
 ( #107735, #31020, #20955, #56791, #90928, #55159 ),
 ( #48400, #46759, #14215, #59006, #50052, #101514 ),
 ( #58448, #85273, #33226, #57365, #16945, #8024 ),
 ( #15309, #15846, #75257, #83627, #6923, #110493 ),
 ( #14770, #67969, #41080, #212, #8573, #76905 ),
 ( #92037, #67415, #23717, #99866, #84180, #92575 ),
 ( #57903, #33773, #49502, #7479, #50595, #109406 ),
 ( #48956, #32682, #109947, #65749, #41640, #75796 ),
 ( #83087, #24801, #93133, #76344, #40528, #32132 ),
 ( #91490, #16401, #23165, #24267, #84727, #66862 ),
 ( #42743, #42192, #100971, #6380, #108835, #74704 ),
 ( #102077, #25360, #59552, #93666, #51147, #66317 ),
 ( #100435, #26476, #104303, #60671, #756, #61240 ),
 ( #62334, #68515, #70197, #43305, #53939, #25914 ),
 ( #9681, #103174, #9142, #45533, #10804, #102614 ),
 ( #19163, #94798, #43849, #77454, #87515, #86945 ),
 ( #88074, #34337, #34884, #18614, #44413, #94230 ),
 ( #60112, #10237, #79672, #103752, #78554, #18073 ),
 ( #11361, #1871, #35442, #17504, #69073, #51703 ),
 ( #69630, #44974, #2430, #77996, #19739, #27594 ),
 ( #52268, #86392, #61778, #1302, #27054, #95354 ),
 ( #96459, #85843, #95902, #52814, #36004, #53369 ),
 ( #79122, #36546, #70743, #104855, #28144, #47708 ),
 ( #63440, #89153, #21910, #105972, #56106, #98092 ),
 ( #38193, #72914, #20831, #107053, #88621, #29249 ),
 ( #21365, #38737, #73469, #54485, #81289, #107603 ),
 ( #13520, #80760, #14079, #12441, #3525, #81837 ),
 ( #56662, #22461, #62908, #2977, #11901, #30338 ),
 ( #90797, #72375, #46076, #105411, #55573, #98643 ),
 ( #97557, #63982, #46626, #55026, #4068, #5141 ),
 ( #97019, #39297, #106504, #48268, #37096, #71297 ),
 ( #29793, #4603, #71855, #28703, #89697, #12978 ),
 ( #80207, #47161, #64529, #20280, #90238, #30886 ),
 ( #65066, #99182, #37650, #57229, #93537, #58862 ),
 ( #16268, #67277, #108703, #57778, #14639, #24661 ),
 ( #84046, #101934, #82413, #82948, #66729, #92434 ),
 ( #48824, #74014, #24122, #16808, #40945, #15710 ),
 ( #6240, #25221, #58312, #83488, #65622, #40390 ),
 ( #49359, #74567, #59425, #50470, #92992, #49912 ),
 ( #110351, #108149, #109270, #67822, #7345, #41508 ),
 ( #75122, #109810, #75667, #31995, #5706, #100303 ),
 ( #100833, #66183, #23587, #33090, #84594, #7885 ),
 ( #76206, #31438, #32554, #101371, #91896, #39852 ),
 ( #99735, #6783, #23027, #42055, #91359, #33628 ),
 ( #15173, #69487, #86806, #10665, #102488, #18473 ),
 ( #103036, #61630, #17923, #62189, #60529, #51561 ) ),
 .UNSPECIFIED., .F., .F., .F.,
 ( 6, 3, 3, 3, 3, 3, 3, 3, 3, 3, 3, 3, 3, 3, 3, 6 ),
 ( 6, 6 ),
 ( 51.34180956679009711, 70.71758386339999447, 85.59913247730000307, 120.0240483330000103, 152.6368677490000039, 161.9753697619999855, 171.3110621919999801, 176.9610724089999962, 178.9129053279999937, 179.8972017420000213, 180.8814981559999922, 181.2916321369999935, 181.4966991269999994, 181.7017661169999769, 181.8155171619999919, 182.0375288639999951 ),
 ( 0.000000000000000000, 0.5002064398120489308 ),
 .UNSPECIFIED. ) ;
#52423 = ORIENTED_EDGE ( 'NONE', *, *, #100930, .F. ) ;
#52424 = CARTESIAN_POINT ( 'NONE',  ( -70.04184978290001595, 1375.054395627170152, 279.7464857826589650 ) ) ;
#52425 = CARTESIAN_POINT ( 'NONE',  ( 12.16691165299999966, 1415.934222462230082, 223.3923867161979899 ) ) ;
#52426 = CARTESIAN_POINT ( 'NONE',  ( -4.039897316195000698, 1516.787536375099990, 204.1233307748069876 ) ) ;
#52427 = ADVANCED_FACE ( 'NONE', ( #7173 ), #29769, .T. ) ;
#52428 = CARTESIAN_POINT ( 'NONE',  ( -28.82219086300000299, 1509.870558443830078, 205.6292521904379953 ) ) ;
#52429 = EDGE_CURVE ( 'NONE', #108583, #101705, #91469, .T. ) ;
#52430 = CARTESIAN_POINT ( 'NONE',  ( -85.86509717699999555, 1384.940999761789953, 289.6770174195589789 ) ) ;
#52431 = CARTESIAN_POINT ( 'NONE',  ( -50.04736368845490091, 1384.619862122030099, 225.3512856688030297 ) ) ;
#52432 = CARTESIAN_POINT ( 'NONE',  ( 9.698064461892839105, 1462.705242386489999, 208.0596150282290182 ) ) ;
#52433 = CARTESIAN_POINT ( 'NONE',  ( -10.73514660131351839, 1424.973046421745494, 139.1354236205272343 ) ) ;
#52435 = ORIENTED_EDGE ( 'NONE', *, *, #56465, .F. ) ;
#52434 = CARTESIAN_POINT ( 'NONE',  ( -11.97780009940000134, 1446.811541358570139, 187.5041657661979855 ) ) ;
#52436 = CARTESIAN_POINT ( 'NONE',  ( 10.57993308616552319, 1425.618513008048012, 196.6680084146474599 ) ) ;
#52437 = CARTESIAN_POINT ( 'NONE',  ( 28.07142279780000038, 1508.133443489229876, 210.4694181319080144 ) ) ;
#52438 = LINE ( 'NONE', #24981, #9116 ) ;
#52439 = CARTESIAN_POINT ( 'NONE',  ( -24.25923418980000079, 1435.344651399380155, 136.2870029874980276 ) ) ;
#52440 = B_SPLINE_CURVE_WITH_KNOTS ( 'NONE', 3,
 ( #6483, #5938, #74807, #40635, #5383, #99421, #49606, #100535, #40084, #99977, #23270, #91592, #92142, #15415, #7035, #41193, #14867, #23815, #83738, #109503, #32779, #58556, #92684, #47398, #60780, #59660, #60212, #94330, #75896, #8125, #41737, #864, #34989, #50693, #8671, #94904, #51244, #17608, #18179, #7582, #102186, #9251, #51809, #42291, #85950 ),
 .UNSPECIFIED., .F., .F.,
 ( 4, 2, 2, 2, 2, 2, 2, 2, 2, 2, 1, 1, 1, 2, 2, 1, 1, 1, 1, 2, 2, 1, 1, 2, 2, 2, 4 ),
 ( 0.000000000000000000, 0.06249999999996011524, 0.09374999999994189370, 0.1093749999999354128, 0.1249999999999289457, 0.1874999999999078792, 0.2187499999999010236, 0.2343749999998975542, 0.2499999999998940847, 0.3749999999998194777, 0.4374999999997830624, 0.4687499999997576938, 0.4843749999997514211, 0.4921874999997538080, 0.4999999999997561950, 0.6249999999998158140, 0.6874999999998389066, 0.7187499999998422373, 0.7343749999998510081, 0.7421874999998467892, 0.7499999999998425704, 0.8124999999998735456, 0.8437499999998785416, 0.8593749999998905320, 0.8749999999999025224, 0.9374999999999512612, 1.000000000000000000 ),
 .UNSPECIFIED. ) ;
#52441 = CARTESIAN_POINT ( 'NONE',  ( 3.461995158685000185, 1516.906233342200039, 211.9877574868770012 ) ) ;
#52442 = CARTESIAN_POINT ( 'NONE',  ( -68.37764721770000165, 1379.747183406850127, 279.2177063942590394 ) ) ;
#52443 = EDGE_CURVE ( 'NONE', #42578, #47608, #101204, .T. ) ;
#52444 = CARTESIAN_POINT ( 'NONE',  ( -14.37531793339999986, 1420.438789880430022, 227.2666485765979871 ) ) ;
#52445 = CARTESIAN_POINT ( 'NONE',  ( 16.33719110018399689, 1478.134947818610044, 222.4389267383260176 ) ) ;
#52446 = CARTESIAN_POINT ( 'NONE',  ( -21.26809175218030035, 1485.919042415889862, 201.7808329802730327 ) ) ;
#52447 = CARTESIAN_POINT ( 'NONE',  ( -1.717139122245000094, 1516.949031626070109, 208.0040058453670042 ) ) ;
#52448 = ORIENTED_EDGE ( 'NONE', *, *, #3914, .T. ) ;
#52449 = CARTESIAN_POINT ( 'NONE',  ( -4.220676207128734703, 1446.230049502166139, 170.5366217123670083 ) ) ;
#52450 = CARTESIAN_POINT ( 'NONE',  ( -0.8368026584929999512, 1412.845967393029923, 233.2028161353979954 ) ) ;
#52451 = CARTESIAN_POINT ( 'NONE',  ( -25.93734973360000140, 1384.843007074499837, 224.2459728783589981 ) ) ;
#52452 = VERTEX_POINT ( 'NONE', #82774 ) ;
#52453 = CARTESIAN_POINT ( 'NONE',  ( -11.00028806098080025, 1385.308172297210149, 218.8195870429669867 ) ) ;
#52454 = CARTESIAN_POINT ( 'NONE',  ( -3.586492549349999948, 1428.590318077689972, 200.4729775719390261 ) ) ;
#52455 = CARTESIAN_POINT ( 'NONE',  ( 12.63018941866619826, 1435.203127805050144, 150.6492594472580038 ) ) ;
#52456 = CARTESIAN_POINT ( 'NONE',  ( 18.29787016638390185, 1469.011283450069868, 228.3214042137699948 ) ) ;
#52457 = CARTESIAN_POINT ( 'NONE',  ( -23.29055829209999828, 1509.739042671430070, 227.3452689062980028 ) ) ;
#52458 = CARTESIAN_POINT ( 'NONE',  ( 0.000000000000000000, 1405.413060387330006, 209.1218459616979999 ) ) ;
#52459 = FACE_OUTER_BOUND ( 'NONE', #12578, .T. ) ;
#52460 = CARTESIAN_POINT ( 'NONE',  ( 9.694557698560979375, 1462.254025613590102, 208.2085395587480150 ) ) ;
#52462 = CARTESIAN_POINT ( 'NONE',  ( 10.53169424880000093, 1481.128073908389979, 211.0447647956590060 ) ) ;
#52461 = CARTESIAN_POINT ( 'NONE',  ( 7.331812085974999782, 1516.906641539930206, 215.6759973964769870 ) ) ;
#52463 = CARTESIAN_POINT ( 'NONE',  ( -8.885472218384601106, 1385.297170050430168, 218.6625727627470042 ) ) ;
#52464 = CARTESIAN_POINT ( 'NONE',  ( -4.616899872884999922, 1517.050041317280147, 216.8443827349270236 ) ) ;
#52465 = ORIENTED_EDGE ( 'NONE', *, *, #20517, .F. ) ;
#52466 = CARTESIAN_POINT ( 'NONE',  ( -12.77667375843740061, 1416.535698381769862, 196.1064608229909823 ) ) ;
#52467 = EDGE_CURVE ( 'NONE', #8321, #3400, #2432, .T. ) ;
#52468 = CYLINDRICAL_SURFACE ( 'NONE', #64212, 2.000000000000003553 ) ;
#52469 = ORIENTED_EDGE ( 'NONE', *, *, #93178, .F. ) ;
#52470 = DIRECTION ( 'NONE',  ( -0.6736849260863837507, 0.000000000000000000, 0.7390186874254154326 ) ) ;
#52471 = CARTESIAN_POINT ( 'NONE',  ( -12.85215753329999977, 1508.300510831589918, 209.4336657455189936 ) ) ;
#52472 = EDGE_CURVE ( 'NONE', #38412, #91781, #27135, .T. ) ;
#52473 = DIRECTION ( 'NONE',  ( -5.980589973904019347E-17, 1.000000000000000000, -1.736889445713099699E-16 ) ) ;
#52474 = CARTESIAN_POINT ( 'NONE',  ( 3.346707516019999940, 1443.005054410889898, 217.3642451189890323 ) ) ;
#52475 = CARTESIAN_POINT ( 'NONE',  ( -29.30029655192939586, 1525.907212628473872, 196.8717316207790589 ) ) ;
#52476 = DIRECTION ( 'NONE',  ( -0.9999176245050241940, -0.003057966218349585878, 0.01246567474455440375 ) ) ;
#52477 = LINE ( 'NONE', #51917, #102170 ) ;
#52478 = CARTESIAN_POINT ( 'NONE',  ( -18.44401098650000037, 1424.710439251030039, 225.1596812334979916 ) ) ;
#52479 = CARTESIAN_POINT ( 'NONE',  ( -7.317283160083440485, 1458.197890023347327, 215.2731315594757007 ) ) ;
#52480 = CARTESIAN_POINT ( 'NONE',  ( -9.821550493440000196, 1443.913060387330006, 148.8455630174979945 ) ) ;
#52481 = CARTESIAN_POINT ( 'NONE',  ( 16.49692068119999888, 1410.833576258530002, 191.6204761995979879 ) ) ;
#52483 = CARTESIAN_POINT ( 'NONE',  ( 8.062587302181759341, 1436.235894220949831, 206.1282943059349861 ) ) ;
#52482 = CARTESIAN_POINT ( 'NONE',  ( -14.33183065600080042, 1418.593864405419936, 201.2805417143829914 ) ) ;
#52484 = CARTESIAN_POINT ( 'NONE',  ( 5.775165528996293318, 1509.036904579127395, 201.6091405375480008 ) ) ;
#52485 = ORIENTED_EDGE ( 'NONE', *, *, #32935, .T. ) ;
#52486 = CARTESIAN_POINT ( 'NONE',  ( 1.421471772691550006, 1507.619497824060090, 186.1880827579659865 ) ) ;
#52487 = CARTESIAN_POINT ( 'NONE',  ( 23.63745125559999849, 1430.455784058630115, 206.9473789965179833 ) ) ;
#52488 = CARTESIAN_POINT ( 'NONE',  ( -24.60733038660000105, 1437.330089494700132, 210.5677010675179872 ) ) ;
#52489 = CARTESIAN_POINT ( 'NONE',  ( 6.366883779533799803, 1410.509502214471695, 186.8986137100159794 ) ) ;
#52490 = CARTESIAN_POINT ( 'NONE',  ( 0.4403324358131759930, 1517.051704035390003, 201.6347831756999938 ) ) ;
#52491 = CARTESIAN_POINT ( 'NONE',  ( 6.501609782144661231, 1517.151704408390060, 217.4228972380528262 ) ) ;
#52492 = CARTESIAN_POINT ( 'NONE',  ( -7.983219840484640173, 1511.369014876942174, 214.5214371862444693 ) ) ;
#52493 = CARTESIAN_POINT ( 'NONE',  ( -1.748695796902800081, 1488.269352622320184, 219.8525110836319811 ) ) ;
#52494 = CARTESIAN_POINT ( 'NONE',  ( 13.13054719219040045, 1414.913526854310021, 198.0719216339290085 ) ) ;
#52495 = CARTESIAN_POINT ( 'NONE',  ( -81.92975575952578993, 1383.775620875610002, 304.8532181189869448 ) ) ;
#52496 = CARTESIAN_POINT ( 'NONE',  ( -107.9702631612849046, 1378.913060387289988, 299.5275268628465710 ) ) ;
#52497 = CARTESIAN_POINT ( 'NONE',  ( 6.232532001850000114, 1398.098440471829917, 220.5304192662980256 ) ) ;
#52498 = CARTESIAN_POINT ( 'NONE',  ( -23.17538855434040101, 1409.994298099240268, 210.0642958403453235 ) ) ;
#52500 = ORIENTED_EDGE ( 'NONE', *, *, #15071, .T. ) ;
#52499 = CARTESIAN_POINT ( 'NONE',  ( 10.40969047044820073, 1451.775060363849889, 207.5610707736619815 ) ) ;
#52501 = CARTESIAN_POINT ( 'NONE',  ( -18.04763499721657993, 1459.633086045522305, 228.0005121999546986 ) ) ;
#52502 = CARTESIAN_POINT ( 'NONE',  ( -87.83602971100000900, 1380.693317143970035, 294.3638560435589966 ) ) ;
#52503 = CARTESIAN_POINT ( 'NONE',  ( 20.36394027541210150, 1509.531394767829852, 230.2454094804139970 ) ) ;
#52504 = VERTEX_POINT ( 'NONE', #25604 ) ;
#52505 = ORIENTED_EDGE ( 'NONE', *, *, #63780, .F. ) ;
#52506 = CARTESIAN_POINT ( 'NONE',  ( 14.26589412800000112, 1443.159997941379970, 189.6457918547979773 ) ) ;
#52507 = CARTESIAN_POINT ( 'NONE',  ( -18.10740131676499942, 1463.999236119600255, 217.9813976188680158 ) ) ;
#52508 = CARTESIAN_POINT ( 'NONE',  ( 39.80925673091419981, 1441.186665741440038, 136.8465300712809949 ) ) ;
#52510 = CARTESIAN_POINT ( 'NONE',  ( -44.59183195640000008, 1449.238671483380131, 266.2372565378979630 ) ) ;
#52509 = CARTESIAN_POINT ( 'NONE',  ( 15.61002862346814268, 1412.588789359010207, 269.3672926532146334 ) ) ;
#52511 = CARTESIAN_POINT ( 'NONE',  ( 8.658448668542680693, 1437.810433862630134, 209.6180638252519941 ) ) ;
#52512 = CARTESIAN_POINT ( 'NONE',  ( -108.4220066540000005, 1383.250329722910010, 297.4825366361590113 ) ) ;
#52513 = CARTESIAN_POINT ( 'NONE',  ( -116.0327476856695341, 1306.913060387289988, 302.7835693414472189 ) ) ;
#52514 = CARTESIAN_POINT ( 'NONE',  ( -20.04281941989999893, 1485.210412383429912, 191.3717997072980097 ) ) ;
#52515 = CARTESIAN_POINT ( 'NONE',  ( 1.811394514909999920, 1409.481637553129985, 185.5992571243980080 ) ) ;
#52516 = CARTESIAN_POINT ( 'NONE',  ( 5.031185190540000463, 1423.053909769329948, 184.8938659814980099 ) ) ;
#52517 = CARTESIAN_POINT ( 'NONE',  ( -9.894253967190000054, 1435.855537208829901, 152.5794184983980131 ) ) ;
#52518 = CARTESIAN_POINT ( 'NONE',  ( -2.500000000000000000, 1440.913060387330006, 137.0999999980979851 ) ) ;
#52519 = CARTESIAN_POINT ( 'NONE',  ( -10.73901725096249926, 1423.590975015609956, 204.3534390747859959 ) ) ;
#52520 = CARTESIAN_POINT ( 'NONE',  ( -3.105266140399999930, 1452.658929098130102, 153.4127541622980004 ) ) ;
#52521 = DIRECTION ( 'NONE',  ( 0.4978433412588638141, 0.000000000000000000, -0.8672669759446687276 ) ) ;
#52522 = VERTEX_POINT ( 'NONE', #11043 ) ;
#52523 = CYLINDRICAL_SURFACE ( 'NONE', #30090, 2.000000000000003553 ) ;
#52524 = CARTESIAN_POINT ( 'NONE',  ( 18.33936911297750072, 1473.566272301189883, 194.9299536566859956 ) ) ;
#52525 = CARTESIAN_POINT ( 'NONE',  ( -41.37369176849999519, 1449.696618274529783, 270.1889136745979840 ) ) ;
#52526 = DIRECTION ( 'NONE',  ( -1.076084536626781954E-17, -1.000000000000000000, -4.313860721084074369E-17 ) ) ;
#52527 = FACE_OUTER_BOUND ( 'NONE', #31270, .T. ) ;
#52528 = CARTESIAN_POINT ( 'NONE',  ( 11.81780673814840021, 1517.151704408390060, 195.5270144474869767 ) ) ;
#52529 = FACE_OUTER_BOUND ( 'NONE', #56396, .T. ) ;
#52530 = CARTESIAN_POINT ( 'NONE',  ( 2.882600136576499938, 1409.337436188870015, 231.1024624802110168 ) ) ;
#52531 = CARTESIAN_POINT ( 'NONE',  ( -28.27139721233033143, 1526.382868172863937, 219.5606225550389752 ) ) ;
#52532 = CARTESIAN_POINT ( 'NONE',  ( -4.504634474840000458, 1417.895784275830010, 234.4460694219980041 ) ) ;
#52533 = DIRECTION ( 'NONE',  ( -0.7074300732359156685, -0.02470400251506888953, -0.7063514732349346348 ) ) ;
#52534 = CARTESIAN_POINT ( 'NONE',  ( -8.006252579206014630, 1359.935925956307983, 209.6218459617033432 ) ) ;
#52535 = CARTESIAN_POINT ( 'NONE',  ( -45.66135036215970189, 1437.717918248189790, 268.7621968117340430 ) ) ;
#52536 = CARTESIAN_POINT ( 'NONE',  ( -2.500000000000000000, 1434.141256042250006, 183.7754221751980026 ) ) ;
#52537 = ORIENTED_EDGE ( 'NONE', *, *, #84884, .T. ) ;
#52538 = CARTESIAN_POINT ( 'NONE',  ( -8.087399829960000730, 1423.889215342339867, 210.5428868746689943 ) ) ;
#52539 = CIRCLE ( 'NONE', #109743, 0.9999999999999952260 ) ;
#52540 = ORIENTED_EDGE ( 'NONE', *, *, #16548, .T. ) ;
#52541 = CARTESIAN_POINT ( 'NONE',  ( 1.135898785685000023, 1516.958737650239982, 210.2414381519470226 ) ) ;
#52542 = CARTESIAN_POINT ( 'NONE',  ( -113.4000000000000057, 1378.913060387289988, 304.2218459572590064 ) ) ;
#52543 = CARTESIAN_POINT ( 'NONE',  ( 19.29437764624872642, 1456.521983837815696, 224.7265922325017300 ) ) ;
#52544 = CARTESIAN_POINT ( 'NONE',  ( 7.506693744642929822, 1425.950106240180048, 212.2988314193449924 ) ) ;
#52545 = AXIS2_PLACEMENT_3D ( 'NONE', #37696, #3024, #89747 ) ;
#52546 = CARTESIAN_POINT ( 'NONE',  ( -1.933463630428559954, 1496.738328175310016, 221.3394013225409935 ) ) ;
#52547 = B_SPLINE_SURFACE_WITH_KNOTS ( 'NONE', 5, 5, ( 
 ( #79308, #80408, #3721, #18266, #96659, #87717 ),
 ( #28900, #54677, #94998, #2619, #36745, #88255 ),
 ( #54128, #27789, #70938, #3171, #105054, #37853 ),
 ( #45724, #88803, #103942, #1500, #28343, #79861 ),
 ( #61421, #95544, #35631, #12086, #62539, #69824 ),
 ( #44608, #20466, #37303, #72038, #44049, #27240 ) ),
 .UNSPECIFIED., .F., .F., .F.,
 ( 6, 6 ),
 ( 6, 6 ),
 ( 4.505366048469999996, 5.371483694130000153 ),
 ( 0.000000000000000000, 1.435063413269999977 ),
 .UNSPECIFIED. ) ;
#52548 = VERTEX_POINT ( 'NONE', #79351 ) ;
#52549 = CARTESIAN_POINT ( 'NONE',  ( -15.64624339300000067, 1506.809279316930088, 193.6024923478979929 ) ) ;
#52551 = CARTESIAN_POINT ( 'NONE',  ( -14.81793325873010048, 1514.080593477700177, 224.0430682687909894 ) ) ;
#52550 = DIRECTION ( 'NONE',  ( -0.02616798426500960631, -0.9993150019883682011, 0.02616798426500970345 ) ) ;
#52552 = CARTESIAN_POINT ( 'NONE',  ( 11.60004869885203682, 1422.222932908421853, 135.5999999980979851 ) ) ;
#52553 = CARTESIAN_POINT ( 'NONE',  ( -18.38283541797299847, 1508.551704415689983, 210.6369374182840204 ) ) ;
#52554 = CARTESIAN_POINT ( 'NONE',  ( 0.6364662242309990781, 1454.894301978690009, 215.7249498071190033 ) ) ;
#52555 = CARTESIAN_POINT ( 'NONE',  ( -8.245270369270169653, 1438.570843674859816, 206.3270951701919955 ) ) ;
#52556 = EDGE_LOOP ( 'NONE', ( #17791, #69781 ) ) ;
#52557 = CARTESIAN_POINT ( 'NONE',  ( -0.5972104939277330660, 1409.781079465039966, 270.0713840979290126 ) ) ;
#52558 = CARTESIAN_POINT ( 'NONE',  ( -7.727327152855000492, 1517.232977404109988, 207.4118332116069894 ) ) ;
#52559 = AXIS2_PLACEMENT_3D ( 'NONE', #100594, #40700, #23875 ) ;
#52560 = CARTESIAN_POINT ( 'NONE',  ( 7.944617962720000648, 1417.384938173330056, 230.8476712041980079 ) ) ;
#52561 = CARTESIAN_POINT ( 'NONE',  ( -0.2669961437037675078, 1507.379266396976391, 237.3398728226291894 ) ) ;
#52563 = ORIENTED_EDGE ( 'NONE', *, *, #61205, .F. ) ;
#52562 = CARTESIAN_POINT ( 'NONE',  ( -6.915728699340433216, 1366.855454596503250, 210.6218459617142003 ) ) ;
#52564 = ORIENTED_EDGE ( 'NONE', *, *, #29192, .T. ) ;
#52565 = CARTESIAN_POINT ( 'NONE',  ( -23.44004119578789869, 1410.414350826220016, 210.3440813114680168 ) ) ;
#52566 = CARTESIAN_POINT ( 'NONE',  ( -4.031755536680000418, 1424.742300799430041, 185.9020548737979937 ) ) ;
#52567 = CARTESIAN_POINT ( 'NONE',  ( 3.648661080172654891, 1424.949000758327884, 184.9096943055786255 ) ) ;
#52568 = DIRECTION ( 'NONE',  ( 0.000000000000000000, -1.000000000000000000, 0.000000000000000000 ) ) ;
#52569 = CARTESIAN_POINT ( 'NONE',  ( -20.23041878443079966, 1482.171314072119912, 192.9891252425980213 ) ) ;
#52570 = CARTESIAN_POINT ( 'NONE',  ( -20.07551605200000111, 1420.830474780429995, 221.7733367695979894 ) ) ;
#52571 = ADVANCED_FACE ( 'NONE', ( #36791 ), #76031, .F. ) ;
#52572 = CARTESIAN_POINT ( 'NONE',  ( 39.35319033365500019, 1459.582669346870034, 267.8286354669800176 ) ) ;
#52573 = CARTESIAN_POINT ( 'NONE',  ( -8.779614049866278691, 1465.164895044473724, 232.9239790886660160 ) ) ;
#52574 = CARTESIAN_POINT ( 'NONE',  ( -16.62457289494420110, 1421.497728909477473, 226.9554053466772814 ) ) ;
#52575 = CARTESIAN_POINT ( 'NONE',  ( -2.298048961635000165, 1516.764084769670262, 205.6764383981169715 ) ) ;
#52576 = ORIENTED_EDGE ( 'NONE', *, *, #94421, .F. ) ;
#52577 = CARTESIAN_POINT ( 'NONE',  ( 2.035102182640000201, 1443.701500078689833, 215.0273390923990178 ) ) ;
#52579 = B_SPLINE_CURVE_WITH_KNOTS ( 'NONE', 3,
 ( #44701, #104587, #78850, #70466 ),
 .UNSPECIFIED., .F., .F.,
 ( 4, 4 ),
 ( 0.000000000000000000, 0.0002960034161023844057 ),
 .UNSPECIFIED. ) ;
#52578 = CARTESIAN_POINT ( 'NONE',  ( 1.476609825382830143, 1480.675250368899924, 182.2662939368339892 ) ) ;
#52580 = CARTESIAN_POINT ( 'NONE',  ( 23.86968260200000103, 1411.113062188429922, 208.1586362411949835 ) ) ;
#52581 = ORIENTED_EDGE ( 'NONE', *, *, #83652, .F. ) ;
#52582 = CARTESIAN_POINT ( 'NONE',  ( 4.487359741654660006, 1509.034536824670113, 206.0057093087000055 ) ) ;
#52584 = EDGE_CURVE ( 'NONE', #6013, #62471, #110666, .T. ) ;
#52583 = CARTESIAN_POINT ( 'NONE',  ( 26.27737804779999919, 1451.834422488929931, 135.7154755371979888 ) ) ;
#52585 = DIRECTION ( 'NONE',  ( 0.000000000000000000, 1.000000000000000000, 0.000000000000000000 ) ) ;
#52586 = CARTESIAN_POINT ( 'NONE',  ( -5.964141498479999193, 1386.998390782689967, 218.2806129090890011 ) ) ;
#52587 = CARTESIAN_POINT ( 'NONE',  ( 6.616506887542479731, 1517.051706634660150, 212.8496527657779893 ) ) ;
#52588 = CARTESIAN_POINT ( 'NONE',  ( 17.09517797430000030, 1409.510037156830094, 194.7435863138979926 ) ) ;
#52589 = B_SPLINE_CURVE_WITH_KNOTS ( 'NONE', 3,
 ( #13351, #48094, #63806, #90627, #14466, #97922 ),
 .UNSPECIFIED., .F., .F.,
 ( 4, 2, 4 ),
 ( 0.000000000000000000, 0.5000000000000000000, 1.000000000000000000 ),
 .UNSPECIFIED. ) ;
#52590 = CARTESIAN_POINT ( 'NONE',  ( 18.64337105059429689, 1444.324653571830140, 162.1710875046050830 ) ) ;
#52591 = CARTESIAN_POINT ( 'NONE',  ( 2.499999945294461678, 1439.622149924839277, 182.9152359685302827 ) ) ;
#52593 = CARTESIAN_POINT ( 'NONE',  ( -19.70148083128903238, 1425.942341657287670, 223.0221936444421829 ) ) ;
#52592 = CARTESIAN_POINT ( 'NONE',  ( 0.3620268206439999914, 1416.991477563229864, 234.1672957265980131 ) ) ;
#52594 = CARTESIAN_POINT ( 'NONE',  ( 1.228127824989470041, 1450.757128850169920, 181.5372027678210145 ) ) ;
#52595 = CARTESIAN_POINT ( 'NONE',  ( -9.622416126109998302, 1382.582223343250007, 217.9576506642389973 ) ) ;
#52596 = CARTESIAN_POINT ( 'NONE',  ( 7.722536764694999611, 1517.050041317280147, 213.7387458049869906 ) ) ;
#52597 = CARTESIAN_POINT ( 'NONE',  ( 3.043251597425320032, 1417.779699503100119, 234.3208248802520188 ) ) ;
#52598 = ORIENTED_EDGE ( 'NONE', *, *, #77429, .T. ) ;
#52599 = CARTESIAN_POINT ( 'NONE',  ( -8.956927351110008928, 1464.257504697786317, 226.7719248702087498 ) ) ;
#52600 = DIRECTION ( 'NONE',  ( 0.000000000000000000, 0.000000000000000000, 1.000000000000000000 ) ) ;
#52601 = CARTESIAN_POINT ( 'NONE',  ( -0.5149987733311249816, 1410.090151802530045, 233.1456135000190102 ) ) ;
#52602 = CARTESIAN_POINT ( 'NONE',  ( -19.63485294834822525, 1508.289801357211218, 209.7406608497707339 ) ) ;
#52603 = CARTESIAN_POINT ( 'NONE',  ( 0.7340478531541532181, 1421.248697517114806, 193.7332822046788010 ) ) ;
#52604 = CARTESIAN_POINT ( 'NONE',  ( -0.09512347170599190493, 1506.606278694979437, 231.2494356483143747 ) ) ;
#52605 = CARTESIAN_POINT ( 'NONE',  ( -5.969073325650000150, 1453.512197679029896, 209.1218459616979999 ) ) ;
#52606 = CARTESIAN_POINT ( 'NONE',  ( -28.44698416550318498, 1526.373507135059299, 198.3684985826631930 ) ) ;
#52607 = CARTESIAN_POINT ( 'NONE',  ( 11.12882730979999835, 1433.637661252139878, 151.6637046936980084 ) ) ;
#52608 = CARTESIAN_POINT ( 'NONE',  ( 24.08292308420000083, 1450.076351702270131, 243.9198229606980135 ) ) ;
#52609 = CARTESIAN_POINT ( 'NONE',  ( 24.89297638757900089, 1440.913060396979972, 215.3507704242990144 ) ) ;
#52610 = CARTESIAN_POINT ( 'NONE',  ( -14.54141060630000126, 1422.922756957550064, 196.4113455912990105 ) ) ;
#52611 = CARTESIAN_POINT ( 'NONE',  ( 11.55003007508270052, 1421.422333198520164, 201.8131330578860059 ) ) ;
#52612 = CIRCLE ( 'NONE', #68770, 2.500000000000002220 ) ;
#52613 = CARTESIAN_POINT ( 'NONE',  ( 24.32116265780000219, 1435.530952642309785, 137.6072328918980077 ) ) ;
#52614 = CARTESIAN_POINT ( 'NONE',  ( 22.71503220009999779, 1409.706269051729805, 209.0936436305159987 ) ) ;
#52615 = CARTESIAN_POINT ( 'NONE',  ( 33.28034951413933129, 1522.382868172863937, 217.4407153818819722 ) ) ;
#52616 = FACE_OUTER_BOUND ( 'NONE', #98286, .T. ) ;
#52617 = CARTESIAN_POINT ( 'NONE',  ( 25.75587219230000002, 1449.806259868670168, 209.4579355261629985 ) ) ;
#52618 = CIRCLE ( 'NONE', #75872, 2.500000000000002220 ) ;
#52619 = CARTESIAN_POINT ( 'NONE',  ( -16.96799521795757215, 1419.980406830895845, 207.7863820104928152 ) ) ;
#52620 = CARTESIAN_POINT ( 'NONE',  ( 26.63291560383849799, 1436.743680851771842, 136.7889385594793055 ) ) ;
#52621 = CARTESIAN_POINT ( 'NONE',  ( -10.57073115472060110, 1383.862563487480202, 218.6316618481800162 ) ) ;
#52622 = CARTESIAN_POINT ( 'NONE',  ( 10.99043261664119875, 1479.494642963729802, 229.8297439004759894 ) ) ;
#52623 = CARTESIAN_POINT ( 'NONE',  ( -7.323034312095000331, 1516.609912606490070, 212.5765947784269940 ) ) ;
#52624 = CARTESIAN_POINT ( 'NONE',  ( 1.984413551915469975, 1517.151704408390060, 198.9129232538419956 ) ) ;
#52625 = CARTESIAN_POINT ( 'NONE',  ( 0.1595995995380000143, 1486.508831850330125, 181.8147405652979671 ) ) ;
#52627 = ORIENTED_EDGE ( 'NONE', *, *, #53214, .T. ) ;
#52626 = CARTESIAN_POINT ( 'NONE',  ( 3.718743811529999999, 1442.790811878290242, 217.1968316306989948 ) ) ;
#52628 = CARTESIAN_POINT ( 'NONE',  ( 20.49599333844834348, 1525.960063244517187, 184.3798832129035077 ) ) ;
#52629 = CARTESIAN_POINT ( 'NONE',  ( -9.839360847350000938, 1382.942182113030185, 200.0986700951989974 ) ) ;
#52630 = CARTESIAN_POINT ( 'NONE',  ( -4.692099526989998992, 1474.463958302690116, 198.6947328130989945 ) ) ;
#52632 = ORIENTED_EDGE ( 'NONE', *, *, #55715, .T. ) ;
#52631 = CARTESIAN_POINT ( 'NONE',  ( -38.20286890324609885, 1450.309401038109854, 134.0999999984079807 ) ) ;
#52633 = CARTESIAN_POINT ( 'NONE',  ( -2.140641997699999965, 1508.551704408389924, 220.0635241299990241 ) ) ;
#52634 = ORIENTED_EDGE ( 'NONE', *, *, #22156, .F. ) ;
#52635 = B_SPLINE_SURFACE_WITH_KNOTS ( 'NONE', 5, 5, ( 
 ( #1772, #70093, #86850, #95257, #70640, #96918 ),
 ( #86298, #104206, #10143, #68980, #87978, #96359 ),
 ( #19637, #36442, #44879, #18518, #52716, #26382 ),
 ( #11266, #20185, #103082, #44316, #79030, #54383 ),
 ( #88516, #104756, #78460, #11800, #79572, #2874 ),
 ( #45968, #28043, #80103, #77905, #12890, #3975 ),
 ( #56014, #29152, #81735, #63877, #98546, #13421 ),
 ( #20726, #30236, #14537, #38099, #108047, #57130 ),
 ( #47611, #48726, #80660, #63338, #89049, #81192 ) ),
 .UNSPECIFIED., .F., .F., .F.,
 ( 6, 3, 6 ),
 ( 6, 6 ),
 ( -0.01213293170383570110, 5.564709931820000399, 10.43218467589399978 ),
 ( -0.01218607079403309992, 1.000000000000000000 ),
 .UNSPECIFIED. ) ;
#52636 = CARTESIAN_POINT ( 'NONE',  ( -13.20168566553750011, 1390.473793852909921, 211.6634096005309971 ) ) ;
#52637 = CARTESIAN_POINT ( 'NONE',  ( 7.308426574864255620, 1447.450532783193239, 203.7166947410731268 ) ) ;
#52638 = CARTESIAN_POINT ( 'NONE',  ( -2.683679964788079353, 1509.031199887366938, 238.5977189156948555 ) ) ;
#52639 = CARTESIAN_POINT ( 'NONE',  ( 22.83133757149967380, 1409.745586299351999, 208.5326685875802752 ) ) ;
#52640 = CARTESIAN_POINT ( 'NONE',  ( -2.074854266390000035, 1432.268094214490020, 217.6750424900990026 ) ) ;
#52641 = DIRECTION ( 'NONE',  ( 0.000000000000000000, 1.000000000000000000, 0.000000000000000000 ) ) ;
#52642 = CARTESIAN_POINT ( 'NONE',  ( 14.24559479254840078, 1409.410527519360130, 204.6418239650080011 ) ) ;
#52643 = CARTESIAN_POINT ( 'NONE',  ( 8.970106519850705951, 1421.589190746440181, 137.0999999980978146 ) ) ;
#52644 = CARTESIAN_POINT ( 'NONE',  ( -74.96301731579400496, 1385.136118946299803, 275.4036379574320108 ) ) ;
#52645 = CARTESIAN_POINT ( 'NONE',  ( -17.00560698389999814, 1410.862957975729842, 191.9516635397980053 ) ) ;
#52646 = CARTESIAN_POINT ( 'NONE',  ( -50.59433295680000242, 1379.743302990699931, 241.3342481622590014 ) ) ;
#52647 = ORIENTED_EDGE ( 'NONE', *, *, #8986, .F. ) ;
#52648 = CARTESIAN_POINT ( 'NONE',  ( 11.45381602559669965, 1491.761437294190046, 209.6400631038679876 ) ) ;
#52650 = ORIENTED_EDGE ( 'NONE', *, *, #86530, .F. ) ;
#52649 = CYLINDRICAL_SURFACE ( 'NONE', #39505, 0.4999999999999449329 ) ;
#52651 = CARTESIAN_POINT ( 'NONE',  ( -9.239957267063561019, 1384.847616872940080, 197.9484498896830189 ) ) ;
#52652 = ORIENTED_EDGE ( 'NONE', *, *, #85746, .F. ) ;
#52653 = CARTESIAN_POINT ( 'NONE',  ( 24.68678492890000342, 1508.521768884430230, 220.7077148987980024 ) ) ;
#52654 = CARTESIAN_POINT ( 'NONE',  ( -6.757614358386126341, 1362.669000810187299, 207.6218459616988241 ) ) ;
#52655 = CARTESIAN_POINT ( 'NONE',  ( -6.058024923110000515, 1495.048144898590181, 199.2280266695289868 ) ) ;
#52656 = CARTESIAN_POINT ( 'NONE',  ( 32.06156897976659792, 1460.613316927345750, 269.4940338796959054 ) ) ;
#52657 = CARTESIAN_POINT ( 'NONE',  ( -29.78220350812331674, 1526.382868172863937, 221.7347658002328501 ) ) ;
#52658 = CARTESIAN_POINT ( 'NONE',  ( 19.38237504630382091, 1439.882993612299288, 212.4558745127706914 ) ) ;
#52659 = CARTESIAN_POINT ( 'NONE',  ( 18.64672481363430379, 1416.851343896850040, 209.6839434896919840 ) ) ;
#52660 = CARTESIAN_POINT ( 'NONE',  ( 3.375977075490000257, 1446.395221907989935, 199.5681765173089843 ) ) ;
#52661 = CARTESIAN_POINT ( 'NONE',  ( -20.37004171859861401, 1507.842607393826938, 228.6074707356000602 ) ) ;
#52662 = CARTESIAN_POINT ( 'NONE',  ( -3.763781937369067965, 1369.097489338547803, 210.6218459616991936 ) ) ;
#52663 = CARTESIAN_POINT ( 'NONE',  ( -30.25425994616995240, 1526.382868172863937, 218.9520509131593258 ) ) ;
#52664 = CARTESIAN_POINT ( 'NONE',  ( -16.06782005780000233, 1459.209651374430223, 230.7189234877979800 ) ) ;
#52665 = B_SPLINE_CURVE_WITH_KNOTS ( 'NONE', 3,
 ( #44457, #27643, #27101, #69680, #103802, #86991, #78601, #3027, #19786, #71346 ),
 .UNSPECIFIED., .F., .F.,
 ( 4, 2, 2, 2, 4 ),
 ( 0.000000000000000000, 0.2500000000000107692, 0.3749999999999965028, 0.4999999999999821809, 1.000000000000000000 ),
 .UNSPECIFIED. ) ;
#52666 = CARTESIAN_POINT ( 'NONE',  ( -1.717432486395000124, 1516.836638729160086, 206.8395443540670158 ) ) ;
#52667 = LINE ( 'NONE', #89002, #60812 ) ;
#52668 = B_SPLINE_SURFACE_WITH_KNOTS ( 'NONE', 5, 5, ( 
 ( #87809, #80501, #87239, #29529, #106243, #27323, #95635, #11094, #10528, #12177, #63719, #62064, #36277, #46366, #20558, #54761, #54218, #88891, #11634, #45812, #78851, #53665, #97829, #104588, #69917, #27883, #96191 ),
 ( #37947, #3262, #19465, #45261, #79396, #1591, #2710, #36834, #28993, #71024, #105145, #62634, #3819, #96753, #37388, #72128, #105711, #55309, #89443, #12735, #78279, #22754, #5436, #100584, #13810, #46917, #81574 ),
 ( #5987, #64263, #72655, #40690, #91642, #106782, #21658, #39020, #30073, #14367, #100034, #98387, #99474, #38478, #39593, #31729, #56958, #89987, #73197, #55866, #40135, #107342, #107888, #13260, #74319, #73765, #47450 ),
 ( #4877, #30638, #90534, #47996, #109007, #64824, #56402, #49110, #98932, #32292, #74863, #22206, #82133, #31179, #65368, #14918, #66476, #91085, #48561, #82697, #108449, #57518, #65916, #23866, #23325, #83244, #6538 ),
 ( #58060, #92194, #81038, #4349, #25517, #17661, #59170, #51862, #93289, #110646, #8173, #69219, #75418, #59711, #32827, #109556, #41788, #68671, #8726, #67018, #103329, #85998, #51292, #94380, #110098, #26636, #17099 ),
 ( #26066, #33932, #16552, #35041, #68129, #9297, #43460, #60261, #93824, #77608, #77062, #916, #60832, #85426, #15467, #42905, #49660, #83795, #33373, #371, #16015, #7089, #34496, #75946, #67567, #50742, #41245 ) ),
 .UNSPECIFIED., .F., .F., .F.,
 ( 6, 6 ),
 ( 6, 3, 3, 3, 3, 3, 3, 3, 6 ),
 ( 1.704359124380000035, 76.86370920020000597 ),
 ( 27.73790463739999979, 34.20638505209999636, 36.61973048189999957, 37.82640319669999940, 38.42973955419999754, 39.03307591160000101, 39.44352330040000254, 39.85397068919999697, 40.67486546690000182 ),
 .UNSPECIFIED. ) ;
#52669 = CARTESIAN_POINT ( 'NONE',  ( -30.90487439922522483, 1525.907212628473872, 216.4335774778785151 ) ) ;
#52670 = CARTESIAN_POINT ( 'NONE',  ( 13.58245579929999991, 1416.835809767730098, 196.3346082735980076 ) ) ;
#52672 = ORIENTED_EDGE ( 'NONE', *, *, #48875, .T. ) ;
#52671 = CARTESIAN_POINT ( 'NONE',  ( -3.805396659119999914, 1495.647976226690162, 219.6495707272989932 ) ) ;
#52673 = CARTESIAN_POINT ( 'NONE',  ( -33.91369265678890343, 1437.010538859309918, 136.5611844326260211 ) ) ;
#52674 = ORIENTED_EDGE ( 'NONE', *, *, #4323, .T. ) ;
#52675 = CARTESIAN_POINT ( 'NONE',  ( 9.126915900878477927, 1516.551188146009054, 213.9333071022012120 ) ) ;
#52676 = CARTESIAN_POINT ( 'NONE',  ( -20.10054294789999929, 1449.792076513850134, 195.1552221568979917 ) ) ;
#52678 = CARTESIAN_POINT ( 'NONE',  ( 16.14453601094659874, 1409.476838033949889, 193.1642425871669957 ) ) ;
#52677 = CARTESIAN_POINT ( 'NONE',  ( -11.55021905039999908, 1426.818422250529920, 130.8136715980980114 ) ) ;
#52679 = CARTESIAN_POINT ( 'NONE',  ( -1.118903308544999975, 1517.003078582959688, 212.0031713441969998 ) ) ;
#52680 =( BOUNDED_CURVE ( )  B_SPLINE_CURVE ( 3, ( #104944, #80299, #3066, #11444 ),
 .UNSPECIFIED., .F., .T. ) 
 B_SPLINE_CURVE_WITH_KNOTS ( ( 4, 4 ),
 ( 1.028502516659682176, 2.113090281714570029 ),
 .UNSPECIFIED. ) 
 CURVE ( )  GEOMETRIC_REPRESENTATION_ITEM ( )  RATIONAL_B_SPLINE_CURVE ( ( 1.000000000000000000, 0.9043513721624834023, 0.9043513721624834023, 1.000000000000000000 ) ) 
 REPRESENTATION_ITEM ( '' )  );
#52681 = CARTESIAN_POINT ( 'NONE',  ( -17.84338787571961049, 1523.382868172864164, 180.3600277896300383 ) ) ;
#52682 = CARTESIAN_POINT ( 'NONE',  ( -19.70612301839999958, 1434.996842494430211, 207.5825951959979818 ) ) ;
#52683 = CARTESIAN_POINT ( 'NONE',  ( -34.48978217860000228, 1440.913060385029894, 250.0021841876980488 ) ) ;
#52684 = CARTESIAN_POINT ( 'NONE',  ( -12.40250920638250065, 1378.632933055699823, 209.1856888407239978 ) ) ;
#52685 = LINE ( 'NONE', #59990, #92049 ) ;
#52686 = CARTESIAN_POINT ( 'NONE',  ( -5.177093926210000419, 1391.906305342289897, 214.5223142673890209 ) ) ;
#52687 = B_SPLINE_CURVE_WITH_KNOTS ( 'NONE', 3,
 ( #43438, #16534, #102221, #85407, #94359, #17639, #26614, #35020, #9278, #77589, #896, #60810, #18207, #86527, #43990, #78125, #35571, #61366, #36140, #88748, #10937, #19868, #71439, #63572, #87085, #87650, #28282 ),
 .UNSPECIFIED., .F., .F.,
 ( 4, 2, 2, 2, 1, 1, 1, 1, 1, 2, 2, 2, 2, 2, 2, 4 ),
 ( 0.000000000000000000, 0.2500000000017412183, 0.3750000000026034730, 0.4375000000030318525, 0.4687500000032479575, 0.4843750000033510972, 0.4921875000034075520, 0.4960937500034376946, 0.4980468750034528491, 0.4990234375034622305, 0.5000000000034716674, 0.6250000000026062486, 0.6875000000021718183, 0.7500000000017372770, 0.8750000000008686385, 1.000000000000000000 ),
 .UNSPECIFIED. ) ;
#52688 = CARTESIAN_POINT ( 'NONE',  ( 33.12914038030000086, 1450.467761070830193, 136.2685675544979915 ) ) ;
#52689 = ORIENTED_EDGE ( 'NONE', *, *, #11153, .F. ) ;
#52690 = CARTESIAN_POINT ( 'NONE',  ( 11.13883711037720126, 1398.243429064360271, 216.8406632416929938 ) ) ;
#52691 = CARTESIAN_POINT ( 'NONE',  ( 9.668880095928939156, 1462.163648629059935, 207.9796277090590024 ) ) ;
#52692 = CARTESIAN_POINT ( 'NONE',  ( -17.07358046210000069, 1458.578126118629825, 230.5958457830979853 ) ) ;
#52693 = VERTEX_POINT ( 'NONE', #6352 ) ;
#52694 = ORIENTED_EDGE ( 'NONE', *, *, #91235, .T. ) ;
#52695 = CARTESIAN_POINT ( 'NONE',  ( 9.430278060304900123, 1452.926932606559831, 211.6524132603890109 ) ) ;
#52696 = CARTESIAN_POINT ( 'NONE',  ( 9.237784538809998836, 1425.317541609140108, 195.2081299371990042 ) ) ;
#52697 = VERTEX_POINT ( 'NONE', #39954 ) ;
#52698 = CARTESIAN_POINT ( 'NONE',  ( -0.7127565730050000603, 1412.056601978030130, 185.0301737879979953 ) ) ;
#52699 = CARTESIAN_POINT ( 'NONE',  ( 9.750569994704919807, 1446.597750952001888, 153.4809583364809384 ) ) ;
#52700 = VECTOR ( 'NONE', #110158, 1000.000000000000227 ) ;
#52701 = CYLINDRICAL_SURFACE ( 'NONE', #8223, 2.000000000000003109 ) ;
#52702 = AXIS2_PLACEMENT_3D ( 'NONE', #104267, #52772, #86910 ) ;
#52703 = CARTESIAN_POINT ( 'NONE',  ( -0.3989523678029999743, 1461.200148461630079, 235.3477028770979871 ) ) ;
#52704 = CARTESIAN_POINT ( 'NONE',  ( 7.012466281385699496, 1508.551704615640119, 203.6085871785070083 ) ) ;
#52705 = PRESENTATION_STYLE_ASSIGNMENT (( #35899 ) ) ;
#52706 = CARTESIAN_POINT ( 'NONE',  ( 4.329341215434487466, 1515.068899831254157, 212.0800836860477432 ) ) ;
#52707 = CARTESIAN_POINT ( 'NONE',  ( -89.81305537822530027, 1384.837953921539793, 292.4503084444569936 ) ) ;
#52708 = CARTESIAN_POINT ( 'NONE',  ( -2.486474780875000512, 1516.560253536979872, 202.1879665292270261 ) ) ;
#52709 = CARTESIAN_POINT ( 'NONE',  ( -6.949703372784999722, 1517.130100026000036, 208.3827239650380250 ) ) ;
#52710 = ORIENTED_EDGE ( 'NONE', *, *, #97888, .T. ) ;
#52711 = CARTESIAN_POINT ( 'NONE',  ( 11.84182917021260018, 1430.667802097110098, 149.7263372980079907 ) ) ;
#52712 = CARTESIAN_POINT ( 'NONE',  ( 12.88207677529630502, 1444.943664110688587, 186.6979557653219501 ) ) ;
#52713 = ORIENTED_EDGE ( 'NONE', *, *, #58849, .F. ) ;
#52714 = CYLINDRICAL_SURFACE ( 'NONE', #103582, 1.999999999999995559 ) ;
#52715 = EDGE_CURVE ( 'NONE', #38044, #100575, #74127, .T. ) ;
#52716 = CARTESIAN_POINT ( 'NONE',  ( -6.461178696532821064, 1508.551704651539922, 219.4694278874889903 ) ) ;
#52717 = CARTESIAN_POINT ( 'NONE',  ( 17.17241001986506888, 1512.187213306747481, 237.6251415217915337 ) ) ;
#52718 = DIRECTION ( 'NONE',  ( 0.1215792179600219541, -0.8574474952671515826, -0.5000022866150888312 ) ) ;
#52719 = CARTESIAN_POINT ( 'NONE',  ( -5.969328413430000424, 1422.018310919130045, 186.6257062000979943 ) ) ;
#52720 = CARTESIAN_POINT ( 'NONE',  ( 1.423691709839809860, 1409.795502070599923, 270.0714555743300025 ) ) ;
#52721 = CARTESIAN_POINT ( 'NONE',  ( 32.38601544705589674, 1523.530935881284904, 216.1237228173871472 ) ) ;
#52722 = CARTESIAN_POINT ( 'NONE',  ( -4.794937653589999904, 1475.260169187289875, 199.8527927719790114 ) ) ;
#52723 = CARTESIAN_POINT ( 'NONE',  ( -2.298880634834130188, 1421.940747973940006, 193.2957375577259995 ) ) ;
#52724 = CARTESIAN_POINT ( 'NONE',  ( -32.66522595970000253, 1379.629515683599948, 215.9478188136090182 ) ) ;
#52725 = CARTESIAN_POINT ( 'NONE',  ( 0.02716074563118510421, 1410.223742506766712, 233.2171245275475542 ) ) ;
#52727 = CARTESIAN_POINT ( 'NONE',  ( 11.01815538213319989, 1470.097469558069861, 206.4145453267350092 ) ) ;
#52726 = DIRECTION ( 'NONE',  ( 0.8775825618903754233, 0.000000000000000000, 0.4794255386041978984 ) ) ;
#52728 = CARTESIAN_POINT ( 'NONE',  ( -4.586155245401363878, 1423.742087943514889, 184.4069333355399181 ) ) ;
#52729 = CARTESIAN_POINT ( 'NONE',  ( 17.87507678963179814, 1419.602358105800022, 225.0615382930280077 ) ) ;
#52730 = CARTESIAN_POINT ( 'NONE',  ( -5.412016405372058969, 1422.582238247259966, 129.2850280054269945 ) ) ;
#52731 = VERTEX_POINT ( 'NONE', #90904 ) ;
#52732 = CARTESIAN_POINT ( 'NONE',  ( 6.438546668639999915, 1410.951844103429949, 268.3665355202980436 ) ) ;
#52733 = CARTESIAN_POINT ( 'NONE',  ( 19.66678637246580053, 1519.551704408389924, 202.3500283489900085 ) ) ;
#52734 = CARTESIAN_POINT ( 'NONE',  ( -21.37469332459370008, 1525.408327360777776, 233.4084527748692892 ) ) ;
#52735 = AXIS2_PLACEMENT_3D ( 'NONE', #108152, #31441, #102490 ) ;
#52736 = CARTESIAN_POINT ( 'NONE',  ( 3.648449339570000394, 1506.945873062889859, 220.2261837244989806 ) ) ;
#52737 = CARTESIAN_POINT ( 'NONE',  ( -14.47535368149999968, 1416.023439710309958, 214.4146907853689754 ) ) ;
#52739 = ORIENTED_EDGE ( 'NONE', *, *, #15689, .T. ) ;
#52738 = CARTESIAN_POINT ( 'NONE',  ( 1.768532852308550174, 1515.064792882589927, 204.7923971856590128 ) ) ;
#52740 = CARTESIAN_POINT ( 'NONE',  ( -15.88354217481895425, 1415.957443832936178, 209.7362470719081102 ) ) ;
#52741 = CARTESIAN_POINT ( 'NONE',  ( -15.57748978299999898, 1507.212883763329955, 192.6976421578980023 ) ) ;
#52742 = CARTESIAN_POINT ( 'NONE',  ( -11.15490121449999883, 1425.160561550830153, 144.1688093937980000 ) ) ;
#52743 = DIRECTION ( 'NONE',  ( 1.000000000000000000, 0.000000000000000000, 0.000000000000000000 ) ) ;
#52744 = CARTESIAN_POINT ( 'NONE',  ( -4.155670335940000015, 1439.704322206689994, 185.4969475932980174 ) ) ;
#52745 = CARTESIAN_POINT ( 'NONE',  ( -14.17772861730700207, 1379.591530685439920, 207.8208986668599891 ) ) ;
#52746 = CARTESIAN_POINT ( 'NONE',  ( -7.717505791104999346, 1516.857914730730045, 201.4043401791270185 ) ) ;
#52747 = CARTESIAN_POINT ( 'NONE',  ( -15.84317036476499929, 1513.136578080079744, 223.4420747407669978 ) ) ;
#52748 = CARTESIAN_POINT ( 'NONE',  ( 13.43806146769999899, 1412.741207332130216, 228.4219197481980075 ) ) ;
#52749 = EDGE_CURVE ( 'NONE', #26525, #41801, #90634, .T. ) ;
#52750 = CARTESIAN_POINT ( 'NONE',  ( -10.67770939150419984, 1481.275619385470236, 208.2056862302819980 ) ) ;
#52751 = CARTESIAN_POINT ( 'NONE',  ( -16.32193376780000094, 1459.453084261929916, 228.9511341082980209 ) ) ;
#52752 = CARTESIAN_POINT ( 'NONE',  ( 2.283570633165000086, 1516.909589401870107, 206.2402975076569760 ) ) ;
#52753 = CARTESIAN_POINT ( 'NONE',  ( 30.03438762969999942, 1414.561137273029999, 268.9518563996979879 ) ) ;
#52754 = CARTESIAN_POINT ( 'NONE',  ( -34.31402925621615196, 1524.244163922423695, 218.0340858097422085 ) ) ;
#52755 = CARTESIAN_POINT ( 'NONE',  ( 1.430288155006089523, 1465.025930583076388, 237.8691320678095167 ) ) ;
#52756 = CARTESIAN_POINT ( 'NONE',  ( 20.75570910649999590, 1488.585678912729918, 191.6580715406979891 ) ) ;
#52757 = CARTESIAN_POINT ( 'NONE',  ( 19.47833342507072274, 1506.473666147355971, 219.3888140167584027 ) ) ;
#52758 = CARTESIAN_POINT ( 'NONE',  ( -13.09309660601929970, 1379.413120505010056, 208.1547604687910109 ) ) ;
#52759 = CARTESIAN_POINT ( 'NONE',  ( -15.62861149524349891, 1418.244676918490086, 203.0179538217920197 ) ) ;
#52760 = CARTESIAN_POINT ( 'NONE',  ( 17.33107428800062522, 1477.785820313406475, 220.5162645747961108 ) ) ;
#52761 = CARTESIAN_POINT ( 'NONE',  ( -1.598721155459999993E-13, 1416.913060387330006, 198.3331309146979891 ) ) ;
#52762 = CARTESIAN_POINT ( 'NONE',  ( -15.57409121169999899, 1415.640300991889944, 209.4226310109950191 ) ) ;
#52763 = CARTESIAN_POINT ( 'NONE',  ( -13.45510625179999842, 1442.037881746980020, 188.3676330511979984 ) ) ;
#52764 = DIRECTION ( 'NONE',  ( -0.8775825618903720926, 0.000000000000000000, -0.4794255386042041156 ) ) ;
#52765 = CARTESIAN_POINT ( 'NONE',  ( -29.18335203569999692, 1435.678379713110189, 136.0914706953979874 ) ) ;
#52766 = CARTESIAN_POINT ( 'NONE',  ( 1.467075754108839503, 1432.098771012052794, 200.8278867525325495 ) ) ;
#52767 = EDGE_LOOP ( 'NONE', ( #50473, #5999, #24569, #39587 ) ) ;
#52768 = DIRECTION ( 'NONE',  ( -0.05489692781948048161, 0.01152269768267543196, -0.9984255379116142581 ) ) ;
#52769 = CARTESIAN_POINT ( 'NONE',  ( -13.17055926657740095, 1409.372986451539873, 202.0656305217389956 ) ) ;
#52770 = AXIS2_PLACEMENT_3D ( 'NONE', #62653, #20044, #26795 ) ;
#52771 = CARTESIAN_POINT ( 'NONE',  ( -13.12541650777430036, 1507.970701092599938, 209.3483060399670137 ) ) ;
#52772 = DIRECTION ( 'NONE',  ( -1.836970198721029688E-16, -1.000000000000000000, 0.000000000000000000 ) ) ;
#52773 = CARTESIAN_POINT ( 'NONE',  ( -42.46955762170000526, 1456.102617841730080, 267.1011643380979876 ) ) ;
#52774 = CARTESIAN_POINT ( 'NONE',  ( -30.44070839969640829, 1525.425665131968344, 196.7701875139011634 ) ) ;
#52775 = CARTESIAN_POINT ( 'NONE',  ( 0.1712859756662860056, 1420.019041673809852, 183.9765777425620001 ) ) ;
#52776 = VECTOR ( 'NONE', #91844, 1000.000000000000000 ) ;
#52777 = CARTESIAN_POINT ( 'NONE',  ( 18.31963684070830212, 1421.106839041940020, 223.3124397329580120 ) ) ;
#52778 = CARTESIAN_POINT ( 'NONE',  ( -68.46353614679770772, 1384.666907584059800, 293.2737738776249898 ) ) ;
#52779 = CARTESIAN_POINT ( 'NONE',  ( -25.34732223421400121, 1384.960228105589977, 203.3983496752080100 ) ) ;
#52780 = CARTESIAN_POINT ( 'NONE',  ( 16.76434746429979938, 1422.577036823120125, 227.0063948903039943 ) ) ;
#52781 = CARTESIAN_POINT ( 'NONE',  ( 15.56083348049999948, 1415.425433635630043, 217.3404540485179837 ) ) ;
#52782 = CARTESIAN_POINT ( 'NONE',  ( -28.26734827197039834, 1508.339354041070010, 208.8484260271879975 ) ) ;
#52783 = DIRECTION ( 'NONE',  ( 0.000000000000000000, 1.000000000000000000, 0.000000000000000000 ) ) ;
#52784 = DIRECTION ( 'NONE',  ( -1.755985294532469921E-16, 1.000000000000000000, -1.338183447452831989E-16 ) ) ;
#52785 = CARTESIAN_POINT ( 'NONE',  ( -7.811850951430000300, 1508.423641399529970, 181.5011841995979864 ) ) ;
#52786 = EDGE_CURVE ( 'NONE', #72650, #28577, #19837, .T. ) ;
#52787 = CARTESIAN_POINT ( 'NONE',  ( -23.47537152620000356, 1410.228075751530014, 207.0042901657579932 ) ) ;
#52788 = ADVANCED_FACE ( 'NONE', ( #98200 ), #65723, .F. ) ;
#52789 = EDGE_CURVE ( 'NONE', #14979, #64002, #95071, .T. ) ;
#52790 = CARTESIAN_POINT ( 'NONE',  ( 15.03806483009999972, 1414.913060387229962, 201.9300244649979845 ) ) ;
#52791 = CARTESIAN_POINT ( 'NONE',  ( 4.297912049859999861, 1484.403092702089907, 220.1616355836989953 ) ) ;
#52792 = CARTESIAN_POINT ( 'NONE',  ( 4.582279963310000426, 1422.267990882979802, 194.3935423355989940 ) ) ;
#52793 = ADVANCED_FACE ( 'NONE', ( #57340 ), #98753, .F. ) ;
#52794 = B_SPLINE_SURFACE_WITH_KNOTS ( 'NONE', 5, 5, ( 
 ( #21765, #82254, #55966, #6649, #92301, #22316, #73312, #13373, #6095 ),
 ( #31848, #72767, #23442, #32411, #13928, #106895, #22871, #81683, #39134 ),
 ( #66034, #107998, #31295, #100157, #107448, #64925, #99038, #40802, #56518 ),
 ( #99588, #90645, #57080, #8843, #77725, #59832, #75533, #109668, #92855 ),
 ( #43026, #69344, #18342, #17777, #32944, #25085, #1038, #16131, #33485 ),
 ( #67134, #67687, #41915, #68250, #94504, #8294, #77184, #93406, #16671 ) ),
 .UNSPECIFIED., .F., .F., .F.,
 ( 6, 6 ),
 ( 6, 3, 6 ),
 ( 4.238752792101360356, 5.659133035218639307 ),
 ( -0.001527176327848870111, 0.5000000000000000000, 1.002061266618639923 ),
 .UNSPECIFIED. ) ;
#52795 = CARTESIAN_POINT ( 'NONE',  ( -12.68266539220000055, 1434.593723365520191, 149.3604887061979696 ) ) ;
#52796 = EDGE_CURVE ( 'NONE', #59575, #94675, #101317, .T. ) ;
#52797 = CARTESIAN_POINT ( 'NONE',  ( -2.613520083516720049, 1448.739697532430000, 188.5780410999010144 ) ) ;
#52798 = CARTESIAN_POINT ( 'NONE',  ( 19.39983987834424539, 1522.861859112239017, 239.2921289694150460 ) ) ;
#52799 = CARTESIAN_POINT ( 'NONE',  ( -7.567241880450000124, 1385.515695150829970, 219.0512258816089854 ) ) ;
#52801 = CARTESIAN_POINT ( 'NONE',  ( -9.362782585499999755, 1381.058213305800109, 200.9707292486589836 ) ) ;
#52800 = CARTESIAN_POINT ( 'NONE',  ( -22.65427071730000108, 1411.066072191229750, 211.5467506970180125 ) ) ;
#52802 = CARTESIAN_POINT ( 'NONE',  ( 1.358317420979999968, 1411.681908635930085, 232.6968902729979902 ) ) ;
#52803 = CARTESIAN_POINT ( 'NONE',  ( 9.816185060832909315, 1435.693060327849935, 209.5517428691599946 ) ) ;
#52804 = CARTESIAN_POINT ( 'NONE',  ( -10.46250751100000009, 1491.356802620389999, 212.5409670600390086 ) ) ;
#52805 = SPHERICAL_SURFACE ( 'NONE', #31811, 2.000000000000000000 ) ;
#52806 = CARTESIAN_POINT ( 'NONE',  ( -0.6083677694837460459, 1420.015852375959867, 184.4634389772880070 ) ) ;
#52807 = CARTESIAN_POINT ( 'NONE',  ( -0.01306004006829850073, 1516.939762005280045, 204.5032625402269844 ) ) ;
#52808 = CARTESIAN_POINT ( 'NONE',  ( -3.761263762889859752, 1398.025418639840154, 221.5750308120653074 ) ) ;
#52809 = CARTESIAN_POINT ( 'NONE',  ( 14.83698683853499922, 1514.217947259989842, 193.9974257499669932 ) ) ;
#52810 = CARTESIAN_POINT ( 'NONE',  ( -14.59402636152660016, 1485.278995523290178, 186.7907175241479933 ) ) ;
#52811 = CARTESIAN_POINT ( 'NONE',  ( -18.20455311950000166, 1430.274367750729880, 193.6929569324979923 ) ) ;
#52812 = CARTESIAN_POINT ( 'NONE',  ( 9.849121764593530060, 1503.262452723809929, 216.7244655636139896 ) ) ;
#52813 = CARTESIAN_POINT ( 'NONE',  ( 41.65411205771810188, 1444.066986349939953, 136.1144878563849829 ) ) ;
#52815 = EDGE_LOOP ( 'NONE', ( #96801, #32294, #46378, #32266 ) ) ;
#52814 = CARTESIAN_POINT ( 'NONE',  ( -66.96278127175379780, 1379.743653987389962, 277.9592658266520289 ) ) ;
#52816 = ORIENTED_EDGE ( 'NONE', *, *, #19123, .T. ) ;
#52817 = CARTESIAN_POINT ( 'NONE',  ( 11.35222491904410091, 1434.076906344789904, 151.4872001750849790 ) ) ;
#52818 = CARTESIAN_POINT ( 'NONE',  ( 22.07691418024165486, 1523.843271061949054, 184.4448120176447503 ) ) ;
#52819 = ORIENTED_EDGE ( 'NONE', *, *, #28685, .F. ) ;
#52820 = DIRECTION ( 'NONE',  ( 0.9858563016923833633, 0.000000000000000000, 0.1675928173085483863 ) ) ;
#52821 = AXIS2_PLACEMENT_3D ( 'NONE', #48872, #82998, #58358 ) ;
#52822 = CARTESIAN_POINT ( 'NONE',  ( -3.487592469308334220, 1508.551704408389469, 213.9802063543035331 ) ) ;
#52824 = CARTESIAN_POINT ( 'NONE',  ( 13.42479616400980014, 1453.338203267170002, 224.7140346886050111 ) ) ;
#52823 = CARTESIAN_POINT ( 'NONE',  ( -0.7920961534389989733, 1444.349757015490013, 199.4831802694889973 ) ) ;
#52825 = CARTESIAN_POINT ( 'NONE',  ( -0.3602478992429999916, 1417.265131029429995, 235.9082177996980079 ) ) ;
#52826 = EDGE_CURVE ( 'NONE', #42035, #12639, #13074, .T. ) ;
#52827 = CARTESIAN_POINT ( 'NONE',  ( 0.3235747208499999972, 1507.644137708130074, 180.9006323824980029 ) ) ;
#52828 = CARTESIAN_POINT ( 'NONE',  ( 1.159955629579999981, 1469.039094341789905, 219.1201689042090095 ) ) ;
#52829 = CARTESIAN_POINT ( 'NONE',  ( -24.05569699374110115, 1444.796293269080024, 211.9644565330009982 ) ) ;
#52830 = CARTESIAN_POINT ( 'NONE',  ( -6.546951720715000533, 1516.606339319019980, 211.9964348928969855 ) ) ;
#52831 = EDGE_CURVE ( 'NONE', #14771, #8790, #47260, .T. ) ;
#52833 = VECTOR ( 'NONE', #51172, 1000.000000000000114 ) ;
#52832 = CARTESIAN_POINT ( 'NONE',  ( 36.31760351622449434, 1436.138747408989957, 134.0999999970809995 ) ) ;
#52835 =( BOUNDED_CURVE ( )  B_SPLINE_CURVE ( 3, ( #46548, #38119, #55494, #56034 ),
 .UNSPECIFIED., .F., .T. ) 
 B_SPLINE_CURVE_WITH_KNOTS ( ( 4, 4 ),
 ( 1.010406472820884138, 2.131186328586304857 ),
 .UNSPECIFIED. ) 
 CURVE ( )  GEOMETRIC_REPRESENTATION_ITEM ( )  RATIONAL_B_SPLINE_CURVE ( ( 1.000000000000000000, 0.8980319481995078235, 0.8980319481995078235, 1.000000000000000000 ) ) 
 REPRESENTATION_ITEM ( '' )  );
#52834 = CARTESIAN_POINT ( 'NONE',  ( -9.970572234719458748, 1422.681531195490152, 209.6984921149189915 ) ) ;
#52836 = CARTESIAN_POINT ( 'NONE',  ( 7.284055418254999914, 1511.816633140279919, 202.4402870219569763 ) ) ;
#52837 = VERTEX_POINT ( 'NONE', #38840 ) ;
#52838 = CARTESIAN_POINT ( 'NONE',  ( 13.90627238822369804, 1435.005108322179922, 148.8090833361299872 ) ) ;
#52839 = CARTESIAN_POINT ( 'NONE',  ( 1.241329981776470026, 1432.830262692500128, 200.7618047978820073 ) ) ;
#52840 = ORIENTED_EDGE ( 'NONE', *, *, #1710, .F. ) ;
#52841 = ORIENTED_EDGE ( 'NONE', *, *, #73472, .F. ) ;
#52842 = EDGE_CURVE ( 'NONE', #5765, #45814, #78556, .T. ) ;
#52843 = ORIENTED_EDGE ( 'NONE', *, *, #10589, .T. ) ;
#52844 = CARTESIAN_POINT ( 'NONE',  ( -7.843966652515001137, 1513.355826799109764, 216.6951227995569980 ) ) ;
#52845 = CARTESIAN_POINT ( 'NONE',  ( 16.60697870052440095, 1513.055456493448446, 197.0683699863935772 ) ) ;
#52846 = CARTESIAN_POINT ( 'NONE',  ( 22.71382099334196525, 1450.890321816409596, 142.2309692183697223 ) ) ;
#52847 = CARTESIAN_POINT ( 'NONE',  ( -3.677613769069999778E-16, 1378.413060387289988, 209.1218459616989946 ) ) ;
#52848 = CARTESIAN_POINT ( 'NONE',  ( 10.10905482369999930, 1461.386512506689996, 208.4426341976229935 ) ) ;
#52849 = ADVANCED_FACE ( 'NONE', ( #101485 ), #67102, .T. ) ;
#52850 = CARTESIAN_POINT ( 'NONE',  ( -19.08445480129999794, 1440.913060387330006, 209.8212738029720299 ) ) ;
#52851 = CARTESIAN_POINT ( 'NONE',  ( -49.19594470377145257, 1379.685644944692058, 238.0301645601815892 ) ) ;
#52852 = CARTESIAN_POINT ( 'NONE',  ( 4.288402489466680123, 1446.931632216600065, 155.2279950395780190 ) ) ;
#52853 = CARTESIAN_POINT ( 'NONE',  ( 8.631780704876279131, 1438.018275767699834, 210.0183142686710198 ) ) ;
#52854 = CARTESIAN_POINT ( 'NONE',  ( 2.864972116015000125, 1516.859514182039902, 206.2412530031170093 ) ) ;
#52855 = ORIENTED_EDGE ( 'NONE', *, *, #85022, .F. ) ;
#52856 = CARTESIAN_POINT ( 'NONE',  ( 30.44909158939109872, 1440.913060387330006, 253.0088576829679994 ) ) ;
#52857 = B_SPLINE_CURVE_WITH_KNOTS ( 'NONE', 3,
 ( #101157, #6018, #100614, #65400 ),
 .UNSPECIFIED., .F., .F.,
 ( 4, 4 ),
 ( 0.000000000000000000, 0.0002960034161023850563 ),
 .UNSPECIFIED. ) ;
#52858 = CARTESIAN_POINT ( 'NONE',  ( -18.25434091379999657, 1509.489596267130310, 186.0409464828979935 ) ) ;
#52859 = ORIENTED_EDGE ( 'NONE', *, *, #70047, .F. ) ;
#52860 = CARTESIAN_POINT ( 'NONE',  ( 27.00209765840460108, 1448.139277255909747, 136.8875338484010058 ) ) ;
#52861 = CARTESIAN_POINT ( 'NONE',  ( -14.20408294209999944, 1409.911027547829917, 190.5440136396979938 ) ) ;
#52862 = CARTESIAN_POINT ( 'NONE',  ( -24.31663051820000021, 1442.649873241249907, 211.4598721613180032 ) ) ;
#52863 = CARTESIAN_POINT ( 'NONE',  ( -10.79382126600000014, 1414.913060387329779, 196.1395803457980094 ) ) ;
#52864 = CARTESIAN_POINT ( 'NONE',  ( 16.81223453394349932, 1414.913060391199906, 210.6693087035600058 ) ) ;
#52865 = CARTESIAN_POINT ( 'NONE',  ( 26.87832337146859629, 1441.334257626130011, 137.4807418192719979 ) ) ;
#52866 = CARTESIAN_POINT ( 'NONE',  ( -13.50070407659999994, 1434.968958018969943, 149.9809230438979739 ) ) ;
#52867 = CARTESIAN_POINT ( 'NONE',  ( -3.389245491280000078, 1507.871109296990198, 220.9917548405990146 ) ) ;
#52869 = CARTESIAN_POINT ( 'NONE',  ( 1.247882269740000050, 1499.086923094689837, 200.6750383293390030 ) ) ;
#52868 = CARTESIAN_POINT ( 'NONE',  ( 20.38673671613194216, 1525.878013734320803, 182.1228282333742072 ) ) ;
#52870 = CARTESIAN_POINT ( 'NONE',  ( 3.456007385174999946, 1516.647534046129977, 215.6697273451470096 ) ) ;
#52871 = CARTESIAN_POINT ( 'NONE',  ( 23.69134289970000395, 1410.129789027929974, 209.5325461888999996 ) ) ;
#52872 = CARTESIAN_POINT ( 'NONE',  ( 5.705922834103000163, 1511.346048414110101, 217.0427200209030048 ) ) ;
#52873 = CARTESIAN_POINT ( 'NONE',  ( 28.09993147489999998, 1509.169756330429891, 207.7492410536980003 ) ) ;
#52874 = CARTESIAN_POINT ( 'NONE',  ( 3.461360093275000160, 1516.874084700499907, 212.3753080308970311 ) ) ;
#52875 = VECTOR ( 'NONE', #8263, 1000.000000000000000 ) ;
#52876 = EDGE_CURVE ( 'NONE', #13362, #44739, #61749, .T. ) ;
#52877 = CARTESIAN_POINT ( 'NONE',  ( -11.78126758929439966, 1482.336360767919814, 207.4553989261059996 ) ) ;
#52878 = CARTESIAN_POINT ( 'NONE',  ( 31.16641183314581554, 1524.201816949777367, 221.8713787598176737 ) ) ;
#52880 = ORIENTED_EDGE ( 'NONE', *, *, #82507, .F. ) ;
#52879 = CARTESIAN_POINT ( 'NONE',  ( -89.95656494280000004, 1388.077005338320077, 307.8707420459589912 ) ) ;
#52881 = CARTESIAN_POINT ( 'NONE',  ( 13.69365045770000044, 1462.915760504130049, 238.2645948893979835 ) ) ;
#52882 = CARTESIAN_POINT ( 'NONE',  ( 10.57855775040389901, 1491.027229822649815, 212.1174194973030183 ) ) ;
#52883 = CARTESIAN_POINT ( 'NONE',  ( -7.550503362009299835, 1510.480349264700180, 214.6730346447039892 ) ) ;
#52884 = CARTESIAN_POINT ( 'NONE',  ( -5.749669252027449495, 1509.117800599190105, 238.0245596231779928 ) ) ;
#52885 = CARTESIAN_POINT ( 'NONE',  ( -19.16951723229999871, 1456.627470220629903, 228.8719212425980061 ) ) ;
#52886 = ADVANCED_FACE ( 'NONE', ( #35976 ), #62440, .F. ) ;
#52888 = CARTESIAN_POINT ( 'NONE',  ( 17.91001729305950008, 1410.383396254900163, 222.9072237126829918 ) ) ;
#52887 = CARTESIAN_POINT ( 'NONE',  ( 10.97596755329999851, 1432.730980201519969, 151.7698537367980123 ) ) ;
#52889 = CARTESIAN_POINT ( 'NONE',  ( 0.1679668313380000000, 1470.808655612629764, 188.5134246798980087 ) ) ;
#52890 = CARTESIAN_POINT ( 'NONE',  ( -108.6040716729050075, 1381.990087626129935, 310.5709923410640272 ) ) ;
#52891 = EDGE_LOOP ( 'NONE', ( #6861, #8490, #40001, #79850, #49069 ) ) ;
#52892 = CARTESIAN_POINT ( 'NONE',  ( 3.449777315724999571, 1516.974592746400049, 204.1104779853070283 ) ) ;
#52893 = CARTESIAN_POINT ( 'NONE',  ( 0.2153512683669999983, 1405.989301470729970, 266.9611412585979906 ) ) ;
#52894 = CARTESIAN_POINT ( 'NONE',  ( 28.29497430790000223, 1509.672356515530055, 207.2299602969580121 ) ) ;
#52895 = AXIS2_PLACEMENT_3D ( 'NONE', #41446, #75611, #109741 ) ;
#52896 = CARTESIAN_POINT ( 'NONE',  ( 43.37196902965609979, 1452.013348346279827, 269.7132147777479645 ) ) ;
#52897 = CARTESIAN_POINT ( 'NONE',  ( -24.04686560566315023, 1437.475348716183362, 212.2910028660378998 ) ) ;
#52898 = CARTESIAN_POINT ( 'NONE',  ( -39.24082110814379831, 1450.608897959999922, 136.0275758983839864 ) ) ;
#52899 = DIRECTION ( 'NONE',  ( -2.664535259100376091E-15, 0.000000000000000000, -1.000000000000000000 ) ) ;
#52900 = CARTESIAN_POINT ( 'NONE',  ( -18.66420869458026388, 1526.382868172863937, 232.7837831374280881 ) ) ;
#52901 = EDGE_CURVE ( 'NONE', #96609, #56358, #21197, .T. ) ;
#52902 = CARTESIAN_POINT ( 'NONE',  ( 37.34923688015930310, 1449.321946719639982, 136.3170601122349979 ) ) ;
#52903 = LINE ( 'NONE', #106051, #5549 ) ;
#52904 = CARTESIAN_POINT ( 'NONE',  ( 1.304943139099999927, 1431.126433557689779, 200.1249384120889943 ) ) ;
#52905 = FACE_OUTER_BOUND ( 'NONE', #81528, .T. ) ;
#52906 = CARTESIAN_POINT ( 'NONE',  ( 3.561968680879999738, 1506.511571059590324, 220.3681565264990070 ) ) ;
#52907 = AXIS2_PLACEMENT_3D ( 'NONE', #38087, #29679, #73350 ) ;
#52908 = CARTESIAN_POINT ( 'NONE',  ( -113.4000000000000057, 1384.899971913130003, 304.2218459572590064 ) ) ;
#52909 = ORIENTED_EDGE ( 'NONE', *, *, #50445, .T. ) ;
#52910 = CARTESIAN_POINT ( 'NONE',  ( 20.70484064406359437, 1525.907212628473872, 185.0411015109854134 ) ) ;
#52911 = CARTESIAN_POINT ( 'NONE',  ( -22.08622291482367217, 1523.456872492435195, 184.4183880513178053 ) ) ;
#52912 = CARTESIAN_POINT ( 'NONE',  ( 4.589161282302300471, 1466.737739933080093, 198.9391871293819918 ) ) ;
#52913 = CARTESIAN_POINT ( 'NONE',  ( -0.3001262975330000193, 1417.357112613329946, 235.2038291758979938 ) ) ;
#52914 = CARTESIAN_POINT ( 'NONE',  ( 11.49580466759999986, 1502.679721642689856, 209.6813715333399841 ) ) ;
#52915 = CARTESIAN_POINT ( 'NONE',  ( -33.42844755917201383, 1522.382868172863709, 196.1165140606795489 ) ) ;
#52916 = CARTESIAN_POINT ( 'NONE',  ( 9.345713659299999421, 1422.635913846680069, 212.8840062826189978 ) ) ;
#52917 = CARTESIAN_POINT ( 'NONE',  ( -13.73849276585309909, 1384.880433421959879, 219.2007748097859690 ) ) ;
#52918 = CARTESIAN_POINT ( 'NONE',  ( -5.923682464646780943, 1517.051704408389924, 223.8623791742500089 ) ) ;
#52919 = CARTESIAN_POINT ( 'NONE',  ( 12.49401126939999962, 1451.800774058590150, 193.6953293048989906 ) ) ;
#52920 = CARTESIAN_POINT ( 'NONE',  ( 26.26971730801799865, 1435.434881028299969, 135.5857965276559867 ) ) ;
#52921 = EDGE_CURVE ( 'NONE', #83491, #17784, #86677, .T. ) ;
#52922 = CARTESIAN_POINT ( 'NONE',  ( -8.775825618903738246, 1374.413060387289988, 204.3275905756569841 ) ) ;
#52923 = ORIENTED_EDGE ( 'NONE', *, *, #89948, .F. ) ;
#52924 = CARTESIAN_POINT ( 'NONE',  ( -16.14700684228250083, 1409.476921796170018, 225.0741814793740332 ) ) ;
#52925 = EDGE_CURVE ( 'NONE', #22416, #31153, #46596, .T. ) ;
#52926 = CARTESIAN_POINT ( 'NONE',  ( -2.782618081592460157, 1489.016425230830009, 216.8593202305619911 ) ) ;
#52927 = ORIENTED_EDGE ( 'NONE', *, *, #35715, .F. ) ;
#52928 = FACE_OUTER_BOUND ( 'NONE', #3001, .T. ) ;
#52929 = CARTESIAN_POINT ( 'NONE',  ( 6.483466624646080589, 1516.674728680589396, 205.3469896361293365 ) ) ;
#52930 = CARTESIAN_POINT ( 'NONE',  ( -21.83550407203883736, 1523.678648413191695, 234.9693198511254195 ) ) ;
#52932 = CARTESIAN_POINT ( 'NONE',  ( 1.388898171294610018, 1456.630141039370073, 219.6509599159400068 ) ) ;
#52931 = CARTESIAN_POINT ( 'NONE',  ( 10.36044274480000027, 1425.414401215230100, 93.45973651769790536 ) ) ;
#52933 = CARTESIAN_POINT ( 'NONE',  ( -0.2329163981069990175, 1457.935017252390253, 202.2546241818889996 ) ) ;
#52934 = CARTESIAN_POINT ( 'NONE',  ( -9.466658637189999226, 1449.313965536590104, 207.5701179724289887 ) ) ;
#52935 = CARTESIAN_POINT ( 'NONE',  ( 7.716878902974999122, 1516.833976295079992, 201.7919207096969672 ) ) ;
#52936 = CARTESIAN_POINT ( 'NONE',  ( 7.424089790420000057, 1424.882440436209890, 212.3756834930689763 ) ) ;
#52937 = CARTESIAN_POINT ( 'NONE',  ( -8.229021304010000648, 1439.448076410589920, 228.6152058856989697 ) ) ;
#52938 = PLANE ( 'NONE',  #108806 ) ;
#52939 = CARTESIAN_POINT ( 'NONE',  ( 3.439533802020000142, 1449.329777843420061, 184.0645408312979896 ) ) ;
#52940 = CARTESIAN_POINT ( 'NONE',  ( 8.122886720353145407, 1364.957098980272804, 208.3718459617061285 ) ) ;
#52941 = ADVANCED_FACE ( 'NONE', ( #21337 ), #50119, .T. ) ;
#52943 = EDGE_LOOP ( 'NONE', ( #50248, #97055, #15597, #9682 ) ) ;
#52942 = DIRECTION ( 'NONE',  ( -1.987342477590000096E-13, 6.939952856120000821E-15, 1.000000000000000000 ) ) ;
#52944 = ORIENTED_EDGE ( 'NONE', *, *, #31563, .T. ) ;
#52945 = CIRCLE ( 'NONE', #95846, 0.5000000000000147660 ) ;
#52946 = CARTESIAN_POINT ( 'NONE',  ( -41.65407267460000185, 1444.067062105530113, 136.1145731928979785 ) ) ;
#52947 = CIRCLE ( 'NONE', #4660, 1.999994602477440653 ) ;
#52948 = CARTESIAN_POINT ( 'NONE',  ( 32.28466283162151029, 1512.187213306747481, 199.0684425896244250 ) ) ;
#52949 = DIRECTION ( 'NONE',  ( 0.000000000000000000, -1.000000000000000000, 0.000000000000000000 ) ) ;
#52950 = CARTESIAN_POINT ( 'NONE',  ( -8.016996095914999287, 1511.645462744430006, 212.5548212549570053 ) ) ;
#52951 = CARTESIAN_POINT ( 'NONE',  ( -1.316513911440000184, 1486.231707541229980, 181.7543151367980272 ) ) ;
#52952 = CARTESIAN_POINT ( 'NONE',  ( 20.58555848629999829, 1507.839439013330093, 189.9311647047979932 ) ) ;
#52953 = CARTESIAN_POINT ( 'NONE',  ( -1.289615935422919968, 1475.477284819069837, 197.7490727346969948 ) ) ;
#52954 = CARTESIAN_POINT ( 'NONE',  ( 22.55885583319999910, 1410.621632374630053, 206.4601081238480162 ) ) ;
#52955 = B_SPLINE_SURFACE_WITH_KNOTS ( 'NONE', 5, 5, ( 
 ( #44078, #26702, #26139, #60899, #18843, #60328 ),
 ( #78216, #1528, #69851, #53039, #87175, #10463 ),
 ( #100332, #53642, #94491, #95065, #78821, #104567 ),
 ( #27861, #3242, #87217, #105126, #69334, #60936 ),
 ( #71005, #36258, #2135, #26747, #95614, #17763 ),
 ( #18880, #43564, #37369, #45793, #70447, #2691 ) ),
 .UNSPECIFIED., .F., .F., .F.,
 ( 6, 6 ),
 ( 6, 6 ),
 ( 7.548656686110299496, 12.57640183248079957 ),
 ( 0.000000000000000000, 0.5000176499936439534 ),
 .UNSPECIFIED. ) ;
#52956 = CARTESIAN_POINT ( 'NONE',  ( 33.91368255268339738, 1435.681798330320134, 135.0664145109430194 ) ) ;
#52957 = CARTESIAN_POINT ( 'NONE',  ( 27.32008277287192755, 1435.451596658461540, 135.2710114260797809 ) ) ;
#52958 = CARTESIAN_POINT ( 'NONE',  ( 15.07167880837459961, 1409.439375008719935, 204.0198465041329996 ) ) ;
#52959 = CARTESIAN_POINT ( 'NONE',  ( 5.661443424597549908E-05, 1405.842742645599856, 267.2348689328309774 ) ) ;
#52960 = B_SPLINE_CURVE_WITH_KNOTS ( 'NONE', 3,
 ( #88167, #28805, #21467, #63002, #97110, #45631, #11455, #20376, #54581, #88716, #11996, #80309, #3625, #89797, #78653, #22557, #5809, #48926, #24230, #65717, #30441, #83054, #6347, #48368, #39949, #32099, #73012, #100934, #15275, #74121, #58415, #99837, #13616, #41044, #108250, #57871, #49468, #83588, #23129, #32651, #73575, #109374, #23686 ),
 .UNSPECIFIED., .F., .F.,
 ( 4, 3, 3, 3, 3, 3, 3, 3, 3, 3, 3, 3, 3, 3, 4 ),
 ( 9.298193603555128917, 10.98315671184179898, 12.97260628368140090, 15.05249941581099904, 16.75275777422749712, 18.32915130324699859, 19.75511727758679825, 19.90554483226650007, 21.13603391183419689, 22.44647941495799870, 23.82709552150320320, 25.30707762746569500, 27.06563981043629497, 29.15018126801379594, 30.45919393759999849 ),
 .UNSPECIFIED. ) ;
#52961 = CARTESIAN_POINT ( 'NONE',  ( -14.11277764225159892, 1435.081315985899892, 149.0355979864779954 ) ) ;
#52962 = ORIENTED_EDGE ( 'NONE', *, *, #63596, .F. ) ;
#52963 = LINE ( 'NONE', #27740, #107248 ) ;
#52964 = CARTESIAN_POINT ( 'NONE',  ( 13.97694847940000074, 1444.778227271800006, 189.3186977499980230 ) ) ;
#52965 = ORIENTED_EDGE ( 'NONE', *, *, #9653, .T. ) ;
#52966 = EDGE_CURVE ( 'NONE', #81429, #82793, #30555, .T. ) ;
#52967 = EDGE_LOOP ( 'NONE', ( #51816, #21636, #97472, #60833 ) ) ;
#52968 = CARTESIAN_POINT ( 'NONE',  ( -4.336802270429999773, 1455.494076152190019, 200.7328417250689938 ) ) ;
#52969 = CARTESIAN_POINT ( 'NONE',  ( 7.340269731169999368, 1361.836778001489847, 207.6218459616989946 ) ) ;
#52970 = EDGE_CURVE ( 'NONE', #21237, #967, #50448, .T. ) ;
#52971 = CARTESIAN_POINT ( 'NONE',  ( -3.255340964424999761, 1516.962555622980062, 213.7459452615670159 ) ) ;
#52972 = CARTESIAN_POINT ( 'NONE',  ( 2.838446966914999869, 1511.534866634170157, 216.7374015997870060 ) ) ;
#52973 = MECHANICAL_DESIGN_GEOMETRIC_PRESENTATION_REPRESENTATION (  '', ( #60162 ), #26147 ) ;
#52974 = B_SPLINE_CURVE_WITH_KNOTS ( 'NONE', 5,
 ( #38235, #38783, #98137, #106550, #29838, #22503, #48314, #37695, #90840 ),
 .UNSPECIFIED., .F., .F.,
 ( 6, 3, 6 ),
 ( 0.000000000000000000, 0.4999997632602161679, 1.000000000000000000 ),
 .UNSPECIFIED. ) ;
#52975 = ORIENTED_EDGE ( 'NONE', *, *, #28120, .F. ) ;
#52976 = CARTESIAN_POINT ( 'NONE',  ( -95.07903399769999453, 1377.031630663760097, 300.1294849942590304 ) ) ;
#52977 = CARTESIAN_POINT ( 'NONE',  ( -106.1512004960610085, 1378.913060387289988, 302.5374961247920282 ) ) ;
#52978 = CARTESIAN_POINT ( 'NONE',  ( -7.720650173434999708, 1516.977993847330026, 203.3422188780170075 ) ) ;
#52979 = CARTESIAN_POINT ( 'NONE',  ( -29.12655649119999879, 1509.869978475729795, 207.5400152816580146 ) ) ;
#52980 = CARTESIAN_POINT ( 'NONE',  ( -0.5955487639629999386, 1497.701650616130109, 231.3320226370980208 ) ) ;
#52981 = CARTESIAN_POINT ( 'NONE',  ( 11.13831797290559500, 1433.014992880461932, 151.6441518879982766 ) ) ;
#52982 = CARTESIAN_POINT ( 'NONE',  ( -57.22511502587629906, 1384.656476375839929, 238.2158304579979813 ) ) ;
#52983 = FACE_OUTER_BOUND ( 'NONE', #51181, .T. ) ;
#52984 = CARTESIAN_POINT ( 'NONE',  ( -2.815577456780000265, 1409.178966352830003, 232.0007561677979879 ) ) ;
#52986 = VERTEX_POINT ( 'NONE', #100085 ) ;
#52985 = CARTESIAN_POINT ( 'NONE',  ( -5.737215272600000304, 1447.742823947540046, 185.4050672243980102 ) ) ;
#52987 = CARTESIAN_POINT ( 'NONE',  ( 1.925297169133120212, 1517.051704408389924, 230.6853930764029883 ) ) ;
#52988 = CARTESIAN_POINT ( 'NONE',  ( 3.181172983203653715, 1442.605928314588482, 217.4126502573513164 ) ) ;
#52989 = CARTESIAN_POINT ( 'NONE',  ( -9.359048371426943902, 1440.623807415093552, 205.4859881516416635 ) ) ;
#52990 = CARTESIAN_POINT ( 'NONE',  ( 15.64138586982451251, 1506.512156827755462, 224.6616658709005776 ) ) ;
#52991 = CARTESIAN_POINT ( 'NONE',  ( -24.99760032100000018, 1435.446235554499935, 136.3617712744980111 ) ) ;
#52992 = B_SPLINE_CURVE_WITH_KNOTS ( 'NONE', 3,
 ( #89257, #22014, #91465, #38293, #63543, #64633, #65175, #48376, #73582, #13623, #107157, #23137, #39955, #106064, #98754, #13075, #29344, #80315, #47262, #47811, #4698, #20931, #74129, #81946, #73018, #65724, #30449, #71953 ),
 .UNSPECIFIED., .F., .F.,
 ( 4, 3, 3, 3, 3, 3, 3, 3, 3, 4 ),
 ( -7.748415063910000455, -7.637761903620339687, -7.426814887477540594, -7.105214711045070075, -6.860935728577989501, -6.655162690954419702, -5.895137996252290513, -5.135113301550160436, -4.241455848545670371, -3.182527802580000120 ),
 .UNSPECIFIED. ) ;
#52993 = CARTESIAN_POINT ( 'NONE',  ( 1.715704490974999885, 1516.757508073510053, 212.3732403323669757 ) ) ;
#52994 = CARTESIAN_POINT ( 'NONE',  ( -66.90724276829999440, 1379.748944712210005, 276.4281807783590352 ) ) ;
#52995 = CARTESIAN_POINT ( 'NONE',  ( -7.824237587485725953, 1425.785369531576407, 225.8505889053163287 ) ) ;
#52996 = CARTESIAN_POINT ( 'NONE',  ( 2.801469573665160251, 1486.711816252329754, 216.6332114747600031 ) ) ;
#52997 = CARTESIAN_POINT ( 'NONE',  ( -22.15968191147809918, 1485.573429526870086, 217.2083819532319922 ) ) ;
#52998 =( BOUNDED_CURVE ( )  B_SPLINE_CURVE ( 3, ( #97861, #90568, #82169, #21136 ),
 .UNSPECIFIED., .F., .F. ) 
 B_SPLINE_CURVE_WITH_KNOTS ( ( 4, 4 ),
 ( 4.137179913343402404, 5.287886354397532074 ),
 .UNSPECIFIED. ) 
 CURVE ( )  GEOMETRIC_REPRESENTATION_ITEM ( )  RATIONAL_B_SPLINE_CURVE ( ( 1.000000000000000000, 0.8926667709749616098, 0.8926667709749616098, 1.000000000000000000 ) ) 
 REPRESENTATION_ITEM ( '' )  );
#52999 = CARTESIAN_POINT ( 'NONE',  ( 5.775625077365000415, 1516.745833913490060, 208.3665194962490261 ) ) ;
#53000 = ORIENTED_EDGE ( 'NONE', *, *, #2530, .F. ) ;
#53001 = CARTESIAN_POINT ( 'NONE',  ( 18.11157372306810132, 1509.545530478630099, 186.5307137986639816 ) ) ;
#53002 = CARTESIAN_POINT ( 'NONE',  ( -8.348226541789999899, 1410.293767215830030, 230.4853368651980077 ) ) ;
#53003 = CARTESIAN_POINT ( 'NONE',  ( -13.36175619390000158, 1385.161385112729931, 218.9601252273889997 ) ) ;
#53004 = ORIENTED_EDGE ( 'NONE', *, *, #80268, .T. ) ;
#53005 = CARTESIAN_POINT ( 'NONE',  ( -17.52406974176239629, 1385.285689121970108, 220.0437453706010160 ) ) ;
#53006 = CARTESIAN_POINT ( 'NONE',  ( -3.179433604570000238, 1429.659768554990023, 201.3028921480589872 ) ) ;
#53007 = CARTESIAN_POINT ( 'NONE',  ( 11.90929545309599824, 1435.055828996039963, 151.1761558931260083 ) ) ;
#53008 = CARTESIAN_POINT ( 'NONE',  ( 17.12655147364909780, 1478.709137272870066, 229.5900271960919952 ) ) ;
#53009 = CARTESIAN_POINT ( 'NONE',  ( -24.29054017925709630, 1443.115968449809316, 212.2937530787580727 ) ) ;
#53010 = CARTESIAN_POINT ( 'NONE',  ( -2.370751091799999877, 1409.499373923630174, 186.6993300599980046 ) ) ;
#53011 = FACE_OUTER_BOUND ( 'NONE', #53266, .T. ) ;
#53012 = CARTESIAN_POINT ( 'NONE',  ( 2.330134126090000368, 1515.064792882589927, 213.4512947377390049 ) ) ;
#53013 = ADVANCED_FACE ( 'NONE', ( #56443 ), #73239, .T. ) ;
#53015 = CARTESIAN_POINT ( 'NONE',  ( -3.633167781729999657, 1421.710620309329897, 184.3832545295979912 ) ) ;
#53014 = CARTESIAN_POINT ( 'NONE',  ( 1.130607463874999885, 1516.632821972880038, 215.6700465578769865 ) ) ;
#53016 = DIRECTION ( 'NONE',  ( 0.000000000000000000, 6.123233995736769734E-17, 1.000000000000000000 ) ) ;
#53017 = CARTESIAN_POINT ( 'NONE',  ( 0.01010282929720150019, 1516.939452820819952, 216.8414868732370167 ) ) ;
#53018 = ORIENTED_EDGE ( 'NONE', *, *, #100665, .T. ) ;
#53019 = CARTESIAN_POINT ( 'NONE',  ( -11.69495607182969898, 1415.089948427380023, 196.2579977906119950 ) ) ;
#53020 = CARTESIAN_POINT ( 'NONE',  ( -9.849896899200842881, 1519.913060387329779, 185.5490084180013923 ) ) ;
#53021 = ORIENTED_EDGE ( 'NONE', *, *, #109801, .T. ) ;
#53022 = LINE ( 'NONE', #26122, #69735 ) ;
#53023 = CARTESIAN_POINT ( 'NONE',  ( 1.959285310369999866, 1474.800623465989929, 220.3715843581990157 ) ) ;
#53024 = CARTESIAN_POINT ( 'NONE',  ( 8.452787181503049752, 1511.603576927810082, 203.2583637611789982 ) ) ;
#53025 = CARTESIAN_POINT ( 'NONE',  ( 2.931649531350000171, 1441.868998527789927, 217.8578126236290302 ) ) ;
#53026 = CARTESIAN_POINT ( 'NONE',  ( -32.77044109517588311, 1525.581535527370306, 199.0807904155091990 ) ) ;
#53027 = CARTESIAN_POINT ( 'NONE',  ( -16.66164933671169024, 1410.683962559431848, 191.7467638837736388 ) ) ;
#53028 = EDGE_CURVE ( 'NONE', #98016, #5707, #15848, .T. ) ;
#53029 = LINE ( 'NONE', #11565, #37772 ) ;
#53030 = CARTESIAN_POINT ( 'NONE',  ( 32.66476241579314177, 1526.382868172863937, 199.1278258474837060 ) ) ;
#53031 = CARTESIAN_POINT ( 'NONE',  ( -15.55222769949999950, 1435.858529176660113, 149.1409779191980078 ) ) ;
#53032 = CARTESIAN_POINT ( 'NONE',  ( -3.100416393482220201, 1464.813281825060130, 198.5539054533549859 ) ) ;
#53033 = CARTESIAN_POINT ( 'NONE',  ( 16.86766716609999861, 1410.829200371529851, 191.8268629579980029 ) ) ;
#53035 = CARTESIAN_POINT ( 'NONE',  ( -19.04725897784324573, 1440.081394454191695, 209.8288540874746388 ) ) ;
#53034 = CARTESIAN_POINT ( 'NONE',  ( 7.898231641030000638, 1488.783166887790003, 199.9435678271790096 ) ) ;
#53036 = CARTESIAN_POINT ( 'NONE',  ( 11.93532938889599393, 1433.537187971887988, 150.1924424211269695 ) ) ;
#53037 = VERTEX_POINT ( 'NONE', #57558 ) ;
#53038 = CARTESIAN_POINT ( 'NONE',  ( 13.32670741457809882, 1443.315591726400044, 195.2732919480440330 ) ) ;
#53039 = CARTESIAN_POINT ( 'NONE',  ( -4.556906923311959901, 1508.729448375579977, 212.2592363442360011 ) ) ;
#53040 = CARTESIAN_POINT ( 'NONE',  ( -11.90006702174173903, 1434.919293211649119, 147.6452046027968663 ) ) ;
#53041 = CARTESIAN_POINT ( 'NONE',  ( 30.90487439922560498, 1525.907212628473644, 216.4335774778780035 ) ) ;
#53042 = LINE ( 'NONE', #9912, #30348 ) ;
#53043 = CARTESIAN_POINT ( 'NONE',  ( 29.86461515634911024, 1525.960063244517187, 220.9690070206020778 ) ) ;
#53044 = CARTESIAN_POINT ( 'NONE',  ( -11.27974060871780004, 1470.421108576400002, 210.7070861076940105 ) ) ;
#53046 = CIRCLE ( 'NONE', #47681, 1.999999999999998668 ) ;
#53045 = CARTESIAN_POINT ( 'NONE',  ( -9.827124267810660285, 1490.452494543219927, 214.0432529463710125 ) ) ;
#53047 = CARTESIAN_POINT ( 'NONE',  ( -3.005245951399999615, 1450.300005596989877, 188.5532306447990152 ) ) ;
#53048 = CARTESIAN_POINT ( 'NONE',  ( -101.2580338645349940, 1383.763198325070107, 310.7707653970629735 ) ) ;
#53049 = CARTESIAN_POINT ( 'NONE',  ( -109.6263796463910012, 1384.395362625620010, 311.2927007664749794 ) ) ;
#53050 = CARTESIAN_POINT ( 'NONE',  ( 3.448830483803564828, 1512.187213306747481, 243.0842028158767789 ) ) ;
#53051 = CARTESIAN_POINT ( 'NONE',  ( -2.325909182683589815, 1516.529980546390107, 201.4129274379639867 ) ) ;
#53053 = ORIENTED_EDGE ( 'NONE', *, *, #19333, .F. ) ;
#53052 = CARTESIAN_POINT ( 'NONE',  ( 10.54136348144620072, 1452.203475739079749, 208.5677207636399828 ) ) ;
#53054 = CARTESIAN_POINT ( 'NONE',  ( 17.22174733035570071, 1507.619498552399818, 193.9103528060259976 ) ) ;
#53055 = CARTESIAN_POINT ( 'NONE',  ( -76.26096196870000199, 1380.057134384339861, 296.1664118935590295 ) ) ;
#53056 = EDGE_CURVE ( 'NONE', #81697, #49156, #34514, .T. ) ;
#53057 = CARTESIAN_POINT ( 'NONE',  ( -1.102182119232619883E-15, 1378.913060387289988, 209.1218459572589836 ) ) ;
#53058 = VERTEX_POINT ( 'NONE', #22796 ) ;
#53059 = ORIENTED_EDGE ( 'NONE', *, *, #60673, .F. ) ;
#53060 = CARTESIAN_POINT ( 'NONE',  ( 19.18344385319309708, 1507.776479758349979, 229.7058228477820023 ) ) ;
#53061 = CARTESIAN_POINT ( 'NONE',  ( -8.123537375139999739, 1500.423749094890127, 210.2681864885289826 ) ) ;
#53062 = CARTESIAN_POINT ( 'NONE',  ( 12.95237937484257706, 1442.920817661757610, 169.4286732187400162 ) ) ;
#53064 = CARTESIAN_POINT ( 'NONE',  ( -43.50118976839999618, 1440.913060407679950, 263.8966299864979987 ) ) ;
#53063 = CARTESIAN_POINT ( 'NONE',  ( 21.31156959599999823, 1488.809466529329939, 209.1693389662900131 ) ) ;
#53065 = CARTESIAN_POINT ( 'NONE',  ( 9.708065270058002127, 1384.913060387289988, 216.1751682406138571 ) ) ;
#53066 = CARTESIAN_POINT ( 'NONE',  ( -107.7002785469999964, 1382.621911665969947, 297.8537995400589580 ) ) ;
#53067 = EDGE_CURVE ( 'NONE', #43885, #101252, #27067, .T. ) ;
#53068 = CARTESIAN_POINT ( 'NONE',  ( 26.34629031029999879, 1509.610131964929906, 199.6751120872679905 ) ) ;
#53069 = CARTESIAN_POINT ( 'NONE',  ( -20.30769014010000006, 1485.515971530630168, 191.7674218760979841 ) ) ;
#53070 = CARTESIAN_POINT ( 'NONE',  ( 10.06884348340000201, 1409.765578029430117, 188.8671861836979815 ) ) ;
#53071 = CARTESIAN_POINT ( 'NONE',  ( 4.691567311940000096, 1422.090921882629800, 184.7225213113979976 ) ) ;
#53072 = CARTESIAN_POINT ( 'NONE',  ( -1.842962231260000028, 1515.064792882589927, 213.4512947377390049 ) ) ;
#53073 = CARTESIAN_POINT ( 'NONE',  ( 11.23219740039999870, 1436.456445610539959, 151.7916777051979977 ) ) ;
#53074 = CARTESIAN_POINT ( 'NONE',  ( -11.39291980906549995, 1423.225053426399882, 204.2085665321329770 ) ) ;
#53075 = EDGE_CURVE ( 'NONE', #43039, #12262, #7385, .T. ) ;
#53076 = CARTESIAN_POINT ( 'NONE',  ( 0.5968024102800000286, 1507.130435900830207, 237.3073193260979963 ) ) ;
#53077 = CARTESIAN_POINT ( 'NONE',  ( 1.762362329279999917, 1472.996463562990130, 219.1807010226990258 ) ) ;
#53078 = ORIENTED_EDGE ( 'NONE', *, *, #89051, .F. ) ;
#53079 = CARTESIAN_POINT ( 'NONE',  ( -2.387854443607448918, 1426.854124017601634, 138.5187392187245052 ) ) ;
#53080 = CARTESIAN_POINT ( 'NONE',  ( 10.67658260354509991, 1477.918112985820017, 229.9062897255660118 ) ) ;
#53081 = CARTESIAN_POINT ( 'NONE',  ( -39.31037117919999702, 1453.720620610329888, 270.1733326691979755 ) ) ;
#53082 = CARTESIAN_POINT ( 'NONE',  ( -1.693092260590000064, 1443.235800063490160, 218.9922120262189935 ) ) ;
#53083 = CARTESIAN_POINT ( 'NONE',  ( 9.704564366399999642, 1443.913060387330006, 153.0477571643979786 ) ) ;
#53084 = CARTESIAN_POINT ( 'NONE',  ( -14.31351010490000064, 1463.285154408930111, 223.3691465441979744 ) ) ;
#53085 = CARTESIAN_POINT ( 'NONE',  ( 0.9756374909739999879, 1431.113060387329824, 189.4389011961980032 ) ) ;
#53086 = CARTESIAN_POINT ( 'NONE',  ( -4.487358987605787775, 1509.034510030707679, 212.9235704655121424 ) ) ;
#53087 = CARTESIAN_POINT ( 'NONE',  ( 1.519498794560000032, 1507.960421343230109, 236.9808823833980114 ) ) ;
#53088 = CARTESIAN_POINT ( 'NONE',  ( -6.380370694819999855, 1418.306873334029888, 233.0248977636979930 ) ) ;
#53089 = CARTESIAN_POINT ( 'NONE',  ( -9.007784044950000180, 1459.287865364090067, 212.7101983019389877 ) ) ;
#53090 = CARTESIAN_POINT ( 'NONE',  ( -5.180616796779289324, 1359.097496083801843, 208.3718459617010978 ) ) ;
#53091 = CARTESIAN_POINT ( 'NONE',  ( -45.19191529902279569, 1433.651650798640048, 267.0047257956459816 ) ) ;
#53092 = CARTESIAN_POINT ( 'NONE',  ( -3.085511914419999613, 1431.475301411720011, 185.4796394390980083 ) ) ;
#53093 = ORIENTED_EDGE ( 'NONE', *, *, #72638, .F. ) ;
#53094 = CARTESIAN_POINT ( 'NONE',  ( -8.833145283479998611, 1423.402459408220011, 209.4147327117469786 ) ) ;
#53095 = VERTEX_POINT ( 'NONE', #98971 ) ;
#53096 = CARTESIAN_POINT ( 'NONE',  ( -1.701850495234999983, 1516.908147884120126, 210.2591426210370003 ) ) ;
#53097 = CARTESIAN_POINT ( 'NONE',  ( -7.512750246095000861, 1509.038615934159907, 203.6084103740969908 ) ) ;
#53098 = EDGE_CURVE ( 'NONE', #1490, #60256, #61138, .T. ) ;
#53099 = CARTESIAN_POINT ( 'NONE',  ( 15.74021840907683512, 1517.051704408389924, 196.3375305114159062 ) ) ;
#53100 = CARTESIAN_POINT ( 'NONE',  ( 7.158490357027510242, 1426.589113566749802, 213.0788671595350081 ) ) ;
#53101 = CIRCLE ( 'NONE', #42361, 1.000000000000000000 ) ;
#53102 = DIRECTION ( 'NONE',  ( -4.857225732735055447E-14, 0.000000000000000000, 1.000000000000000000 ) ) ;
#53103 = VERTEX_POINT ( 'NONE', #22245 ) ;
#53104 = CARTESIAN_POINT ( 'NONE',  ( -17.21804373259962162, 1410.146604591630194, 225.6635976644989228 ) ) ;
#53106 = DIRECTION ( 'NONE',  ( 0.9125304618754024322, 0.000000000000000000, 0.4090087482554191078 ) ) ;
#53105 = CARTESIAN_POINT ( 'NONE',  ( 3.415238410854999795, 1511.775527460079957, 205.7066075212470082 ) ) ;
#53107 = EDGE_CURVE ( 'NONE', #1407, #26502, #28896, .T. ) ;
#53108 = DIRECTION ( 'NONE',  ( -0.8164965809278529330, 0.5773502691894464300, 0.000000000000000000 ) ) ;
#53109 = CARTESIAN_POINT ( 'NONE',  ( -10.78872034305570082, 1416.913057013679918, 195.9645814724030117 ) ) ;
#53110 = CARTESIAN_POINT ( 'NONE',  ( 5.626793905219999559, 1472.332539098689949, 217.6352975007490045 ) ) ;
#53111 = CARTESIAN_POINT ( 'NONE',  ( -8.768286811978629913, 1439.919956341389934, 206.3771518704159860 ) ) ;
#53112 = VERTEX_POINT ( 'NONE', #39635 ) ;
#53113 = CARTESIAN_POINT ( 'NONE',  ( -22.23813439964190053, 1414.926657347039963, 269.4023535884739999 ) ) ;
#53114 = CARTESIAN_POINT ( 'NONE',  ( 1.701850457105000158, 1516.908147884120126, 207.9845492812970065 ) ) ;
#53115 = CARTESIAN_POINT ( 'NONE',  ( 8.157130779410179500, 1418.866591275500014, 233.1788703964780041 ) ) ;
#53116 = CARTESIAN_POINT ( 'NONE',  ( 8.678482696542719310, 1436.053160561679988, 208.0948695542589917 ) ) ;
#53118 = VERTEX_POINT ( 'NONE', #100621 ) ;
#53117 = CARTESIAN_POINT ( 'NONE',  ( -4.253946116614677919, 1367.780938548775339, 210.6218459617142003 ) ) ;
#53119 = ORIENTED_EDGE ( 'NONE', *, *, #73891, .F. ) ;
#53120 = CARTESIAN_POINT ( 'NONE',  ( -23.37718023422289804, 1410.146351715440005, 210.1164981839299912 ) ) ;
#53121 = CARTESIAN_POINT ( 'NONE',  ( -0.8068904912131519280, 1409.444758023880013, 185.4044988326020302 ) ) ;
#53122 = CARTESIAN_POINT ( 'NONE',  ( 31.23437356469446868, 1512.187213306747481, 222.8968241038843701 ) ) ;
#53123 = CARTESIAN_POINT ( 'NONE',  ( -0.01306565375790010031, 1408.945229229399956, 186.1619460894229974 ) ) ;
#53124 = CIRCLE ( 'NONE', #46014, 2.000000000000002220 ) ;
#53125 = CARTESIAN_POINT ( 'NONE',  ( -18.82790724813750316, 1416.384967866799798, 207.5738806952579978 ) ) ;
#53126 = CARTESIAN_POINT ( 'NONE',  ( -18.55240991700000208, 1425.816903541530110, 225.0696803572979832 ) ) ;
#53127 = CARTESIAN_POINT ( 'NONE',  ( 22.55223415318489799, 1471.819675376130135, 267.0319875137560075 ) ) ;
#53128 = CARTESIAN_POINT ( 'NONE',  ( -8.103600148213331522, 1465.442638966462937, 233.2443155374635069 ) ) ;
#53129 = CARTESIAN_POINT ( 'NONE',  ( -4.987078454525000204, 1508.551704408389924, 209.1218459511669892 ) ) ;
#53130 = CARTESIAN_POINT ( 'NONE',  ( 4.996642160164999957, 1516.697242742309982, 206.2447328616370044 ) ) ;
#53131 = VERTEX_POINT ( 'NONE', #38520 ) ;
#53132 = CARTESIAN_POINT ( 'NONE',  ( -0.05714988119310079884, 1445.012840177589851, 215.4090402065690171 ) ) ;
#53133 = CARTESIAN_POINT ( 'NONE',  ( 1.473482235510590099, 1483.325061647019993, 182.1507347926400087 ) ) ;
#53134 = CARTESIAN_POINT ( 'NONE',  ( 23.60963409220000031, 1410.976028183930111, 207.8292014694679892 ) ) ;
#53135 = ORIENTED_EDGE ( 'NONE', *, *, #108035, .F. ) ;
#53136 = CARTESIAN_POINT ( 'NONE',  ( 4.556906923312060265, 1508.729448375579977, 205.9844555791620166 ) ) ;
#53137 = CARTESIAN_POINT ( 'NONE',  ( 26.08016064264459999, 1451.549772369049833, 136.2273410839000007 ) ) ;
#53138 = CARTESIAN_POINT ( 'NONE',  ( 11.53086876047703058, 1425.452087397813557, 137.7849336002779523 ) ) ;
#53139 = CARTESIAN_POINT ( 'NONE',  ( -6.165516677240000298, 1391.030806526970082, 208.7341617952090189 ) ) ;
#53140 = CARTESIAN_POINT ( 'NONE',  ( -18.63864992402650955, 1509.044553702126677, 230.2784244607928770 ) ) ;
#53141 = CARTESIAN_POINT ( 'NONE',  ( 17.54187789610000081, 1410.889696661429980, 192.7129300596980102 ) ) ;
#53142 = CARTESIAN_POINT ( 'NONE',  ( 20.22153155800000235, 1444.740067931809790, 161.9155394238979966 ) ) ;
#53143 = CARTESIAN_POINT ( 'NONE',  ( 2.618800203428223394, 1439.646264171884695, 183.4501813373113066 ) ) ;
#53145 = CARTESIAN_POINT ( 'NONE',  ( -19.57795677556049796, 1425.757239151944532, 223.2432467385563939 ) ) ;
#53144 = CARTESIAN_POINT ( 'NONE',  ( -3.829620154745601468, 1515.551704408389924, 205.9132087081559064 ) ) ;
#53146 = CARTESIAN_POINT ( 'NONE',  ( 0.6122773730909090162, 1450.961374533219896, 181.9623258240119696 ) ) ;
#53147 = AXIS2_PLACEMENT_3D ( 'NONE', #11289, #104231, #79054 ) ;
#53148 = CARTESIAN_POINT ( 'NONE',  ( 4.329791490734999471, 1515.051704408389924, 205.7917117663469924 ) ) ;
#53149 = CARTESIAN_POINT ( 'NONE',  ( 7.069913306463050162, 1426.666554464499995, 213.2414280066960259 ) ) ;
#53150 = CARTESIAN_POINT ( 'NONE',  ( 4.040527303974999818, 1516.815231249920089, 213.7327841816070020 ) ) ;
#53151 = CARTESIAN_POINT ( 'NONE',  ( 3.351183042480982976, 1524.075000532256581, 242.0172247929413629 ) ) ;
#53152 = ORIENTED_EDGE ( 'NONE', *, *, #75456, .T. ) ;
#53153 = CARTESIAN_POINT ( 'NONE',  ( -3.666694481987490040, 1509.114858341099989, 179.5219341129400163 ) ) ;
#53154 = CARTESIAN_POINT ( 'NONE',  ( 21.38516915558662035, 1522.906561336852974, 237.8497028174188586 ) ) ;
#53155 = CARTESIAN_POINT ( 'NONE',  ( -0.4760850685511259783, 1409.509622399980117, 232.8916950008960214 ) ) ;
#53156 = CARTESIAN_POINT ( 'NONE',  ( 33.93019615848946557, 1522.382868172863937, 197.6607374645996060 ) ) ;
#53157 = FACE_OUTER_BOUND ( 'NONE', #53959, .T. ) ;
#53158 = CARTESIAN_POINT ( 'NONE',  ( -10.79825500028279883, 1462.862626845389968, 206.7546097349500087 ) ) ;
#53159 = CARTESIAN_POINT ( 'NONE',  ( -20.41675336379999806, 1443.170379801809759, 219.6133833292979887 ) ) ;
#53160 = CARTESIAN_POINT ( 'NONE',  ( 28.38725554550000041, 1468.332764320925207, 266.6435172761978833 ) ) ;
#53161 = CARTESIAN_POINT ( 'NONE',  ( -12.31743044086090144, 1378.338386037660030, 209.6284750056420023 ) ) ;
#53162 = CARTESIAN_POINT ( 'NONE',  ( 3.330669073880000049E-15, 1462.614442895030152, 248.0989693021979861 ) ) ;
#53163 = CARTESIAN_POINT ( 'NONE',  ( -10.92059295481699976, 1461.979801184900225, 210.5672364399190144 ) ) ;
#53164 = CARTESIAN_POINT ( 'NONE',  ( 14.43086985023570001, 1426.807458679940282, 195.4949786040619983 ) ) ;
#53165 = CARTESIAN_POINT ( 'NONE',  ( -1.906499758064230099E-08, 1515.051704408389924, 209.1218459511669892 ) ) ;
#53166 = CARTESIAN_POINT ( 'NONE',  ( 9.717826194827521746, 1463.678457587320054, 210.3770332206470073 ) ) ;
#53167 = AXIS2_PLACEMENT_3D ( 'NONE', #100089, #96939, #71773 ) ;
#53168 = DIRECTION ( 'NONE',  ( 0.000000000000000000, 0.000000000000000000, 1.000000000000000000 ) ) ;
#53169 = CARTESIAN_POINT ( 'NONE',  ( -2.273033093151333617, 1525.821544997590763, 240.9339456143065092 ) ) ;
#53170 = CARTESIAN_POINT ( 'NONE',  ( -29.42360915972939850, 1510.018182097579938, 200.5862550365469872 ) ) ;
#53171 = CARTESIAN_POINT ( 'NONE',  ( 24.71942444319999765, 1469.238022045029993, 216.2125151713479738 ) ) ;
#53172 = AXIS2_PLACEMENT_3D ( 'NONE', #26325, #60517, #77853 ) ;
#53173 = CARTESIAN_POINT ( 'NONE',  ( -15.79259793311170057, 1420.293458116122565, 210.0948661461389690 ) ) ;
#53174 = CARTESIAN_POINT ( 'NONE',  ( 30.51231035492521571, 1524.382868172863937, 218.1578534183718432 ) ) ;
#53175 = CARTESIAN_POINT ( 'NONE',  ( -27.96151500746649887, 1383.844585648530028, 225.8420327614329892 ) ) ;
#53176 = CARTESIAN_POINT ( 'NONE',  ( -11.77905465891600123, 1483.168200228759815, 228.2502074522770101 ) ) ;
#53177 = CARTESIAN_POINT ( 'NONE',  ( 2.632631803615880450, 1417.642869435429930, 234.7516633181379859 ) ) ;
#53178 = CARTESIAN_POINT ( 'NONE',  ( 21.62164173326539895, 1519.551704408389924, 208.0273405521070060 ) ) ;
#53179 = CARTESIAN_POINT ( 'NONE',  ( 8.930242950181860095, 1451.533433059749996, 211.6080513519700048 ) ) ;
#53181 = EDGE_LOOP ( 'NONE', ( #22263, #10521, #18545, #7118, #3127, #98174 ) ) ;
#53180 = CARTESIAN_POINT ( 'NONE',  ( 3.346695691219999880, 1443.005063871489938, 217.3642547372890022 ) ) ;
#53182 = CARTESIAN_POINT ( 'NONE',  ( -28.08752589700002744, 1445.052233488288948, 160.7519773376980936 ) ) ;
#53183 = CARTESIAN_POINT ( 'NONE',  ( -9.258223055952665703, 1388.601410234513878, 200.8677487422715728 ) ) ;
#53184 = EDGE_CURVE ( 'NONE', #37255, #109848, #45058, .T. ) ;
#53185 = CARTESIAN_POINT ( 'NONE',  ( -20.34464802829999996, 1507.870840051529967, 189.3862473984979999 ) ) ;
#53187 = ORIENTED_EDGE ( 'NONE', *, *, #94125, .F. ) ;
#53186 = CARTESIAN_POINT ( 'NONE',  ( 32.02808312589922224, 1512.187213306747481, 219.9649204700462235 ) ) ;
#53188 = CARTESIAN_POINT ( 'NONE',  ( -2.158775737652639748, 1508.551704408389924, 220.0625486152149790 ) ) ;
#53189 = EDGE_LOOP ( 'NONE', ( #78593, #109434, #17073, #41854 ) ) ;
#53190 = CARTESIAN_POINT ( 'NONE',  ( -12.29865557582230018, 1392.006777630620036, 209.7412721249799858 ) ) ;
#53191 = CARTESIAN_POINT ( 'NONE',  ( 6.852456351503855458, 1447.063841582483519, 203.1720596810001780 ) ) ;
#53192 = CARTESIAN_POINT ( 'NONE',  ( 11.44665326297827335, 1425.798162341591706, 139.1345266541928538 ) ) ;
#53193 = CARTESIAN_POINT ( 'NONE',  ( -2.867396511858420372, 1368.019296321386491, 208.2077839524759781 ) ) ;
#53194 = CARTESIAN_POINT ( 'NONE',  ( 0.2196276506829989983, 1429.899695672290136, 217.4576539075590063 ) ) ;
#53195 = B_SPLINE_CURVE_WITH_KNOTS ( 'NONE', 5,
 ( #73665, #22100, #20460, #46273, #29425, #12638 ),
 .UNSPECIFIED., .F., .F.,
 ( 6, 6 ),
 ( 0.000000000000000000, 1.000000000000000000 ),
 .UNSPECIFIED. ) ;
#53196 = CARTESIAN_POINT ( 'NONE',  ( -10.43378839784119982, 1471.950490389920105, 207.0189331983069962 ) ) ;
#53197 = AXIS2_PLACEMENT_3D ( 'NONE', #66530, #23920, #91695 ) ;
#53198 = CARTESIAN_POINT ( 'NONE',  ( 14.34357294504789948, 1409.413948991840016, 204.9548362799079939 ) ) ;
#53199 = CARTESIAN_POINT ( 'NONE',  ( -12.06041275870000185, 1391.852782912460043, 208.2296565975740066 ) ) ;
#53200 = CARTESIAN_POINT ( 'NONE',  ( -94.11294163072489027, 1385.205045773489928, 294.6186134169249726 ) ) ;
#53201 = CARTESIAN_POINT ( 'NONE',  ( -17.93337622780000373, 1421.490724472430202, 193.1272588093980289 ) ) ;
#53202 = CARTESIAN_POINT ( 'NONE',  ( -32.85805783624314813, 1523.678648413191695, 201.0453875934059340 ) ) ;
#53203 = EDGE_LOOP ( 'NONE', ( #95379, #42300, #96185, #76965 ) ) ;
#53204 = CARTESIAN_POINT ( 'NONE',  ( 11.59720850580749918, 1491.204161894499975, 206.7870309651650018 ) ) ;
#53205 = ADVANCED_FACE ( 'NONE', ( #46956 ), #57597, .F. ) ;
#53207 = ORIENTED_EDGE ( 'NONE', *, *, #34372, .F. ) ;
#53206 = DIRECTION ( 'NONE',  ( 0.000000000000000000, 0.000000000000000000, 1.000000000000000000 ) ) ;
#53208 = CARTESIAN_POINT ( 'NONE',  ( 17.04532911661896932, 1522.051704408389924, 221.2898363890541589 ) ) ;
#53209 = EDGE_LOOP ( 'NONE', ( #60153, #56219, #99539, #38639 ) ) ;
#53210 = LINE ( 'NONE', #85678, #80169 ) ;
#53211 = CARTESIAN_POINT ( 'NONE',  ( -4.745098151936928410, 1360.923919868569783, 210.6218459616987957 ) ) ;
#53212 = CARTESIAN_POINT ( 'NONE',  ( -11.90604050199999975, 1433.732568523099872, 150.6972470776979947 ) ) ;
#53213 = B_SPLINE_CURVE_WITH_KNOTS ( 'NONE', 5,
 ( #46285, #80413, #72568, #99944, #39508, #100507, #38392, #108364, #4787 ),
 .UNSPECIFIED., .F., .F.,
 ( 6, 3, 6 ),
 ( 0.000000000000000000, 0.4797001321658070916, 1.000000000000000000 ),
 .UNSPECIFIED. ) ;
#53214 = EDGE_CURVE ( 'NONE', #22220, #8434, #53949, .T. ) ;
#53215 = CARTESIAN_POINT ( 'NONE',  ( 16.23342327852422429, 1469.050322811229080, 269.3700830507254409 ) ) ;
#53216 = CARTESIAN_POINT ( 'NONE',  ( 12.37353479079889951, 1427.152528082410072, 207.0190610342110062 ) ) ;
#53217 = CARTESIAN_POINT ( 'NONE',  ( 2.290107552079999831, 1395.993032705530140, 220.3039202953980009 ) ) ;
#53218 = CARTESIAN_POINT ( 'NONE',  ( 1.789086269730000067, 1417.552112839030087, 233.6888163188979775 ) ) ;
#53219 = CARTESIAN_POINT ( 'NONE',  ( -9.225907677606096868, 1522.051704408389924, 219.6631043460218393 ) ) ;
#53220 = CARTESIAN_POINT ( 'NONE',  ( -19.59053950279439960, 1486.265866315750145, 189.8955481462990065 ) ) ;
#53221 = CARTESIAN_POINT ( 'NONE',  ( -3.978066776185401388, 1370.279108416835925, 210.6218459617030021 ) ) ;
#53222 = CARTESIAN_POINT ( 'NONE',  ( -26.55481977066866861, 1436.735068348699770, 136.8009166751634211 ) ) ;
#53223 = CARTESIAN_POINT ( 'NONE',  ( 20.61542114513792257, 1508.364347661922238, 227.6602567161955051 ) ) ;
#53224 = CARTESIAN_POINT ( 'NONE',  ( 0.7351097711180020200, 1516.977504706749869, 206.6301902066870184 ) ) ;
#53225 = AXIS2_PLACEMENT_3D ( 'NONE', #69716, #34967, #51788 ) ;
#53226 = CARTESIAN_POINT ( 'NONE',  ( -0.5656601614563600000, 1424.194575819369902, 228.0927458373740251 ) ) ;
#53227 = LINE ( 'NONE', #59974, #90585 ) ;
#53228 = CARTESIAN_POINT ( 'NONE',  ( -0.3690012737985599589, 1443.315611438030146, 189.9060334618889954 ) ) ;
#53230 = ORIENTED_EDGE ( 'NONE', *, *, #88332, .T. ) ;
#53229 = CARTESIAN_POINT ( 'NONE',  ( -1.228179860600000062, 1495.213118903489885, 220.2649180232990034 ) ) ;
#53231 = FACE_OUTER_BOUND ( 'NONE', #99987, .T. ) ;
#53232 = ORIENTED_EDGE ( 'NONE', *, *, #70043, .T. ) ;
#53233 = CARTESIAN_POINT ( 'NONE',  ( 42.47347430450000161, 1432.913525160240169, 263.9447136157980367 ) ) ;
#53234 = CARTESIAN_POINT ( 'NONE',  ( -26.60955424449999995, 1469.249567707230199, 208.9444902198429759 ) ) ;
#53236 = CARTESIAN_POINT ( 'NONE',  ( 16.63867649748380018, 1409.594336716910220, 192.8496594819030179 ) ) ;
#53235 = CARTESIAN_POINT ( 'NONE',  ( -11.00605453490000052, 1426.944684141429889, 91.15820994169789060 ) ) ;
#53237 = CARTESIAN_POINT ( 'NONE',  ( 6.949574947644999945, 1517.102359858469754, 212.3809477691169718 ) ) ;
#53238 = EDGE_CURVE ( 'NONE', #15989, #107938, #36060, .T. ) ;
#53239 = CARTESIAN_POINT ( 'NONE',  ( 3.321478032336870001, 1396.029048956019778, 198.6099121833759966 ) ) ;
#53240 = CYLINDRICAL_SURFACE ( 'NONE', #108867, 2.000000000000003109 ) ;
#53241 = CARTESIAN_POINT ( 'NONE',  ( -27.17992431780000118, 1424.801532950129968, 248.2870168944980094 ) ) ;
#53242 = CARTESIAN_POINT ( 'NONE',  ( -14.01094583181789943, 1379.700363488999983, 208.2836208941100153 ) ) ;
#53243 = CARTESIAN_POINT ( 'NONE',  ( 28.27864386421530085, 1508.411229478540008, 209.3995008269750144 ) ) ;
#53244 = CARTESIAN_POINT ( 'NONE',  ( 3.012478497202149885, 1508.551704408389924, 214.0547362871380130 ) ) ;
#53245 = CARTESIAN_POINT ( 'NONE',  ( 33.14188593189999921, 1451.755856666429963, 135.1722003460979806 ) ) ;
#53246 = ORIENTED_EDGE ( 'NONE', *, *, #96434, .F. ) ;
#53247 = CARTESIAN_POINT ( 'NONE',  ( 6.232524879136110307, 1398.098455824979965, 220.5304231573819891 ) ) ;
#53248 = CARTESIAN_POINT ( 'NONE',  ( 10.88300501365269923, 1460.705383129390157, 207.9797520299849793 ) ) ;
#53249 = CARTESIAN_POINT ( 'NONE',  ( -16.16332356590000074, 1459.159536845130106, 229.6201735760980114 ) ) ;
#53250 = ORIENTED_EDGE ( 'NONE', *, *, #1467, .F. ) ;
#53251 = ORIENTED_EDGE ( 'NONE', *, *, #106862, .F. ) ;
#53252 = CIRCLE ( 'NONE', #74746, 33.13701971169416538 ) ;
#53253 = CARTESIAN_POINT ( 'NONE',  ( 9.772779914185960592, 1453.284091914029887, 211.9285179305149995 ) ) ;
#53254 = CARTESIAN_POINT ( 'NONE',  ( 9.147586507279999779, 1424.572281473970179, 196.5102056844989704 ) ) ;
#53255 = ORIENTED_EDGE ( 'NONE', *, *, #2239, .T. ) ;
#53256 = CARTESIAN_POINT ( 'NONE',  ( -1.356502621700000022, 1410.320696896230174, 185.6044186391980020 ) ) ;
#53257 = CARTESIAN_POINT ( 'NONE',  ( -6.910430994591643561, 1419.227950353617871, 195.3558243408897681 ) ) ;
#53258 = DIRECTION ( 'NONE',  ( -0.8907681516580484571, 1.273087901431153894E-31, 0.4544580288560254311 ) ) ;
#53259 = CIRCLE ( 'NONE', #78253, 1.999999999999999556 ) ;
#53260 = CARTESIAN_POINT ( 'NONE',  ( -6.614451065750000858, 1470.478371390330040, 234.0809738164980160 ) ) ;
#53261 = CARTESIAN_POINT ( 'NONE',  ( 0.4486526232410890103, 1420.573293467059784, 182.8046371172480065 ) ) ;
#53262 = VECTOR ( 'NONE', #37642, 1000.000000000000000 ) ;
#53263 = CARTESIAN_POINT ( 'NONE',  ( 9.394917065999061734, 1451.852087569300011, 209.9058690040849910 ) ) ;
#53264 = CARTESIAN_POINT ( 'NONE',  ( -4.247299066680000124, 1502.738124400289962, 230.1067396463990065 ) ) ;
#53265 = CARTESIAN_POINT ( 'NONE',  ( 14.57526300359999993, 1474.749940818629966, 224.7313656968979956 ) ) ;
#53266 = EDGE_LOOP ( 'NONE', ( #77636, #72222, #75992, #74034 ) ) ;
#53267 = CARTESIAN_POINT ( 'NONE',  ( 6.940473334145000450, 1516.833525648419936, 202.5658237375970145 ) ) ;
#53268 = CARTESIAN_POINT ( 'NONE',  ( -4.997718276504999224, 1516.693851263360102, 210.2547950466569944 ) ) ;
#53269 = ORIENTED_EDGE ( 'NONE', *, *, #7195, .T. ) ;
#53270 = CARTESIAN_POINT ( 'NONE',  ( 11.85935220418699920, 1431.865067821940102, 149.9620054296389924 ) ) ;
#53271 = CARTESIAN_POINT ( 'NONE',  ( 12.64036215934078022, 1445.032014182524335, 186.2682781246677166 ) ) ;
#53272 = ORIENTED_EDGE ( 'NONE', *, *, #97593, .T. ) ;
#53273 = CARTESIAN_POINT ( 'NONE',  ( -15.62326149431152089, 1506.535970900717984, 193.5355000223906075 ) ) ;
#53274 = CARTESIAN_POINT ( 'NONE',  ( -13.35741048202589809, 1443.501467202830099, 164.9741927960640453 ) ) ;
#53275 = CARTESIAN_POINT ( 'NONE',  ( 9.021136374670000180, 1508.721785377329979, 235.3723347276979894 ) ) ;
#53276 = CARTESIAN_POINT ( 'NONE',  ( -10.54306353004690067, 1469.936069848170064, 213.3750816242119868 ) ) ;
#53277 = CARTESIAN_POINT ( 'NONE',  ( -4.789983303610000576, 1423.864849667030057, 185.3823132089979993 ) ) ;
#53278 = CARTESIAN_POINT ( 'NONE',  ( 3.565775598909999733, 1407.753784349630223, 270.1349117941979898 ) ) ;
#53279 = DIRECTION ( 'NONE',  ( 0.9900965937346509760, 0.1403878024439500216, 3.790652827686680047E-16 ) ) ;
#53280 = CARTESIAN_POINT ( 'NONE',  ( -109.7922251892066043, 1383.411727247472299, 297.1256090396871627 ) ) ;
#53281 = CARTESIAN_POINT ( 'NONE',  ( 10.03804068110000003, 1493.022037044190029, 214.8448302025189776 ) ) ;
#53282 = CARTESIAN_POINT ( 'NONE',  ( -21.19337473369999714, 1379.596559222110045, 209.5042946936439989 ) ) ;
#53283 = CARTESIAN_POINT ( 'NONE',  ( 9.331170596321376465, 1425.274930616336405, 195.5633789865317453 ) ) ;
#53285 = CARTESIAN_POINT ( 'NONE',  ( 11.13973213087689906, 1470.272412021129867, 206.9146623043149873 ) ) ;
#53284 = CARTESIAN_POINT ( 'NONE',  ( -17.68441402020000197, 1504.382480553090090, 209.0725129034710221 ) ) ;
#53286 = CARTESIAN_POINT ( 'NONE',  ( -3.249999999999999556, 1524.551704408390151, 209.1218459616989946 ) ) ;
#53287 = AXIS2_PLACEMENT_3D ( 'NONE', #17738, #10482, #19416 ) ;
#53288 = CARTESIAN_POINT ( 'NONE',  ( 17.91313270363389876, 1420.835020208859987, 225.0974074490680152 ) ) ;
#53289 = CARTESIAN_POINT ( 'NONE',  ( -6.262845595265000398, 1511.198876514819858, 201.6723168475869841 ) ) ;
#53290 = ORIENTED_EDGE ( 'NONE', *, *, #6388, .T. ) ;
#53291 = CARTESIAN_POINT ( 'NONE',  ( 12.85916294189999931, 1411.892799971530167, 268.3665355204980187 ) ) ;
#53292 = CARTESIAN_POINT ( 'NONE',  ( -3.451191875628176753, 1523.678648413191695, 175.1707361340005207 ) ) ;
#53293 = CARTESIAN_POINT ( 'NONE',  ( 40.96765513241462742, 1447.290458505206743, 135.1834236911112441 ) ) ;
#53294 = CARTESIAN_POINT ( 'NONE',  ( 3.838475640130000421, 1505.530984303090008, 221.3004008607989874 ) ) ;
#53295 = FACE_OUTER_BOUND ( 'NONE', #32510, .T. ) ;
#53297 = VERTEX_POINT ( 'NONE', #9197 ) ;
#53296 = CARTESIAN_POINT ( 'NONE',  ( 1.201530806705199961, 1515.093215458460008, 204.7931414570770130 ) ) ;
#53298 = CARTESIAN_POINT ( 'NONE',  ( -15.77498267344473071, 1415.804408449163247, 209.6953390818695198 ) ) ;
#53299 = CARTESIAN_POINT ( 'NONE',  ( -10.18374426391977039, 1473.001081400295334, 208.1334165208762386 ) ) ;
#53300 = CARTESIAN_POINT ( 'NONE',  ( -15.94270011119999708, 1416.079343365249997, 209.7066342856829806 ) ) ;
#53301 = CARTESIAN_POINT ( 'NONE',  ( -6.375523666339999451, 1460.280735373489961, 210.0338255622669976 ) ) ;
#53302 = DIRECTION ( 'NONE',  ( 0.7054602837376293678, -3.121166767548191889E-15, -0.7087494536638624387 ) ) ;
#53303 = CARTESIAN_POINT ( 'NONE',  ( 5.370527602886283169, 1422.356908813907012, 139.1416118586824666 ) ) ;
#53304 = CARTESIAN_POINT ( 'NONE',  ( 30.54334960032450041, 1509.992611366529900, 207.3226989945189871 ) ) ;
#53305 = CARTESIAN_POINT ( 'NONE',  ( 13.33986755048250039, 1429.041205739520137, 222.0838351576450123 ) ) ;
#53306 = CARTESIAN_POINT ( 'NONE',  ( -4.360582346120001063, 1431.113060387329824, 227.9437648745980027 ) ) ;
#53307 = CARTESIAN_POINT ( 'NONE',  ( 16.18846431829999943, 1410.409213254730048, 226.7751941885980216 ) ) ;
#53308 = CARTESIAN_POINT ( 'NONE',  ( 9.982819585849640021, 1469.474122878060143, 210.3108196173600106 ) ) ;
#53310 = CARTESIAN_POINT ( 'NONE',  ( -16.62342269400000205, 1460.779327316729905, 228.2681772136979816 ) ) ;
#53309 = AXIS2_PLACEMENT_3D ( 'NONE', #28123, #103154, #94208 ) ;
#53311 = CARTESIAN_POINT ( 'NONE',  ( -2.299656354225000143, 1516.843453247299749, 206.6453952679669896 ) ) ;
#53312 = CARTESIAN_POINT ( 'NONE',  ( 39.02011237019999612, 1422.796720904130098, 269.1561393349979880 ) ) ;
#53313 = CARTESIAN_POINT ( 'NONE',  ( -30.51231035492510557, 1526.382868172863937, 218.1578534183722979 ) ) ;
#53314 = CARTESIAN_POINT ( 'NONE',  ( 15.43924878589999850, 1436.272480559940050, 149.3456521445980059 ) ) ;
#53315 = CARTESIAN_POINT ( 'NONE',  ( 21.03034198799999999, 1488.584892799430008, 192.0921482354980014 ) ) ;
#53316 = CARTESIAN_POINT ( 'NONE',  ( -21.08953343030000127, 1428.992258108429951, 221.5629153413979964 ) ) ;
#53317 = CARTESIAN_POINT ( 'NONE',  ( -12.33253358726570070, 1378.517501885649835, 208.8148673690130011 ) ) ;
#53318 = CARTESIAN_POINT ( 'NONE',  ( -7.055157488669999921, 1475.427864936029891, 266.9413125670979525 ) ) ;
#53319 = CARTESIAN_POINT ( 'NONE',  ( -11.38916143032739825, 1500.505134839040011, 209.9622123043970134 ) ) ;
#53320 = CARTESIAN_POINT ( 'NONE',  ( -41.49265034658910167, 1443.149328808269956, 136.5063902170460040 ) ) ;
#53321 = CARTESIAN_POINT ( 'NONE',  ( -20.13566255811392480, 1506.560172253814471, 200.0397955187486048 ) ) ;
#53322 = CARTESIAN_POINT ( 'NONE',  ( -15.88926427640000050, 1416.064503262980224, 209.5444336918569945 ) ) ;
#53323 = CARTESIAN_POINT ( 'NONE',  ( -12.68686629940000010, 1442.617705476030096, 187.1386741737979946 ) ) ;
#53324 = CARTESIAN_POINT ( 'NONE',  ( -33.14721542679999544, 1436.549951028310034, 136.5342324578980140 ) ) ;
#53325 = DIRECTION ( 'NONE',  ( 1.755985294532464991E-16, -1.000000000000000000, 1.338183447452830017E-16 ) ) ;
#53326 = ORIENTED_EDGE ( 'NONE', *, *, #24716, .F. ) ;
#53327 = CARTESIAN_POINT ( 'NONE',  ( 5.761500013727863134, 1510.554407338701822, 216.6633153120424424 ) ) ;
#53328 = CARTESIAN_POINT ( 'NONE',  ( -13.55472914751489988, 1409.386401959430032, 215.4052957893119924 ) ) ;
#53329 = AXIS2_PLACEMENT_3D ( 'NONE', #95428, #78067, #51213 ) ;
#53330 = CARTESIAN_POINT ( 'NONE',  ( -2.478067412690000193, 1440.020830691129959, 157.7869724642980032 ) ) ;
#53331 = CARTESIAN_POINT ( 'NONE',  ( -21.13431252044160047, 1409.651086843229905, 211.8287216663260040 ) ) ;
#53332 = CARTESIAN_POINT ( 'NONE',  ( -45.85460265660000800, 1445.993250122450036, 268.7562748562979777 ) ) ;
#53333 = CARTESIAN_POINT ( 'NONE',  ( -11.82991541994420004, 1481.593101321090217, 209.9800737738590044 ) ) ;
#53334 = AXIS2_PLACEMENT_3D ( 'NONE', #4834, #107303, #30596 ) ;
#53335 = CARTESIAN_POINT ( 'NONE',  ( 0.1715103366868419854, 1420.360261608449946, 183.3974109806000001 ) ) ;
#53336 = CARTESIAN_POINT ( 'NONE',  ( -26.91031503490000176, 1509.852789295929824, 218.7452626102079876 ) ) ;
#53337 = CARTESIAN_POINT ( 'NONE',  ( -77.49021889145849684, 1384.643977683190087, 302.0747173313980056 ) ) ;
#53338 = CARTESIAN_POINT ( 'NONE',  ( -44.91689487631180100, 1385.002850385320016, 218.2146715890750102 ) ) ;
#53339 = CARTESIAN_POINT ( 'NONE',  ( 17.33879185520300226, 1422.603306420210174, 226.6220729339370052 ) ) ;
#53340 = CARTESIAN_POINT ( 'NONE',  ( 20.61548266710000021, 1508.365537841329797, 227.7135694462980098 ) ) ;
#53341 = AXIS2_PLACEMENT_3D ( 'NONE', #67777, #92953, #8947 ) ;
#53342 = CARTESIAN_POINT ( 'NONE',  ( 3.552713678799999608E-15, 1432.353292893639946, 155.3998094795979910 ) ) ;
#53343 = CARTESIAN_POINT ( 'NONE',  ( 5.161277877375379575, 1424.205378946189967, 193.2953230041809718 ) ) ;
#53344 = CARTESIAN_POINT ( 'NONE',  ( 4.329448786299999519, 1515.064792490889886, 207.2788827064790098 ) ) ;
#53345 = CARTESIAN_POINT ( 'NONE',  ( -7.965967244980000750, 1384.921491711900217, 199.4892246039989914 ) ) ;
#53346 = VECTOR ( 'NONE', #34810, 1000.000000000000000 ) ;
#53347 = CARTESIAN_POINT ( 'NONE',  ( 19.53786426059019021, 1512.187213306747481, 180.5239794925693388 ) ) ;
#53348 =( BOUNDED_SURFACE ( )  B_SPLINE_SURFACE ( 1, 2, ( 
 ( #17244, #1056, #66610 ),
 ( #32964, #33504, #67705 ) ),
 .UNSPECIFIED., .F., .F., .F. ) 
 B_SPLINE_SURFACE_WITH_KNOTS ( ( 2, 2 ),
 ( 3, 3 ),
 ( -10000.00000000000000, 10000.00000000000000 ),
 ( 5.300753508068379638, 6.148747966334259907 ),
 .UNSPECIFIED. ) 
 GEOMETRIC_REPRESENTATION_ITEM ( )  RATIONAL_B_SPLINE_SURFACE ( (
 ( 0.8627701935022110691, 0.8231028658330309389, 0.9541560038134260235),
 ( 0.8627701935022110691, 0.8231028658330309389, 0.9541560038134260235) ) ) 
 REPRESENTATION_ITEM ( '' )  SURFACE ( )  );
#53349 = CARTESIAN_POINT ( 'NONE',  ( 16.63199911499999928, 1416.518938591829965, 201.3741761614680001 ) ) ;
#53350 = CARTESIAN_POINT ( 'NONE',  ( -16.16632277704816900, 1512.187213306747481, 181.3470724465437627 ) ) ;
#53351 = CARTESIAN_POINT ( 'NONE',  ( 10.50536461352409923, 1481.125266294730181, 208.0189701215730054 ) ) ;
#53352 = CARTESIAN_POINT ( 'NONE',  ( 23.68159507920000095, 1410.235400666329951, 210.4508981972280139 ) ) ;
#53353 = CARTESIAN_POINT ( 'NONE',  ( -106.9545585610730001, 1391.913060387289988, 306.5861216815010266 ) ) ;
#53354 = CARTESIAN_POINT ( 'NONE',  ( 7.755360837189519962, 1459.738753866829938, 228.9106046784149839 ) ) ;
#53355 = CARTESIAN_POINT ( 'NONE',  ( -15.56072141409999965, 1422.731526910729826, 229.1456929959980187 ) ) ;
#53357 = CARTESIAN_POINT ( 'NONE',  ( -8.108123535929999903, 1383.554056671639955, 199.6539754186189839 ) ) ;
#53356 = CARTESIAN_POINT ( 'NONE',  ( -11.86937547910000035, 1432.581147039740017, 149.9818613170979802 ) ) ;
#53358 = CARTESIAN_POINT ( 'NONE',  ( 0.7119424177869999593, 1411.661590166830138, 233.1969697336979834 ) ) ;
#53359 = CARTESIAN_POINT ( 'NONE',  ( -124.7066708634027208, 1371.894749952188477, 298.0449835127481037 ) ) ;
#53360 = CARTESIAN_POINT ( 'NONE',  ( -10.97106033540000070, 1491.549773342590015, 210.1503302054390190 ) ) ;
#53361 = LINE ( 'NONE', #80199, #53262 ) ;
#53362 = CARTESIAN_POINT ( 'NONE',  ( -9.351945459730000465, 1366.519103298159962, 210.6218459616991936 ) ) ;
#53363 = CARTESIAN_POINT ( 'NONE',  ( 3.449149195745000007, 1516.947419719950176, 204.4980579627370219 ) ) ;
#53364 = AXIS2_PLACEMENT_3D ( 'NONE', #82668, #14339, #57487 ) ;
#53365 = CARTESIAN_POINT ( 'NONE',  ( -19.61843130789999989, 1426.543110900729744, 225.3457329349979830 ) ) ;
#53366 = DIRECTION ( 'NONE',  ( -0.5877852522924820189, 0.000000000000000000, -0.8090169943749410120 ) ) ;
#53367 =( NAMED_UNIT ( * ) SI_UNIT ( $, .STERADIAN. ) SOLID_ANGLE_UNIT ( ) );
#53368 = CARTESIAN_POINT ( 'NONE',  ( -9.200421138165051360, 1422.937291722789951, 210.7384568321920142 ) ) ;
#53370 = VERTEX_POINT ( 'NONE', #69120 ) ;
#53369 = CARTESIAN_POINT ( 'NONE',  ( -66.93736618710819641, 1379.743976683229903, 277.9760783128850221 ) ) ;
#53371 = ORIENTED_EDGE ( 'NONE', *, *, #84635, .F. ) ;
#53372 = CARTESIAN_POINT ( 'NONE',  ( 11.81528372083669964, 1433.677274197049883, 150.7650281621870079 ) ) ;
#53373 = CARTESIAN_POINT ( 'NONE',  ( 21.08704007906474942, 1525.317349363550420, 184.4717524171098546 ) ) ;
#53374 = ORIENTED_EDGE ( 'NONE', *, *, #54196, .F. ) ;
#53375 = CARTESIAN_POINT ( 'NONE',  ( -11.75869035857540013, 1517.151704408390060, 190.9442076533970010 ) ) ;
#53376 = CARTESIAN_POINT ( 'NONE',  ( 11.01047161400000007, 1501.676453312990134, 205.9410319520989674 ) ) ;
#53378 = CARTESIAN_POINT ( 'NONE',  ( 0.2916220566639999845, 1508.974498516630092, 179.3904948502979835 ) ) ;
#53377 = CARTESIAN_POINT ( 'NONE',  ( 17.63154828746949931, 1477.220527230660082, 189.4679263864980214 ) ) ;
#53379 = CARTESIAN_POINT ( 'NONE',  ( 2.601659696316710235, 1468.435074765370018, 215.8528558269860298 ) ) ;
#53380 = CARTESIAN_POINT ( 'NONE',  ( 0.7726025625319999923, 1488.176002970830268, 181.8096760246980068 ) ) ;
#53381 = CARTESIAN_POINT ( 'NONE',  ( -105.9085581613829845, 1378.913060388459826, 305.0251771309630158 ) ) ;
#53382 = CARTESIAN_POINT ( 'NONE',  ( -24.47690167607559886, 1444.776640416369901, 211.0359720841289857 ) ) ;
#53383 = CARTESIAN_POINT ( 'NONE',  ( -6.935133418554999096, 1516.613881697390070, 212.3834819030570031 ) ) ;
#53384 = CARTESIAN_POINT ( 'NONE',  ( 35.72409870452920444, 1435.953719464650021, 134.0999999973689967 ) ) ;
#53385 = CARTESIAN_POINT ( 'NONE',  ( -4.646147438016499542, 1378.399971910029990, 214.5514622210689879 ) ) ;
#53386 = DIRECTION ( 'NONE',  ( 6.332794898383918850E-17, 1.000000000000000000, -8.716344404180429969E-17 ) ) ;
#53387 = VERTEX_POINT ( 'NONE', #78605 ) ;
#53388 = CARTESIAN_POINT ( 'NONE',  ( 14.37148033386480073, 1435.528465542959793, 149.6149653547480227 ) ) ;
#53389 = CARTESIAN_POINT ( 'NONE',  ( 0.8791306092667371397, 1432.688050419320007, 200.7222455119930089 ) ) ;
#53390 = ORIENTED_EDGE ( 'NONE', *, *, #5680, .F. ) ;
#53391 = VERTEX_POINT ( 'NONE', #76955 ) ;
#53392 = ORIENTED_EDGE ( 'NONE', *, *, #21579, .T. ) ;
#53393 = CARTESIAN_POINT ( 'NONE',  ( 12.68761320032887774, 1445.019507500634973, 169.4610301561137646 ) ) ;
#53394 = LINE ( 'NONE', #68542, #84905 ) ;
#53395 = CARTESIAN_POINT ( 'NONE',  ( 7.061178118806066273, 1451.421219515312714, 153.2201617045464559 ) ) ;
#53396 = CARTESIAN_POINT ( 'NONE',  ( -7.769230765519999693, 1384.924143725650083, 218.9178332174689956 ) ) ;
#53397 = CARTESIAN_POINT ( 'NONE',  ( 1.665089994623440095, 1465.819159950360017, 198.2247081585720139 ) ) ;
#53398 = CARTESIAN_POINT ( 'NONE',  ( -18.63793804202000004, 1508.544021955199923, 210.2772651711879917 ) ) ;
#53399 = CARTESIAN_POINT ( 'NONE',  ( -53.93365159477244219, 1379.703206717382272, 247.7545238405864438 ) ) ;
#53400 = CARTESIAN_POINT ( 'NONE',  ( 4.240698138573309350, 1446.387872175620032, 162.7199821555450114 ) ) ;
#53401 = CARTESIAN_POINT ( 'NONE',  ( 8.602499828956750250, 1437.170389814990131, 208.2906584274039972 ) ) ;
#53402 = VERTEX_POINT ( 'NONE', #26531 ) ;
#53403 = CARTESIAN_POINT ( 'NONE',  ( 1.700706776364999895, 1516.923170579120097, 206.8211163054370161 ) ) ;
#53404 = ORIENTED_EDGE ( 'NONE', *, *, #32949, .F. ) ;
#53405 = CARTESIAN_POINT ( 'NONE',  ( 30.22378019458900056, 1440.913060387330006, 252.5570269051040100 ) ) ;
#53406 = CARTESIAN_POINT ( 'NONE',  ( -20.01701400349999815, 1508.375006160530120, 188.9474772183980065 ) ) ;
#53407 = VERTEX_POINT ( 'NONE', #60727 ) ;
#53408 = CARTESIAN_POINT ( 'NONE',  ( 25.71410359372319832, 1448.114898661300003, 138.0507843406130064 ) ) ;
#53409 = CARTESIAN_POINT ( 'NONE',  ( -13.57875502439999948, 1410.319880166030089, 190.0093725944979894 ) ) ;
#53410 = CARTESIAN_POINT ( 'NONE',  ( -59.34479193474174963, 1379.724027908502649, 264.5115275510683546 ) ) ;
#53412 = CARTESIAN_POINT ( 'NONE',  ( 15.15436960869729965, 1512.305164330070056, 196.2951117818919897 ) ) ;
#53411 = CARTESIAN_POINT ( 'NONE',  ( -24.36454078510000087, 1441.184224637150010, 211.6994343379179782 ) ) ;
#53413 = CARTESIAN_POINT ( 'NONE',  ( -10.79382126600000014, 1414.913060387329779, 196.1395803457980094 ) ) ;
#53414 = CARTESIAN_POINT ( 'NONE',  ( 3.512785867830420180E-12, 1395.913060387330006, 198.1220674046479928 ) ) ;
#53415 = CARTESIAN_POINT ( 'NONE',  ( -13.57096693066059245, 1434.971412459564817, 146.5999775064138078 ) ) ;
#53416 = CARTESIAN_POINT ( 'NONE',  ( -13.50087351860000062, 1434.968964114900245, 149.2725308732979954 ) ) ;
#53417 = CARTESIAN_POINT ( 'NONE',  ( -6.569523906889999765, 1508.426336951290068, 219.8379881403990055 ) ) ;
#53419 = CARTESIAN_POINT ( 'NONE',  ( 5.532282641970000192, 1438.101548169890066, 209.4569669644060355 ) ) ;
#53418 = CARTESIAN_POINT ( 'NONE',  ( -0.8350686643532190256, 1526.382868172863937, 240.9330574173806951 ) ) ;
#53420 = B_SPLINE_CURVE_WITH_KNOTS ( 'NONE', 3,
 ( #100655, #73836, #39668, #40214, #14990, #40765, #81646 ),
 .UNSPECIFIED., .F., .F.,
 ( 4, 3, 4 ),
 ( -157.3797848890000068, -135.2383462476790044, -79.35007823249820547 ),
 .UNSPECIFIED. ) ;
#53421 = AXIS2_PLACEMENT_3D ( 'NONE', #81975, #32140, #14779 ) ;
#53422 = CARTESIAN_POINT ( 'NONE',  ( 3.263521904354999670, 1516.676340709600026, 214.8942497445370066 ) ) ;
#53423 = VECTOR ( 'NONE', #48693, 1000.000000000000000 ) ;
#53424 = CARTESIAN_POINT ( 'NONE',  ( -31.41104781486814090, 1511.187213306747708, 215.9140555522426723 ) ) ;
#53425 = DIRECTION ( 'NONE',  ( 4.440892098500004934E-16, 1.000000000000000000, -1.817990202819999994E-15 ) ) ;
#53426 = VECTOR ( 'NONE', #48885, 1000.000000000000114 ) ;
#53428 = EDGE_CURVE ( 'NONE', #101252, #101260, #43358, .T. ) ;
#53427 = CARTESIAN_POINT ( 'NONE',  ( 29.74048404330000039, 1509.991911966430052, 208.2083000408450175 ) ) ;
#53429 = CARTESIAN_POINT ( 'NONE',  ( 0.01328393942530149870, 1516.939580991450157, 212.3834982571270018 ) ) ;
#53430 = EDGE_CURVE ( 'NONE', #5750, #39868, #42242, .T. ) ;
#53431 = CARTESIAN_POINT ( 'NONE',  ( -20.60842128280000196, 1470.808655613029941, 208.9538791287869799 ) ) ;
#53432 = CARTESIAN_POINT ( 'NONE',  ( -15.48476762197763712, 1486.079411782601710, 186.6377642270500132 ) ) ;
#53434 = ORIENTED_EDGE ( 'NONE', *, *, #59412, .T. ) ;
#53433 = CARTESIAN_POINT ( 'NONE',  ( -88.00931505469999649, 1389.318458636940022, 305.2260502545590271 ) ) ;
#53435 = CARTESIAN_POINT ( 'NONE',  ( -1.052431931479999916, 1415.163755984229965, 226.8636908286979974 ) ) ;
#53436 = B_SPLINE_CURVE_WITH_KNOTS ( 'NONE', 3,
 ( #77511, #103229, #26539, #27655, #61841, #19222, #87576, #55086, #108210, #14143 ),
 .UNSPECIFIED., .F., .F.,
 ( 4, 2, 2, 2, 4 ),
 ( 3.925231146709437917E-17, 0.0007406479101619153297, 0.001481295820323791411, 0.002221943730485667710, 0.002962591640647543791 ),
 .UNSPECIFIED. ) ;
#53437 = CARTESIAN_POINT ( 'NONE',  ( 24.68961616380000024, 1449.416966549430072, 225.7902685641979872 ) ) ;
#53438 = EDGE_CURVE ( 'NONE', #99771, #42647, #806, .T. ) ;
#53439 = CARTESIAN_POINT ( 'NONE',  ( 5.161034791280000533, 1485.814572579490005, 218.5690567784690188 ) ) ;
#53440 = CARTESIAN_POINT ( 'NONE',  ( -27.36363609755069959, 1509.868619615939906, 219.7361812052210155 ) ) ;
#53441 = EDGE_CURVE ( 'NONE', #79053, #73912, #63693, .T. ) ;
#53442 = CARTESIAN_POINT ( 'NONE',  ( -8.259315774359869522, 1509.138868980799998, 236.6356052361459774 ) ) ;
#53443 = CARTESIAN_POINT ( 'NONE',  ( -22.59132398960000288, 1450.596213101380044, 220.3211801345979950 ) ) ;
#53445 = CARTESIAN_POINT ( 'NONE',  ( 17.99788318405029841, 1410.854924907409895, 222.9846978063220320 ) ) ;
#53444 = CARTESIAN_POINT ( 'NONE',  ( 4.219439073160000220, 1446.230224797059918, 176.4605749492980067 ) ) ;
#53446 = CARTESIAN_POINT ( 'NONE',  ( -0.3713800987810000342, 1452.819910075930011, 189.4897211325980209 ) ) ;
#53447 = CARTESIAN_POINT ( 'NONE',  ( -105.0172044093909989, 1380.697436583209765, 308.0009267516720115 ) ) ;
#53448 = AXIS2_PLACEMENT_3D ( 'NONE', #25660, #69926, #110229 ) ;
#53449 = ORIENTED_EDGE ( 'NONE', *, *, #65942, .F. ) ;
#53450 = CARTESIAN_POINT ( 'NONE',  ( -5.784008673325000238, 1516.911981270829983, 204.1205073037870079 ) ) ;
#53451 = CARTESIAN_POINT ( 'NONE',  ( 1.624206324989999992E-09, 1405.716796065430117, 267.8540375962979851 ) ) ;
#53452 = CARTESIAN_POINT ( 'NONE',  ( 27.89933032689999948, 1509.196990926829812, 207.5041886574580019 ) ) ;
#53453 = CARTESIAN_POINT ( 'NONE',  ( 19.23545976010510117, 1469.948318476340091, 270.3616590758479674 ) ) ;
#53454 = CARTESIAN_POINT ( 'NONE',  ( 2.478942931479999778, 1432.372492341360157, 157.5167539238979941 ) ) ;
#53455 = ADVANCED_FACE ( 'NONE', ( #84774 ), #75575, .T. ) ;
#53456 = CARTESIAN_POINT ( 'NONE',  ( 3.401546208480000111, 1468.225227913490016, 218.5224274127089927 ) ) ;
#53457 = CARTESIAN_POINT ( 'NONE',  ( -41.70033323359630373, 1440.913060410520075, 261.5743097596159714 ) ) ;
#53458 = CARTESIAN_POINT ( 'NONE',  ( 34.72830299008759880, 1450.359847782400038, 136.2305431565669949 ) ) ;
#53459 = CARTESIAN_POINT ( 'NONE',  ( 1.081131680213342827, 1450.824894072367897, 154.2469214281843506 ) ) ;
#53460 = CARTESIAN_POINT ( 'NONE',  ( 1.038038148820000117, 1431.814275748890168, 200.6412883882290146 ) ) ;
#53461 = CARTESIAN_POINT ( 'NONE',  ( 1.171201999982100173, 1450.815562198650014, 154.2439547458699849 ) ) ;
#53462 = CARTESIAN_POINT ( 'NONE',  ( -0.2520374592430009719, 1508.165742498189957, 220.8827497849989925 ) ) ;
#53463 = EDGE_CURVE ( 'NONE', #31461, #56666, #94279, .T. ) ;
#53464 = ORIENTED_EDGE ( 'NONE', *, *, #107488, .F. ) ;
#53465 = CARTESIAN_POINT ( 'NONE',  ( 2.416798835000000256, 1426.601114010129777, 146.0361887655980127 ) ) ;
#53466 = EDGE_CURVE ( 'NONE', #22743, #65683, #3609, .T. ) ;
#53467 = CARTESIAN_POINT ( 'NONE',  ( -1.262039348750485956, 1450.743516540221663, 181.7894505913149601 ) ) ;
#53468 = CARTESIAN_POINT ( 'NONE',  ( 3.193605244039539937, 1466.133281249020001, 198.9725477671120188 ) ) ;
#53469 = CARTESIAN_POINT ( 'NONE',  ( -1.333756890899999936, 1476.036794647129909, 268.4830614120980385 ) ) ;
#53470 = CARTESIAN_POINT ( 'NONE',  ( 6.263982046360000666, 1500.597020525990047, 203.1398415524789982 ) ) ;
#53472 = B_SPLINE_CURVE_WITH_KNOTS ( 'NONE', 3,
 ( #22969, #48769, #6186, #34695, #2651, #102987, #19965, #88836, #94045, #63127, #53606, #85638, #54710, #20500, #87750, #62576, #28376, #13, #45757, #97229, #37889, #72072, #28937 ),
 .UNSPECIFIED., .F., .F.,
 ( 4, 2, 1, 1, 2, 2, 2, 1, 2, 2, 2, 2, 4 ),
 ( 0.000000000000000000, 0.1249999999999765188, 0.1874999999999680533, 0.2187499999998618327, 0.2343749999999021894, 0.2499999999999425460, 0.3749999999996026512, 0.4374999999995266564, 0.4687499999994845790, 0.4999999999994425015, 0.6249999999996125322, 0.7499999999997823963, 1.000000000000000000 ),
 .UNSPECIFIED. ) ;
#53471 = CARTESIAN_POINT ( 'NONE',  ( -29.61947536759999977, 1509.969965958529883, 210.6832956776279673 ) ) ;
#53473 = CARTESIAN_POINT ( 'NONE',  ( -3.832095730067969441, 1448.295222384574345, 185.0250836445331970 ) ) ;
#53474 = CARTESIAN_POINT ( 'NONE',  ( -22.40689292945249989, 1384.854677225240039, 222.0968912656800001 ) ) ;
#53475 = AXIS2_PLACEMENT_3D ( 'NONE', #64134, #98255, #39460 ) ;
#53476 = B_SPLINE_SURFACE_WITH_KNOTS ( 'NONE', 5, 4, ( 
 ( #104240, #81225, #3456, #4540, #96396 ),
 ( #70129, #27530, #19103, #53306, #97492 ),
 ( #62266, #44915, #37029, #70678, #104792 ),
 ( #37584, #88552, #11298, #12372, #105346 ),
 ( #71787, #20760, #89085, #48759, #57716 ),
 ( #82341, #39224, #66665, #91831, #58253 ) ),
 .UNSPECIFIED., .F., .F., .F.,
 ( 6, 6 ),
 ( 5, 5 ),
 ( 0.000000000000000000, 111.1101480259999903 ),
 ( 25.81581217359999769, 39.03307591160000101 ),
 .UNSPECIFIED. ) ;
#53477 = CARTESIAN_POINT ( 'NONE',  ( -17.74184486700000107, 1415.163755984229965, 208.0694140301980326 ) ) ;
#53478 = CARTESIAN_POINT ( 'NONE',  ( -12.10384762496500066, 1512.631076693560090, 217.6901596511270043 ) ) ;
#53479 = CARTESIAN_POINT ( 'NONE',  ( 26.25308187535300419, 1435.420717402130094, 135.4969117712219884 ) ) ;
#53480 = CARTESIAN_POINT ( 'NONE',  ( -7.087593545181670507, 1396.160564607840115, 200.6470654363129995 ) ) ;
#53481 = CARTESIAN_POINT ( 'NONE',  ( -17.33378134921720104, 1410.882908438999948, 225.8654669597239888 ) ) ;
#53482 = CARTESIAN_POINT ( 'NONE',  ( 4.989973902650000070, 1442.756953654919926, 150.3769280849980134 ) ) ;
#53483 = EDGE_LOOP ( 'NONE', ( #79297, #105148 ) ) ;
#53484 = CARTESIAN_POINT ( 'NONE',  ( -11.41402561306639996, 1500.969831351809944, 208.5831151434670119 ) ) ;
#53485 = CARTESIAN_POINT ( 'NONE',  ( -13.58855293548379883, 1508.389930495940007, 209.7948077685939836 ) ) ;
#53486 = CARTESIAN_POINT ( 'NONE',  ( 0.3788332004054269508, 1408.926289534200123, 231.6114332047860103 ) ) ;
#53488 = CARTESIAN_POINT ( 'NONE',  ( -9.951253231297551238, 1438.974309065549960, 209.5953120751400149 ) ) ;
#53487 = CARTESIAN_POINT ( 'NONE',  ( 10.87934504459999907, 1425.316387834530133, 126.2846869380979911 ) ) ;
#53489 = LINE ( 'NONE', #70308, #30700 ) ;
#53490 = CARTESIAN_POINT ( 'NONE',  ( -9.231470400260000986, 1449.703074994190047, 207.7616675809790081 ) ) ;
#53491 = CARTESIAN_POINT ( 'NONE',  ( -1.128757599205000073, 1516.608208975040043, 201.4108789544669946 ) ) ;
#53492 =( GEOMETRIC_REPRESENTATION_CONTEXT ( 3 ) GLOBAL_UNCERTAINTY_ASSIGNED_CONTEXT ( ( #19946 ) ) GLOBAL_UNIT_ASSIGNED_CONTEXT ( ( #22879, #81507, #55246 ) ) REPRESENTATION_CONTEXT ( 'NONE', 'WORKASPACE' ) );
#53493 = CARTESIAN_POINT ( 'NONE',  ( 7.901745564190000515, 1424.856359000810016, 211.6778634635190031 ) ) ;
#53494 = CARTESIAN_POINT ( 'NONE',  ( -14.82503814461925273, 1430.093753747135452, 221.8913042101295048 ) ) ;
#53495 = CARTESIAN_POINT ( 'NONE',  ( -5.551188713984379852, 1510.480349263560129, 201.5713426139130320 ) ) ;
#53496 = CARTESIAN_POINT ( 'NONE',  ( -0.3621993323151809774, 1416.825784014559986, 191.0664209890499876 ) ) ;
#53497 = CARTESIAN_POINT ( 'NONE',  ( -105.6107621120000033, 1376.170439489020055, 306.5935537603590433 ) ) ;
#53498 = CIRCLE ( 'NONE', #5201, 30.13701971169416183 ) ;
#53499 = CARTESIAN_POINT ( 'NONE',  ( 9.943976501839999926, 1365.461622992600041, 207.6218459616989946 ) ) ;
#53502 = ORIENTED_EDGE ( 'NONE', *, *, #86300, .F. ) ;
#53501 = CARTESIAN_POINT ( 'NONE',  ( 5.741164914759999682, 1453.932054823290173, 216.5784219893689908 ) ) ;
#53500 = PRODUCT_RELATED_PRODUCT_CATEGORY ( 'part', '', ( #71492 ) ) ;
#53503 = ORIENTED_EDGE ( 'NONE', *, *, #76021, .T. ) ;
#53504 = CARTESIAN_POINT ( 'NONE',  ( -12.94626818629999931, 1441.161188681390058, 188.2109162517980110 ) ) ;
#53505 = AXIS2_PLACEMENT_3D ( 'NONE', #63358, #12354, #100230 ) ;
#53506 = CARTESIAN_POINT ( 'NONE',  ( 0.04366246281853980449, 1474.775529741679975, 236.0040081736329967 ) ) ;
#53507 = DIRECTION ( 'NONE',  ( 0.1324471657667971036, -0.9756113948842708439, -0.1750432930800552289 ) ) ;
#53508 = CARTESIAN_POINT ( 'NONE',  ( -8.245978546805000420, 1511.399604276809896, 214.2323161589669951 ) ) ;
#53509 = DIRECTION ( 'NONE',  ( 0.000000000000000000, -2.622151149039999577E-17, 1.000000000000000000 ) ) ;
#53510 = CARTESIAN_POINT ( 'NONE',  ( 23.69809918860000053, 1507.890500233530020, 195.1972782134980093 ) ) ;
#53511 = CARTESIAN_POINT ( 'NONE',  ( -1.625910793146879918, 1463.710942619060006, 199.4574199946389683 ) ) ;
#53512 = DIRECTION ( 'NONE',  ( 0.7454942576402798782, 5.172905559738552453E-15, 0.6665120492724555534 ) ) ;
#53513 = CARTESIAN_POINT ( 'NONE',  ( -2.500000000000039968, 1448.775613387130079, 156.9598478879729839 ) ) ;
#53514 = CARTESIAN_POINT ( 'NONE',  ( 28.37196897381756244, 1435.488267112151334, 135.2384693731098082 ) ) ;
#53515 = CARTESIAN_POINT ( 'NONE',  ( 6.707555271009190356, 1408.966021048169750, 196.0542721895619991 ) ) ;
#53516 = CARTESIAN_POINT ( 'NONE',  ( -5.365730855182169634, 1405.947096103700005, 267.8417508978809565 ) ) ;
#53517 = DIRECTION ( 'NONE',  ( 0.4794255386042036160, 0.000000000000000000, 0.8775825618903725367 ) ) ;
#53518 = VERTEX_POINT ( 'NONE', #53418 ) ;
#53519 = CARTESIAN_POINT ( 'NONE',  ( -11.57646188839999901, 1432.336252568690043, 151.1966908189980074 ) ) ;
#53520 = CARTESIAN_POINT ( 'NONE',  ( 12.53380416529999941, 1442.773886989730045, 186.4115681209980266 ) ) ;
#53521 = EDGE_LOOP ( 'NONE', ( #42663, #51429, #90162, #73201 ) ) ;
#53522 = EDGE_LOOP ( 'NONE', ( #78198, #92335, #546, #18572, #47870, #82221, #99615, #80924, #40678 ) ) ;
#53523 = EDGE_CURVE ( 'NONE', #16284, #65282, #72636, .T. ) ;
#53524 = CARTESIAN_POINT ( 'NONE',  ( -7.799999999999999822, 1412.913060387329779, 209.1218459616989946 ) ) ;
#53525 = CARTESIAN_POINT ( 'NONE',  ( -8.538839991170000587, 1362.569232148550100, 207.6218459616989946 ) ) ;
#53526 = CIRCLE ( 'NONE', #28483, 477.3395627918638411 ) ;
#53527 = ADVANCED_FACE ( 'NONE', ( #45030 ), #29343, .F. ) ;
#53528 = CARTESIAN_POINT ( 'NONE',  ( 0.7553264358530019651, 1516.745833913490060, 214.8974710475970085 ) ) ;
#53529 = CARTESIAN_POINT ( 'NONE',  ( 2.412416358654999815, 1511.982868782460173, 216.7116937071870097 ) ) ;
#53530 = B_SPLINE_CURVE_WITH_KNOTS ( 'NONE', 5,
 ( #77109, #86594, #9886, #2070, #44054, #70385 ),
 .UNSPECIFIED., .F., .F.,
 ( 6, 6 ),
 ( 0.000000000000000000, 1.000000000000000000 ),
 .UNSPECIFIED. ) ;
#53531 = EDGE_LOOP ( 'NONE', ( #93441, #33246, #8300, #90000, #109044 ) ) ;
#53532 = CARTESIAN_POINT ( 'NONE',  ( 7.944350852719999523, 1425.480812533560083, 211.5441705370589887 ) ) ;
#53533 = CARTESIAN_POINT ( 'NONE',  ( -84.31096497809998880, 1379.600296256509864, 298.0935392271590558 ) ) ;
#53534 = CARTESIAN_POINT ( 'NONE',  ( 10.03978052889999972, 1416.217772598529791, 224.7103670548980006 ) ) ;
#53535 = CARTESIAN_POINT ( 'NONE',  ( -2.489617576474999705, 1516.665179208830068, 204.1258511445269903 ) ) ;
#53536 = EDGE_CURVE ( 'NONE', #82244, #777, #101126, .T. ) ;
#53537 = CARTESIAN_POINT ( 'NONE',  ( -28.27139721233033143, 1526.382868172863937, 219.5606225550389752 ) ) ;
#53538 = CARTESIAN_POINT ( 'NONE',  ( -41.48541085310784382, 1435.896297111339663, 269.6377304084467141 ) ) ;
#53539 = CARTESIAN_POINT ( 'NONE',  ( 9.332531155627359354, 1462.059220043490086, 206.3768343672439869 ) ) ;
#53540 = CARTESIAN_POINT ( 'NONE',  ( -6.493240042750000107, 1410.513797117929926, 231.2937525223979947 ) ) ;
#53542 = VERTEX_POINT ( 'NONE', #42659 ) ;
#53541 = CARTESIAN_POINT ( 'NONE',  ( -7.303238992729999879, 1446.886847238160044, 185.6134793553979989 ) ) ;
#53543 = LINE ( 'NONE', #11525, #92241 ) ;
#53544 = CARTESIAN_POINT ( 'NONE',  ( 11.26564539523899100, 1425.481176323582531, 139.1357185245598487 ) ) ;
#53545 = CARTESIAN_POINT ( 'NONE',  ( -17.51956951369999871, 1383.856177979750100, 219.7926916635590260 ) ) ;
#53546 = DIRECTION ( 'NONE',  ( -1.755985294532469921E-16, 1.000000000000000000, -1.338183447452831989E-16 ) ) ;
#53547 = CARTESIAN_POINT ( 'NONE',  ( -24.83630077529999980, 1435.383754686160046, 136.1505334551980013 ) ) ;
#53548 = ADVANCED_FACE ( 'NONE', ( #94148 ), #107527, .F. ) ;
#53549 = CARTESIAN_POINT ( 'NONE',  ( -7.321455911854999776, 1516.545806094630279, 211.6076919691270177 ) ) ;
#53550 = CIRCLE ( 'NONE', #19539, 2.000000000000001776 ) ;
#53551 = CARTESIAN_POINT ( 'NONE',  ( -67.67522575920000349, 1379.745358396210122, 277.8355432199589927 ) ) ;
#53552 = CARTESIAN_POINT ( 'NONE',  ( -8.515748345960094667, 1426.079849815119815, 225.4758549209027478 ) ) ;
#53553 = DIRECTION ( 'NONE',  ( 1.836970198721029688E-16, 1.000000000000000000, -1.262177448353620010E-31 ) ) ;
#53555 = EDGE_CURVE ( 'NONE', #62929, #28257, #42112, .T. ) ;
#53554 = CARTESIAN_POINT ( 'NONE',  ( 20.78146551274081943, 1410.998373634254449, 199.3095149131587505 ) ) ;
#53556 = CARTESIAN_POINT ( 'NONE',  ( 2.297629621054999571, 1516.970035769810011, 209.8568691683980205 ) ) ;
#53557 = ORIENTED_EDGE ( 'NONE', *, *, #102340, .T. ) ;
#53558 = LINE ( 'NONE', #1486, #15085 ) ;
#53559 = CARTESIAN_POINT ( 'NONE',  ( -14.09893512380000047, 1417.904223768229940, 227.3332539714980101 ) ) ;
#53560 = CARTESIAN_POINT ( 'NONE',  ( -49.58302355399999328, 1384.869362640140025, 260.9124492692590138 ) ) ;
#53561 = ADVANCED_FACE ( 'NONE', ( #673 ), #28438, .F. ) ;
#53562 = ORIENTED_EDGE ( 'NONE', *, *, #71271, .F. ) ;
#53563 = CARTESIAN_POINT ( 'NONE',  ( 22.08622291488258327, 1523.456924617339155, 233.8253038720255574 ) ) ;
#53564 = VECTOR ( 'NONE', #90070, 1000.000000000000114 ) ;
#53565 = CARTESIAN_POINT ( 'NONE',  ( 7.734617087614999775, 1513.613303996360173, 201.3001138717470155 ) ) ;
#53566 = PRODUCT_DEFINITION_SHAPE ( 'NONE', 'NONE',  #21967 ) ;
#53567 = CARTESIAN_POINT ( 'NONE',  ( 17.85726237922320081, 1469.009919690150127, 228.6204578493800170 ) ) ;
#53568 = CARTESIAN_POINT ( 'NONE',  ( -24.69948770750570333, 1509.552006277990131, 222.6391526336500135 ) ) ;
#53569 = CARTESIAN_POINT ( 'NONE',  ( -2.935740854740000128, 1409.954265560430031, 186.6342706574980070 ) ) ;
#53570 = DIRECTION ( 'NONE',  ( 0.000000000000000000, 0.000000000000000000, -1.000000000000000000 ) ) ;
#53571 = CARTESIAN_POINT ( 'NONE',  ( 0.05285025628535950509, 1420.446797781519990, 182.6782354290490105 ) ) ;
#53572 = EDGE_CURVE ( 'NONE', #8387, #99599, #37098, .T. ) ;
#53574 = CARTESIAN_POINT ( 'NONE',  ( -4.250070903060000127, 1421.703404100430134, 185.6649461332980025 ) ) ;
#53573 = CARTESIAN_POINT ( 'NONE',  ( 2.874588922665000545, 1516.606339319019980, 215.6687976528169770 ) ) ;
#53575 = CARTESIAN_POINT ( 'NONE',  ( -5.931183514203220319, 1391.913060387289988, 215.1140006419229849 ) ) ;
#53576 = CARTESIAN_POINT ( 'NONE',  ( 10.94950459731960102, 1470.725626738129904, 208.8250202921669825 ) ) ;
#53577 = ORIENTED_EDGE ( 'NONE', *, *, #9321, .T. ) ;
#53578 = CARTESIAN_POINT ( 'NONE',  ( -12.25440271872340148, 1415.429375168349907, 196.4054266176139834 ) ) ;
#53579 = CARTESIAN_POINT ( 'NONE',  ( -20.49599333844893678, 1525.960063244516959, 184.3798832129038203 ) ) ;
#53580 = VERTEX_POINT ( 'NONE', #64980 ) ;
#53581 = VECTOR ( 'NONE', #55247, 1000.000000000000000 ) ;
#53582 = CARTESIAN_POINT ( 'NONE',  ( 0.3313159878120000013, 1417.263519912130050, 235.9102102634980156 ) ) ;
#53583 = EDGE_CURVE ( 'NONE', #55469, #22181, #84268, .T. ) ;
#53584 = CARTESIAN_POINT ( 'NONE',  ( 9.934585978703848852, 1435.770999680745945, 152.5360695867651089 ) ) ;
#53585 = CARTESIAN_POINT ( 'NONE',  ( 8.600792717434700307, 1511.535603804869879, 203.3761131401680018 ) ) ;
#53586 = LINE ( 'NONE', #44624, #14575 ) ;
#53587 = PLANE ( 'NONE',  #103292 ) ;
#53588 = CARTESIAN_POINT ( 'NONE',  ( -21.01415622427472485, 1519.551704408389924, 217.3717009491090835 ) ) ;
#53589 = CARTESIAN_POINT ( 'NONE',  ( 17.86855543449999928, 1415.163755998629995, 210.6784302842380043 ) ) ;
#53590 = CARTESIAN_POINT ( 'NONE',  ( -2.446787376320000096, 1432.353341358199941, 150.2884730787980061 ) ) ;
#53591 = CARTESIAN_POINT ( 'NONE',  ( -22.85501015979999906, 1436.107805423079981, 141.7713381877979941 ) ) ;
#53592 = CARTESIAN_POINT ( 'NONE',  ( -13.40786186986500006, 1517.051704408389924, 199.6217297329870064 ) ) ;
#53593 = CARTESIAN_POINT ( 'NONE',  ( 16.64856530119999789, 1416.208557986029973, 191.4534465615980139 ) ) ;
#53595 = CARTESIAN_POINT ( 'NONE',  ( -18.97549637783819421, 1439.232629296661344, 210.2045300455428389 ) ) ;
#53594 = CARTESIAN_POINT ( 'NONE',  ( 0.6414547015549999509, 1416.067629290630066, 190.6212042380979881 ) ) ;
#53596 = EDGE_CURVE ( 'NONE', #53095, #81952, #57149, .T. ) ;
#53597 = CARTESIAN_POINT ( 'NONE',  ( -113.4000000000000057, 1347.163060387289988, 304.2218459572590064 ) ) ;
#53598 = ORIENTED_EDGE ( 'NONE', *, *, #57715, .F. ) ;
#53599 = CARTESIAN_POINT ( 'NONE',  ( 13.73472823738089943, 1456.560500377009930, 194.8610419970869998 ) ) ;
#53600 = CARTESIAN_POINT ( 'NONE',  ( 26.56868433090000181, 1488.557140808829899, 207.4007234374079758 ) ) ;
#53601 = ADVANCED_FACE ( 'NONE', ( #91808 ), #38274, .F. ) ;
#53602 = CARTESIAN_POINT ( 'NONE',  ( -23.67281635530000017, 1436.130135845430004, 211.8387132574179930 ) ) ;
#53603 = CARTESIAN_POINT ( 'NONE',  ( -4.878045583760000525, 1484.465894326689977, 199.1376824933889793 ) ) ;
#53604 = CARTESIAN_POINT ( 'NONE',  ( -18.51591345220000306, 1509.559650331729927, 231.0978208730980157 ) ) ;
#53605 = CARTESIAN_POINT ( 'NONE',  ( 0.3788332004054269508, 1408.926289534200123, 231.6114332047860103 ) ) ;
#53606 = CARTESIAN_POINT ( 'NONE',  ( 11.52616021266821278, 1434.866878790148348, 151.4211076298512637 ) ) ;
#53607 = B_SPLINE_SURFACE_WITH_KNOTS ( 'NONE', 4, 5, ( 
 ( #85991, #35032, #17653, #70891, #61378, #19318 ),
 ( #44002, #28294, #95497, #53519, #69211, #78137 ),
 ( #43452, #9289, #45123, #79265, #2575, #78703 ),
 ( #26059, #1440, #36697, #88211, #62490, #35586 ),
 ( #94372, #69778, #51854, #96610, #19879, #94949 ) ),
 .UNSPECIFIED., .F., .F., .F.,
 ( 5, 5 ),
 ( 6, 6 ),
 ( 13.83774376510000081, 13.94215241960000107 ),
 ( 0.000000000000000000, 2.228199836199999950 ),
 .UNSPECIFIED. ) ;
#53608 = CARTESIAN_POINT ( 'NONE',  ( 29.36007807473284359, 1526.208281990542673, 220.5288989449384189 ) ) ;
#53609 = CARTESIAN_POINT ( 'NONE',  ( -22.59870855689359814, 1509.715337612740086, 188.9651625613269914 ) ) ;
#53610 = EDGE_CURVE ( 'NONE', #26627, #40693, #109896, .T. ) ;
#53611 = CARTESIAN_POINT ( 'NONE',  ( -9.051675461232269626, 1490.533562533649956, 215.4358965029069850 ) ) ;
#53612 = CARTESIAN_POINT ( 'NONE',  ( 5.076294927523219869, 1469.790098474529941, 187.8425670808459813 ) ) ;
#53613 = CARTESIAN_POINT ( 'NONE',  ( -77.70051540026119596, 1383.778684295149787, 302.0161327210769855 ) ) ;
#53614 = CARTESIAN_POINT ( 'NONE',  ( -109.4951920581290068, 1383.413356185199973, 311.1619299154190230 ) ) ;
#53615 = CARTESIAN_POINT ( 'NONE',  ( -15.45308515272032501, 1506.474306115792388, 224.8043937606940688 ) ) ;
#53616 = CARTESIAN_POINT ( 'NONE',  ( -1.398549609401959826, 1516.583792872650065, 201.4115183126079955 ) ) ;
#53618 = ORIENTED_EDGE ( 'NONE', *, *, #35110, .F. ) ;
#53617 = CARTESIAN_POINT ( 'NONE',  ( 10.47377178300940059, 1451.946270717840207, 207.9508650615720171 ) ) ;
#53619 = CARTESIAN_POINT ( 'NONE',  ( -18.41191564635506950, 1458.954972189355885, 227.7144718060530977 ) ) ;
#53620 = AXIS2_PLACEMENT_3D ( 'NONE', #26154, #7169, #85506 ) ;
#53621 = CARTESIAN_POINT ( 'NONE',  ( -59.81489691519999496, 1382.332781621870026, 279.6089507563589791 ) ) ;
#53622 = FACE_OUTER_BOUND ( 'NONE', #40110, .T. ) ;
#53623 = ORIENTED_EDGE ( 'NONE', *, *, #59118, .F. ) ;
#53624 = EDGE_LOOP ( 'NONE', ( #29368, #41111, #82652, #86969 ) ) ;
#53625 = CARTESIAN_POINT ( 'NONE',  ( 23.89882922079599936, 1419.330057139640076, 207.7533880750820003 ) ) ;
#53626 = CARTESIAN_POINT ( 'NONE',  ( 13.70391237549999985, 1509.385661485429864, 234.3784090209980207 ) ) ;
#53627 = CARTESIAN_POINT ( 'NONE',  ( 13.14452880787822586, 1443.063641493199384, 169.3992238275367299 ) ) ;
#53629 = CARTESIAN_POINT ( 'NONE',  ( -39.40331983270000649, 1445.870378090409758, 259.1105268160980586 ) ) ;
#53628 = CARTESIAN_POINT ( 'NONE',  ( -13.13561839920526886, 1517.051704408389924, 208.3084799397878157 ) ) ;
#53630 = CARTESIAN_POINT ( 'NONE',  ( -3.613876939720699788, 1495.512358501490098, 197.3347655600630333 ) ) ;
#53631 = CARTESIAN_POINT ( 'NONE',  ( -11.39963766959999880, 1433.910854737510135, 151.4262557347980191 ) ) ;
#53632 = CARTESIAN_POINT ( 'NONE',  ( 25.78155807829999802, 1509.813372234129929, 195.1138720307980066 ) ) ;
#53633 = CARTESIAN_POINT ( 'NONE',  ( -20.68237067309999944, 1485.791741470130091, 191.8803888813980052 ) ) ;
#53634 = CARTESIAN_POINT ( 'NONE',  ( 9.698169174809999404, 1409.251727919130190, 189.5635320467980307 ) ) ;
#53635 = CARTESIAN_POINT ( 'NONE',  ( 1.925297169133120212, 1521.951704408389787, 230.6853930764029883 ) ) ;
#53636 = CARTESIAN_POINT ( 'NONE',  ( -10.92774616719999869, 1436.036447822629952, 151.9134056697980100 ) ) ;
#53637 = CARTESIAN_POINT ( 'NONE',  ( 10.64187387509999994, 1435.613679513749958, 152.0651251919979927 ) ) ;
#53638 = CARTESIAN_POINT ( 'NONE',  ( -12.04274590166719960, 1422.870584108250114, 204.0708875435599907 ) ) ;
#53639 = CARTESIAN_POINT ( 'NONE',  ( -14.51584819470000021, 1452.406155798529880, 148.7179611920979880 ) ) ;
#53640 = CARTESIAN_POINT ( 'NONE',  ( 1.348363413820000245, 1466.040058158929924, 235.1849735751980006 ) ) ;
#53641 = VERTEX_POINT ( 'NONE', #92354 ) ;
#53642 = CARTESIAN_POINT ( 'NONE',  ( -4.544860949933259953, 1508.551704410290085, 213.0837902323600019 ) ) ;
#53643 = CARTESIAN_POINT ( 'NONE',  ( -5.294782532323449864, 1489.664752326729968, 185.8873045459189939 ) ) ;
#53644 = CARTESIAN_POINT ( 'NONE',  ( -38.65570300630000133, 1453.321626439029842, 269.5859728025980075 ) ) ;
#53645 = DIRECTION ( 'NONE',  ( 0.1159387279768451934, 0.9932563673871469545, 0.000000000000000000 ) ) ;
#53646 = CARTESIAN_POINT ( 'NONE',  ( 3.312638106410000116, 1440.449723275869928, 155.6633363266980155 ) ) ;
#53647 = CARTESIAN_POINT ( 'NONE',  ( -16.68599179819999989, 1461.099982565929849, 230.2790296985980092 ) ) ;
#53648 = CIRCLE ( 'NONE', #82216, 1.000000000000000000 ) ;
#53649 = CARTESIAN_POINT ( 'NONE',  ( 4.329068131566989663, 1515.079329108569937, 210.5320604527299793 ) ) ;
#53650 = CARTESIAN_POINT ( 'NONE',  ( 2.905858652024770006, 1409.547798013280044, 231.3102161809150061 ) ) ;
#53651 = CARTESIAN_POINT ( 'NONE',  ( -2.782343519255962239, 1516.553084368694726, 201.4123224916152424 ) ) ;
#53652 = CARTESIAN_POINT ( 'NONE',  ( -9.848894837239999589, 1418.540965017630015, 230.1861045164980055 ) ) ;
#53653 = CARTESIAN_POINT ( 'NONE',  ( -9.311658524700000328, 1460.574498714589936, 213.2399738195690304 ) ) ;
#53654 = CARTESIAN_POINT ( 'NONE',  ( 9.622136349625579399, 1363.684386430212044, 210.6218459616991936 ) ) ;
#53655 = CARTESIAN_POINT ( 'NONE',  ( -45.56365896290319739, 1436.758397562629852, 266.4221133662970260 ) ) ;
#53656 = CARTESIAN_POINT ( 'NONE',  ( -4.152137804869999727, 1434.229915741350169, 185.7429424955980153 ) ) ;
#53657 = AXIS2_PLACEMENT_3D ( 'NONE', #47045, #38615, #28018 ) ;
#53658 = ORIENTED_EDGE ( 'NONE', *, *, #15065, .F. ) ;
#53659 = CARTESIAN_POINT ( 'NONE',  ( 26.79414481833639883, 1435.433178084320161, 135.2874577367330176 ) ) ;
#53660 = EDGE_LOOP ( 'NONE', ( #14360, #67847, #47049, #24017 ) ) ;
#53661 = CARTESIAN_POINT ( 'NONE',  ( -7.326072182274999456, 1516.714320817460020, 209.8751461055349807 ) ) ;
#53662 = ADVANCED_FACE ( 'NONE', ( #50928 ), #18540, .F. ) ;
#53663 = CARTESIAN_POINT ( 'NONE',  ( -8.928049104570000338, 1472.922707491090023, 201.8104512964389983 ) ) ;
#53664 = FACE_OUTER_BOUND ( 'NONE', #10733, .T. ) ;
#53665 = CARTESIAN_POINT ( 'NONE',  ( -15.71820076539999889, 1410.407305047730006, 191.1858524523979952 ) ) ;
#53666 = AXIS2_PLACEMENT_3D ( 'NONE', #62158, #96285, #19562 ) ;
#53667 = DIRECTION ( 'NONE',  ( -0.000000000000000000, -1.000000000000000000, -0.000000000000000000 ) ) ;
#53668 = ORIENTED_EDGE ( 'NONE', *, *, #29677, .F. ) ;
#53669 = CARTESIAN_POINT ( 'NONE',  ( 24.55901760909999965, 1439.292416066280111, 213.0859795990780015 ) ) ;
#53671 = CARTESIAN_POINT ( 'NONE',  ( -29.36007807473230713, 1526.208281990539035, 197.7147929784467806 ) ) ;
#53670 = CARTESIAN_POINT ( 'NONE',  ( -2.494564929293782818, 1524.201670966335769, 175.5409631904079788 ) ) ;
#53672 =( BOUNDED_CURVE ( )  B_SPLINE_CURVE ( 3, ( #15957, #5380, #31125, #50160 ),
 .UNSPECIFIED., .F., .F. ) 
 B_SPLINE_CURVE_WITH_KNOTS ( ( 4, 4 ),
 ( 0.9002477009694579424, 1.144704973640545909 ),
 .UNSPECIFIED. ) 
 CURVE ( )  GEOMETRIC_REPRESENTATION_ITEM ( )  RATIONAL_B_SPLINE_CURVE ( ( 1.000000000000000000, 0.9950262503666102987, 0.9950262503666102987, 1.000000000000000000 ) ) 
 REPRESENTATION_ITEM ( '' )  );
#53673 = CARTESIAN_POINT ( 'NONE',  ( 1.761008324855960039, 1487.196696357248584, 219.8036233159708388 ) ) ;
#53674 = CARTESIAN_POINT ( 'NONE',  ( -17.13701823974819760, 1508.493192689929856, 212.9882043946190322 ) ) ;
#53675 = EDGE_CURVE ( 'NONE', #110163, #56949, #55764, .T. ) ;
#53676 = CARTESIAN_POINT ( 'NONE',  ( 5.586191088959999718, 1473.645535070089863, 218.5932301067289814 ) ) ;
#53677 = B_SPLINE_CURVE_WITH_KNOTS ( 'NONE', 5,
 ( #70660, #72294, #71206, #87997, #20744, #3991 ),
 .UNSPECIFIED., .F., .F.,
 ( 6, 6 ),
 ( 0.000000000000000000, 1.000000000000000000 ),
 .UNSPECIFIED. ) ;
#53678 = CARTESIAN_POINT ( 'NONE',  ( -8.248738497215569510, 1439.101388822510216, 206.2653402195520016 ) ) ;
#53679 = ORIENTED_EDGE ( 'NONE', *, *, #101553, .T. ) ;
#53680 = CARTESIAN_POINT ( 'NONE',  ( -23.16921277159769943, 1412.901786882649958, 270.3115576615130067 ) ) ;
#53681 = CARTESIAN_POINT ( 'NONE',  ( 2.868112131164999745, 1516.855632454399938, 208.3641823986619954 ) ) ;
#53682 = CARTESIAN_POINT ( 'NONE',  ( 2.920857164672000295, 1415.930116342160090, 231.8786464872950148 ) ) ;
#53683 = CARTESIAN_POINT ( 'NONE',  ( 8.496650132276949208, 1436.860065467399863, 207.6057550149429858 ) ) ;
#53684 = EDGE_CURVE ( 'NONE', #86033, #67895, #41226, .T. ) ;
#53686 = ORIENTED_EDGE ( 'NONE', *, *, #17166, .T. ) ;
#53685 = CARTESIAN_POINT ( 'NONE',  ( -7.148069258222480293, 1365.798506070639633, 209.6218459617148824 ) ) ;
#53687 = ORIENTED_EDGE ( 'NONE', *, *, #633, .F. ) ;
#53688 = CARTESIAN_POINT ( 'NONE',  ( 45.59681776243620277, 1442.353254080252782, 268.9758503888685368 ) ) ;
#53689 = CARTESIAN_POINT ( 'NONE',  ( 0.03042691127746960031, 1467.462897955010249, 220.2118647206560240 ) ) ;
#53690 = CARTESIAN_POINT ( 'NONE',  ( 3.668705825779739804, 1424.252539915140460, 184.0936608447964886 ) ) ;
#53691 = AXIS2_PLACEMENT_3D ( 'NONE', #34861, #23695, #100946 ) ;
#53692 = CARTESIAN_POINT ( 'NONE',  ( -0.009463166745531850083, 1408.928470256950050, 186.2540302668519985 ) ) ;
#53693 = B_SPLINE_CURVE_WITH_KNOTS ( 'NONE', 3,
 ( #5230, #22544, #81927, #106048, #90882, #47791, #13054, #38273, #80296, #39383, #73560, #72457, #38821, #29325, #37735, #74107, #12533, #65703, #107693, #65153, #14169, #55662 ),
 .UNSPECIFIED., .F., .F.,
 ( 4, 2, 1, 1, 2, 2, 2, 2, 1, 1, 2, 2, 4 ),
 ( 0.000000000000000000, 0.1249999999998943900, 0.1874999999998415712, 0.2187499999998157307, 0.2343749999997886413, 0.2499999999997615241, 0.4999999999997214450, 0.6249999999997183364, 0.6874999999997178923, 0.7187499999997348787, 0.7343749999997226663, 0.7499999999997104538, 1.000000000000000000 ),
 .UNSPECIFIED. ) ;
#53694 = CARTESIAN_POINT ( 'NONE',  ( -20.90608034417369510, 1506.501081265402263, 216.1110890664156727 ) ) ;
#53695 = CARTESIAN_POINT ( 'NONE',  ( -17.62832093970000003, 1420.842712498729952, 226.1633071633980023 ) ) ;
#53696 = CARTESIAN_POINT ( 'NONE',  ( -0.0001227683397465710060, 1475.836931224890122, 266.9609101321269691 ) ) ;
#53697 = CARTESIAN_POINT ( 'NONE',  ( -11.64901520891459974, 1391.913060387140149, 208.7065094566399921 ) ) ;
#53698 = FACE_OUTER_BOUND ( 'NONE', #55044, .T. ) ;
#53699 = CARTESIAN_POINT ( 'NONE',  ( -6.950214971414999887, 1517.129577905929864, 206.2502655435069983 ) ) ;
#53700 = ORIENTED_EDGE ( 'NONE', *, *, #54340, .F. ) ;
#53701 = CARTESIAN_POINT ( 'NONE',  ( 2.306961389589999634, 1443.485925623590219, 214.8977830156290167 ) ) ;
#53702 = CARTESIAN_POINT ( 'NONE',  ( 1.514633574868839760, 1459.047947303010005, 183.2114944213780063 ) ) ;
#53703 = ORIENTED_EDGE ( 'NONE', *, *, #98518, .T. ) ;
#53705 = AXIS2_PLACEMENT_3D ( 'NONE', #100697, #41370, #99040 ) ;
#53704 = DIRECTION ( 'NONE',  ( 4.057416247971030182E-16, 1.000000000000000000, -4.440892098500000003E-16 ) ) ;
#53706 = EDGE_CURVE ( 'NONE', #9501, #68723, #27927, .T. ) ;
#53707 = CARTESIAN_POINT ( 'NONE',  ( 26.47436799094689874, 1450.913174653700025, 136.4782587642529847 ) ) ;
#53708 = CARTESIAN_POINT ( 'NONE',  ( 14.35445997400000095, 1416.822690122629865, 196.6654169409980000 ) ) ;
#53709 = CARTESIAN_POINT ( 'NONE',  ( -35.17158829440000289, 1389.591391915819941, 212.7234995045390065 ) ) ;
#53710 = ADVANCED_FACE ( 'NONE', ( #4780 ), #75344, .T. ) ;
#53711 = CARTESIAN_POINT ( 'NONE',  ( 7.457021537675000644, 1517.051697240460271, 213.5019697367769993 ) ) ;
#53712 = CARTESIAN_POINT ( 'NONE',  ( 18.06824345470000281, 1410.907293943229888, 193.5833886661979761 ) ) ;
#53713 = CARTESIAN_POINT ( 'NONE',  ( 22.16158255899999929, 1409.686959905830236, 207.7669082622679753 ) ) ;
#53714 = CARTESIAN_POINT ( 'NONE',  ( 2.515271632033067029, 1439.627825555826803, 183.0399134896231601 ) ) ;
#53716 = CARTESIAN_POINT ( 'NONE',  ( -19.37919121348099338, 1425.467690119061444, 223.5898347255973988 ) ) ;
#53715 = CARTESIAN_POINT ( 'NONE',  ( 0.3238590051470000009, 1415.419573753229997, 233.4172068791979768 ) ) ;
#53717 = CARTESIAN_POINT ( 'NONE',  ( 0.7878817032865200742, 1452.621947969149915, 183.3487653229790055 ) ) ;
#53718 = EDGE_CURVE ( 'NONE', #87268, #8026, #71865, .T. ) ;
#53719 = CARTESIAN_POINT ( 'NONE',  ( -8.148860876500000572, 1382.487756853370001, 218.5247792508289990 ) ) ;
#53720 = CARTESIAN_POINT ( 'NONE',  ( -2.287084308194999860, 1517.068517094990057, 214.1351209316169957 ) ) ;
#53721 = CARTESIAN_POINT ( 'NONE',  ( 26.34505535303209811, 1447.162759454769912, 137.4478556263329949 ) ) ;
#53722 = ORIENTED_EDGE ( 'NONE', *, *, #65817, .F. ) ;
#53723 = DIRECTION ( 'NONE',  ( -0.2054769195713318786, 0.000000000000000000, 0.9786619618251628516 ) ) ;
#53724 = CARTESIAN_POINT ( 'NONE',  ( 22.66254714602126441, 1523.342713519622748, 236.8145175431291989 ) ) ;
#53725 = CARTESIAN_POINT ( 'NONE',  ( -0.3999176547066230492, 1409.147139264330008, 232.5106188436409980 ) ) ;
#53726 = EDGE_CURVE ( 'NONE', #9730, #73741, #59074, .T. ) ;
#53727 = DIRECTION ( 'NONE',  ( -1.000000000000000000, 0.000000000000000000, 0.000000000000000000 ) ) ;
#53728 = CARTESIAN_POINT ( 'NONE',  ( -37.14121207673490233, 1449.456133586259966, 136.3012389827200082 ) ) ;
#53729 = CARTESIAN_POINT ( 'NONE',  ( -32.86802468386279941, 1501.977400791986611, 217.2040256693919957 ) ) ;
#53730 = CARTESIAN_POINT ( 'NONE',  ( -10.05164998770000118, 1455.338937666430184, 224.8635561661979807 ) ) ;
#53731 = CARTESIAN_POINT ( 'NONE',  ( -1.941439933476549973, 1451.940361028549887, 184.3724788387269768 ) ) ;
#53732 = CARTESIAN_POINT ( 'NONE',  ( 11.21314269340000180, 1433.085161743930030, 151.5744673939979918 ) ) ;
#53733 = CARTESIAN_POINT ( 'NONE',  ( 8.934239303591028146E-06, 1474.175163912050039, 270.1377477021339928 ) ) ;
#53734 = B_SPLINE_SURFACE_WITH_KNOTS ( 'NONE', 5, 4, ( 
 ( #88286, #96128, #8938, #97777, #11580 ),
 ( #11030, #106187, #569, #59926, #71532 ),
 ( #17311, #42549, #63662, #25726, #45199 ),
 ( #12122, #43112, #36779, #21052, #29469 ),
 ( #55255, #46314, #80443, #34148, #3757 ),
 ( #96695, #77271, #89387, #26286, #60475 ) ),
 .UNSPECIFIED., .F., .F., .F.,
 ( 6, 6 ),
 ( 5, 5 ),
 ( 0.000000000000000000, 111.1101480259999903 ),
 ( 25.81581217359999769, 39.03307591160000101 ),
 .UNSPECIFIED. ) ;
#53735 = CARTESIAN_POINT ( 'NONE',  ( 27.46979534332119854, 1440.913060388420035, 228.9356845949239982 ) ) ;
#53736 = CARTESIAN_POINT ( 'NONE',  ( -21.33960867280000073, 1508.012995197530017, 227.2182461948980006 ) ) ;
#53737 = CARTESIAN_POINT ( 'NONE',  ( 2.788373426233030195, 1425.940953389439983, 188.8017441523220157 ) ) ;
#53738 = ORIENTED_EDGE ( 'NONE', *, *, #91505, .F. ) ;
#53739 = CIRCLE ( 'NONE', #19729, 2.000000000000068390 ) ;
#53740 = EDGE_CURVE ( 'NONE', #100597, #23737, #75425, .T. ) ;
#53741 = CARTESIAN_POINT ( 'NONE',  ( -105.4624709189999834, 1391.255327103129957, 304.2078109453590287 ) ) ;
#53742 = CARTESIAN_POINT ( 'NONE',  ( 14.56320595439999899, 1474.359403032329965, 224.0680315863980070 ) ) ;
#53743 = CARTESIAN_POINT ( 'NONE',  ( -6.972327688130000034, 1486.046393097330110, 182.7313348475980206 ) ) ;
#53744 = CARTESIAN_POINT ( 'NONE',  ( -1.116585105924089969E-07, 1397.914279478820163, 196.1218459578329885 ) ) ;
#53745 = CARTESIAN_POINT ( 'NONE',  ( 2.371440457460000317, 1490.912983831230122, 235.3311647238980129 ) ) ;
#53746 = EDGE_CURVE ( 'NONE', #15491, #90688, #74226, .T. ) ;
#53747 = AXIS2_PLACEMENT_3D ( 'NONE', #69353, #103463, #26770 ) ;
#53748 = CARTESIAN_POINT ( 'NONE',  ( 25.29760786760000002, 1449.800867294439968, 211.5544486736880003 ) ) ;
#53749 = B_SPLINE_CURVE_WITH_KNOTS ( 'NONE', 5,
 ( #24962, #85428, #100586, #42906, #59172, #93290 ),
 .UNSPECIFIED., .F., .F.,
 ( 6, 6 ),
 ( -1.999999843773010211, -1.697648102094717615E-07 ),
 .UNSPECIFIED. ) ;
#53750 = CARTESIAN_POINT ( 'NONE',  ( -8.881784197000000993E-16, 1392.213060387289943, 209.1218459616989946 ) ) ;
#53751 = CARTESIAN_POINT ( 'NONE',  ( 7.069913306463050162, 1426.666554464499995, 213.2414280066960259 ) ) ;
#53752 = CARTESIAN_POINT ( 'NONE',  ( -28.88780438494880087, 1383.843457635159893, 226.6985655709949867 ) ) ;
#53753 = CARTESIAN_POINT ( 'NONE',  ( -4.833436910021659649, 1508.551704408290107, 205.8972885837780211 ) ) ;
#53754 = CARTESIAN_POINT ( 'NONE',  ( 2.158908090871114016, 1417.717801426661936, 234.2951402407404373 ) ) ;
#53755 = CARTESIAN_POINT ( 'NONE',  ( 0.1596481920543649791, 1486.478835695869975, 181.8160301856430010 ) ) ;
#53757 = ORIENTED_EDGE ( 'NONE', *, *, #35568, .T. ) ;
#53756 = DIRECTION ( 'NONE',  ( 0.7835778714266642409, -0.02736314221910695482, 0.6206907264156240611 ) ) ;
#53758 = CARTESIAN_POINT ( 'NONE',  ( -1.121218466020000193, 1416.837080248530128, 228.0853546194979913 ) ) ;
#53759 = CARTESIAN_POINT ( 'NONE',  ( -3.078458307820000073, 1379.815171990729823, 214.0599463573090020 ) ) ;
#53760 = CARTESIAN_POINT ( 'NONE',  ( -20.55810159319999997, 1507.794327612029974, 189.9655093376980233 ) ) ;
#53762 = ORIENTED_EDGE ( 'NONE', *, *, #74069, .T. ) ;
#53761 = CARTESIAN_POINT ( 'NONE',  ( -32.35345263957390216, 1524.872178180564333, 217.0491086732562280 ) ) ;
#53763 = CARTESIAN_POINT ( 'NONE',  ( -3.030734320792309422, 1508.551704408389924, 219.9920206123570097 ) ) ;
#53764 = VERTEX_POINT ( 'NONE', #23779 ) ;
#53765 = CARTESIAN_POINT ( 'NONE',  ( -14.50876837679670039, 1379.873341110849879, 208.4861929993290062 ) ) ;
#53766 = DIRECTION ( 'NONE',  ( 0.000000000000000000, 1.000000000000000000, 0.000000000000000000 ) ) ;
#53767 = CARTESIAN_POINT ( 'NONE',  ( -16.66231036550682987, 1523.604703353109699, 237.7554842931448036 ) ) ;
#53768 = LINE ( 'NONE', #3356, #73301 ) ;
#53769 = CARTESIAN_POINT ( 'NONE',  ( 0.7324858582209989866, 1431.361405734790196, 218.1975961472689960 ) ) ;
#53770 = CARTESIAN_POINT ( 'NONE',  ( -15.59561454159999982, 1421.682133015659929, 211.4342267833790174 ) ) ;
#53771 = CARTESIAN_POINT ( 'NONE',  ( 13.01686471861349936, 1409.367619315190041, 216.4512120152259911 ) ) ;
#53772 = CARTESIAN_POINT ( 'NONE',  ( 18.52319328460000136, 1425.707465110329849, 225.1076900885979910 ) ) ;
#53773 = CARTESIAN_POINT ( 'NONE',  ( -93.78740748285459006, 1385.204112366519894, 294.4874550187400359 ) ) ;
#53774 = LINE ( 'NONE', #11736, #37205 ) ;
#53775 = CARTESIAN_POINT ( 'NONE',  ( 10.82765054261410143, 1427.328577260649809, 209.3704925542409967 ) ) ;
#53776 = ORIENTED_EDGE ( 'NONE', *, *, #1108, .F. ) ;
#53777 = CARTESIAN_POINT ( 'NONE',  ( 12.22822919944690057, 1491.662241031820031, 207.6548834463269770 ) ) ;
#53779 = ORIENTED_EDGE ( 'NONE', *, *, #29523, .T. ) ;
#53778 = CARTESIAN_POINT ( 'NONE',  ( -1.815594625336599988, 1438.273795259480039, 227.6128410382069944 ) ) ;
#53780 = VERTEX_POINT ( 'NONE', #109467 ) ;
#53781 = CARTESIAN_POINT ( 'NONE',  ( -11.29240054898340162, 1415.034069335250024, 195.6281518637269983 ) ) ;
#53782 = CARTESIAN_POINT ( 'NONE',  ( 0.05823133897989880153, 1360.390585217559874, 207.6218459616989946 ) ) ;
#53783 = CARTESIAN_POINT ( 'NONE',  ( 0.8769335050712490087, 1496.770081789519963, 196.7770485174839905 ) ) ;
#53784 = CIRCLE ( 'NONE', #84113, 1.000000000000000000 ) ;
#53785 = CARTESIAN_POINT ( 'NONE',  ( 29.24997129405418761, 1509.943677684565046, 213.2686300063438125 ) ) ;
#53786 = CARTESIAN_POINT ( 'NONE',  ( -115.5939564047259296, 1379.913060387289988, 305.4204098037694735 ) ) ;
#53787 = CARTESIAN_POINT ( 'NONE',  ( 2.403403406279999821, 1396.180594103330122, 220.9064825637979936 ) ) ;
#53788 = CARTESIAN_POINT ( 'NONE',  ( 2.241849513110000025, 1417.743522105730108, 234.2089936445980243 ) ) ;
#53789 = CARTESIAN_POINT ( 'NONE',  ( 12.65728676410210163, 1420.119835224449844, 200.3472210950669989 ) ) ;
#53790 = CARTESIAN_POINT ( 'NONE',  ( -19.23500960428314954, 1486.267560991677101, 189.5407332401421741 ) ) ;
#53791 = CARTESIAN_POINT ( 'NONE',  ( -11.03264336018479774, 1364.917927611109917, 207.6218459616987673 ) ) ;
#53792 = DIRECTION ( 'NONE',  ( 0.1484981130679619565, -0.4511266441233499069, 0.8800187846729518037 ) ) ;
#53793 = CARTESIAN_POINT ( 'NONE',  ( -3.268859434184999913, 1516.922519270759949, 206.6438591998669949 ) ) ;
#53794 = CARTESIAN_POINT ( 'NONE',  ( 19.68364361584636768, 1521.951704408389787, 197.0079017806501156 ) ) ;
#53795 = CARTESIAN_POINT ( 'NONE',  ( 6.305024129259999555, 1422.156209412130011, 144.1468801376980196 ) ) ;
#53796 = CARTESIAN_POINT ( 'NONE',  ( 22.08327125186944428, 1523.604703353109699, 233.8169256665487694 ) ) ;
#53797 = FACE_OUTER_BOUND ( 'NONE', #40960, .T. ) ;
#53798 = CARTESIAN_POINT ( 'NONE',  ( 41.64578063898380123, 1444.020661637949843, 135.8457820201300024 ) ) ;
#53799 = VERTEX_POINT ( 'NONE', #32745 ) ;
#53800 = CARTESIAN_POINT ( 'NONE',  ( 13.01666426059999893, 1409.302076636529819, 262.4458742036980539 ) ) ;
#53801 = CARTESIAN_POINT ( 'NONE',  ( -21.04266092970000201, 1508.126368072830019, 192.1685821131979992 ) ) ;
#53803 = CARTESIAN_POINT ( 'NONE',  ( 3.062523615019999729E-14, 1419.211677883429957, 248.0989693021979861 ) ) ;
#53802 = CARTESIAN_POINT ( 'NONE',  ( -10.08898255699300073, 1425.184020547399996, 99.92021504015251310 ) ) ;
#53804 = CARTESIAN_POINT ( 'NONE',  ( -7.321455911854999776, 1516.545806094630279, 211.6076919691270177 ) ) ;
#53805 = AXIS2_PLACEMENT_3D ( 'NONE', #49650, #50209, #8718 ) ;
#53806 = LINE ( 'NONE', #61108, #19406 ) ;
#53807 = CARTESIAN_POINT ( 'NONE',  ( -32.18001475150000346, 1422.275299834130237, 259.4130713564979942 ) ) ;
#53808 = CARTESIAN_POINT ( 'NONE',  ( 2.875920673130000438, 1485.134067338089835, 220.2246146252990115 ) ) ;
#53809 = CARTESIAN_POINT ( 'NONE',  ( 29.09134681033120273, 1509.695701322400055, 209.5707846826050229 ) ) ;
#53810 = CARTESIAN_POINT ( 'NONE',  ( 20.12205423489999845, 1473.683723071389977, 208.1594102018889885 ) ) ;
#53811 = CARTESIAN_POINT ( 'NONE',  ( 32.75710912790000151, 1451.616054398930146, 135.6209638249980003 ) ) ;
#53812 = ORIENTED_EDGE ( 'NONE', *, *, #88500, .T. ) ;
#53813 = CARTESIAN_POINT ( 'NONE',  ( -2.500000000000000000, 1432.334889290770207, 157.4941654934979738 ) ) ;
#53814 = CARTESIAN_POINT ( 'NONE',  ( 14.09486193512188557, 1514.059034343702706, 225.7345132044199545 ) ) ;
#53815 = CARTESIAN_POINT ( 'NONE',  ( 5.969656829619999883, 1509.201939557829974, 238.6262948603979908 ) ) ;
#53816 = VERTEX_POINT ( 'NONE', #50658 ) ;
#53817 = ORIENTED_EDGE ( 'NONE', *, *, #90299, .T. ) ;
#53818 = CARTESIAN_POINT ( 'NONE',  ( 9.020493505376890653, 1451.396381989520023, 211.2518042107480198 ) ) ;
#53819 = CARTESIAN_POINT ( 'NONE',  ( 5.161277909749999893, 1424.205379146819951, 193.2953227953989881 ) ) ;
#53820 = EDGE_LOOP ( 'NONE', ( #16617, #5872, #90947, #91272, #3660, #40413, #28597, #75161, #94568, #70748, #87395, #25361, #63174, #109387 ) ) ;
#53821 = CARTESIAN_POINT ( 'NONE',  ( -2.769884583023930258, 1507.289917905509810, 221.6734208851810308 ) ) ;
#53822 = CARTESIAN_POINT ( 'NONE',  ( -5.836690765424191518, 1419.530734798173626, 194.8705258415808430 ) ) ;
#53823 = AXIS2_PLACEMENT_3D ( 'NONE', #49232, #57087, #66598 ) ;
#53824 = CARTESIAN_POINT ( 'NONE',  ( -1.430539248151910137, 1444.328264662749916, 199.1703804428329931 ) ) ;
#53825 = CARTESIAN_POINT ( 'NONE',  ( -4.681481053319999752, 1470.480737942429869, 234.7256992237980171 ) ) ;
#53826 = CARTESIAN_POINT ( 'NONE',  ( 1.760102192101790086, 1421.041668313049968, 183.1006875787430204 ) ) ;
#53827 = CARTESIAN_POINT ( 'NONE',  ( 10.34950197149999873, 1451.639534151889848, 207.2650128789090047 ) ) ;
#53828 = CARTESIAN_POINT ( 'NONE',  ( 3.956753969209999777, 1501.434984088090005, 230.1161809861990264 ) ) ;
#53829 = CARTESIAN_POINT ( 'NONE',  ( 14.76019812800000075, 1485.703140196630102, 225.4605170203979867 ) ) ;
#53830 = ORIENTED_EDGE ( 'NONE', *, *, #35983, .F. ) ;
#53831 = CARTESIAN_POINT ( 'NONE',  ( -5.008848238024999233, 1516.858456333729919, 204.1217621043670079 ) ) ;
#53832 = CARTESIAN_POINT ( 'NONE',  ( 3.463767257884999839, 1517.014196759610059, 210.8246003415769962 ) ) ;
#53833 = ORIENTED_EDGE ( 'NONE', *, *, #47341, .F. ) ;
#53834 = CARTESIAN_POINT ( 'NONE',  ( 11.85939795343059977, 1431.868251362790033, 149.9622777773220150 ) ) ;
#53835 = EDGE_CURVE ( 'NONE', #60506, #77151, #91818, .T. ) ;
#53836 = CARTESIAN_POINT ( 'NONE',  ( 5.129994116337838861, 1511.406468244438429, 217.6882656312603785 ) ) ;
#53837 = ORIENTED_EDGE ( 'NONE', *, *, #20664, .F. ) ;
#53838 = CARTESIAN_POINT ( 'NONE',  ( -0.3329474807077908993, 1507.873469256806402, 221.0089344692910061 ) ) ;
#53839 = EDGE_CURVE ( 'NONE', #5409, #31217, #10989, .T. ) ;
#53840 = CARTESIAN_POINT ( 'NONE',  ( -17.22592482065197927, 1443.501467202829190, 162.9227486220069920 ) ) ;
#53841 = CARTESIAN_POINT ( 'NONE',  ( 4.922541436569999540, 1508.072814005929786, 235.9300658385979830 ) ) ;
#53842 = VECTOR ( 'NONE', #84420, 1000.000000000000114 ) ;
#53843 = CARTESIAN_POINT ( 'NONE',  ( -10.33479253082609972, 1470.226221615439954, 212.6830489766190055 ) ) ;
#53844 = CARTESIAN_POINT ( 'NONE',  ( -5.307042958110000264, 1425.580209374029891, 186.3543675766980243 ) ) ;
#53845 = CARTESIAN_POINT ( 'NONE',  ( 4.832498183603440189, 1410.233947744540046, 269.8672858344739893 ) ) ;
#53846 = CARTESIAN_POINT ( 'NONE',  ( -108.5296511849999916, 1386.299881632349980, 297.3615022879590128 ) ) ;
#53847 = CARTESIAN_POINT ( 'NONE',  ( -5.716297456320000414, 1474.267417701390059, 199.6561424594189873 ) ) ;
#53848 = CARTESIAN_POINT ( 'NONE',  ( -2.351942935348799946, 1422.085795762910038, 193.1347480034229989 ) ) ;
#53849 = CARTESIAN_POINT ( 'NONE',  ( -16.49045045709999968, 1379.616809272110004, 208.4493337902689802 ) ) ;
#53850 = CARTESIAN_POINT ( 'NONE',  ( 0.02372484621392087142, 1410.241830673391405, 233.2188489835018004 ) ) ;
#53852 = LINE ( 'NONE', #2342, #26082 ) ;
#53851 = CARTESIAN_POINT ( 'NONE',  ( -15.00012675720000033, 1503.680446340089929, 208.8094518185369850 ) ) ;
#53853 = CARTESIAN_POINT ( 'NONE',  ( 11.29467570687139855, 1422.466426227199918, 207.0751064078369836 ) ) ;
#53854 = AXIS2_PLACEMENT_3D ( 'NONE', #10642, #35281, #96296 ) ;
#53855 = CARTESIAN_POINT ( 'NONE',  ( 18.01326382707690144, 1424.078348992020210, 225.1918633016099704 ) ) ;
#53856 = CARTESIAN_POINT ( 'NONE',  ( -7.569982699715000152, 1513.743447518339963, 202.8797921858770223 ) ) ;
#53857 = VERTEX_POINT ( 'NONE', #92645 ) ;
#53858 = CARTESIAN_POINT ( 'NONE',  ( 9.019386498959999443, 1419.938649402030023, 248.0989692945980210 ) ) ;
#53859 = CARTESIAN_POINT ( 'NONE',  ( 19.74623141735625254, 1455.440022657526697, 226.3245780267467921 ) ) ;
#53860 = CARTESIAN_POINT ( 'NONE',  ( -72.87732534374360682, 1385.014528329849782, 298.0934590963260007 ) ) ;
#53861 = EDGE_CURVE ( 'NONE', #21042, #30294, #65270, .T. ) ;
#53862 = CARTESIAN_POINT ( 'NONE',  ( -16.87900699709440033, 1524.382868172804365, 181.2327155136482020 ) ) ;
#53863 = CARTESIAN_POINT ( 'NONE',  ( 5.068064628910000202, 1505.106222020589939, 220.8372522273990057 ) ) ;
#53864 = CARTESIAN_POINT ( 'NONE',  ( -14.95539309770000003, 1415.677402225710011, 211.5193032282590195 ) ) ;
#53866 = EDGE_LOOP ( 'NONE', ( #50301, #28320, #2178, #56259 ) ) ;
#53865 = CARTESIAN_POINT ( 'NONE',  ( 0.3115382523218440114, 1515.152701004710025, 204.7946991408759914 ) ) ;
#53867 = CARTESIAN_POINT ( 'NONE',  ( -15.88437691653640726, 1415.959283172465575, 209.7365679856393399 ) ) ;
#53868 = AXIS2_PLACEMENT_3D ( 'NONE', #35819, #8946, #26293 ) ;
#53869 = CARTESIAN_POINT ( 'NONE',  ( -24.25306927760000164, 1442.945495109479907, 211.8921142785780205 ) ) ;
#53870 = CARTESIAN_POINT ( 'NONE',  ( -15.92986844570000038, 1416.139044365829932, 209.7537133023089950 ) ) ;
#53871 = CARTESIAN_POINT ( 'NONE',  ( -12.03882787510478991, 1391.913092977432598, 209.7302847345281407 ) ) ;
#53872 = CARTESIAN_POINT ( 'NONE',  ( 14.76985291543500090, 1513.863307887919973, 224.0959146767670234 ) ) ;
#53873 = CARTESIAN_POINT ( 'NONE',  ( -8.888076702530000262, 1441.588620940000283, 186.2917108085980260 ) ) ;
#53874 = CARTESIAN_POINT ( 'NONE',  ( -0.05095195904217150046, 1508.992415879220061, 179.2594346809810020 ) ) ;
#53875 = CARTESIAN_POINT ( 'NONE',  ( 13.15671565689999944, 1428.802034784529951, 222.6511392629980151 ) ) ;
#53876 = CARTESIAN_POINT ( 'NONE',  ( 12.10956687129965914, 1433.934677003899651, 149.7611593085945287 ) ) ;
#53877 = CARTESIAN_POINT ( 'NONE',  ( 12.57627033670000039, 1417.420077678930056, 229.0684564266980203 ) ) ;
#53878 = B_SPLINE_CURVE_WITH_KNOTS ( 'NONE', 3,
 ( #71192, #52721, #11271, #78465 ),
 .UNSPECIFIED., .F., .F.,
 ( 4, 4 ),
 ( 0.000000000000000000, 0.0002220129587134773411 ),
 .UNSPECIFIED. ) ;
#53879 = CARTESIAN_POINT ( 'NONE',  ( 9.660635392548039491, 1469.975679021050155, 211.9824950547769902 ) ) ;
#53880 = CARTESIAN_POINT ( 'NONE',  ( -16.10352984969999923, 1459.579123770429760, 228.9550806997980033 ) ) ;
#53881 = CARTESIAN_POINT ( 'NONE',  ( -7.338411997524999286, 1517.170512887980067, 206.6372682748769876 ) ) ;
#53882 = CARTESIAN_POINT ( 'NONE',  ( 46.08680262619999723, 1436.858513228260108, 267.5959981427980097 ) ) ;
#53883 = CARTESIAN_POINT ( 'NONE',  ( -17.17898592970000138, 1409.512963795129963, 223.3525532678980312 ) ) ;
#53884 = EDGE_CURVE ( 'NONE', #48466, #94675, #18227, .T. ) ;
#53885 = CARTESIAN_POINT ( 'NONE',  ( 17.95374924460000088, 1435.124687891739995, 145.3138471459980110 ) ) ;
#53886 = CARTESIAN_POINT ( 'NONE',  ( 23.15253664929999999, 1508.008712515430034, 194.0884348405979836 ) ) ;
#53887 = CARTESIAN_POINT ( 'NONE',  ( 29.52808524179070915, 1509.958252097621653, 207.2780779163062732 ) ) ;
#53888 = CARTESIAN_POINT ( 'NONE',  ( 3.932775080253070321, 1448.980696629100066, 184.2693358254829832 ) ) ;
#53889 = CARTESIAN_POINT ( 'NONE',  ( -45.67177343128329881, 1440.913044206929953, 266.1885934837860077 ) ) ;
#53890 = CARTESIAN_POINT ( 'NONE',  ( 6.522563371079319161, 1422.592431503280068, 144.1528597180129907 ) ) ;
#53891 = CARTESIAN_POINT ( 'NONE',  ( -41.16998753702269198, 1440.713062679589939, 135.8149046629820305 ) ) ;
#53892 = EDGE_CURVE ( 'NONE', #109119, #1510, #14278, .T. ) ;
#53893 = CARTESIAN_POINT ( 'NONE',  ( -13.75903336753860096, 1409.893113308419970, 226.9379569541520141 ) ) ;
#53894 = CARTESIAN_POINT ( 'NONE',  ( 13.90334061950979994, 1519.913060387329779, 234.5717402564966960 ) ) ;
#53895 = CARTESIAN_POINT ( 'NONE',  ( -11.99325728100000177, 1441.735653989300090, 187.5768839477979668 ) ) ;
#53896 = CARTESIAN_POINT ( 'NONE',  ( -7.542953837611409362, 1384.718779688529821, 219.0831055481480121 ) ) ;
#53897 = CARTESIAN_POINT ( 'NONE',  ( -33.93529465689999824, 1436.159566638689967, 136.2997917595980084 ) ) ;
#53898 = CARTESIAN_POINT ( 'NONE',  ( -8.196734810833769203, 1456.222872452821093, 227.1897744870182123 ) ) ;
#53899 = VERTEX_POINT ( 'NONE', #5899 ) ;
#53900 = CARTESIAN_POINT ( 'NONE',  ( 5.707844853767014115, 1510.531931295588947, 216.6676495880327309 ) ) ;
#53901 = CARTESIAN_POINT ( 'NONE',  ( -11.73233732503739901, 1409.322762634679975, 218.3858963278959777 ) ) ;
#53902 = CARTESIAN_POINT ( 'NONE',  ( 33.82780500856040362, 1523.429859730330463, 197.6825146852528974 ) ) ;
#53903 = CARTESIAN_POINT ( 'NONE',  ( -13.09068094276110017, 1508.241445731279782, 209.4862166979580138 ) ) ;
#53904 = DIRECTION ( 'NONE',  ( 0.000000000000000000, 0.000000000000000000, 1.000000000000000000 ) ) ;
#53905 = CARTESIAN_POINT ( 'NONE',  ( -30.24616429450000155, 1467.598942926229938, 268.0936122245979618 ) ) ;
#53906 = CARTESIAN_POINT ( 'NONE',  ( -30.25946001110623129, 1524.776010967693765, 196.4597699223641314 ) ) ;
#53907 = CARTESIAN_POINT ( 'NONE',  ( 0.1905848792942149983, 1419.866718629129991, 184.1430962726229836 ) ) ;
#53908 = CARTESIAN_POINT ( 'NONE',  ( 18.98249322453000332, 1526.382868172864164, 232.9711420821685692 ) ) ;
#53909 = CARTESIAN_POINT ( 'NONE',  ( -107.6419135281290096, 1384.586188811220154, 311.2437287102239907 ) ) ;
#53910 = CARTESIAN_POINT ( 'NONE',  ( -30.87778110501150408, 1384.970453077349930, 206.0489399718400136 ) ) ;
#53911 = CYLINDRICAL_SURFACE ( 'NONE', #31831, 2.000000000000003553 ) ;
#53912 = CARTESIAN_POINT ( 'NONE',  ( 11.96393163419999972, 1414.971352895729979, 220.7371289333979973 ) ) ;
#53913 = CARTESIAN_POINT ( 'NONE',  ( -9.400735251840000473, 1432.346452651970139, 153.1462979580980175 ) ) ;
#53914 = CARTESIAN_POINT ( 'NONE',  ( 0.7910245917146940808, 1426.918876941764893, 137.0999999980980135 ) ) ;
#53915 = CARTESIAN_POINT ( 'NONE',  ( 2.641027167160353795, 1370.251786685222896, 206.7745814587238158 ) ) ;
#53916 = CARTESIAN_POINT ( 'NONE',  ( -3.611928636060000031, 1508.978187703030244, 180.0004874563979911 ) ) ;
#53917 = CARTESIAN_POINT ( 'NONE',  ( -23.82773097239999771, 1410.240654944330117, 208.3948794269180098 ) ) ;
#53918 = CLOSED_SHELL ( 'NONE', ( #82885, #92446, #95326, #40379, #11390, #54366, #13853, #82298, #11693, #13986, #14735, #82091, #79479, #64716, #76820, #44565, #50321, #31002, #84977, #5782, #14611, #91208, #63504, #10537, #9185, #102711, #48827, #24057, #81242, #1458, #47339, #1931, #107659, #59103, #85487, #27526, #99272, #89951, #99264, #77563, #108231, #48783, #22798, #82293, #3319, #57610, #14636, #61756, #18581, #71372, #61928, #61838, #51405, #72758, #38309, #59879, #95883, #96574, #106982, #30408, #106894, #18728, #7109, #85576, #93838, #102089, #100675, #14497, #49682, #84032, #50132, #67872, #80388, #40588, #70785, #101307, #73689, #62742, #85670, #88106, #42692, #28217, #65910, #24677, #60552, #35578, #38148, #21064, #66274, #57901, #24367, #12718, #75492, #71514, #3036, #43934, #53527, #25525, #21359, #13968, #23333, #5091, #10330, #50746, #47136, #72851, #35067, #31945, #17007, #106414, #53662, #98732, #10473, #81442, #65300, #17394, #66892, #55098, #71273, #75596, #45763, #70122, #63790, #27909, #103303, #52325, #28170, #41134, #82232, #74169, #103529, #60066, #102012, #6395, #65168, #74958, #57115, #104746, #71387, #41553, #56920, #96006, #90480, #10572, #36613, #30129, #15510, #36328, #105367, #91106, #90430, #82655, #38500, #50141, #109064, #2668, #7328, #70, #82499, #40436, #33763, #7025, #104712, #101564, #12852, #18184, #73513, #85955, #47485, #106430, #12367, #84852, #14768, #71996, #37785, #5935, #87299, #52339, #78612, #74, #36964, #30987, #70282, #98444, #69274, #101381, #12736, #81266, #11067, #50634, #51421, #4281, #89679, #23478, #42057, #81099, #97368, #80843, #108361, #37750, #97337, #43415, #1257, #46132, #52149, #42941, #7319, #13680, #8249, #15859, #104381, #72176, #81091, #29632, #41140, #45489, #57245, #89292, #61016, #28080, #89330, #59883, #110283, #22519, #18667, #87904, #100191, #102096, #48675, #63087, #47647, #50311, #56510, #45635, #93086, #76689, #36756, #108419, #79249, #71675, #94270, #45342, #13949, #74051, #74932, #84541, #58372, #15941, #52027, #59031, #59706, #103081, #52237, #107290, #2949, #29146, #22529, #45381, #89799, #98802, #42814, #20507, #23570, #108191, #84276, #15168, #33323, #12453, #81758, #12400, #68270, #58008, #12627, #98206, #84380, #96787, #67130, #95152, #105146, #61417, #94576, #74026, #75422, #34911, #69232, #65257, #89852, #25406, #31797, #2421, #6371, #49450, #35365, #65217, #1691, #108131, #84282, #5794, #93829, #59253, #13198, #35209, #100000, #60237, #61074, #3049, #58241, #38747, #46248, #22138, #89210, #108411, #1453, #35662, #73429, #101414, #46263, #102800, #74020, #102806, #101598, #20953, #87042, #42645, #78987, #64572, #54809, #38013, #20199, #109845, #26233, #75104, #70817, #105545, #2565, #74929, #98655, #45305, #85768, #853, #76125, #52849, #82633, #51506, #58499, #26153, #93959, #28858, #26750, #58842, #87854, #36355, #57240, #76571, #82648, #109541, #59307, #52941, #73577, #67302, #109701, #35820, #101081, #101678, #85621, #15818, #84242, #92758, #24036, #100656, #81870, #2393, #69322, #63198, #16491, #47397, #107615, #59123, #55591, #108942, #39025, #87063, #91863, #16141, #46880, #34704, #63473, #80001, #98291, #7149, #74201, #79741, #52280, #52571, #985, #66758, #66083, #1541, #1794, #108123, #103313, #32427, #15301, #84413, #94469, #41320, #59434, #7164, #75987, #62708, #38591, #82839, #9083, #33819, #64452, #76749, #87139, #109658, #35073, #58753, #100056, #12544, #50891, #29429, #105028, #68289, #80293, #56193, #91823, #3723, #22168, #77548, #75292, #71282, #22658, #6250, #79779, #22678, #79711, #107001, #30299, #352, #43800, #60648, #80529, #13056, #55218, #67190, #40930, #85275, #110083, #59141, #68608, #109341, #16099, #57606, #92629, #26032, #74308, #18776, #15696, #81595, #11488, #68590, #19437, #89448, #76927, #72075, #56216, #23617, #38663, #75528, #58306, #97281, #9582, #76161, #65326, #63061, #4942, #51699, #46420, #75548, #90584, #17170, #26188, #31635, #62499, #5491, #84861, #107179, #12491, #93616, #99712, #67616, #66411, #8428, #46289, #63805, #78911, #27491, #61308, #49410, #47029, #99274, #69378, #26854, #68870, #74210, #64464, #67522, #11729, #78779, #89979, #1641, #86261, #78059, #1104, #14588, #37522, #70150, #84397, #39846, #41155, #72441, #10447, #32943, #76753, #34308, #96698, #71545, #38139, #71557, #62453, #79104, #32915, #104965, #28275, #76341, #26259, #89672, #50550, #27531, #192, #4882, #100942, #13178, #4546, #98118, #86995, #52886, #59921, #76172, #6875, #48612, #4355, #89896, #7186, #89194, #98809, #88968, #61901, #56303, #22646, #99911, #76789, #24477, #12435, #3151, #99909, #39200, #107926, #19258, #35894, #101074, #7051, #23398, #61034, #2912, #30164, #39745, #30764, #41920, #48296, #74765 ) ) ;
#53919 = CARTESIAN_POINT ( 'NONE',  ( 17.16585544539999830, 1415.931391677429929, 203.8399221076179799 ) ) ;
#53920 = CARTESIAN_POINT ( 'NONE',  ( -11.83559671189999918, 1415.245980412430072, 195.4349966776979670 ) ) ;
#53921 = CARTESIAN_POINT ( 'NONE',  ( -0.4580525536099979700, 1421.902170014840067, 193.5483135711990030 ) ) ;
#53922 = CARTESIAN_POINT ( 'NONE',  ( 22.91612949529999810, 1409.877774706829769, 211.9495050228480011 ) ) ;
#53923 = CARTESIAN_POINT ( 'NONE',  ( -106.8632684893990046, 1391.913060387289988, 306.3664403480210012 ) ) ;
#53924 = CARTESIAN_POINT ( 'NONE',  ( 10.22890245830000033, 1453.871432809989983, 189.8803906307990133 ) ) ;
#53925 = CARTESIAN_POINT ( 'NONE',  ( -5.369163863342579113, 1427.164133926789873, 153.2148359060929863 ) ) ;
#53927 = CARTESIAN_POINT ( 'NONE',  ( -11.25209998319999904, 1378.783920428300007, 203.9551270864290302 ) ) ;
#53926 = DIRECTION ( 'NONE',  ( 0.9455185755993178454, 0.000000000000000000, -0.3255681544571537578 ) ) ;
#53928 = FACE_OUTER_BOUND ( 'NONE', #23825, .T. ) ;
#53929 = FACE_OUTER_BOUND ( 'NONE', #81096, .T. ) ;
#53930 = CARTESIAN_POINT ( 'NONE',  ( -15.36119880041499997, 1420.424379057629949, 211.0657862475889885 ) ) ;
#53931 = CARTESIAN_POINT ( 'NONE',  ( -22.87440001419999902, 1415.994159370630086, 211.5426778979280016 ) ) ;
#53932 = CARTESIAN_POINT ( 'NONE',  ( -1.244790792857130013, 1420.670971867490152, 184.3462124761589962 ) ) ;
#53933 = CIRCLE ( 'NONE', #10976, 2.000000000000003553 ) ;
#53934 = CARTESIAN_POINT ( 'NONE',  ( -2.295485539174999978, 1516.651306816259876, 204.1261199623870368 ) ) ;
#53935 = CARTESIAN_POINT ( 'NONE',  ( -23.60070218908893480, 1435.435984317846305, 213.5551715964222979 ) ) ;
#53936 = CARTESIAN_POINT ( 'NONE',  ( -18.40312947852670078, 1485.456034533320008, 189.1500380655480171 ) ) ;
#53937 = CARTESIAN_POINT ( 'NONE',  ( -9.241005602170000444, 1423.079004508810158, 209.8534315543390107 ) ) ;
#53938 = CARTESIAN_POINT ( 'NONE',  ( -4.274194808379749411, 1441.075114845419876, 157.3205200675280082 ) ) ;
#53940 = VERTEX_POINT ( 'NONE', #41700 ) ;
#53939 = CARTESIAN_POINT ( 'NONE',  ( -60.13904085021329848, 1379.723828619409915, 265.9902606016499931 ) ) ;
#53941 = EDGE_LOOP ( 'NONE', ( #68540, #62041, #75303 ) ) ;
#53942 = CARTESIAN_POINT ( 'NONE',  ( -20.69303424980000372, 1486.764600954290017, 209.1218459616989946 ) ) ;
#53943 = ORIENTED_EDGE ( 'NONE', *, *, #21399, .F. ) ;
#53944 = DIRECTION ( 'NONE',  ( 5.980589973904019347E-17, -1.000000000000000000, 1.736889445713099699E-16 ) ) ;
#53945 = CARTESIAN_POINT ( 'NONE',  ( -109.4841057800000073, 1384.929175104179876, 311.2840925992589973 ) ) ;
#53947 = CARTESIAN_POINT ( 'NONE',  ( 4.665393456780000392, 1427.510941591930077, 123.0297916884979941 ) ) ;
#53946 = CARTESIAN_POINT ( 'NONE',  ( 0.8041763403130000043, 1426.566393376330097, 144.1938086916980239 ) ) ;
#53948 = CARTESIAN_POINT ( 'NONE',  ( 27.74152896581870209, 1446.393007474679962, 137.1637341980689939 ) ) ;
#53949 = CIRCLE ( 'NONE', #78939, 2.000000000000003109 ) ;
#53950 = CARTESIAN_POINT ( 'NONE',  ( 1.765878059339999862, 1488.173956647230170, 181.9972861322979725 ) ) ;
#53951 = CARTESIAN_POINT ( 'NONE',  ( -1.131513733160000035, 1469.206973085589880, 219.1156501392690075 ) ) ;
#53952 = CARTESIAN_POINT ( 'NONE',  ( 7.289026058960000221, 1410.103226084029757, 230.7281513803979749 ) ) ;
#53953 = SURFACE_SIDE_STYLE ('',( #19178 ) ) ;
#53954 = CARTESIAN_POINT ( 'NONE',  ( 6.949265646015000186, 1517.089216728169959, 212.5747629931370000 ) ) ;
#53955 = CARTESIAN_POINT ( 'NONE',  ( 41.56943536068610001, 1444.920853409699930, 134.0999999984259716 ) ) ;
#53957 = AXIS2_PLACEMENT_3D ( 'NONE', #109610, #33425, #24475 ) ;
#53956 = CARTESIAN_POINT ( 'NONE',  ( -12.86537294912139906, 1421.504292501779901, 209.5023190072500086 ) ) ;
#53958 = CARTESIAN_POINT ( 'NONE',  ( -9817.198717879920878, 2837.742859910730203, 1424.354596106799818 ) ) ;
#53959 = EDGE_LOOP ( 'NONE', ( #17205, #109508, #83375, #44297 ) ) ;
#53960 = CARTESIAN_POINT ( 'NONE',  ( 13.85413686636590036, 1434.981310748690021, 148.6151550497299922 ) ) ;
#53961 = DIRECTION ( 'NONE',  ( -0.1070030146457386366, 0.000000000000000000, -0.9942586961433749204 ) ) ;
#53962 = ORIENTED_EDGE ( 'NONE', *, *, #85411, .T. ) ;
#53963 = ORIENTED_EDGE ( 'NONE', *, *, #62089, .F. ) ;
#53964 = EDGE_LOOP ( 'NONE', ( #78842, #21932, #41123, #43227, #16554 ) ) ;
#53965 = DIRECTION ( 'NONE',  ( 0.1070030146457317810, 0.000000000000000000, -0.9942586961433755866 ) ) ;
#53966 = CARTESIAN_POINT ( 'NONE',  ( -0.9163463255799999541, 1464.976965922729960, 237.2656658263979921 ) ) ;
#53967 = CARTESIAN_POINT ( 'NONE',  ( 21.15490488532373448, 1450.943175079559978, 144.2761602908674945 ) ) ;
#53968 = CARTESIAN_POINT ( 'NONE',  ( -2.924053139080000197, 1485.138221895729885, 183.1581825105979817 ) ) ;
#53969 = CARTESIAN_POINT ( 'NONE',  ( 1.334158748144050000, 1465.731125543059989, 198.1841065779290147 ) ) ;
#53970 = AXIS2_PLACEMENT_3D ( 'NONE', #31241, #65424, #31791 ) ;
#53971 = CARTESIAN_POINT ( 'NONE',  ( -13.19353006659999927, 1379.589451595169976, 208.3384645246609921 ) ) ;
#53972 = CARTESIAN_POINT ( 'NONE',  ( -28.30903825226335613, 1379.623442209230689, 212.7910287074695646 ) ) ;
#53973 = CARTESIAN_POINT ( 'NONE',  ( 4.227393864177829919, 1446.270024740570079, 165.6814982219489991 ) ) ;
#53974 = CARTESIAN_POINT ( 'NONE',  ( -5.371346839171279974, 1516.551188146539971, 218.7599618298110045 ) ) ;
#53975 = ORIENTED_EDGE ( 'NONE', *, *, #96912, .F. ) ;
#53976 = CARTESIAN_POINT ( 'NONE',  ( 3.251394362135000105, 1516.757508073510053, 207.4061414411269766 ) ) ;
#53977 = ORIENTED_EDGE ( 'NONE', *, *, #80072, .F. ) ;
#53978 = CARTESIAN_POINT ( 'NONE',  ( 26.67958435172820231, 1440.913060387330006, 244.1583708425140173 ) ) ;
#53979 = CARTESIAN_POINT ( 'NONE',  ( 11.75011454135350064, 1479.292909357789995, 208.4591119443479954 ) ) ;
#53980 = ORIENTED_EDGE ( 'NONE', *, *, #53441, .F. ) ;
#53981 = CARTESIAN_POINT ( 'NONE',  ( -7.512750272452770162, 1509.038617453179995, 203.6086426773880191 ) ) ;
#53982 = CARTESIAN_POINT ( 'NONE',  ( -14.27906159650000006, 1409.411696205929957, 191.9865084241980071 ) ) ;
#53983 = CARTESIAN_POINT ( 'NONE',  ( -61.23078504541961564, 1379.729633516930562, 268.1594380621943969 ) ) ;
#53985 = CARTESIAN_POINT ( 'NONE',  ( 19.93504378490000306, 1473.377435931889750, 206.2335637307590162 ) ) ;
#53984 = CARTESIAN_POINT ( 'NONE',  ( -24.67145409169999581, 1441.066589285630016, 210.6900421876080145 ) ) ;
#53986 = CARTESIAN_POINT ( 'NONE',  ( -8.414060040230721071, 1436.602101947940128, 214.1363812467849925 ) ) ;
#53987 = DIRECTION ( 'NONE',  ( -0.6736849260863841948, 0.000000000000000000, 0.7390186874254148774 ) ) ;
#53988 = CARTESIAN_POINT ( 'NONE',  ( -12.84999653021897359, 1434.699229520601421, 147.0734321989873763 ) ) ;
#53989 = DIRECTION ( 'NONE',  ( -0.9998780035959983215, 8.712314624148121749E-33, 0.01561979272847786350 ) ) ;
#53990 = CARTESIAN_POINT ( 'NONE',  ( -4.542951805869999582, 1507.945432530890002, 220.8303236145989956 ) ) ;
#53992 = CARTESIAN_POINT ( 'NONE',  ( -1.661949936129999861, 1498.085228650090130, 200.7325862837689954 ) ) ;
#53991 = CARTESIAN_POINT ( 'NONE',  ( 9.888958272120000004, 1463.772371499329893, 232.6549650238979723 ) ) ;
#53994 = CARTESIAN_POINT ( 'NONE',  ( 2.874588922665000545, 1516.606339319019980, 215.6687976528169770 ) ) ;
#53993 = STYLED_ITEM ( 'NONE', ( #102094 ), #17149 ) ;
#53995 = FACE_OUTER_BOUND ( 'NONE', #11364, .T. ) ;
#53996 = CARTESIAN_POINT ( 'NONE',  ( 5.523053254439029836, 1510.639750819960000, 216.6759469071630235 ) ) ;
#53997 = EDGE_CURVE ( 'NONE', #67084, #71877, #3893, .T. ) ;
#53998 = DIRECTION ( 'NONE',  ( 0.1010290445074205484, 0.000000000000000000, 0.9948834766775040972 ) ) ;
#53999 = CARTESIAN_POINT ( 'NONE',  ( -4.997250192034999650, 1516.727068157269969, 212.3866247496169990 ) ) ;
#54000 = B_SPLINE_CURVE_WITH_KNOTS ( 'NONE', 3,
 ( #90174, #74514, #40883, #58257, #109213, #15649, #83988, #31930, #49855, #66124, #13456, #7288, #22399, #100248, #47645, #23526, #81774, #72854, #57719, #56599, #106988, #90733 ),
 .UNSPECIFIED., .F., .F.,
 ( 4, 3, 3, 3, 3, 3, 3, 4 ),
 ( 5.710169621319999251E-17, 1.340335073529090204, 2.650534160768720060, 3.343413429321489883, 4.426679877969149857, 5.556753218544390194, 6.458769871279841368, 6.686826559119630531 ),
 .UNSPECIFIED. ) ;
#54001 = CARTESIAN_POINT ( 'NONE',  ( -11.56497786232949920, 1482.641537608759791, 206.2850871889860116 ) ) ;
#54002 = CARTESIAN_POINT ( 'NONE',  ( -9.956645445956299412, 1517.051704408389924, 185.5808665542169820 ) ) ;
#54004 = ORIENTED_EDGE ( 'NONE', *, *, #53067, .F. ) ;
#54003 = CARTESIAN_POINT ( 'NONE',  ( -92.33864210410000339, 1388.280693857359893, 295.1786243173589810 ) ) ;
#54005 = CARTESIAN_POINT ( 'NONE',  ( -17.19739463999614060, 1525.960063244517187, 236.2603809477411119 ) ) ;
#54006 = CARTESIAN_POINT ( 'NONE',  ( 8.718798080230000025, 1462.898524229230134, 232.0462147568979958 ) ) ;
#54007 = EDGE_CURVE ( 'NONE', #32529, #45568, #93217, .T. ) ;
#54008 = CARTESIAN_POINT ( 'NONE',  ( -11.02044644817170749, 1489.051081239631230, 214.3262939459677341 ) ) ;
#54009 = CARTESIAN_POINT ( 'NONE',  ( -15.61208392800000055, 1415.847366682379970, 208.3828643427310112 ) ) ;
#54010 = CARTESIAN_POINT ( 'NONE',  ( 2.190948469950000366, 1413.140243969430003, 231.9855873312979782 ) ) ;
#54011 = CARTESIAN_POINT ( 'NONE',  ( -22.42321380570000144, 1451.074909188629817, 219.8762963758979936 ) ) ;
#54012 = CIRCLE ( 'NONE', #23504, 9.000000000000007105 ) ;
#54014 = CARTESIAN_POINT ( 'NONE',  ( 5.372020988824510290, 1428.211245194210051, 153.7601568675739827 ) ) ;
#54013 = CARTESIAN_POINT ( 'NONE',  ( -23.59318075118283531, 1411.097233843727054, 206.6698092424495599 ) ) ;
#54015 = CARTESIAN_POINT ( 'NONE',  ( -9.279725527415630282, 1449.470959070069739, 208.1994392316480003 ) ) ;
#54016 = CARTESIAN_POINT ( 'NONE',  ( -104.4920613472269935, 1380.551098421130064, 307.6454722610029648 ) ) ;
#54017 = ORIENTED_EDGE ( 'NONE', *, *, #107194, .F. ) ;
#54018 = CARTESIAN_POINT ( 'NONE',  ( 3.449149195745000007, 1516.947419719950176, 204.4980579627370219 ) ) ;
#54019 = CARTESIAN_POINT ( 'NONE',  ( 1.327512982840000078, 1406.079504512129915, 269.0450431314979483 ) ) ;
#54020 = CARTESIAN_POINT ( 'NONE',  ( -1.842962231260000028, 1515.219201591190085, 213.4472514034090125 ) ) ;
#54021 = CARTESIAN_POINT ( 'NONE',  ( 43.48865956637619945, 1446.139721542620009, 270.3367078615700052 ) ) ;
#54022 = CARTESIAN_POINT ( 'NONE',  ( 2.478548031669999929, 1437.283191558279896, 157.6756789685979925 ) ) ;
#54023 =( BOUNDED_CURVE ( )  B_SPLINE_CURVE ( 3, ( #90905, #46730, #37760, #55682 ),
 .UNSPECIFIED., .F., .F. ) 
 B_SPLINE_CURVE_WITH_KNOTS ( ( 4, 4 ),
 ( 1.020731224408165883, 2.120869708383349650 ),
 .UNSPECIFIED. ) 
 CURVE ( )  GEOMETRIC_REPRESENTATION_ITEM ( )  RATIONAL_B_SPLINE_CURVE ( ( 1.000000000000000000, 0.9016588854088134486, 0.9016588854088134486, 1.000000000000000000 ) ) 
 REPRESENTATION_ITEM ( '' )  );
#54024 = CARTESIAN_POINT ( 'NONE',  ( 11.60004869886325451, 1423.252659004586349, 137.0072935635085116 ) ) ;
#54025 = CIRCLE ( 'NONE', #68316, 1.000000000000001332 ) ;
#54026 = CARTESIAN_POINT ( 'NONE',  ( -43.52170781963269519, 1440.913060407769990, 263.8029430533659934 ) ) ;
#54027 = CARTESIAN_POINT ( 'NONE',  ( 36.90203174740399561, 1449.595941984130150, 136.2855500997040110 ) ) ;
#54028 = CARTESIAN_POINT ( 'NONE',  ( -30.31940284292398857, 1523.382868172864164, 222.4933038710547919 ) ) ;
#54029 = DIRECTION ( 'NONE',  ( 0.000000000000000000, 0.000000000000000000, -1.000000000000000000 ) ) ;
#54030 = CARTESIAN_POINT ( 'NONE',  ( 1.453744393529480039, 1450.692426104239985, 154.2448216313819955 ) ) ;
#54031 = CARTESIAN_POINT ( 'NONE',  ( -21.53712143570596638, 1523.621879633029039, 183.9400870382965820 ) ) ;
#54032 = CARTESIAN_POINT ( 'NONE',  ( 7.105427357599999217E-15, 1418.913060387330006, 172.2701767054979882 ) ) ;
#54033 = ORIENTED_EDGE ( 'NONE', *, *, #100830, .T. ) ;
#54034 = CARTESIAN_POINT ( 'NONE',  ( -26.42894385079999964, 1421.320559242730042, 262.6648722463980334 ) ) ;
#54035 = CARTESIAN_POINT ( 'NONE',  ( -1.441072598602595400, 1450.659596873665123, 182.0284431214944618 ) ) ;
#54036 = CARTESIAN_POINT ( 'NONE',  ( -22.91663120903140083, 1507.606285602550088, 207.6071078552859888 ) ) ;
#54037 = CARTESIAN_POINT ( 'NONE',  ( -1.318284353409999943, 1475.306440821630076, 269.4981144188980124 ) ) ;
#54038 = CARTESIAN_POINT ( 'NONE',  ( -32.05911371000000543, 1451.793557196030179, 134.7701858639979946 ) ) ;
#54039 = CARTESIAN_POINT ( 'NONE',  ( -28.77213280049999966, 1509.917805404830006, 211.3774502238480295 ) ) ;
#54040 = CARTESIAN_POINT ( 'NONE',  ( -3.910181740847316956, 1448.296520225016820, 185.0509912937746719 ) ) ;
#54041 = CARTESIAN_POINT ( 'NONE',  ( -23.12467871438520461, 1384.852336965640006, 222.5014426972579997 ) ) ;
#54042 = CIRCLE ( 'NONE', #36109, 12.50000000000001066 ) ;
#54043 = CARTESIAN_POINT ( 'NONE',  ( -17.80652095830000192, 1415.128105756529976, 207.8722581125280158 ) ) ;
#54044 = CARTESIAN_POINT ( 'NONE',  ( -10.13917572520000121, 1483.516014936390093, 202.7009691187589908 ) ) ;
#54045 = CARTESIAN_POINT ( 'NONE',  ( 26.00338574347900078, 1435.702077567190145, 136.3120532782230043 ) ) ;
#54046 = CARTESIAN_POINT ( 'NONE',  ( -3.088399681877699532, 1396.020909680820068, 219.6995886521329737 ) ) ;
#54047 = AXIS2_PLACEMENT_3D ( 'NONE', #4858, #89969, #73180 ) ;
#54048 = CARTESIAN_POINT ( 'NONE',  ( -3.410009189096530058, 1508.551704408389924, 204.3096965353510086 ) ) ;
#54049 = CARTESIAN_POINT ( 'NONE',  ( -16.42060166099630081, 1409.511629218500048, 225.2012082830180191 ) ) ;
#54050 = CARTESIAN_POINT ( 'NONE',  ( -5.100876313898289993, 1482.122728626309936, 228.9673692973009906 ) ) ;
#54051 = ORIENTED_EDGE ( 'NONE', *, *, #69299, .T. ) ;
#54052 = CARTESIAN_POINT ( 'NONE',  ( -20.61546995289999984, 1508.365016819430139, 190.3615313974979983 ) ) ;
#54053 = CARTESIAN_POINT ( 'NONE',  ( 2.325354419860000021, 1408.994263553030123, 230.2593898277980031 ) ) ;
#54055 = CARTESIAN_POINT ( 'NONE',  ( -14.74158148776499999, 1513.636261293280086, 193.1162984930670063 ) ) ;
#54054 = CARTESIAN_POINT ( 'NONE',  ( 10.66436153279999921, 1425.356347891630094, 112.6539006775979885 ) ) ;
#54056 = DIRECTION ( 'NONE',  ( -1.755985294532469921E-16, 1.000000000000000000, -1.338183447452831989E-16 ) ) ;
#54057 = CARTESIAN_POINT ( 'NONE',  ( -11.23388613411650638, 1445.063428794548372, 205.3674499604519212 ) ) ;
#54058 = CARTESIAN_POINT ( 'NONE',  ( -4.877525054610000410, 1387.235930920489864, 203.5864774107689925 ) ) ;
#54059 = CARTESIAN_POINT ( 'NONE',  ( 7.794108548359999666, 1424.952531890930004, 211.7688989986990009 ) ) ;
#54060 = CARTESIAN_POINT ( 'NONE',  ( -21.26810766760000249, 1485.919195121089842, 201.7808564926190229 ) ) ;
#54061 = CARTESIAN_POINT ( 'NONE',  ( 15.18044682233499998, 1511.791180387469922, 197.3654389570669991 ) ) ;
#54062 = CARTESIAN_POINT ( 'NONE',  ( 11.55221630640000008, 1480.217597331290108, 211.4789166796290090 ) ) ;
#54063 = CARTESIAN_POINT ( 'NONE',  ( -68.69232588285649399, 1379.746858116560134, 280.5557452193770587 ) ) ;
#54064 = CARTESIAN_POINT ( 'NONE',  ( 8.793514412655110135, 1365.053261579362697, 210.6218459617142003 ) ) ;
#54066 = EDGE_LOOP ( 'NONE', ( #35130, #85717, #80908, #71976, #4397, #110073, #45015, #74238 ) ) ;
#54065 = CARTESIAN_POINT ( 'NONE',  ( 7.973908635610000850, 1452.896654755889813, 214.0341050940890000 ) ) ;
#54067 = ORIENTED_EDGE ( 'NONE', *, *, #43312, .T. ) ;
#54068 = CARTESIAN_POINT ( 'NONE',  ( -41.65882839649999880, 1443.939635522049912, 136.1335186928980079 ) ) ;
#54069 = EDGE_CURVE ( 'NONE', #32529, #57665, #62918, .T. ) ;
#54070 = CARTESIAN_POINT ( 'NONE',  ( -13.35522314810000033, 1409.379435056429884, 191.4683303614979764 ) ) ;
#54071 = DIRECTION ( 'NONE',  ( -0.3090169943749383474, 0.000000000000000000, 0.9510565162951566398 ) ) ;
#54072 = CARTESIAN_POINT ( 'NONE',  ( -8.652776140254999859, 1511.435001052829875, 214.5073691319269926 ) ) ;
#54074 = CARTESIAN_POINT ( 'NONE',  ( 0.1596058210269999944, 1486.508833526429953, 181.8147405216979848 ) ) ;
#54073 = CARTESIAN_POINT ( 'NONE',  ( -7.870791249149999835, 1383.842518133449857, 218.8008077258490118 ) ) ;
#54075 = CARTESIAN_POINT ( 'NONE',  ( 20.15452300067990166, 1507.845791525220193, 189.3412703910400126 ) ) ;
#54076 = CARTESIAN_POINT ( 'NONE',  ( 2.621457251729789384, 1517.151704408390060, 190.1820379210428200 ) ) ;
#54077 = CARTESIAN_POINT ( 'NONE',  ( -40.10254738438180055, 1447.671539697419803, 136.3432379383139903 ) ) ;
#54078 = ADVANCED_FACE ( 'NONE', ( #85908 ), #17009, .T. ) ;
#54079 = SURFACE_STYLE_FILL_AREA ( #19311 ) ;
#54080 = CARTESIAN_POINT ( 'NONE',  ( -2.500000000000000000, 1448.349747921640073, 163.1876093918550055 ) ) ;
#54081 = CARTESIAN_POINT ( 'NONE',  ( 9.366452427309480910, 1396.240144116259899, 215.0016878971990195 ) ) ;
#54082 = CARTESIAN_POINT ( 'NONE',  ( 11.93818824289999903, 1433.480083226980014, 149.8972169559980046 ) ) ;
#54083 = CARTESIAN_POINT ( 'NONE',  ( -1.525162025860949955, 1406.078293633129988, 269.0451533397849744 ) ) ;
#54084 = CARTESIAN_POINT ( 'NONE',  ( 41.49211893279999686, 1443.779781417970071, 136.5764383342979897 ) ) ;
#54085 = ORIENTED_EDGE ( 'NONE', *, *, #90745, .T. ) ;
#54086 = DIRECTION ( 'NONE',  ( 0.000000000000000000, 0.000000000000000000, -1.000000000000000000 ) ) ;
#54087 = CARTESIAN_POINT ( 'NONE',  ( 20.72500163403594797, 1525.697946996619521, 233.5887219448511303 ) ) ;
#54088 = VERTEX_POINT ( 'NONE', #60743 ) ;
#54089 = ORIENTED_EDGE ( 'NONE', *, *, #24203, .T. ) ;
#54090 = CARTESIAN_POINT ( 'NONE',  ( -7.219069869235789305, 1424.874073124720098, 212.8049191124847823 ) ) ;
#54091 = CARTESIAN_POINT ( 'NONE',  ( -9.978586514379999883, 1364.539968386210148, 207.6218459616989946 ) ) ;
#54092 = CARTESIAN_POINT ( 'NONE',  ( -4.613762395014999740, 1516.939574742129935, 214.9064842900469898 ) ) ;
#54093 = CARTESIAN_POINT ( 'NONE',  ( 2.841932018395000092, 1512.089957059379913, 216.8946056602869703 ) ) ;
#54094 = ORIENTED_EDGE ( 'NONE', *, *, #4812, .F. ) ;
#54095 = CARTESIAN_POINT ( 'NONE',  ( 8.439944554000000210, 1428.238409027789885, 213.1498827361689905 ) ) ;
#54096 = CARTESIAN_POINT ( 'NONE',  ( -71.62432532130000595, 1379.712643070030026, 285.2199721836589674 ) ) ;
#54097 = CARTESIAN_POINT ( 'NONE',  ( 11.99296739220000063, 1415.426952351230057, 223.0765513814980068 ) ) ;
#54098 = CARTESIAN_POINT ( 'NONE',  ( 3.449149195745000007, 1516.947419719950176, 204.4980579627370219 ) ) ;
#54099 = CARTESIAN_POINT ( 'NONE',  ( -42.06231979437640689, 1440.913089571769888, 269.6487552725350270 ) ) ;
#54100 = CARTESIAN_POINT ( 'NONE',  ( 11.87499106303466867, 1433.007134994034459, 150.0931956004157541 ) ) ;
#54101 = PLANE ( 'NONE',  #31170 ) ;
#54102 = CARTESIAN_POINT ( 'NONE',  ( -10.94435082380000068, 1409.295245542529983, 227.9482308656980081 ) ) ;
#54104 = VERTEX_POINT ( 'NONE', #35508 ) ;
#54103 = CARTESIAN_POINT ( 'NONE',  ( -7.631942175340000745, 1445.746736454730126, 183.8563304949979909 ) ) ;
#54105 = DIRECTION ( 'NONE',  ( -5.980589973904019347E-17, 1.000000000000000000, -1.736889445713099699E-16 ) ) ;
#54106 = CARTESIAN_POINT ( 'NONE',  ( 1.712115010999669895, 1498.987102177869929, 236.1549197538539886 ) ) ;
#54107 = CARTESIAN_POINT ( 'NONE',  ( -2.446860826606596540, 1485.861696308259752, 182.3251189179504479 ) ) ;
#54108 = CARTESIAN_POINT ( 'NONE',  ( 15.76866870594087544, 1506.436298846738964, 224.4414140739798995 ) ) ;
#54109 = CARTESIAN_POINT ( 'NONE',  ( 40.36598731044649924, 1427.956512246619923, 270.3380825022459817 ) ) ;
#54110 = CARTESIAN_POINT ( 'NONE',  ( -1.119439127814999990, 1517.026534522949987, 212.3908711059869745 ) ) ;
#54111 = AXIS2_PLACEMENT_3D ( 'NONE', #26820, #95133, #41973 ) ;
#54112 = CARTESIAN_POINT ( 'NONE',  ( -67.89413382450000256, 1379.746388715500188, 278.3036684585590024 ) ) ;
#54113 = CARTESIAN_POINT ( 'NONE',  ( 0.01998521568534358459, 1507.240582288022779, 237.3618852806027917 ) ) ;
#54114 = CARTESIAN_POINT ( 'NONE',  ( 13.80525599937890036, 1426.970508858360063, 197.4369866690030051 ) ) ;
#54115 = CARTESIAN_POINT ( 'NONE',  ( -0.3862514052426599953, 1500.063116292059931, 233.1571727059169916 ) ) ;
#54116 = CARTESIAN_POINT ( 'NONE',  ( -5.000330033664999618, 1516.770163853809890, 209.8779366980180328 ) ) ;
#54117 = ORIENTED_EDGE ( 'NONE', *, *, #28893, .T. ) ;
#54118 = CARTESIAN_POINT ( 'NONE',  ( 0.05765900138281670334, 1424.300292107330051, 227.5770399881510002 ) ) ;
#54119 = CARTESIAN_POINT ( 'NONE',  ( -6.024103323599999449, 1420.442878368530046, 231.9530688324979906 ) ) ;
#54120 = CARTESIAN_POINT ( 'NONE',  ( -67.03985474800001043, 1384.791062983040092, 292.1873690184589805 ) ) ;
#54121 = EDGE_LOOP ( 'NONE', ( #46646, #2179, #85471, #10619 ) ) ;
#54122 = CARTESIAN_POINT ( 'NONE',  ( -27.55265326522230040, 1385.244708163680116, 225.6838886635030121 ) ) ;
#54123 = CARTESIAN_POINT ( 'NONE',  ( 18.95884658670000178, 1416.837177087930058, 210.4637960667579932 ) ) ;
#54124 = EDGE_CURVE ( 'NONE', #66885, #27633, #105121, .T. ) ;
#54125 = CARTESIAN_POINT ( 'NONE',  ( 18.19935571605649827, 1478.711533688430109, 228.8851065908069984 ) ) ;
#54126 = DIRECTION ( 'NONE',  ( -1.755985294532469921E-16, 1.000000000000000000, -1.338183447452831989E-16 ) ) ;
#54127 = CARTESIAN_POINT ( 'NONE',  ( 10.22326110114815201, 1375.913060387289988, 204.3929701860967896 ) ) ;
#54128 = CARTESIAN_POINT ( 'NONE',  ( -0.1416905494029999935, 1408.918008330330167, 231.7806227986979764 ) ) ;
#54129 = CARTESIAN_POINT ( 'NONE',  ( 0.1336799119265279778, 1420.462095040470103, 182.7174734993599827 ) ) ;
#54130 = CARTESIAN_POINT ( 'NONE',  ( 3.263521904354999670, 1516.676340709600026, 214.8942497445370066 ) ) ;
#54131 = CARTESIAN_POINT ( 'NONE',  ( 18.63535449669999977, 1508.532394786529949, 188.3246405779979966 ) ) ;
#54132 = CARTESIAN_POINT ( 'NONE',  ( 11.81780673814840021, 1522.051704408389924, 195.5270144474869767 ) ) ;
#54133 = ORIENTED_EDGE ( 'NONE', *, *, #65951, .F. ) ;
#54134 = CARTESIAN_POINT ( 'NONE',  ( 3.260357128764999946, 1517.133889586189980, 201.3971135232069969 ) ) ;
#54135 = CARTESIAN_POINT ( 'NONE',  ( -7.799999999999999822, 1402.913060387289988, 209.1218459616989946 ) ) ;
#54136 = ORIENTED_EDGE ( 'NONE', *, *, #110279, .F. ) ;
#54137 = CARTESIAN_POINT ( 'NONE',  ( 11.60004869885205103, 1426.752151907737016, 134.4009923342575235 ) ) ;
#54138 = FACE_OUTER_BOUND ( 'NONE', #93425, .T. ) ;
#54139 = CARTESIAN_POINT ( 'NONE',  ( 7.679314465743660278, 1511.182265711489890, 203.2312592673829670 ) ) ;
#54140 = CARTESIAN_POINT ( 'NONE',  ( 1.941845906307360092, 1423.938214695210036, 191.2749242764670043 ) ) ;
#54141 = CARTESIAN_POINT ( 'NONE',  ( -27.61919202599030143, 1509.794165504519924, 201.0446006437040296 ) ) ;
#54142 = CARTESIAN_POINT ( 'NONE',  ( 11.15120484728000072, 1517.151704408390060, 220.1441346914401720 ) ) ;
#54143 = CARTESIAN_POINT ( 'NONE',  ( 18.50064172359999759, 1416.067629290630066, 209.7633006632509876 ) ) ;
#54144 = CARTESIAN_POINT ( 'NONE',  ( -18.29297708900000075, 1425.080551783529927, 226.8406087971980014 ) ) ;
#54145 = CARTESIAN_POINT ( 'NONE',  ( -22.37002394150000129, 1435.422720654210025, 141.4343147051980054 ) ) ;
#54146 = DIRECTION ( 'NONE',  ( -0.000000000000000000, -1.000000000000000000, -0.000000000000000000 ) ) ;
#54147 = CARTESIAN_POINT ( 'NONE',  ( 17.00461789839999938, 1428.771240263530217, 191.0631962805980208 ) ) ;
#54149 = CARTESIAN_POINT ( 'NONE',  ( -4.518180742295140181E-06, 1509.047264790930058, 179.1218459713510072 ) ) ;
#54148 = CARTESIAN_POINT ( 'NONE',  ( 1.039061157835060145, 1409.452459111349981, 232.6817842876129987 ) ) ;
#54150 = CARTESIAN_POINT ( 'NONE',  ( 2.057041824812614106, 1523.342713519622521, 244.8463988825301385 ) ) ;
#54152 = VERTEX_POINT ( 'NONE', #42810 ) ;
#54151 = B_SPLINE_CURVE_WITH_KNOTS ( 'NONE', 3,
 ( #70146, #87471, #38149, #72329, #36502, #44932, #27003, #70698, #45485, #79627, #2931, #37047, #62861, #88571, #66140, #30841, #83444, #106459, #74527, #64483, #72867, #73419, #99686, #4558, #99135, #63931, #100263, #39807, #90750, #98598, #23542, #12935, #57183, #6194, #91307, #73967, #107555, #21862, #6739, #40897, #57734, #22978, #56061 ),
 .UNSPECIFIED., .F., .F.,
 ( 4, 3, 3, 3, 3, 3, 3, 3, 3, 3, 3, 3, 3, 3, 4 ),
 ( -1.999999998298850112, -1.913740754577760050, -1.770581378075359869, -1.625369123173900032, -1.478912460535070084, -1.330584048827429866, -1.181323947785520190, -1.031451248172440049, -0.8813277763345430671, -0.7315909901474011434, -0.5826190372449879806, -0.4347499881818699397, -0.2882457491577810060, -0.1432907418691580226, -3.793644199889811830E-06 ),
 .UNSPECIFIED. ) ;
#54153 = CARTESIAN_POINT ( 'NONE',  ( 1.552003028135559903, 1415.724942522449965, 190.6284710308260060 ) ) ;
#54154 = CARTESIAN_POINT ( 'NONE',  ( 26.60755023664092533, 1509.169828502769633, 216.8086214747193310 ) ) ;
#54155 = ADVANCED_FACE ( 'NONE', ( #43916 ), #103238, .T. ) ;
#54156 = CARTESIAN_POINT ( 'NONE',  ( -24.17602266159999758, 1436.642150718030052, 210.9689740457980065 ) ) ;
#54157 = CARTESIAN_POINT ( 'NONE',  ( -2.091756139799999747, 1484.248104535490029, 198.6248114345989677 ) ) ;
#54158 = CARTESIAN_POINT ( 'NONE',  ( 1.191524307911315805, 1526.382868172863937, 239.2353018730792087 ) ) ;
#54159 = CARTESIAN_POINT ( 'NONE',  ( -2.273033093151334061, 1525.821544997590763, 240.9339456143064808 ) ) ;
#54160 = CARTESIAN_POINT ( 'NONE',  ( -10.98649148439782230, 1433.355625015306487, 151.7689635225571578 ) ) ;
#54161 = CARTESIAN_POINT ( 'NONE',  ( -24.89939545272470056, 1440.978110083920001, 210.4300214511639808 ) ) ;
#54162 = CARTESIAN_POINT ( 'NONE',  ( -22.70690864871570014, 1509.745348826289955, 188.8675591137879906 ) ) ;
#54163 = B_SPLINE_CURVE_WITH_KNOTS ( 'NONE', 3,
 ( #57590, #73834, #99549, #67093, #90048, #48072 ),
 .UNSPECIFIED., .F., .F.,
 ( 4, 2, 4 ),
 ( -0.04927314538870530142, -0.02504330357724929984, 0.000000000000000000 ),
 .UNSPECIFIED. ) ;
#54164 = CARTESIAN_POINT ( 'NONE',  ( -6.225488187964329789, 1488.541277401709976, 218.3275497249479997 ) ) ;
#54165 = CARTESIAN_POINT ( 'NONE',  ( -18.80014186020000011, 1505.319236276690162, 222.5373108268989881 ) ) ;
#54166 = CARTESIAN_POINT ( 'NONE',  ( -90.49287011937269654, 1383.770007548130025, 308.6794120424070229 ) ) ;
#54167 = CARTESIAN_POINT ( 'NONE',  ( -108.8617172214759989, 1383.656556793380105, 311.0417015030730568 ) ) ;
#54168 = CARTESIAN_POINT ( 'NONE',  ( 18.64672481363430379, 1416.851343896850040, 209.6839434896919840 ) ) ;
#54169 = CARTESIAN_POINT ( 'NONE',  ( 5.571279536309999614, 1428.142529990690036, 215.3037492004590092 ) ) ;
#54171 = ORIENTED_EDGE ( 'NONE', *, *, #93511, .T. ) ;
#54170 = CARTESIAN_POINT ( 'NONE',  ( -13.02294863090000021, 1410.743074594430027, 220.9912686835980082 ) ) ;
#54172 = CARTESIAN_POINT ( 'NONE',  ( -94.23475628420000305, 1381.920488750169852, 295.6479955697590185 ) ) ;
#54173 = DIRECTION ( 'NONE',  ( 1.755985294532464991E-16, -1.000000000000000000, 1.338183447452830017E-16 ) ) ;
#54174 = ORIENTED_EDGE ( 'NONE', *, *, #90884, .F. ) ;
#54175 = VERTEX_POINT ( 'NONE', #51772 ) ;
#54176 = CARTESIAN_POINT ( 'NONE',  ( 31.32995031131198616, 1523.678648413191695, 221.9013357025044115 ) ) ;
#54177 = CARTESIAN_POINT ( 'NONE',  ( 13.20177346510000049, 1508.090222725930062, 233.1545818560979910 ) ) ;
#54178 = CARTESIAN_POINT ( 'NONE',  ( 13.13028867889093831, 1443.050727194750380, 169.4013764991958624 ) ) ;
#54180 = CARTESIAN_POINT ( 'NONE',  ( -16.98088719460000107, 1467.669747903330062, 255.1565003930980140 ) ) ;
#54179 = CARTESIAN_POINT ( 'NONE',  ( 39.93378919416216632, 1431.329204280520116, 269.6090686156236416 ) ) ;
#54181 = CARTESIAN_POINT ( 'NONE',  ( 9.651063919191019025, 1425.440657924460083, 195.4941620015079877 ) ) ;
#54182 = CARTESIAN_POINT ( 'NONE',  ( -109.3504515160000068, 1384.878600923439990, 297.1334136532590264 ) ) ;
#54183 = B_SPLINE_CURVE_WITH_KNOTS ( 'NONE', 3,
 ( #109772, #41476, #49877, #65024 ),
 .UNSPECIFIED., .F., .F.,
 ( 4, 4 ),
 ( 28.60746992390000187, 29.16358566613400072 ),
 .UNSPECIFIED. ) ;
#54184 = CARTESIAN_POINT ( 'NONE',  ( 1.711549605159999876, 1487.306758494089991, 217.0375303586090183 ) ) ;
#54185 = CARTESIAN_POINT ( 'NONE',  ( -19.12700648050000041, 1485.852572981329786, 189.6184868647980011 ) ) ;
#54186 = CARTESIAN_POINT ( 'NONE',  ( 5.281843194899999538, 1410.032092550429979, 186.4939589901979957 ) ) ;
#54187 = CARTESIAN_POINT ( 'NONE',  ( 5.210622763619999986, 1424.684339385929889, 185.7917198324980177 ) ) ;
#54188 = CARTESIAN_POINT ( 'NONE',  ( -1.384206943626949959, 1515.080800108630001, 213.4508755731779956 ) ) ;
#54189 = CARTESIAN_POINT ( 'NONE',  ( -107.2951360021110645, 1379.629536132615613, 309.1752404442335660 ) ) ;
#54190 = CARTESIAN_POINT ( 'NONE',  ( -8.952478501675889433, 1478.958333138210037, 216.6003120932589923 ) ) ;
#54191 = CARTESIAN_POINT ( 'NONE',  ( 0.05914941296659999292, 1451.662743609429981, 154.0810085997979968 ) ) ;
#54193 = VERTEX_POINT ( 'NONE', #87586 ) ;
#54192 = DIRECTION ( 'NONE',  ( 0.000000000000000000, 0.000000000000000000, 1.000000000000000000 ) ) ;
#54194 = ORIENTED_EDGE ( 'NONE', *, *, #83645, .F. ) ;
#54195 = CARTESIAN_POINT ( 'NONE',  ( -11.66445033169999945, 1507.156462614389966, 208.0785273261190014 ) ) ;
#54196 = EDGE_CURVE ( 'NONE', #66425, #20723, #54368, .T. ) ;
#54197 = ADVANCED_FACE ( 'NONE', ( #43373 ), #1938, .F. ) ;
#54198 = CARTESIAN_POINT ( 'NONE',  ( -17.95741408820000018, 1489.793908604289982, 195.2635802347990079 ) ) ;
#54199 = CARTESIAN_POINT ( 'NONE',  ( -12.94491415900000142, 1469.989349686730066, 269.3560571862979600 ) ) ;
#54200 = CARTESIAN_POINT ( 'NONE',  ( 7.477592609290000247, 1422.768710552009907, 195.6698503542990011 ) ) ;
#54201 = CARTESIAN_POINT ( 'NONE',  ( 9.325873406849999120E-15, 1443.913060387330006, 155.8032249175980155 ) ) ;
#54202 = EDGE_CURVE ( 'NONE', #4434, #69831, #31731, .T. ) ;
#54203 = CARTESIAN_POINT ( 'NONE',  ( -14.26333328529999989, 1452.396687225829965, 223.0069981153980052 ) ) ;
#54205 = EDGE_CURVE ( 'NONE', #2071, #84627, #107889, .T. ) ;
#54204 = CARTESIAN_POINT ( 'NONE',  ( 4.561655832029999580, 1453.313060387329870, 189.3102883226979998 ) ) ;
#54206 = CARTESIAN_POINT ( 'NONE',  ( -0.4967073565345429542, 1415.438070636819930, 233.3911243540180180 ) ) ;
#54207 = EDGE_CURVE ( 'NONE', #35548, #32575, #23223, .T. ) ;
#54208 = CARTESIAN_POINT ( 'NONE',  ( -7.607391025489999237, 1458.811203548390040, 215.0925692294790110 ) ) ;
#54209 = CARTESIAN_POINT ( 'NONE',  ( 11.38406662287786908, 1362.730911202566858, 209.6218459617033432 ) ) ;
#54210 = CARTESIAN_POINT ( 'NONE',  ( -45.16361212240940404, 1433.663185462369711, 268.2380307924040039 ) ) ;
#54211 = ORIENTED_EDGE ( 'NONE', *, *, #6871, .F. ) ;
#54212 = CARTESIAN_POINT ( 'NONE',  ( -7.974153723309999720, 1424.391113290319936, 210.4473931630890036 ) ) ;
#54213 = EDGE_CURVE ( 'NONE', #22689, #6446, #82517, .T. ) ;
#54214 = ORIENTED_EDGE ( 'NONE', *, *, #37390, .T. ) ;
#54215 = CARTESIAN_POINT ( 'NONE',  ( 5.011551368014999674, 1517.080322339569875, 209.8587501411369942 ) ) ;
#54216 = CARTESIAN_POINT ( 'NONE',  ( -9.356374587081988992, 1447.096916614799966, 212.1461378009350085 ) ) ;
#54217 = CARTESIAN_POINT ( 'NONE',  ( -21.92444879440000349, 1509.678679009930192, 190.3921826488979718 ) ) ;
#54218 = CARTESIAN_POINT ( 'NONE',  ( -15.02738316969999843, 1410.405006173230049, 190.7838349957980029 ) ) ;
#54219 = CARTESIAN_POINT ( 'NONE',  ( -2.992477406865740264, 1497.069668661619971, 221.1429599211379866 ) ) ;
#54220 = ORIENTED_EDGE ( 'NONE', *, *, #30691, .F. ) ;
#54221 = DIRECTION ( 'NONE',  ( -2.220446049250000002E-16, -1.000000000000000000, 2.220446049250000002E-16 ) ) ;
#54222 = ADVANCED_FACE ( 'NONE', ( #105482 ), #44510, .T. ) ;
#54223 = CARTESIAN_POINT ( 'NONE',  ( -6.942344729965000738, 1516.810037859429940, 201.4055938791270250 ) ) ;
#54224 = CARTESIAN_POINT ( 'NONE',  ( 9.965113123260000094, 1472.070687861889837, 213.8432150078189977 ) ) ;
#54225 = EDGE_CURVE ( 'NONE', #64661, #5750, #50402, .T. ) ;
#54226 = CARTESIAN_POINT ( 'NONE',  ( -8.377793394620750789, 1439.624820938689936, 206.1458744547390154 ) ) ;
#54227 = ORIENTED_EDGE ( 'NONE', *, *, #49510, .F. ) ;
#54228 = CARTESIAN_POINT ( 'NONE',  ( -17.14221562505780128, 1410.074669699509968, 270.0731992386910179 ) ) ;
#54229 = CARTESIAN_POINT ( 'NONE',  ( -2.299668004004999933, 1516.965971551240045, 208.0037412025070012 ) ) ;
#54230 = CARTESIAN_POINT ( 'NONE',  ( -27.23873044170000313, 1435.448403991980058, 135.2737774014979948 ) ) ;
#54231 = CYLINDRICAL_SURFACE ( 'NONE', #46530, 23.69926344187880929 ) ;
#54233 = EDGE_LOOP ( 'NONE', ( #13786, #30136, #82269, #104325 ) ) ;
#54232 = CARTESIAN_POINT ( 'NONE',  ( -7.450033292409739438, 1367.931913175477803, 210.6218459616987957 ) ) ;
#54234 = ORIENTED_EDGE ( 'NONE', *, *, #80484, .F. ) ;
#54235 = EDGE_CURVE ( 'NONE', #73756, #103878, #48340, .T. ) ;
#54236 = CARTESIAN_POINT ( 'NONE',  ( 45.55971553987971845, 1442.925831206288649, 268.9768701855822428 ) ) ;
#54237 = CARTESIAN_POINT ( 'NONE',  ( 11.29696953253679936, 1471.442257073440032, 210.8247801971820081 ) ) ;
#54238 = CARTESIAN_POINT ( 'NONE',  ( 3.626131424302643236, 1424.567267193513317, 184.5641229779018317 ) ) ;
#54239 = CARTESIAN_POINT ( 'NONE',  ( -0.002896907270607540063, 1408.914043369009960, 186.4050159525630193 ) ) ;
#54240 = ADVANCED_FACE ( 'NONE', ( #23660 ), #49195, .T. ) ;
#54241 = CARTESIAN_POINT ( 'NONE',  ( -18.60802716234039877, 1415.890045856200004, 207.5710866051209962 ) ) ;
#54242 = CARTESIAN_POINT ( 'NONE',  ( -17.99573535500000077, 1435.780247436960053, 226.7275259980980024 ) ) ;
#54243 = CARTESIAN_POINT ( 'NONE',  ( 5.319351013645369441, 1475.836928872520048, 266.9609103791869984 ) ) ;
#54244 = CARTESIAN_POINT ( 'NONE',  ( -1.110837182595547201, 1467.058882683617185, 235.4628246916891783 ) ) ;
#54245 = CARTESIAN_POINT ( 'NONE',  ( 7.144588282590000006, 1446.888283566400105, 185.2265207297980112 ) ) ;
#54246 = CARTESIAN_POINT ( 'NONE',  ( 7.709032137684999952, 1516.534320418310244, 206.6366287381669906 ) ) ;
#54247 = EDGE_LOOP ( 'NONE', ( #33648, #93711, #3446, #96273 ) ) ;
#54248 = CARTESIAN_POINT ( 'NONE',  ( 21.75593670543157288, 1411.033169560906572, 216.6130940229133728 ) ) ;
#54249 = CARTESIAN_POINT ( 'NONE',  ( 1.470204857257540132, 1486.276663417369946, 182.0220377839359855 ) ) ;
#54250 = ORIENTED_EDGE ( 'NONE', *, *, #15906, .F. ) ;
#54251 = CARTESIAN_POINT ( 'NONE',  ( -4.992349863779999453, 1391.620913471789891, 214.4361776263990009 ) ) ;
#54252 = CARTESIAN_POINT ( 'NONE',  ( 25.07944958343669839, 1451.314395594800089, 137.5314305375449919 ) ) ;
#54253 = CARTESIAN_POINT ( 'NONE',  ( -22.12673812478050195, 1409.685743108969973, 209.8966867368829980 ) ) ;
#54254 = CARTESIAN_POINT ( 'NONE',  ( -46.09131934240000561, 1385.005100670120100, 219.0267588369590044 ) ) ;
#54255 = DIRECTION ( 'NONE',  ( 1.000000000000000000, 0.000000000000000000, 0.000000000000000000 ) ) ;
#54256 = CARTESIAN_POINT ( 'NONE',  ( 21.03603951619999890, 1411.006939957029999, 199.9012218170380208 ) ) ;
#54257 = CARTESIAN_POINT ( 'NONE',  ( 28.38894342380001490, 1444.994950788470987, 176.3316754166978910 ) ) ;
#54258 = CARTESIAN_POINT ( 'NONE',  ( 17.40898828889999805, 1410.017881507529864, 225.1690343474979841 ) ) ;
#54259 = CARTESIAN_POINT ( 'NONE',  ( -21.53076271701005240, 1429.163937548285730, 219.2231547731813919 ) ) ;
#54260 = CARTESIAN_POINT ( 'NONE',  ( 0.5791559346779789896, 1451.093235343550077, 182.2615577885279947 ) ) ;
#54261 = CARTESIAN_POINT ( 'NONE',  ( -9.902446976249999366, 1380.336055740079928, 216.6871926996190041 ) ) ;
#54262 = CARTESIAN_POINT ( 'NONE',  ( -0.7386049428049979992, 1517.122674412569950, 215.6839400395269877 ) ) ;
#54263 = CARTESIAN_POINT ( 'NONE',  ( -1.984413551915469975, 1517.151704408390060, 219.3307686695569885 ) ) ;
#54264 = EDGE_LOOP ( 'NONE', ( #55748, #72337, #52581, #84085 ) ) ;
#54265 = CARTESIAN_POINT ( 'NONE',  ( -6.218708227939995226, 1463.827981907927779, 227.8629900557837402 ) ) ;
#54266 = B_SPLINE_SURFACE_WITH_KNOTS ( 'NONE', 5, 5, ( 
 ( #2556, #43982, #103876, #60803, #26607, #94929 ),
 ( #9815, #51835, #86521, #1998, #96029, #890 ),
 ( #43432, #53501, #85972, #44536, #87644, #78119 ),
 ( #71432, #10930, #78681, #1423, #35563, #69760 ),
 ( #45106, #105547, #19862, #104985, #36679, #70872 ),
 ( #3105, #54065, #13101, #82545, #98777, #64660 ),
 ( #21495, #37787, #88742, #81407, #81967, #65201 ),
 ( #55708, #72496, #4184, #107182, #99314, #106625 ),
 ( #89829, #46206, #12577, #5839, #22040, #108286 ) ),
 .UNSPECIFIED., .F., .F., .F.,
 ( 6, 3, 6 ),
 ( 6, 6 ),
 ( 0.000000000000000000, 6.504696678220000194, 13.00939335640000039 ),
 ( 0.000000000000000000, 2.000000000000000000 ),
 .UNSPECIFIED. ) ;
#54267 = CARTESIAN_POINT ( 'NONE',  ( 21.92916355573715492, 1523.390106123591067, 235.1782814742748258 ) ) ;
#54268 = CARTESIAN_POINT ( 'NONE',  ( -0.3894626618421410114, 1409.116368191170068, 232.4611552482589900 ) ) ;
#54269 = EDGE_CURVE ( 'NONE', #101208, #46523, #95146, .T. ) ;
#54270 = CARTESIAN_POINT ( 'NONE',  ( 8.656023402515000242, 1514.496907775660020, 214.3647812291569892 ) ) ;
#54271 = EDGE_CURVE ( 'NONE', #80182, #43125, #22528, .T. ) ;
#54272 = CARTESIAN_POINT ( 'NONE',  ( -39.57266623269340045, 1446.793018509809826, 136.6753323040810244 ) ) ;
#54273 = CARTESIAN_POINT ( 'NONE',  ( -4.328264056532950654, 1515.110035495290049, 208.1359449714740038 ) ) ;
#54274 = CARTESIAN_POINT ( 'NONE',  ( -19.00000000000000000, 1440.913060387330006, 209.1218459616979999 ) ) ;
#54275 = CARTESIAN_POINT ( 'NONE',  ( -29.13504683812242035, 1526.073434386619283, 197.1475439643201355 ) ) ;
#54276 = CARTESIAN_POINT ( 'NONE',  ( -31.22294729666610280, 1523.678648413191695, 222.8955943986482282 ) ) ;
#54277 = CARTESIAN_POINT ( 'NONE',  ( -35.31631333859999700, 1462.797633448130000, 269.2416639850980005 ) ) ;
#54278 = CARTESIAN_POINT ( 'NONE',  ( 11.21638122688047012, 1414.413060387330006, 209.8266014933970780 ) ) ;
#54279 = CARTESIAN_POINT ( 'NONE',  ( -110.0482600249999905, 1385.373320011429996, 296.9711117020590336 ) ) ;
#54280 = CARTESIAN_POINT ( 'NONE',  ( 17.71193101246160140, 1521.951704408389787, 196.6727161460330251 ) ) ;
#54281 = ORIENTED_EDGE ( 'NONE', *, *, #71422, .F. ) ;
#54282 = LINE ( 'NONE', #54825, #98419 ) ;
#54283 = FACE_OUTER_BOUND ( 'NONE', #60276, .T. ) ;
#54284 = EDGE_CURVE ( 'NONE', #68646, #37961, #26832, .T. ) ;
#54285 = CARTESIAN_POINT ( 'NONE',  ( -19.14870982884896478, 1485.551433189229783, 189.6725793120419894 ) ) ;
#54286 = B_SPLINE_CURVE_WITH_KNOTS ( 'NONE', 3,
 ( #47382, #81505, #63654, #20490, #71522, #97769, #80433, #70963, #4807, #105642, #38953, #3747, #98870, #21041, #11572, #73132 ),
 .UNSPECIFIED., .F., .F.,
 ( 4, 3, 3, 3, 3, 4 ),
 ( -7.319250911990000219, -7.043526182202069386, -6.032818062830740402, -5.022172799713979785, -4.011090015075000181, -2.998981459959999540 ),
 .UNSPECIFIED. ) ;
#54287 = CARTESIAN_POINT ( 'NONE',  ( -7.512750246095000861, 1509.038615934159907, 203.6084103740969908 ) ) ;
#54288 = CARTESIAN_POINT ( 'NONE',  ( 11.90986840160970139, 1501.627808534720089, 211.5369186294690280 ) ) ;
#54289 = CARTESIAN_POINT ( 'NONE',  ( 25.53333737239999834, 1449.803091282509968, 210.5361858600879827 ) ) ;
#54290 = CARTESIAN_POINT ( 'NONE',  ( -17.19739463999618678, 1525.960063244516959, 236.2603809477411971 ) ) ;
#54291 = CARTESIAN_POINT ( 'NONE',  ( -14.69790105030000049, 1509.426322401930065, 234.2227378565979734 ) ) ;
#54292 = CARTESIAN_POINT ( 'NONE',  ( -17.57918762556300152, 1383.856065982129849, 219.9043076063699971 ) ) ;
#54293 = CARTESIAN_POINT ( 'NONE',  ( 1.275935789888901439, 1416.411555056025691, 232.9857727263382117 ) ) ;
#54294 = CARTESIAN_POINT ( 'NONE',  ( 2.330134122034449806, 1515.551704408389924, 205.2922258479440245 ) ) ;
#54295 = CARTESIAN_POINT ( 'NONE',  ( 9.045806960450768486, 1451.339811764609976, 211.1085978657239934 ) ) ;
#54297 = ORIENTED_EDGE ( 'NONE', *, *, #18770, .F. ) ;
#54296 = CARTESIAN_POINT ( 'NONE',  ( 10.11452303199940062, 1452.508778506509771, 209.7496972492980092 ) ) ;
#54298 = CARTESIAN_POINT ( 'NONE',  ( -0.9464041199730000020, 1451.043408575430021, 182.5116545072980045 ) ) ;
#54299 = EDGE_CURVE ( 'NONE', #75258, #86231, #5718, .T. ) ;
#54300 = CARTESIAN_POINT ( 'NONE',  ( -9.251598888397834841, 1388.591673295162082, 200.8599406664134506 ) ) ;
#54301 = CARTESIAN_POINT ( 'NONE',  ( -3.013235680273810058, 1440.805531640480012, 157.2037855315670072 ) ) ;
#54303 = ORIENTED_EDGE ( 'NONE', *, *, #81452, .T. ) ;
#54302 = CARTESIAN_POINT ( 'NONE',  ( -16.88248175295160181, 1414.913057834419988, 207.9312177863439786 ) ) ;
#54304 = CARTESIAN_POINT ( 'NONE',  ( -4.887556115857369932, 1508.551704408389924, 219.6953829590910061 ) ) ;
#54305 = ORIENTED_EDGE ( 'NONE', *, *, #9303, .F. ) ;
#54306 = CARTESIAN_POINT ( 'NONE',  ( -10.06453687412319908, 1387.658551857550037, 217.5792455951880129 ) ) ;
#54307 = CARTESIAN_POINT ( 'NONE',  ( 3.179666502929999972, 1490.437437189990078, 188.4750071136990073 ) ) ;
#54308 = CARTESIAN_POINT ( 'NONE',  ( -1.808982817633178586, 1509.008938970973759, 238.7270464612732894 ) ) ;
#54309 = EDGE_CURVE ( 'NONE', #94269, #38319, #90419, .T. ) ;
#54310 = CIRCLE ( 'NONE', #6001, 29.51505616007316135 ) ;
#54311 = CARTESIAN_POINT ( 'NONE',  ( 5.529365985937329420, 1466.685659397790005, 204.7973175625270130 ) ) ;
#54312 = CARTESIAN_POINT ( 'NONE',  ( 1.338019038549999928, 1431.361301794989913, 218.5179653796290040 ) ) ;
#54313 = CARTESIAN_POINT ( 'NONE',  ( 21.04236285220000013, 1494.763913780290068, 208.1091839946190021 ) ) ;
#54314 = CARTESIAN_POINT ( 'NONE',  ( 10.01139723437129980, 1409.262666079100200, 220.2341507100319973 ) ) ;
#54315 = CARTESIAN_POINT ( 'NONE',  ( 0.6364662388029991291, 1454.894302228490005, 215.7249496973589942 ) ) ;
#54316 = CARTESIAN_POINT ( 'NONE',  ( -103.4461152369070049, 1385.229357875270125, 296.7794697699490030 ) ) ;
#54317 = CARTESIAN_POINT ( 'NONE',  ( -17.50241060500000145, 1410.867113670829895, 192.6239589323980113 ) ) ;
#54318 = CARTESIAN_POINT ( 'NONE',  ( -25.99322061230196113, 1379.720623260343245, 211.7359130857557545 ) ) ;
#54319 = FACE_OUTER_BOUND ( 'NONE', #11769, .T. ) ;
#54320 = ORIENTED_EDGE ( 'NONE', *, *, #60815, .T. ) ;
#54321 = VERTEX_POINT ( 'NONE', #9609 ) ;
#54322 = EDGE_CURVE ( 'NONE', #60349, #63956, #33704, .T. ) ;
#54323 =( BOUNDED_CURVE ( )  B_SPLINE_CURVE ( 3, ( #33458, #58150, #98057, #66013 ),
 .UNSPECIFIED., .F., .F. ) 
 B_SPLINE_CURVE_WITH_KNOTS ( ( 4, 4 ),
 ( 2.436781329611978464, 3.141592653589793116 ),
 .UNSPECIFIED. ) 
 CURVE ( )  GEOMETRIC_REPRESENTATION_ITEM ( )  RATIONAL_B_SPLINE_CURVE ( ( 1.000000000000000000, 0.9590300661663082593, 0.9590300661663082593, 1.000000000000000000 ) ) 
 REPRESENTATION_ITEM ( '' )  );
#54324 = CARTESIAN_POINT ( 'NONE',  ( -18.66135599109209764, 1441.829349819740173, 210.7852733701969896 ) ) ;
#54325 = CARTESIAN_POINT ( 'NONE',  ( 2.475018581880529922, 1497.111080376900190, 196.9667223532030107 ) ) ;
#54326 = EDGE_CURVE ( 'NONE', #67527, #91965, #8912, .T. ) ;
#54327 = CARTESIAN_POINT ( 'NONE',  ( 28.55528612434519076, 1509.910687724684976, 216.1464615550907808 ) ) ;
#54328 = DIRECTION ( 'NONE',  ( 0.01484500364079635246, -0.5669078173018518019, -0.8236474686107856380 ) ) ;
#54329 = CARTESIAN_POINT ( 'NONE',  ( -28.24318413590000176, 1508.132100804830088, 209.6063173613950141 ) ) ;
#54330 = CARTESIAN_POINT ( 'NONE',  ( 31.56779946216476418, 1525.408327360769590, 202.0372978226081102 ) ) ;
#54331 = CARTESIAN_POINT ( 'NONE',  ( 1.842962231260000028, 1515.551704408389924, 205.2922258481490303 ) ) ;
#54332 = CARTESIAN_POINT ( 'NONE',  ( -10.87716623425449569, 1367.819513648856628, 209.6218459617033432 ) ) ;
#54333 = CARTESIAN_POINT ( 'NONE',  ( -25.79637238690366630, 1436.656401712661818, 137.0607721643913521 ) ) ;
#54334 = CARTESIAN_POINT ( 'NONE',  ( -5.012938901904998801, 1517.051603658920158, 206.6410320471169939 ) ) ;
#54335 = CARTESIAN_POINT ( 'NONE',  ( -13.07366137487360014, 1434.838828088369837, 149.4347582794279674 ) ) ;
#54336 = CARTESIAN_POINT ( 'NONE',  ( -8.861482052969998691, 1384.950957082100103, 218.6848127019790127 ) ) ;
#54337 = CARTESIAN_POINT ( 'NONE',  ( 1.342110471609999856, 1416.822692809430009, 190.1636843969979793 ) ) ;
#54338 = CARTESIAN_POINT ( 'NONE',  ( 0.1132302339970009813, 1498.032890047989895, 197.7962523521989908 ) ) ;
#54339 = DIRECTION ( 'NONE',  ( -0.5969061220947670110, 0.8023110876747169273, 0.000000000000000000 ) ) ;
#54340 = EDGE_CURVE ( 'NONE', #11785, #66900, #43282, .T. ) ;
#54341 = EDGE_CURVE ( 'NONE', #21520, #53297, #62307, .T. ) ;
#54342 = CARTESIAN_POINT ( 'NONE',  ( -103.5847285859999971, 1379.882004272549921, 303.6035322816589996 ) ) ;
#54343 = EDGE_LOOP ( 'NONE', ( #94266, #95380, #43769, #59160 ) ) ;
#54344 = CARTESIAN_POINT ( 'NONE',  ( -3.400317100450000321E-09, 1409.477337460029958, 259.9484463448980023 ) ) ;
#54345 = CARTESIAN_POINT ( 'NONE',  ( -23.50062168420000219, 1488.679648898629921, 197.2621013953979912 ) ) ;
#54347 = CARTESIAN_POINT ( 'NONE',  ( -19.53786426058999481, 1512.187213306747481, 236.7197124308268030 ) ) ;
#54346 = CARTESIAN_POINT ( 'NONE',  ( -11.08399775210000016, 1426.906423284629909, 96.73292351169779124 ) ) ;
#54348 = CARTESIAN_POINT ( 'NONE',  ( -1.984413551915469975, 1522.051704408389924, 219.3307686695569885 ) ) ;
#54349 = CARTESIAN_POINT ( 'NONE',  ( -29.43658766380000102, 1426.244274385030167, 250.1802633625980263 ) ) ;
#54350 = CARTESIAN_POINT ( 'NONE',  ( 20.46980501909149908, 1509.670375995580116, 230.6918749470270029 ) ) ;
#54351 = LINE ( 'NONE', #29121, #10581 ) ;
#54352 = CARTESIAN_POINT ( 'NONE',  ( -24.08426305480000451, 1411.115211393229856, 208.6111285346999864 ) ) ;
#54353 = ORIENTED_EDGE ( 'NONE', *, *, #53438, .T. ) ;
#54354 = CARTESIAN_POINT ( 'NONE',  ( -5.386547031804509444, 1432.371148517990150, 154.6078450733400018 ) ) ;
#54355 = CARTESIAN_POINT ( 'NONE',  ( 11.65717857212529296, 1512.939392324944947, 225.5530975207334166 ) ) ;
#54356 = B_SPLINE_CURVE_WITH_KNOTS ( 'NONE', 5,
 ( #96259, #86750, #19534, #28503, #86194, #80008 ),
 .UNSPECIFIED., .F., .F.,
 ( 6, 6 ),
 ( -158.0163518690000046, -29.52656374809998852 ),
 .UNSPECIFIED. ) ;
#54357 = EDGE_CURVE ( 'NONE', #8168, #12203, #17435, .T. ) ;
#54358 = CARTESIAN_POINT ( 'NONE',  ( 38.39760561534620109, 1443.174109818610077, 137.1306153789140012 ) ) ;
#54359 = ORIENTED_EDGE ( 'NONE', *, *, #93859, .T. ) ;
#54360 = VERTEX_POINT ( 'NONE', #16882 ) ;
#54361 = CARTESIAN_POINT ( 'NONE',  ( -22.99522306489999579, 1384.540050732020063, 202.4077213122689898 ) ) ;
#54362 = CARTESIAN_POINT ( 'NONE',  ( 5.920277381630000058, 1423.127765564700212, 194.8707734773990126 ) ) ;
#54363 = VERTEX_POINT ( 'NONE', #9069 ) ;
#54364 = CARTESIAN_POINT ( 'NONE',  ( -0.04561968975039999707, 1424.313206842929958, 227.6130361704979919 ) ) ;
#54365 = CARTESIAN_POINT ( 'NONE',  ( -8.080260711212272184, 1418.884620420010833, 195.9946716912613169 ) ) ;
#54366 = ADVANCED_FACE ( 'NONE', ( #35374 ), #43238, .T. ) ;
#54367 = CARTESIAN_POINT ( 'NONE',  ( 0.3651880982969999967, 1451.159209398729899, 182.5636267636980108 ) ) ;
#54368 = B_SPLINE_CURVE_WITH_KNOTS ( 'NONE', 5,
 ( #94294, #104368, #45046, #9213, #17572, #10302 ),
 .UNSPECIFIED., .F., .F.,
 ( 6, 6 ),
 ( 0.000000000000000000, 11.48858425020000240 ),
 .UNSPECIFIED. ) ;
#54369 = CARTESIAN_POINT ( 'NONE',  ( -11.79378255399999986, 1479.764572231929833, 232.1975610188979999 ) ) ;
#54370 = CARTESIAN_POINT ( 'NONE',  ( 2.487924109712380094, 1508.884228866460035, 213.6131300634060040 ) ) ;
#54371 = ORIENTED_EDGE ( 'NONE', *, *, #81578, .T. ) ;
#54372 = CARTESIAN_POINT ( 'NONE',  ( 11.73709356449999852, 1426.695943566229971, 144.1748013792980032 ) ) ;
#54373 = CARTESIAN_POINT ( 'NONE',  ( -11.91079909292840000, 1414.913060387399810, 220.1328973762649923 ) ) ;
#54374 = CARTESIAN_POINT ( 'NONE',  ( 15.59061307620000036, 1507.637957935030045, 225.5593735085980143 ) ) ;
#54375 = ORIENTED_EDGE ( 'NONE', *, *, #100062, .T. ) ;
#54376 = CARTESIAN_POINT ( 'NONE',  ( 7.325541787135000149, 1516.710692850270107, 204.1167749238070144 ) ) ;
#54377 = ORIENTED_EDGE ( 'NONE', *, *, #49642, .F. ) ;
#54378 = CARTESIAN_POINT ( 'NONE',  ( 11.86457202409800082, 1432.229187294399935, 149.9813147920380061 ) ) ;
#54379 = CARTESIAN_POINT ( 'NONE',  ( 5.513435558552500559, 1508.551704408428805, 201.9802063542013855 ) ) ;
#54380 = ORIENTED_EDGE ( 'NONE', *, *, #34757, .T. ) ;
#54381 = ORIENTED_EDGE ( 'NONE', *, *, #28433, .T. ) ;
#54382 = CARTESIAN_POINT ( 'NONE',  ( 4.487358956434530199, 1509.034509900239300, 212.9235808158116470 ) ) ;
#54383 = CARTESIAN_POINT ( 'NONE',  ( -5.833099474469870316, 1508.551704408389924, 219.4902126349500122 ) ) ;
#54384 = CARTESIAN_POINT ( 'NONE',  ( -21.62302451687340010, 1409.668153042179938, 204.8506916389789865 ) ) ;
#54385 = CARTESIAN_POINT ( 'NONE',  ( -2.916662559637150043, 1468.341157279690151, 219.5036260853820238 ) ) ;
#54386 = CARTESIAN_POINT ( 'NONE',  ( -4.653266759930000163, 1425.827076154429960, 186.2156706901979817 ) ) ;
#54387 = CARTESIAN_POINT ( 'NONE',  ( 0.9453222513162000684, 1410.394701501269992, 269.3347007296789570 ) ) ;
#54388 = CARTESIAN_POINT ( 'NONE',  ( 3.744312463839459593, 1509.032014876046560, 204.8809009122383600 ) ) ;
#54389 = CARTESIAN_POINT ( 'NONE',  ( -7.437974795490000623, 1473.518143733989973, 200.3716835635890163 ) ) ;
#54390 = CARTESIAN_POINT ( 'NONE',  ( 10.41203720280000056, 1493.307641990389811, 215.0005194938290174 ) ) ;
#54391 = CARTESIAN_POINT ( 'NONE',  ( -20.61514741043744792, 1509.679810159945191, 230.5809340611079108 ) ) ;
#54392 = CIRCLE ( 'NONE', #95449, 23.69926344187880929 ) ;
#54393 = LINE ( 'NONE', #69543, #8826 ) ;
#54395 = CARTESIAN_POINT ( 'NONE',  ( 14.76593576959999865, 1434.994542537580173, 195.9393237157979968 ) ) ;
#54394 = CARTESIAN_POINT ( 'NONE',  ( -17.64814166450000243, 1504.515913262890081, 208.9742322240140027 ) ) ;
#54396 = CARTESIAN_POINT ( 'NONE',  ( -26.04447212934309164, 1379.718901743828837, 215.2627710545450839 ) ) ;
#54397 = CARTESIAN_POINT ( 'NONE',  ( 17.70992611605910128, 1414.252993047500013, 224.9060675817109995 ) ) ;
#54398 = CARTESIAN_POINT ( 'NONE',  ( -6.760013159984999298, 1512.520476835120007, 201.4807483541169972 ) ) ;
#54399 = VERTEX_POINT ( 'NONE', #69006 ) ;
#54400 = CARTESIAN_POINT ( 'NONE',  ( 1.199040866600000048E-14, 1416.825952160429779, 255.3819207742980097 ) ) ;
#54401 = CIRCLE ( 'NONE', #86494, 1.000000000000000000 ) ;
#54402 = CARTESIAN_POINT ( 'NONE',  ( 18.63864990483601858, 1509.044553701713312, 187.9652674624242366 ) ) ;
#54403 = CARTESIAN_POINT ( 'NONE',  ( -55.04432150766159992, 1385.092390689839931, 271.8936798544510225 ) ) ;
#54404 = B_SPLINE_SURFACE_WITH_KNOTS ( 'NONE', 5, 5, ( 
 ( #99330, #73059, #57383, #39450, #82563, #38878 ),
 ( #73623, #107753, #47300, #107201, #31036, #108304 ),
 ( #64678, #29932, #31589, #13661, #32148, #65219 ),
 ( #99884, #30489, #65766, #23182, #22057, #48975 ),
 ( #83107, #91509, #12596, #6401, #40547, #74721 ),
 ( #98795, #55174, #108854, #5855, #90945, #66336 ),
 ( #56254, #55726, #22604, #98244, #48420, #21514 ),
 ( #100452, #39996, #56807, #74175, #90382, #14231 ),
 ( #89845, #13117, #89300, #46774, #4201, #106641 ),
 ( #80905, #47850, #81984, #5292, #38333, #72513 ),
 ( #81424, #34359, #77474, #17523, #85292, #75276 ),
 ( #102098, #68535, #43326, #100990, #16420, #33244 ),
 ( #25934, #59026, #24821, #41659, #67987, #24286 ),
 ( #42763, #25379, #67434, #8591, #8043, #6942 ),
 ( #775, #9162, #57923, #76923, #34904, #92055 ),
 ( #69090, #59571, #75815, #60130, #42211, #51164 ),
 ( #93685, #76362, #110511, #15868, #109967, #33793 ),
 ( #109423, #101532, #32700, #232, #93151, #23735 ),
 ( #94249, #102633, #84200, #51726, #85861, #50613 ),
 ( #7497, #15327, #49522, #83647, #41097, #66880 ),
 ( #84745, #16965, #58467, #92594, #50071, #10822 ) ),
 .UNSPECIFIED., .F., .F., .F.,
 ( 6, 3, 3, 3, 3, 3, 6 ),
 ( 6, 6 ),
 ( 3.497608506310000198, 12.90721938930000157, 16.34806485209999849, 18.06848758349999784, 18.75464242129999803, 19.44079725900000000, 19.78891031479999896 ),
 ( 0.000000000000000000, 2.205736517120000073 ),
 .UNSPECIFIED. ) ;
#54405 = CARTESIAN_POINT ( 'NONE',  ( 7.020660495122974076, 1374.031200045389824, 212.9572502705326258 ) ) ;
#54406 = CARTESIAN_POINT ( 'NONE',  ( 4.875788219060000372, 1505.619959711089905, 220.1093002778990240 ) ) ;
#54407 = DIRECTION ( 'NONE',  ( -0.9455185755993178454, 0.000000000000000000, 0.3255681544571539243 ) ) ;
#54409 = ORIENTED_EDGE ( 'NONE', *, *, #106852, .F. ) ;
#54408 = CARTESIAN_POINT ( 'NONE',  ( -17.83876811113470140, 1419.521416245730052, 206.8588588664190127 ) ) ;
#54410 = CARTESIAN_POINT ( 'NONE',  ( 17.38235994490000280, 1414.983771850430003, 210.5633853858680027 ) ) ;
#54411 = CARTESIAN_POINT ( 'NONE',  ( -24.11773784480000060, 1444.076521055339981, 211.7353999850080015 ) ) ;
#54412 = CARTESIAN_POINT ( 'NONE',  ( -0.7006591791222261945, 1450.888592821566363, 154.2444655603070203 ) ) ;
#54413 = CARTESIAN_POINT ( 'NONE',  ( 6.202741644639123031, 1439.658053187385121, 216.9645217985598435 ) ) ;
#54414 = CARTESIAN_POINT ( 'NONE',  ( 14.46755550443499949, 1513.509764667529907, 224.2886214921669819 ) ) ;
#54415 = CARTESIAN_POINT ( 'NONE',  ( 3.724606435798804682, 1370.320419915130969, 208.2352337144575074 ) ) ;
#54416 = CARTESIAN_POINT ( 'NONE',  ( 19.12393420247930109, 1509.659725678649920, 184.6857789466980080 ) ) ;
#54417 = CARTESIAN_POINT ( 'NONE',  ( 6.282508756548999429, 1459.626149291560068, 201.6398963661700066 ) ) ;
#54418 = B_SPLINE_CURVE_WITH_KNOTS ( 'NONE', 5,
 ( #33760, #76332, #92028, #23708, #40516, #83614, #84715, #58436, #75246 ),
 .UNSPECIFIED., .F., .F.,
 ( 6, 3, 6 ),
 ( 0.8631819983265639484, 2.053866004040000082, 3.194083030974049997 ),
 .UNSPECIFIED. ) ;
#54419 = CARTESIAN_POINT ( 'NONE',  ( -13.23366354170440040, 1419.304941490409874, 221.9853583435139797 ) ) ;
#54420 = B_SPLINE_CURVE_WITH_KNOTS ( 'NONE', 3,
 ( #78417, #9542, #95763, #68938 ),
 .UNSPECIFIED., .F., .F.,
 ( 4, 4 ),
 ( 0.000000000000000000, 1.000000000000000000 ),
 .UNSPECIFIED. ) ;
#54421 = CARTESIAN_POINT ( 'NONE',  ( 5.856052932189999893, 1412.733406791530115, 231.2218989843980239 ) ) ;
#54422 = CARTESIAN_POINT ( 'NONE',  ( -7.981287325994377291, 1424.856636039371779, 210.5242404286136377 ) ) ;
#54423 = CARTESIAN_POINT ( 'NONE',  ( -16.50825790430000239, 1460.843606021430105, 228.2701616867980192 ) ) ;
#54424 = CARTESIAN_POINT ( 'NONE',  ( -4.044321718124999521, 1517.001127920769704, 206.8363583507369867 ) ) ;
#54425 = CARTESIAN_POINT ( 'NONE',  ( 46.27886452250000104, 1438.889480702049923, 267.5894389992980109 ) ) ;
#54426 = CARTESIAN_POINT ( 'NONE',  ( -19.08749734139999887, 1410.075444410930004, 222.3596486551979865 ) ) ;
#54427 = CARTESIAN_POINT ( 'NONE',  ( 21.17685425119999820, 1435.236150072139935, 141.6298919720979939 ) ) ;
#54428 = CARTESIAN_POINT ( 'NONE',  ( 19.82449983040000063, 1469.159611771130130, 191.7468874958980223 ) ) ;
#54429 = CARTESIAN_POINT ( 'NONE',  ( 24.59498489902570029, 1440.913044926110160, 213.3385239659299941 ) ) ;
#54430 = CARTESIAN_POINT ( 'NONE',  ( -3.168001005839999884, 1479.750044315889909, 229.3575515971990058 ) ) ;
#54431 = CARTESIAN_POINT ( 'NONE',  ( -3.758278191160000059, 1475.720032253530007, 266.9554522522980164 ) ) ;
#54432 = CARTESIAN_POINT ( 'NONE',  ( -32.38845791999504797, 1518.913060387330006, 202.1182848005516348 ) ) ;
#54433 = DIRECTION ( 'NONE',  ( -1.000000000000000000, 0.000000000000000000, -1.224646799147351975E-16 ) ) ;
#54434 = FACE_OUTER_BOUND ( 'NONE', #106919, .T. ) ;
#54435 = CARTESIAN_POINT ( 'NONE',  ( -15.42032581149999970, 1415.152828348040202, 209.2822251248840075 ) ) ;
#54436 = CARTESIAN_POINT ( 'NONE',  ( -17.31002161700749653, 1410.038357211269840, 193.4350317523646368 ) ) ;
#54437 = ADVANCED_FACE ( 'NONE', ( #26411 ), #67899, .F. ) ;
#54438 = CARTESIAN_POINT ( 'NONE',  ( -7.582807648377508869, 1384.152347710639788, 219.0341480461830201 ) ) ;
#54439 = CARTESIAN_POINT ( 'NONE',  ( 11.87984373510000147, 1433.310963811120018, 146.4341632258980042 ) ) ;
#54440 = CARTESIAN_POINT ( 'NONE',  ( -30.79850881079999780, 1436.468376053830070, 136.6063225575979914 ) ) ;
#54441 = ORIENTED_EDGE ( 'NONE', *, *, #85625, .T. ) ;
#54442 = CARTESIAN_POINT ( 'NONE',  ( 5.670155014969999741, 1477.128358946589969, 199.4032014051190060 ) ) ;
#54443 = CARTESIAN_POINT ( 'NONE',  ( -11.06770810696790086, 1409.299553270950128, 219.1756186191919937 ) ) ;
#54444 = CARTESIAN_POINT ( 'NONE',  ( -16.68463225901000158, 1445.052233488270076, 162.0935120915889911 ) ) ;
#54445 = CARTESIAN_POINT ( 'NONE',  ( -4.748707386669323682, 1463.075551767410161, 200.5806828470055621 ) ) ;
#54446 = CARTESIAN_POINT ( 'NONE',  ( -16.68463225827704122, 1442.773887286370382, 162.0935120918187806 ) ) ;
#54447 = CARTESIAN_POINT ( 'NONE',  ( -42.38294288630000040, 1456.046607473030008, 266.8007141661980199 ) ) ;
#54448 = CARTESIAN_POINT ( 'NONE',  ( -11.82625070047500060, 1481.580697255540144, 210.0186159470979987 ) ) ;
#54449 = CARTESIAN_POINT ( 'NONE',  ( 0.3751301725765759931, 1419.058492625649933, 184.6369606967579955 ) ) ;
#54450 = CARTESIAN_POINT ( 'NONE',  ( 20.70484064406395674, 1525.907212628473644, 233.2025904124104443 ) ) ;
#54451 = CARTESIAN_POINT ( 'NONE',  ( -84.08298741828620848, 1384.630359715449913, 306.2334057474649853 ) ) ;
#54452 = CARTESIAN_POINT ( 'NONE',  ( -43.92410954080200014, 1385.000048749679991, 217.0325689943980194 ) ) ;
#54453 = CARTESIAN_POINT ( 'NONE',  ( 18.29126995980630355, 1425.098100345099965, 226.7651582995079877 ) ) ;
#54454 = CARTESIAN_POINT ( 'NONE',  ( 11.49747567979999907, 1414.913060387329779, 220.3427040543980127 ) ) ;
#54455 = CARTESIAN_POINT ( 'NONE',  ( 15.14740264819999993, 1485.055112692129796, 223.7344915146980213 ) ) ;
#54456 = CARTESIAN_POINT ( 'NONE',  ( 2.663428195552854927, 1419.688227176016881, 137.0999999980978430 ) ) ;
#54458 = ORIENTED_EDGE ( 'NONE', *, *, #1598, .T. ) ;
#54457 = CARTESIAN_POINT ( 'NONE',  ( 4.123245670370000227, 1515.545044289889802, 208.3730318020869845 ) ) ;
#54459 = CARTESIAN_POINT ( 'NONE',  ( -5.669846970490000082, 1507.854450105929800, 181.2109580980980184 ) ) ;
#54460 = CARTESIAN_POINT ( 'NONE',  ( 4.786039370545940308, 1421.795857048071412, 137.9175743968286270 ) ) ;
#54461 = CARTESIAN_POINT ( 'NONE',  ( -4.077284799680000127, 1495.755251076190007, 219.5524077617990315 ) ) ;
#54462 = CARTESIAN_POINT ( 'NONE',  ( -11.46423597849999965, 1415.041103191630100, 195.6823422413980040 ) ) ;
#54463 = CARTESIAN_POINT ( 'NONE',  ( 0.4842866986810019925, 1421.662812042720134, 193.6869198051990111 ) ) ;
#54464 = EDGE_CURVE ( 'NONE', #44414, #71213, #22177, .T. ) ;
#54465 = FACE_OUTER_BOUND ( 'NONE', #62942, .T. ) ;
#54466 = CARTESIAN_POINT ( 'NONE',  ( -106.5689870562550112, 1391.913060387289988, 305.4639128772769823 ) ) ;
#54467 = CARTESIAN_POINT ( 'NONE',  ( 20.81211029356619946, 1456.820296889740121, 206.9378353218430107 ) ) ;
#54468 = CARTESIAN_POINT ( 'NONE',  ( -15.06280285359999915, 1422.388303686929930, 229.4662104616980116 ) ) ;
#54470 = CARTESIAN_POINT ( 'NONE',  ( -10.66583685980000062, 1379.443864687059886, 202.8590315047190131 ) ) ;
#54469 = CARTESIAN_POINT ( 'NONE',  ( -11.87111153510000072, 1432.721389748929823, 150.3961583812979939 ) ) ;
#54471 = DIRECTION ( 'NONE',  ( 0.3538510588705020554, 0.9352971592855031657, 0.002941422902738410894 ) ) ;
#54472 = CARTESIAN_POINT ( 'NONE',  ( -120.0305877506754513, 1377.418846546390341, 293.0440248834586896 ) ) ;
#54473 = EDGE_CURVE ( 'NONE', #35126, #51888, #79026, .T. ) ;
#54474 = CARTESIAN_POINT ( 'NONE',  ( -1766.069695707609526, -8382.262153571264207, -1964.859607327509593 ) ) ;
#54475 = CARTESIAN_POINT ( 'NONE',  ( 19.66678637211940028, 1517.051704408389924, 202.3500283489059939 ) ) ;
#54476 = AXIS2_PLACEMENT_3D ( 'NONE', #45103, #55704, #89825 ) ;
#54477 = CARTESIAN_POINT ( 'NONE',  ( -9.209502321770001387, 1366.683160837839978, 210.6218459616991936 ) ) ;
#54478 = EDGE_CURVE ( 'NONE', #29958, #49356, #810, .T. ) ;
#54479 = CARTESIAN_POINT ( 'NONE',  ( 3.255967386345000047, 1516.989560013210166, 204.1101670940770134 ) ) ;
#54480 = CARTESIAN_POINT ( 'NONE',  ( 13.38442537232469931, 1507.877059872409745, 233.1002377268139867 ) ) ;
#54481 = CARTESIAN_POINT ( 'NONE',  ( -16.28589060890169549, 1485.388328323199858, 187.7393477621970135 ) ) ;
#54482 = CARTESIAN_POINT ( 'NONE',  ( 11.15128118274900082, 1503.005909027870075, 212.1832507974499720 ) ) ;
#54483 = CARTESIAN_POINT ( 'NONE',  ( -11.42514667305001730, 1422.040958530333455, 210.6386249240756854 ) ) ;
#54484 = AXIS2_PLACEMENT_3D ( 'NONE', #45759, #37337, #989 ) ;
#54486 = ORIENTED_EDGE ( 'NONE', *, *, #8293, .F. ) ;
#54485 = CARTESIAN_POINT ( 'NONE',  ( -67.65809801332019902, 1379.745325822590075, 278.9855928749340137 ) ) ;
#54487 = EDGE_CURVE ( 'NONE', #14695, #45310, #87670, .T. ) ;
#54488 = ORIENTED_EDGE ( 'NONE', *, *, #87635, .T. ) ;
#54489 = CARTESIAN_POINT ( 'NONE',  ( 28.79939580839999991, 1509.589065600929871, 209.5214383132930038 ) ) ;
#54490 = ORIENTED_EDGE ( 'NONE', *, *, #2861, .F. ) ;
#54491 = CARTESIAN_POINT ( 'NONE',  ( -105.3072927039999911, 1379.015832552830034, 304.0377861886589699 ) ) ;
#54492 = CARTESIAN_POINT ( 'NONE',  ( -109.4847723999999971, 1384.941599254929997, 311.2840177552590717 ) ) ;
#54494 = CARTESIAN_POINT ( 'NONE',  ( 0.8261844755670000318, 1508.165896155429891, 180.7872846942979947 ) ) ;
#54493 = CARTESIAN_POINT ( 'NONE',  ( 15.75137492476309831, 1413.122398938390006, 191.4468246197170060 ) ) ;
#54495 = DIRECTION ( 'NONE',  ( 0.02617694830785694329, 0.9996573249755577040, -1.920531143124581619E-16 ) ) ;
#54496 = CARTESIAN_POINT ( 'NONE',  ( -25.70055298538810007, 1451.293284185210041, 136.6856562540129971 ) ) ;
#54497 = CARTESIAN_POINT ( 'NONE',  ( 11.42137624728064793, 1437.875189691955484, 152.0075177772093582 ) ) ;
#54498 = CARTESIAN_POINT ( 'NONE',  ( 11.50002771670000001, 1409.817236179030033, 229.0027380318980192 ) ) ;
#54499 = CARTESIAN_POINT ( 'NONE',  ( -4.517196230222687348, 1522.051704408389924, 190.6118719775071781 ) ) ;
#54500 = PRODUCT ( 'Handle Screw', 'Handle Screw', '', ( #42618 ) ) ;
#54501 = CARTESIAN_POINT ( 'NONE',  ( 2.879642153204999833, 1516.812046502680005, 212.5681757458869754 ) ) ;
#54502 = CARTESIAN_POINT ( 'NONE',  ( 41.28347186110210032, 1446.141341654809821, 134.0999999985599800 ) ) ;
#54503 = DIRECTION ( 'NONE',  ( 0.9983395709201744461, 0.05760296116452706672, 0.000000000000000000 ) ) ;
#54504 = ORIENTED_EDGE ( 'NONE', *, *, #70193, .F. ) ;
#54505 = CARTESIAN_POINT ( 'NONE',  ( 19.03958014020000178, 1453.804227313890124, 200.7927590370090059 ) ) ;
#54506 = DIRECTION ( 'NONE',  ( 1.755985294532469921E-16, -1.000000000000000000, 1.338183447452831989E-16 ) ) ;
#54507 = ORIENTED_EDGE ( 'NONE', *, *, #44859, .T. ) ;
#54508 = ORIENTED_EDGE ( 'NONE', *, *, #97224, .T. ) ;
#54509 = ORIENTED_EDGE ( 'NONE', *, *, #60980, .T. ) ;
#54510 = CARTESIAN_POINT ( 'NONE',  ( -7.381112355834999583, 1512.341575225279939, 215.8975307908470143 ) ) ;
#54511 = CARTESIAN_POINT ( 'NONE',  ( 16.27599025125675070, 1514.537600256206815, 194.3631480892788943 ) ) ;
#54512 = CARTESIAN_POINT ( 'NONE',  ( 8.020248913699530746, 1451.388689963839852, 152.9391484428220735 ) ) ;
#54513 = DIRECTION ( 'NONE',  ( 0.000000000000000000, 0.000000000000000000, -1.000000000000000000 ) ) ;
#54514 = CARTESIAN_POINT ( 'NONE',  ( -1.207243347426069979, 1465.149812066310005, 198.1847202192419957 ) ) ;
#54515 = AXIS2_PLACEMENT_3D ( 'NONE', #95484, #12030, #80345 ) ;
#54516 = ADVANCED_FACE ( 'NONE', ( #72845 ), #110008, .T. ) ;
#54517 = CARTESIAN_POINT ( 'NONE',  ( -16.87886782060054358, 1449.383582043091110, 219.7154039679069797 ) ) ;
#54518 = CARTESIAN_POINT ( 'NONE',  ( -68.02398329241702868, 1379.746453776986527, 278.4801873761143725 ) ) ;
#54519 = CARTESIAN_POINT ( 'NONE',  ( 4.279348318663660500, 1446.810037118880018, 156.6083306040470120 ) ) ;
#54520 = EDGE_CURVE ( 'NONE', #108323, #55409, #46167, .T. ) ;
#54521 = CARTESIAN_POINT ( 'NONE',  ( -0.05360592782209999685, 1508.805584758630175, 238.3850021203980134 ) ) ;
#54522 = AXIS2_PLACEMENT_3D ( 'NONE', #64585, #48323, #107105 ) ;
#54523 = ORIENTED_EDGE ( 'NONE', *, *, #14612, .T. ) ;
#54524 = CARTESIAN_POINT ( 'NONE',  ( -5.788436372295000076, 1517.116049120239950, 206.8334885244969712 ) ) ;
#54525 = ORIENTED_EDGE ( 'NONE', *, *, #55623, .F. ) ;
#54526 = CARTESIAN_POINT ( 'NONE',  ( 25.52987090084080180, 1440.913060387330006, 240.7947691460219914 ) ) ;
#54527 = CARTESIAN_POINT ( 'NONE',  ( -20.99310676700000400, 1509.712615454430079, 187.9175748575979981 ) ) ;
#54528 = VERTEX_POINT ( 'NONE', #11830 ) ;
#54529 = CARTESIAN_POINT ( 'NONE',  ( -33.92644764715539196, 1450.868595403629342, 136.1710051450618835 ) ) ;
#54530 = CARTESIAN_POINT ( 'NONE',  ( -13.30454290660000005, 1409.377665263330073, 191.4591812459979963 ) ) ;
#54531 = CARTESIAN_POINT ( 'NONE',  ( -22.14212065537508778, 1379.609184651877058, 213.9947383123216014 ) ) ;
#54533 = CARTESIAN_POINT ( 'NONE',  ( 20.12874795999999833, 1473.837606016890049, 209.1218459616989946 ) ) ;
#54532 = CARTESIAN_POINT ( 'NONE',  ( -24.34453575608964826, 1439.510801930967091, 212.0368851435746933 ) ) ;
#54534 = CARTESIAN_POINT ( 'NONE',  ( -9.678629675803538390, 1438.172449264850002, 211.2476436863910010 ) ) ;
#54535 = CARTESIAN_POINT ( 'NONE',  ( -6.127742290290780325, 1511.645100227919784, 200.3268099136730314 ) ) ;
#54536 = CARTESIAN_POINT ( 'NONE',  ( -2.472529913803023227, 1523.678648413191695, 175.3762130535718597 ) ) ;
#54537 = CARTESIAN_POINT ( 'NONE',  ( -13.80504973719999917, 1434.979586003610166, 149.9810040114979870 ) ) ;
#54538 = CARTESIAN_POINT ( 'NONE',  ( -5.388545155500000128, 1508.534844389690079, 220.1281070202990122 ) ) ;
#54540 = CARTESIAN_POINT ( 'NONE',  ( 5.501490042989999552, 1437.654011727689976, 208.9193339014500168 ) ) ;
#54539 = CARTESIAN_POINT ( 'NONE',  ( 4.458165412510000536, 1464.757726041729939, 234.6072865489980188 ) ) ;
#54541 = B_SPLINE_SURFACE_WITH_KNOTS ( 'NONE', 5, 5, ( 
 ( #80193, #2415, #45517, #44960, #55558, #11888, #80745, #79659, #54468 ),
 ( #104841, #37080, #4054, #38180, #4590, #20814, #27577, #53355, #3511 ),
 ( #37635, #87500, #10790, #58300, #14624, #92422, #109258, #39838, #82397 ),
 ( #23013, #48254, #15697, #21897, #5694, #82934, #64514, #65608, #23573 ),
 ( #24108, #65053, #49900, #49349, #74557, #48811, #40933, #74001, #75111 ),
 ( #57217, #31426, #66715, #84035, #108133, #83476, #56095, #31982, #38723 ),
 ( #15158, #100292, #99720, #32542, #6769, #57766, #91885, #91343, #72898 ),
 ( #107038, #73457, #30325, #90222, #14065, #108690, #56648, #6225, #39282 ),
 ( #40380, #99166, #90782, #66172, #100821, #13507, #98629, #47695, #81823 ) ),
 .UNSPECIFIED., .F., .F., .F.,
 ( 6, 3, 6 ),
 ( 6, 3, 6 ),
 ( 14.04571185090000007, 21.32310247789999735, 23.98960798969999786 ),
 ( 0.000000000000000000, 1.000000000000000000, 2.000000000000000000 ),
 .UNSPECIFIED. ) ;
#54542 = CARTESIAN_POINT ( 'NONE',  ( 0.01171160595180150039, 1516.939568781210028, 215.6786969668069958 ) ) ;
#54543 = CARTESIAN_POINT ( 'NONE',  ( -32.39779788405879657, 1524.816846803860926, 217.0524034676090537 ) ) ;
#54544 = CARTESIAN_POINT ( 'NONE',  ( 5.987023787224379667, 1511.685461860059831, 217.5892553512100278 ) ) ;
#54545 = CARTESIAN_POINT ( 'NONE',  ( 27.79064039369999861, 1508.605033448830227, 207.7520403698979976 ) ) ;
#54546 = CARTESIAN_POINT ( 'NONE',  ( 5.011678838024999472, 1516.989560013210166, 212.3778133565769792 ) ) ;
#54547 = DIRECTION ( 'NONE',  ( -0.08340294689716752641, -0.004098122787120126072, -0.9965074780645100105 ) ) ;
#54548 = CARTESIAN_POINT ( 'NONE',  ( -34.68852446352935459, 1501.977400791986611, 218.2490599186011764 ) ) ;
#54550 = ORIENTED_EDGE ( 'NONE', *, *, #25614, .F. ) ;
#54549 = CARTESIAN_POINT ( 'NONE',  ( -109.9987473150000028, 1388.279950299490110, 298.2983701788589883 ) ) ;
#54551 = CARTESIAN_POINT ( 'NONE',  ( -18.51267908742608626, 1508.236097877770362, 229.7333076609436944 ) ) ;
#54552 = CARTESIAN_POINT ( 'NONE',  ( 28.33103133819999897, 1450.578314058649994, 240.1819618854979979 ) ) ;
#54553 = CARTESIAN_POINT ( 'NONE',  ( -16.48650050839999892, 1458.966229476530089, 230.7111281069979896 ) ) ;
#54554 = CARTESIAN_POINT ( 'NONE',  ( -15.33858234790000097, 1415.710400555009983, 207.8621270138890225 ) ) ;
#54555 = CARTESIAN_POINT ( 'NONE',  ( -0.4228048877666359950, 1508.822484023469769, 238.3615180857069902 ) ) ;
#54556 = CARTESIAN_POINT ( 'NONE',  ( 7.374483138519999592, 1422.905762710230192, 195.5806561682990150 ) ) ;
#54557 = AXIS2_PLACEMENT_3D ( 'NONE', #67612, #7139, #74911 ) ;
#54559 = CARTESIAN_POINT ( 'NONE',  ( 2.500000000000000000, 1419.446092955830181, 146.1320802672979937 ) ) ;
#54558 = CARTESIAN_POINT ( 'NONE',  ( 11.87312836989999987, 1432.864053697380086, 149.9809862119980153 ) ) ;
#54560 = CARTESIAN_POINT ( 'NONE',  ( -9.811846248468439668, 1449.015403504370170, 207.4084956377189997 ) ) ;
#54561 = CARTESIAN_POINT ( 'NONE',  ( -104.0127261669699976, 1380.213078394089962, 306.6829892870579783 ) ) ;
#54562 = ORIENTED_EDGE ( 'NONE', *, *, #73976, .F. ) ;
#54563 = CARTESIAN_POINT ( 'NONE',  ( 1.704794803334999997, 1517.096587378560116, 204.4952540647470016 ) ) ;
#54564 = CARTESIAN_POINT ( 'NONE',  ( 1.334517921909999849, 1405.730281140330135, 267.8533188392980264 ) ) ;
#54565 = AXIS2_PLACEMENT_3D ( 'NONE', #79603, #105343, #44346 ) ;
#54566 = CARTESIAN_POINT ( 'NONE',  ( 1.070047859700000048, 1515.100834970490041, 213.4503509424489778 ) ) ;
#54567 = VECTOR ( 'NONE', #107405, 1000.000000000000227 ) ;
#54568 = CARTESIAN_POINT ( 'NONE',  ( 42.54900313428320402, 1445.932418601849804, 270.0692078791809649 ) ) ;
#54569 = CARTESIAN_POINT ( 'NONE',  ( 5.510117011110000185, 1440.199971711759872, 154.7606381671979818 ) ) ;
#54570 = CARTESIAN_POINT ( 'NONE',  ( 11.60004869885203682, 1422.222932908421399, 137.0999999980977293 ) ) ;
#54571 = CARTESIAN_POINT ( 'NONE',  ( -45.67177343128329881, 1440.913044206929953, 266.1885934837860077 ) ) ;
#54572 = CARTESIAN_POINT ( 'NONE',  ( 10.34950188612880062, 1451.639534178259964, 207.2650128704659949 ) ) ;
#54573 = DIRECTION ( 'NONE',  ( 0.000000000000000000, 1.000000000000000000, 0.000000000000000000 ) ) ;
#54574 = CARTESIAN_POINT ( 'NONE',  ( 10.52570377039936567, 1462.363426962881704, 212.2902492825397474 ) ) ;
#54575 = CARTESIAN_POINT ( 'NONE',  ( 0.8058486770669990307, 1507.409867506390128, 220.9636447390989815 ) ) ;
#54576 = CARTESIAN_POINT ( 'NONE',  ( -5.313130013509999472, 1438.470987382389922, 207.5386937753289942 ) ) ;
#54577 = ORIENTED_EDGE ( 'NONE', *, *, #70506, .T. ) ;
#54578 = CARTESIAN_POINT ( 'NONE',  ( -3.804422478559999821, 1422.873164475230169, 234.3916895697979612 ) ) ;
#54579 = CARTESIAN_POINT ( 'NONE',  ( 10.91046689108939916, 1469.917267936679991, 205.8964561295520070 ) ) ;
#54580 = CARTESIAN_POINT ( 'NONE',  ( -0.2144367069559999783, 1475.560912059630027, 269.2947081849980009 ) ) ;
#54581 = CARTESIAN_POINT ( 'NONE',  ( -4.265921920120119282, 1446.647485887290031, 158.6289097731119853 ) ) ;
#54582 = CARTESIAN_POINT ( 'NONE',  ( -30.80549360313099072, 1524.130440953581001, 196.3987987232749219 ) ) ;
#54583 = CARTESIAN_POINT ( 'NONE',  ( -18.46438761643240056, 1509.557851011080174, 231.7133587057680018 ) ) ;
#54584 = CARTESIAN_POINT ( 'NONE',  ( -38.78333047650129828, 1384.792994315660053, 240.0455148828049801 ) ) ;
#54585 = CARTESIAN_POINT ( 'NONE',  ( -18.71036172829999700, 1415.996778984329922, 208.1550592490559950 ) ) ;
#54586 = CARTESIAN_POINT ( 'NONE',  ( -9.793579503809999309, 1482.279599785289975, 204.6454782706190088 ) ) ;
#54587 = CARTESIAN_POINT ( 'NONE',  ( 26.68598823788470042, 1436.588321450659805, 136.7639126871760027 ) ) ;
#54588 = VECTOR ( 'NONE', #97305, 1000.000000000000000 ) ;
#54589 = CARTESIAN_POINT ( 'NONE',  ( -4.597933714602949529, 1396.073623771769917, 219.1466160566309895 ) ) ;
#54590 = CARTESIAN_POINT ( 'NONE',  ( -2.994312402752280278, 1508.551704408389924, 204.1866477444860095 ) ) ;
#54591 = CARTESIAN_POINT ( 'NONE',  ( 7.320561577120000329, 1432.353341358199941, 149.5448088695980005 ) ) ;
#54592 = EDGE_CURVE ( 'NONE', #71185, #64042, #9302, .T. ) ;
#54593 = ORIENTED_EDGE ( 'NONE', *, *, #76944, .T. ) ;
#54594 = CARTESIAN_POINT ( 'NONE',  ( -11.35404705328023844, 1501.711889457069674, 207.5713905607231027 ) ) ;
#54595 = CARTESIAN_POINT ( 'NONE',  ( 2.431084916239999671, 1409.932888328230092, 231.7225720581979829 ) ) ;
#54596 = CIRCLE ( 'NONE', #2719, 1.000000000000000888 ) ;
#54597 = CARTESIAN_POINT ( 'NONE',  ( -11.73563882241239931, 1425.610159415710086, 144.1657444112690030 ) ) ;
#54599 = CARTESIAN_POINT ( 'NONE',  ( -14.28353075656500160, 1513.113451381389950, 193.4746005378669906 ) ) ;
#54598 = CARTESIAN_POINT ( 'NONE',  ( 11.09525485650000043, 1425.652349456129969, 121.0021085274979953 ) ) ;
#54600 = LINE ( 'NONE', #107170, #27199 ) ;
#54601 = CARTESIAN_POINT ( 'NONE',  ( -13.07882001760000179, 1380.090973434839952, 209.8378495415080067 ) ) ;
#54602 = B_SPLINE_CURVE_WITH_KNOTS ( 'NONE', 5,
 ( #22786, #56992, #13843, #4380, #21133, #29025 ),
 .UNSPECIFIED., .F., .F.,
 ( 6, 6 ),
 ( 0.000000000000000000, 1.000000000000000000 ),
 .UNSPECIFIED. ) ;
#54603 = CARTESIAN_POINT ( 'NONE',  ( -109.9877442644620089, 1384.809409080889964, 311.4546249735340098 ) ) ;
#54604 = CARTESIAN_POINT ( 'NONE',  ( 7.537484560389999366, 1425.561342251899987, 212.1802124335790154 ) ) ;
#54605 = CARTESIAN_POINT ( 'NONE',  ( -21.51339057090000040, 1505.551704408389924, 209.1218459616989946 ) ) ;
#54606 = CARTESIAN_POINT ( 'NONE',  ( 1.669890710080000007, 1508.956865050929991, 179.7751757191980175 ) ) ;
#54607 = DIRECTION ( 'NONE',  ( 0.000000000000000000, 0.000000000000000000, 1.000000000000000000 ) ) ;
#54608 = CARTESIAN_POINT ( 'NONE',  ( -93.86205675402460713, 1379.086295911220077, 304.7318000099389792 ) ) ;
#54609 = CARTESIAN_POINT ( 'NONE',  ( 5.215187551879999717, 1368.779556716650177, 207.6218459616989946 ) ) ;
#54611 = ORIENTED_EDGE ( 'NONE', *, *, #47038, .F. ) ;
#54610 = CARTESIAN_POINT ( 'NONE',  ( -16.70762542998109978, 1379.711292899869932, 211.9326756087270098 ) ) ;
#54612 = ORIENTED_EDGE ( 'NONE', *, *, #51552, .F. ) ;
#54613 = EDGE_CURVE ( 'NONE', #65987, #48650, #84055, .T. ) ;
#54614 = CARTESIAN_POINT ( 'NONE',  ( -8.589176046050001290, 1397.858446770630053, 199.0029481086979786 ) ) ;
#54615 = CARTESIAN_POINT ( 'NONE',  ( 0.4520741306692179773, 1482.864041210959840, 236.3239132953789863 ) ) ;
#54616 = CARTESIAN_POINT ( 'NONE',  ( 13.91344329460000040, 1453.313060387329870, 224.4164659125979995 ) ) ;
#54617 = CARTESIAN_POINT ( 'NONE',  ( -7.548872338225000256, 1510.418062979269962, 214.3032561208869993 ) ) ;
#54619 = CARTESIAN_POINT ( 'NONE',  ( 11.22085813615770000, 1414.913060387329779, 197.6243702374680140 ) ) ;
#54618 = CARTESIAN_POINT ( 'NONE',  ( -105.0196309849999921, 1390.463858102760014, 304.1900860135590392 ) ) ;
#54620 = CARTESIAN_POINT ( 'NONE',  ( 6.602193856980000497, 1410.296089514130017, 187.0051498391979976 ) ) ;
#54621 = ADVANCED_FACE ( 'NONE', ( #58247 ), #100238, .T. ) ;
#54622 = CARTESIAN_POINT ( 'NONE',  ( -39.76109132672340252, 1448.193450711350124, 136.2665313895609813 ) ) ;
#54623 = DIRECTION ( 'NONE',  ( -0.6709778558543766369, 0.000000000000000000, -0.7414773880254632576 ) ) ;
#54624 = CARTESIAN_POINT ( 'NONE',  ( 3.286051671319225598, 1371.185232598742687, 209.6218459617033432 ) ) ;
#54625 = CARTESIAN_POINT ( 'NONE',  ( -17.04532912216367180, 1519.551704408389924, 196.9538555332918293 ) ) ;
#54626 = CARTESIAN_POINT ( 'NONE',  ( -3.818053759430319882, 1406.099154933030150, 266.9556830280999975 ) ) ;
#54627 = FACE_OUTER_BOUND ( 'NONE', #90014, .T. ) ;
#54628 = ORIENTED_EDGE ( 'NONE', *, *, #50782, .F. ) ;
#54629 = CARTESIAN_POINT ( 'NONE',  ( 4.363122458829999495, 1423.854802366329977, 183.5697733487979804 ) ) ;
#54630 = CARTESIAN_POINT ( 'NONE',  ( 21.35005939118691032, 1525.163457223744672, 234.4064223797113868 ) ) ;
#54631 = B_SPLINE_CURVE_WITH_KNOTS ( 'NONE', 3,
 ( #16180, #7256, #51463, #103508, #8894, #42504, #76664, #86167, #83956, #60999, #76117, #43073, #77233, #534, #59338, #92906, #84508, #43625, #7797, #110813, #110257, #59881, #34658, #68842, #33533, #102945, #68297, #34106, #41418, #101842, #25135, #93448, #32991, #77773, #1085, #26247, #75584, #102405, #16718, #60435, #50919, #85050, #94553, #17826, #35211, #95125, #67180, #71061, #97322 ),
 .UNSPECIFIED., .F., .F.,
 ( 4, 3, 3, 3, 3, 3, 3, 3, 3, 3, 3, 3, 3, 3, 3, 3, 4 ),
 ( -12.57638456930000004, -12.28317881154790037, -11.95680856226570121, -11.62570944429999997, -11.51472436866950133, -11.17721019273979977, -10.83638269430850087, -10.49376597961390090, -10.14927726971910005, -9.804494079901610704, -9.458815398425139520, -9.117616600358399381, -8.780289087992249719, -8.445887014764290157, -8.114782773701358920, -7.787209585419999414, -7.548674336829999554 ),
 .UNSPECIFIED. ) ;
#54633 = EDGE_LOOP ( 'NONE', ( #103797, #98620, #98927, #26225 ) ) ;
#54632 = B_SPLINE_CURVE_WITH_KNOTS ( 'NONE', 3,
 ( #71567, #48533, #73740, #38996, #55840, #98362, #90509, #5963, #89962, #97806, #73173, #29501, #106758, #65888, #82109, #91616, #21084, #13785, #81549, #14893, #107863, #22727, #5407, #13236, #31152, #46892, #80474, #56929, #3792, #14343, #65341, #30048, #47426, #81016, #55288, #89418, #72627, #64240, #37923, #4324, #64799, #38454, #21635, #91057, #22180, #98908, #4849, #107317, #72104, #63695, #30612, #56377, #23295, #31704, #47967, #99450, #57492, #106219, #39567, #40108, #74290, #108421, #100007, #84848, #77035, #74835, #75920, #34470, #50719, #16528, #8149, #7607, #76470, #59144, #41218, #83219, #66987, #15441, #33348, #7063, #49632, #23840, #32265, #93797, #101098, #109527, #24398, #68100, #75390, #102215, #67543, #343, #84316, #42316 ),
 .UNSPECIFIED., .F., .F.,
 ( 4, 3, 3, 3, 3, 3, 3, 3, 3, 3, 3, 3, 3, 3, 3, 3, 3, 3, 3, 3, 3, 3, 3, 3, 3, 3, 3, 3, 3, 3, 3, 4 ),
 ( -31.18846563725180232, -31.00774817696539998, -29.91343961047510192, -28.82901376052130260, -27.75228773005839855, -26.68937329812260018, -25.63621693740660135, -24.59289539267759750, -23.55938141437490074, -22.54133121024409903, -21.54281980820089970, -20.54474872284400178, -19.55609317380470102, -18.57652819858910220, -17.60572709955240001, -16.64336675927789955, -15.67369350074630141, -14.07561117147439944, -12.28927372929120310, -10.62231242529870201, -8.938518733482830214, -7.370289770217699044, -5.839433697936598833, -4.341848494604818143, -4.231108194414311185, -2.815296474105110747, -1.445085169337431807, -0.1034094330291317476, 1.196738312870451182, 2.472340971179193048, 3.725905068250661145, 4.959507408170033216 ),
 .UNSPECIFIED. ) ;
#54634 = VERTEX_POINT ( 'NONE', #109204 ) ;
#54635 = CARTESIAN_POINT ( 'NONE',  ( 32.38114538885255200, 1523.604703353109699, 216.1203639561429100 ) ) ;
#54636 = CARTESIAN_POINT ( 'NONE',  ( 20.45347777980000004, 1495.695647834889996, 214.2365953844490036 ) ) ;
#54637 = CARTESIAN_POINT ( 'NONE',  ( 7.719392382375000139, 1516.929962200689943, 215.6766245038770080 ) ) ;
#54638 = CARTESIAN_POINT ( 'NONE',  ( 2.566007165815000324, 1512.021995456199875, 216.7432650908669984 ) ) ;
#54639 = VERTEX_POINT ( 'NONE', #5069 ) ;
#54640 = CARTESIAN_POINT ( 'NONE',  ( 2.500000000000000000, 1448.397602632589951, 162.2732098858260201 ) ) ;
#54641 = CARTESIAN_POINT ( 'NONE',  ( -72.92954128540000625, 1379.405105560169886, 284.3347022608589896 ) ) ;
#54642 = AXIS2_PLACEMENT_3D ( 'NONE', #74533, #58821, #6200 ) ;
#54643 = ADVANCED_FACE ( 'NONE', ( #41443 ), #98573, .F. ) ;
#54644 = CARTESIAN_POINT ( 'NONE',  ( -15.17646696946499851, 1516.904916668740043, 225.0580773729669772 ) ) ;
#54645 = CARTESIAN_POINT ( 'NONE',  ( -3.266349512195000138, 1516.797038924770050, 205.0935381919470046 ) ) ;
#54646 = CARTESIAN_POINT ( 'NONE',  ( -31.17186646729999921, 1440.913060387330006, 255.0393818639979884 ) ) ;
#54647 = B_SPLINE_SURFACE_WITH_KNOTS ( 'NONE', 5, 5, ( 
 ( #5891, #5333, #40037, #107796, #78615, #8080 ),
 ( #76962, #110550, #78053, #43910, #271, #85899 ),
 ( #43366, #85330, #52330, #42250, #34398, #1930 ),
 ( #93188, #84783, #27112, #68572, #50652, #67470 ),
 ( #101575, #1359, #25415, #18679, #77514, #59609 ),
 ( #815, #102137, #24863, #102672, #94286, #76397 ) ),
 .UNSPECIFIED., .F., .F., .F.,
 ( 6, 6 ),
 ( 6, 6 ),
 ( 8.853503526680000846, 11.83085891290000013 ),
 ( 0.000000000000000000, 1.446538132919999997 ),
 .UNSPECIFIED. ) ;
#54648 = B_SPLINE_CURVE_WITH_KNOTS ( 'NONE', 5,
 ( #19896, #106663, #62506, #70905, #2588, #27755, #61948, #54646, #105585, #89319, #71467, #54099 ),
 .UNSPECIFIED., .F., .F.,
 ( 6, 3, 3, 6 ),
 ( -32.81232995010000053, -6.990622299171700860, 15.67373306494047114, 31.61444093042090486 ),
 .UNSPECIFIED. ) ;
#54649 = CARTESIAN_POINT ( 'NONE',  ( -109.9987473190000031, 1384.904025801279886, 297.1695833602590255 ) ) ;
#54650 = CARTESIAN_POINT ( 'NONE',  ( -9.910331035380000486, 1409.425488993030058, 229.0636521845979985 ) ) ;
#54652 = ORIENTED_EDGE ( 'NONE', *, *, #110431, .F. ) ;
#54651 = FACE_OUTER_BOUND ( 'NONE', #53181, .T. ) ;
#54653 = CARTESIAN_POINT ( 'NONE',  ( 27.84004021000000151, 1451.940495779430194, 134.8938502556979984 ) ) ;
#54654 = CARTESIAN_POINT ( 'NONE',  ( 1.726858845393010045, 1482.796399496739923, 235.4332745739710049 ) ) ;
#54655 = CARTESIAN_POINT ( 'NONE',  ( 20.59684376970620079, 1507.762609625729965, 227.3086063979779965 ) ) ;
#54656 = CARTESIAN_POINT ( 'NONE',  ( -13.33054336736499934, 1517.051704408389924, 207.1218459511669892 ) ) ;
#54657 = B_SPLINE_CURVE_WITH_KNOTS ( 'NONE', 3,
 ( #109649, #22855, #23961, #76594, #32926, #101773, #83886, #48660, #6080, #40232, #7730, #67115, #93384, #65463, #110192, #74415, #83335, #25064, #108541, #91735, #31830, #66017, #40785, #75516, #100140, #84976, #59267, #67666, #50848, #6631, #8271, #33465, #23426, #74962, #109112, #32392, #49756, #66573, #100678, #58156, #15556, #101216, #41348 ),
 .UNSPECIFIED., .F., .F.,
 ( 4, 3, 3, 3, 3, 3, 3, 3, 3, 3, 3, 3, 3, 3, 4 ),
 ( -77.98061142476200303, -77.46682292029849748, -77.28802957387100037, -76.91618970811789779, -75.85176799147379256, -74.38254242284349971, -72.90580023232000428, -71.43113070119559893, -69.96812857060400859, -68.52304788189539408, -67.09990280889999781, -66.55476356243740099, -65.17590846059749765, -63.76822099488400397, -62.33963421249379877 ),
 .UNSPECIFIED. ) ;
#54658 = CARTESIAN_POINT ( 'NONE',  ( 41.83993043035380310, 1432.387293077269760, 270.1928086331030272 ) ) ;
#54659 = CARTESIAN_POINT ( 'NONE',  ( 7.724423394095000894, 1517.122088787240045, 212.5760185856570104 ) ) ;
#54660 = CARTESIAN_POINT ( 'NONE',  ( -67.64911565900000312, 1379.747065449480033, 277.8485390883590185 ) ) ;
#54661 = CARTESIAN_POINT ( 'NONE',  ( -25.91590772737680126, 1441.261220175949802, 138.4451201564890255 ) ) ;
#54662 = CARTESIAN_POINT ( 'NONE',  ( 13.28133272618789995, 1426.800456727919936, 196.8617550854280012 ) ) ;
#54664 = CARTESIAN_POINT ( 'NONE',  ( 19.42032769166468853, 1410.952570011139869, 196.1050306194517816 ) ) ;
#54663 = VECTOR ( 'NONE', #43395, 1000.000000000000000 ) ;
#54665 = CARTESIAN_POINT ( 'NONE',  ( 3.267039691854999983, 1517.012231669750008, 209.8574146130079896 ) ) ;
#54666 = ORIENTED_EDGE ( 'NONE', *, *, #56421, .F. ) ;
#54667 = CARTESIAN_POINT ( 'NONE',  ( 23.10442899973940101, 1411.095127650270115, 207.3185325528490068 ) ) ;
#54668 = CARTESIAN_POINT ( 'NONE',  ( -33.91369120209999721, 1435.681798817170147, 134.0999999980979851 ) ) ;
#54669 =( BOUNDED_CURVE ( )  B_SPLINE_CURVE ( 3, ( #7047, #14330, #65870, #32251 ),
 .UNSPECIFIED., .F., .F. ) 
 B_SPLINE_CURVE_WITH_KNOTS ( ( 4, 4 ),
 ( 6.239037601373940589, 6.281338949178555175 ),
 .UNSPECIFIED. ) 
 CURVE ( )  GEOMETRIC_REPRESENTATION_ITEM ( )  RATIONAL_B_SPLINE_CURVE ( ( 1.000000000000000000, 0.9998508885567132243, 0.9998508885567132243, 1.000000000000000000 ) ) 
 REPRESENTATION_ITEM ( '' )  );
#54670 = FACE_OUTER_BOUND ( 'NONE', #59737, .T. ) ;
#54671 = ORIENTED_EDGE ( 'NONE', *, *, #92439, .T. ) ;
#54672 = CARTESIAN_POINT ( 'NONE',  ( -28.75295618251070096, 1385.239309608959957, 226.7833509653069939 ) ) ;
#54673 = CARTESIAN_POINT ( 'NONE',  ( -7.396545081224999763, 1511.069621805459974, 215.4940135707269917 ) ) ;
#54674 = AXIS2_PLACEMENT_3D ( 'NONE', #62787, #1200, #20173 ) ;
#54675 = DIRECTION ( 'NONE',  ( -0.6456624059243071256, -0.004098122786995253737, 0.7636119845613070778 ) ) ;
#54676 = CARTESIAN_POINT ( 'NONE',  ( 7.583791906034999641, 1511.751588929339960, 206.7961148284170179 ) ) ;
#54677 = CARTESIAN_POINT ( 'NONE',  ( -0.2517843955729999750, 1408.921852844929845, 232.2115700972980221 ) ) ;
#54678 = CARTESIAN_POINT ( 'NONE',  ( 2.632631803615880450, 1417.642869435429930, 234.7516633181379859 ) ) ;
#54680 = CARTESIAN_POINT ( 'NONE',  ( -4.523944140811339665, 1455.378620635879997, 200.8408219016489795 ) ) ;
#54679 = CARTESIAN_POINT ( 'NONE',  ( -4.033653302454999867, 1517.028034847769959, 215.6825881955670070 ) ) ;
#54681 = DIRECTION ( 'NONE',  ( -1.755985294532469921E-16, 1.000000000000000000, -1.338183447452831989E-16 ) ) ;
#54682 = CARTESIAN_POINT ( 'NONE',  ( 10.23319004314000047, 1470.053042612599938, 209.0118140887069842 ) ) ;
#54683 = ORIENTED_EDGE ( 'NONE', *, *, #24674, .T. ) ;
#54684 = CARTESIAN_POINT ( 'NONE',  ( 7.717505752974999744, 1516.857914730730045, 201.4043401791270185 ) ) ;
#54685 = CARTESIAN_POINT ( 'NONE',  ( -16.11904265886499843, 1512.169992403149990, 220.5902712816669862 ) ) ;
#54686 = ORIENTED_EDGE ( 'NONE', *, *, #20041, .F. ) ;
#54687 = DIRECTION ( 'NONE',  ( 0.1010290445074209786, 0.000000000000000000, 0.9948834766775040972 ) ) ;
#54688 = CARTESIAN_POINT ( 'NONE',  ( 10.56668910718356535, 1434.889276759676477, 152.0929273929996839 ) ) ;
#54689 = CARTESIAN_POINT ( 'NONE',  ( 38.61927353243170558, 1444.188088105049928, 137.1592452208769828 ) ) ;
#54690 = PRODUCT_DEFINITION_CONTEXT ( 'detailed design', #104952, 'design' ) ;
#54691 = CARTESIAN_POINT ( 'NONE',  ( 0.3990618680159989662, 1443.956493356090050, 218.0653600664390126 ) ) ;
#54692 = DIRECTION ( 'NONE',  ( -1.000000000000000000, 0.000000000000000000, 0.000000000000000000 ) ) ;
#54693 = CARTESIAN_POINT ( 'NONE',  ( 6.301535050710000085, 1423.297843521130062, 186.2731961210980103 ) ) ;
#54694 = CARTESIAN_POINT ( 'NONE',  ( -17.84818147429999868, 1423.997650907529987, 226.0612537164979869 ) ) ;
#54695 = CARTESIAN_POINT ( 'NONE',  ( -14.99308972890000113, 1435.024836507099963, 148.2840791620979815 ) ) ;
#54696 = CARTESIAN_POINT ( 'NONE',  ( 33.91369266730000476, 1450.440660192670066, 136.2454535554979884 ) ) ;
#54697 = CARTESIAN_POINT ( 'NONE',  ( -1.735723226805210073, 1473.469101322430106, 183.2265203639830133 ) ) ;
#54699 = CARTESIAN_POINT ( 'NONE',  ( -17.60714162564125118, 1434.290496652245110, 215.9208836820417332 ) ) ;
#54698 = CYLINDRICAL_SURFACE ( 'NONE', #19675, 4.000000000000007994 ) ;
#54700 = CARTESIAN_POINT ( 'NONE',  ( 2.425477467415915189, 1523.390106123591067, 243.0915840373823471 ) ) ;
#54701 = VERTEX_POINT ( 'NONE', #32489 ) ;
#54702 = CARTESIAN_POINT ( 'NONE',  ( -105.6234263439999950, 1377.955790496569762, 303.2972783946590312 ) ) ;
#54703 = LINE ( 'NONE', #97771, #53581 ) ;
#54705 = VERTEX_POINT ( 'NONE', #13447 ) ;
#54704 = CARTESIAN_POINT ( 'NONE',  ( -3.448830483803564828, 1512.187213306747481, 243.0842028158767789 ) ) ;
#54706 = DIRECTION ( 'NONE',  ( 0.7063774289747313251, 0.04540766091858271930, -0.7063774289747313251 ) ) ;
#54707 = CARTESIAN_POINT ( 'NONE',  ( 29.00779973304137371, 1526.382868172863937, 217.2942086403122914 ) ) ;
#54708 = CARTESIAN_POINT ( 'NONE',  ( -16.69414477714984102, 1417.182685337895919, 207.2247089525174317 ) ) ;
#54709 = CARTESIAN_POINT ( 'NONE',  ( -6.896890933126118993E-05, 1408.913065613199933, 231.7784170915439859 ) ) ;
#54710 = CARTESIAN_POINT ( 'NONE',  ( 11.67163616197805887, 1435.064040831317016, 151.3452733738369318 ) ) ;
#54711 = DIRECTION ( 'NONE',  ( 1.836970198721029688E-16, 1.000000000000000000, 0.000000000000000000 ) ) ;
#54712 = CARTESIAN_POINT ( 'NONE',  ( -6.844578743112079700, 1507.263722753517868, 235.7154808215367723 ) ) ;
#54713 = CARTESIAN_POINT ( 'NONE',  ( -10.87802087445689914, 1489.387117259759862, 213.6045155262730191 ) ) ;
#54714 = CARTESIAN_POINT ( 'NONE',  ( -12.04603691750549999, 1481.197963875999903, 227.9689184246500133 ) ) ;
#54715 = CARTESIAN_POINT ( 'NONE',  ( -86.90971335866299796, 1383.772295304499949, 307.3582144528240292 ) ) ;
#54716 = CIRCLE ( 'NONE', #45764, 86.30410767968433561 ) ;
#54717 = CYLINDRICAL_SURFACE ( 'NONE', #12502, 2.000000000000001776 ) ;
#54718 = CARTESIAN_POINT ( 'NONE',  ( 4.859679523539999657, 1428.484836093189870, 215.8649822896190074 ) ) ;
#54720 = ORIENTED_EDGE ( 'NONE', *, *, #56458, .T. ) ;
#54719 = CARTESIAN_POINT ( 'NONE',  ( 22.43276589599999937, 1508.963982320630066, 192.2846129824980324 ) ) ;
#54721 = CARTESIAN_POINT ( 'NONE',  ( -98.86569637809999733, 1383.405061561229786, 296.2692300583589713 ) ) ;
#54722 = CARTESIAN_POINT ( 'NONE',  ( 13.52455577884570026, 1512.715996828750121, 224.4318246187129944 ) ) ;
#54723 = ORIENTED_EDGE ( 'NONE', *, *, #17320, .T. ) ;
#54724 = VERTEX_POINT ( 'NONE', #15642 ) ;
#54725 = CARTESIAN_POINT ( 'NONE',  ( 24.24763046536200051, 1427.549423795960138, 207.7433240213180170 ) ) ;
#54726 = CARTESIAN_POINT ( 'NONE',  ( 13.77725779630000069, 1509.394201300130135, 235.0109963963979851 ) ) ;
#54727 = CARTESIAN_POINT ( 'NONE',  ( 13.14336223832311568, 1443.062568900890710, 169.3993974764935047 ) ) ;
#54729 = CARTESIAN_POINT ( 'NONE',  ( -30.53571888289999947, 1442.873932102629851, 240.1260121736980011 ) ) ;
#54728 = CARTESIAN_POINT ( 'NONE',  ( 40.51831965869402552, 1432.752226466759566, 269.6196524019716776 ) ) ;
#54730 = LINE ( 'NONE', #12142, #41163 ) ;
#54731 = CARTESIAN_POINT ( 'NONE',  ( -11.36702043620000069, 1433.804590679680132, 151.4517328811979837 ) ) ;
#54732 = CARTESIAN_POINT ( 'NONE',  ( 4.709520687179999499, 1480.407452823689937, 228.9869292435990076 ) ) ;
#54733 = CARTESIAN_POINT ( 'NONE',  ( -19.45775078520000179, 1486.277066373030038, 189.7536442620979926 ) ) ;
#54734 = CARTESIAN_POINT ( 'NONE',  ( 10.14578895520000046, 1410.638169269630225, 188.6745756209980129 ) ) ;
#54735 = CARTESIAN_POINT ( 'NONE',  ( 4.581316872830000442, 1422.049244984730194, 184.0357665752979983 ) ) ;
#54736 = CARTESIAN_POINT ( 'NONE',  ( 0.4393421188271590117, 1515.147356017579796, 213.4491327457870113 ) ) ;
#54737 = CARTESIAN_POINT ( 'NONE',  ( 16.88182070999999951, 1417.652932793330137, 226.6960533187979934 ) ) ;
#54738 = CARTESIAN_POINT ( 'NONE',  ( 12.75521900933300046, 1428.291927597070071, 223.8668883416810047 ) ) ;
#54739 = CARTESIAN_POINT ( 'NONE',  ( -22.28769322179999790, 1450.904749962159940, 143.2988008388979893 ) ) ;
#54741 = ORIENTED_EDGE ( 'NONE', *, *, #24912, .T. ) ;
#54740 = LINE ( 'NONE', #88869, #55082 ) ;
#54742 = ORIENTED_EDGE ( 'NONE', *, *, #63095, .T. ) ;
#54743 = CARTESIAN_POINT ( 'NONE',  ( -11.86119678505159847, 1431.993545301180120, 149.9716976446269996 ) ) ;
#54744 = CARTESIAN_POINT ( 'NONE',  ( 9.611475570199999652, 1494.388845096189925, 188.1518348324989915 ) ) ;
#54745 = CARTESIAN_POINT ( 'NONE',  ( -12.98194342669999912, 1470.141184529730026, 269.6330410522980401 ) ) ;
#54746 = CARTESIAN_POINT ( 'NONE',  ( -24.20882859423510070, 1435.739118765830199, 210.8967395777180229 ) ) ;
#54747 = CARTESIAN_POINT ( 'NONE',  ( -125.6580589596999431, 1375.179104070690755, 316.4799049169587306 ) ) ;
#54748 = CYLINDRICAL_SURFACE ( 'NONE', #103740, 2.000000000000003553 ) ;
#54749 = CARTESIAN_POINT ( 'NONE',  ( 0.2075316472611209995, 1452.106270034880026, 183.0908634647769873 ) ) ;
#54750 = CARTESIAN_POINT ( 'NONE',  ( -13.12562721870000182, 1421.054977677129955, 228.8117867079979817 ) ) ;
#54751 = AXIS2_PLACEMENT_3D ( 'NONE', #66785, #15762, #102539 ) ;
#54752 = CARTESIAN_POINT ( 'NONE',  ( -9.702736503189999695, 1460.950281053889967, 212.1761309882089961 ) ) ;
#54753 = CARTESIAN_POINT ( 'NONE',  ( 10.52374552228457105, 1363.241692960809132, 207.6218459616987673 ) ) ;
#54754 = CARTESIAN_POINT ( 'NONE',  ( -45.11518327334809442, 1435.673159459739963, 268.9894092425899998 ) ) ;
#54755 = VERTEX_POINT ( 'NONE', #92369 ) ;
#54756 = CARTESIAN_POINT ( 'NONE',  ( -3.545193281622200043, 1502.970594565849979, 181.1540523117359953 ) ) ;
#54757 = ORIENTED_EDGE ( 'NONE', *, *, #9057, .T. ) ;
#54758 = CARTESIAN_POINT ( 'NONE',  ( -4.997718276504999224, 1516.693851263360102, 210.2547950466569944 ) ) ;
#54759 = DIRECTION ( 'NONE',  ( -0.1215792179600209827, -0.8574474952671518047, -0.5000022866150889422 ) ) ;
#54760 = CARTESIAN_POINT ( 'NONE',  ( -20.59678674160000256, 1507.763197054029888, 190.3721467792980206 ) ) ;
#54761 = CARTESIAN_POINT ( 'NONE',  ( -14.81926257019999937, 1410.404433816730034, 190.6668097203979926 ) ) ;
#54762 = CARTESIAN_POINT ( 'NONE',  ( 1.382080682762369950, 1495.864354590530183, 221.3843093997170115 ) ) ;
#54763 = VERTEX_POINT ( 'NONE', #90725 ) ;
#54764 = CARTESIAN_POINT ( 'NONE',  ( 3.454172615424999648, 1517.122088787240045, 201.3974225380069925 ) ) ;
#54765 = CARTESIAN_POINT ( 'NONE',  ( 5.794788514299999527, 1472.774664811089906, 217.7075892082590087 ) ) ;
#54766 = CARTESIAN_POINT ( 'NONE',  ( -8.474153735295640644, 1438.741029936910081, 207.0760172009069890 ) ) ;
#54767 = ORIENTED_EDGE ( 'NONE', *, *, #1464, .T. ) ;
#54768 = CARTESIAN_POINT ( 'NONE',  ( -25.68853613209369868, 1416.734612324150021, 269.4293337505479826 ) ) ;
#54769 = CARTESIAN_POINT ( 'NONE',  ( 2.913665321129999787E-15, 1426.935925255829943, 133.6118001900980232 ) ) ;
#54770 = CARTESIAN_POINT ( 'NONE',  ( 0.006135415692569999579, 1395.974572303430023, 197.4936679487979916 ) ) ;
#54772 = ORIENTED_EDGE ( 'NONE', *, *, #6203, .T. ) ;
#54771 = CARTESIAN_POINT ( 'NONE',  ( -8.647453749692138203, 1364.394047320720802, 210.6218459617142003 ) ) ;
#54773 = ORIENTED_EDGE ( 'NONE', *, *, #51374, .T. ) ;
#54774 = CARTESIAN_POINT ( 'NONE',  ( 45.62655422193257237, 1441.650256554816224, 268.9750399244037453 ) ) ;
#54775 = EDGE_CURVE ( 'NONE', #18861, #95096, #10099, .T. ) ;
#54776 = CARTESIAN_POINT ( 'NONE',  ( 8.790084679516168009, 1511.590044791230184, 203.1124153264186418 ) ) ;
#54777 = CARTESIAN_POINT ( 'NONE',  ( -14.25110351248640050, 1436.256065985239957, 150.0865086527120127 ) ) ;
#54778 = CARTESIAN_POINT ( 'NONE',  ( 17.80990364915628632, 1474.300541546459954, 199.4615574247595760 ) ) ;
#54779 = CARTESIAN_POINT ( 'NONE',  ( -18.11230055478630163, 1415.348334732599824, 207.5667894811009830 ) ) ;
#54780 = CARTESIAN_POINT ( 'NONE',  ( -23.11183678279999754, 1435.763572499130078, 215.1866059518479801 ) ) ;
#54781 = CARTESIAN_POINT ( 'NONE',  ( 22.35545660506620180, 1471.322756690530014, 269.3294010533080609 ) ) ;
#54782 = CARTESIAN_POINT ( 'NONE',  ( 11.70751967719999875, 1415.128105756529976, 222.5965497224979970 ) ) ;
#54783 = CARTESIAN_POINT ( 'NONE',  ( -17.73406580063780069, 1423.343214054229975, 226.1884525926029994 ) ) ;
#54784 = CARTESIAN_POINT ( 'NONE',  ( -7.725372170364999569, 1517.158319634930194, 206.2490093095770192 ) ) ;
#54785 = ORIENTED_EDGE ( 'NONE', *, *, #54299, .T. ) ;
#54786 = CARTESIAN_POINT ( 'NONE',  ( -2.234897892418939769, 1512.314859079350072, 200.5229006381079842 ) ) ;
#54787 = CARTESIAN_POINT ( 'NONE',  ( -22.48690821953700691, 1451.619460217190408, 219.5055000607859483 ) ) ;
#54788 = EDGE_LOOP ( 'NONE', ( #67319, #6568, #35731 ) ) ;
#54789 = CARTESIAN_POINT ( 'NONE',  ( 10.58313173430331489, 1455.148896507045947, 226.2839261739179051 ) ) ;
#54790 = CARTESIAN_POINT ( 'NONE',  ( 25.21692146640110010, 1450.980894760169804, 137.5957989584090058 ) ) ;
#54791 = CARTESIAN_POINT ( 'NONE',  ( -15.09047375999176843, 1522.051704408389924, 202.6311677367078232 ) ) ;
#54792 = CARTESIAN_POINT ( 'NONE',  ( -9.122186852882011365, 1384.516432268700100, 199.9701712313529924 ) ) ;
#54793 = CARTESIAN_POINT ( 'NONE',  ( 21.01921312860000057, 1410.567660014329931, 199.9123866135879837 ) ) ;
#54794 = CARTESIAN_POINT ( 'NONE',  ( -2.964074117308931111, 1446.907475440849339, 170.5322007353207994 ) ) ;
#54795 = CARTESIAN_POINT ( 'NONE',  ( 17.29614329919999705, 1410.879761755329810, 225.9915122344980034 ) ) ;
#54796 = CARTESIAN_POINT ( 'NONE',  ( 10.20961878419999991, 1488.772996682489975, 205.0373668638989955 ) ) ;
#54797 = CARTESIAN_POINT ( 'NONE',  ( 0.5349531902123869642, 1451.469306295839942, 182.7928085713219843 ) ) ;
#54798 = B_SPLINE_CURVE_WITH_KNOTS ( 'NONE', 3,
 ( #47819, #23703, #24250, #57887 ),
 .UNSPECIFIED., .F., .F.,
 ( 4, 4 ),
 ( 0.000000000000000000, 1.000000000000000000 ),
 .UNSPECIFIED. ) ;
#54799 = CARTESIAN_POINT ( 'NONE',  ( 2.500000000000000000, 1439.402073890429847, 161.8071954337849832 ) ) ;
#54800 = CARTESIAN_POINT ( 'NONE',  ( 1.130607463874999885, 1516.632821972880038, 215.6700465578769865 ) ) ;
#54801 = CARTESIAN_POINT ( 'NONE',  ( 2.692976938448822466, 1524.059547553519224, 242.0866667222398121 ) ) ;
#54802 = ORIENTED_EDGE ( 'NONE', *, *, #15076, .T. ) ;
#54803 = LINE ( 'NONE', #45311, #72368 ) ;
#54804 = CARTESIAN_POINT ( 'NONE',  ( -10.01326586723869916, 1481.014341800280135, 205.7823588363200145 ) ) ;
#54805 = CARTESIAN_POINT ( 'NONE',  ( 15.12003195112066933, 1517.051704408389924, 199.7262892757531745 ) ) ;
#54806 = TOROIDAL_SURFACE ( 'NONE', #6508, 1.000000000000000000, 1.000000000000000000 ) ;
#54807 = EDGE_CURVE ( 'NONE', #4305, #22619, #14009, .T. ) ;
#54808 = CARTESIAN_POINT ( 'NONE',  ( -11.60004869885203682, 0.000000000000000000, 137.0999999980979851 ) ) ;
#54809 = ADVANCED_FACE ( 'NONE', ( #99662 ), #1593, .F. ) ;
#54810 = CARTESIAN_POINT ( 'NONE',  ( -36.80391333867880377, 1449.651525888219794, 136.2794198540989896 ) ) ;
#54811 = EDGE_CURVE ( 'NONE', #8029, #41235, #37932, .T. ) ;
#54812 = CARTESIAN_POINT ( 'NONE',  ( 11.60004869885203682, 1425.221648007341628, 138.0074162802604860 ) ) ;
#54813 = CARTESIAN_POINT ( 'NONE',  ( 2.378525042339323825, 1417.651026746295884, 233.6043764637433355 ) ) ;
#54814 = B_SPLINE_CURVE_WITH_KNOTS ( 'NONE', 5,
 ( #84408, #42970, #67082, #58668, #32888, #59232 ),
 .UNSPECIFIED., .F., .F.,
 ( 6, 6 ),
 ( 396.1714721989999930, 406.4187164909999979 ),
 .UNSPECIFIED. ) ;
#54815 = CARTESIAN_POINT ( 'NONE',  ( -14.31200010202953621, 1415.739699867087893, 203.9225122205529885 ) ) ;
#54816 = EDGE_CURVE ( 'NONE', #107758, #67300, #32897, .T. ) ;
#54817 = CARTESIAN_POINT ( 'NONE',  ( 11.80036447210000006, 1433.149496178429899, 150.6216816897980095 ) ) ;
#54818 = CARTESIAN_POINT ( 'NONE',  ( -3.323641320539999722, 1474.972506225130019, 269.6411426393979696 ) ) ;
#54820 = EDGE_CURVE ( 'NONE', #14716, #13288, #89785, .T. ) ;
#54819 = CARTESIAN_POINT ( 'NONE',  ( -9.588314140733929847, 1460.162249162269973, 210.2003709356519892 ) ) ;
#54821 = CARTESIAN_POINT ( 'NONE',  ( -109.5386125330000056, 1385.082371152899896, 297.1260739345589741 ) ) ;
#54822 = CIRCLE ( 'NONE', #6526, 1.999999999999998668 ) ;
#54823 = DIRECTION ( 'NONE',  ( 5.980589973904019347E-17, -1.000000000000000000, 1.736889445713099699E-16 ) ) ;
#54824 = ORIENTED_EDGE ( 'NONE', *, *, #98190, .T. ) ;
#54825 = CARTESIAN_POINT ( 'NONE',  ( -18.19590854888185660, 1512.187213306747481, 180.0410247165186490 ) ) ;
#54826 = B_SPLINE_CURVE_WITH_KNOTS ( 'NONE', 3,
 ( #15219, #75712, #7392, #109858, #30938, #31483 ),
 .UNSPECIFIED., .F., .F.,
 ( 4, 2, 4 ),
 ( 0.000000000000000000, 0.5000000000000000000, 1.000000000000000000 ),
 .UNSPECIFIED. ) ;
#54827 = CARTESIAN_POINT ( 'NONE',  ( 12.37499353609999986, 1442.762691980110048, 206.9242620747189960 ) ) ;
#54828 = CARTESIAN_POINT ( 'NONE',  ( -19.39682342001572835, 1485.601863261859762, 189.9014862107358113 ) ) ;
#54829 = CARTESIAN_POINT ( 'NONE',  ( 8.039070834880659433, 1398.151819186490229, 198.9054696569589566 ) ) ;
#54830 = CARTESIAN_POINT ( 'NONE',  ( 12.44780704128189974, 1501.268281525590055, 211.7240718234590133 ) ) ;
#54831 = CARTESIAN_POINT ( 'NONE',  ( -15.98971164002714573, 1420.239571111833811, 209.6843301561163173 ) ) ;
#54832 = CARTESIAN_POINT ( 'NONE',  ( -13.97249221049999868, 1508.900185047429886, 233.0230284711979891 ) ) ;
#54833 = CARTESIAN_POINT ( 'NONE',  ( -22.35747404037720187, 1383.851046513379970, 221.8738471675100072 ) ) ;
#54834 = CARTESIAN_POINT ( 'NONE',  ( -16.33500296837753041, 1522.051704408389924, 204.2067034917001536 ) ) ;
#54835 = CARTESIAN_POINT ( 'NONE',  ( 6.825986730469999486, 1409.091027440530070, 221.7399762292980085 ) ) ;
#54836 = EDGE_CURVE ( 'NONE', #89045, #52311, #16810, .T. ) ;
#54837 = FACE_OUTER_BOUND ( 'NONE', #57366, .T. ) ;
#54838 = CARTESIAN_POINT ( 'NONE',  ( 1.540611278380000115, 1465.978124834829941, 234.9895109092980192 ) ) ;
#54840 = EDGE_LOOP ( 'NONE', ( #83185, #100075, #41642, #24272 ) ) ;
#54839 = CARTESIAN_POINT ( 'NONE',  ( -9.838665332836511013, 1435.926116633432457, 152.6147087539863776 ) ) ;
#54841 = CARTESIAN_POINT ( 'NONE',  ( -0.6637618131060000204, 1452.913539784329942, 183.3365650660979895 ) ) ;
#54842 = CARTESIAN_POINT ( 'NONE',  ( -10.25244544798204949, 1389.903864462993852, 202.2017625968174741 ) ) ;
#54843 = FACE_OUTER_BOUND ( 'NONE', #12526, .T. ) ;
#54845 = EDGE_LOOP ( 'NONE', ( #101822, #42837, #61427, #54377, #52647 ) ) ;
#54844 = CARTESIAN_POINT ( 'NONE',  ( -18.33918424680000214, 1416.543503932829935, 208.8538484177919656 ) ) ;
#54846 = CARTESIAN_POINT ( 'NONE',  ( -17.51439927794370277, 1442.104016966609834, 219.2287862311399920 ) ) ;
#54847 = ORIENTED_EDGE ( 'NONE', *, *, #28303, .T. ) ;
#54848 = EDGE_CURVE ( 'NONE', #39742, #89980, #98984, .T. ) ;
#54849 = CARTESIAN_POINT ( 'NONE',  ( -11.78173983558050075, 1389.131401572190043, 215.6488607812810017 ) ) ;
#54850 = CARTESIAN_POINT ( 'NONE',  ( 12.26979804483799974, 1416.828039243390094, 223.5793509210460002 ) ) ;
#54851 = CARTESIAN_POINT ( 'NONE',  ( 11.87563351815570023, 1433.006677199550040, 147.6591432317509884 ) ) ;
#54852 = EDGE_CURVE ( 'NONE', #91726, #70768, #46239, .T. ) ;
#54853 = CARTESIAN_POINT ( 'NONE',  ( -5.883891048220000641, 1463.750324872290093, 200.7608182267589996 ) ) ;
#54854 = CARTESIAN_POINT ( 'NONE',  ( -2.777734314609999977, 1432.637008328589900, 217.4880619237290205 ) ) ;
#54855 = FACE_OUTER_BOUND ( 'NONE', #46833, .T. ) ;
#54856 = CARTESIAN_POINT ( 'NONE',  ( 14.14831249788200118, 1409.407130346769918, 204.3310347178599784 ) ) ;
#54857 = CARTESIAN_POINT ( 'NONE',  ( 5.225857906580000822, 1452.691914677890054, 212.7582739490889878 ) ) ;
#54858 = CARTESIAN_POINT ( 'NONE',  ( -107.6301326754700085, 1385.239087081850130, 297.0876625113839395 ) ) ;
#54859 = CARTESIAN_POINT ( 'NONE',  ( -17.99328812619999951, 1452.004064770530022, 190.5764782675980200 ) ) ;
#54860 = CARTESIAN_POINT ( 'NONE',  ( 11.86607075090000052, 1432.333944803479881, 149.9824168323980018 ) ) ;
#54861 = AXIS2_PLACEMENT_3D ( 'NONE', #70692, #1817, #45479 ) ;
#54862 = CARTESIAN_POINT ( 'NONE',  ( 12.09532526841919875, 1491.441359186789896, 206.9399676582060010 ) ) ;
#54863 = ORIENTED_EDGE ( 'NONE', *, *, #20930, .F. ) ;
#54864 = EDGE_LOOP ( 'NONE', ( #29481, #28021, #32702, #38194 ) ) ;
#54865 = CARTESIAN_POINT ( 'NONE',  ( -109.1656546792999904, 1384.956445601399992, 297.1328575267269798 ) ) ;
#54866 = CARTESIAN_POINT ( 'NONE',  ( -12.03450403503200050, 1415.834070663139983, 194.8936510722510036 ) ) ;
#54867 = CARTESIAN_POINT ( 'NONE',  ( -2.900738715952500435, 1495.748930167899971, 197.1341948204009782 ) ) ;
#54868 = CARTESIAN_POINT ( 'NONE',  ( 28.15443155984639745, 1509.896245780209938, 217.4026704617729990 ) ) ;
#54869 = CARTESIAN_POINT ( 'NONE',  ( -29.99620953741478502, 1526.382868172863937, 219.7462484079463252 ) ) ;
#54870 = CARTESIAN_POINT ( 'NONE',  ( 10.79382269979189957, 1414.913060387349788, 222.1041130917409987 ) ) ;
#54871 = CARTESIAN_POINT ( 'NONE',  ( 31.31962989724480551, 1525.556089352344543, 201.5436831772797746 ) ) ;
#54872 = CARTESIAN_POINT ( 'NONE',  ( -0.8893320598190000981, 1471.149508548330232, 182.5957142173980117 ) ) ;
#54873 = CARTESIAN_POINT ( 'NONE',  ( -10.90152747735140615, 1365.778415155553830, 207.6218459616987673 ) ) ;
#54874 = DIRECTION ( 'NONE',  ( 0.9900965937346510870, 0.1403878024439500494, 3.790652827686684978E-16 ) ) ;
#54875 = CARTESIAN_POINT ( 'NONE',  ( 1.575457917789999884, 1508.276376928829905, 237.0209898277979903 ) ) ;
#54876 = CARTESIAN_POINT ( 'NONE',  ( -2.494758036134999912, 1516.937508036699910, 207.4208181092269854 ) ) ;
#54877 = CARTESIAN_POINT ( 'NONE',  ( -2.485517042439642221, 1524.599984580802357, 175.7312637537736748 ) ) ;
#54878 = CARTESIAN_POINT ( 'NONE',  ( 30.68434753602730680, 1526.000688113718297, 201.3936004808388702 ) ) ;
#54879 = LINE ( 'NONE', #79523, #17566 ) ;
#54880 = CARTESIAN_POINT ( 'NONE',  ( 0.8568566378070020528, 1497.755226128189861, 197.7133750264989942 ) ) ;
#54881 = CARTESIAN_POINT ( 'NONE',  ( -9.199712988752910547, 1490.512384490800059, 190.1963207482600069 ) ) ;
#54882 = CARTESIAN_POINT ( 'NONE',  ( -108.7852627620000021, 1383.811234508949838, 297.2705451043590301 ) ) ;
#54883 = ORIENTED_EDGE ( 'NONE', *, *, #11153, .T. ) ;
#54884 = CARTESIAN_POINT ( 'NONE',  ( 5.805165734619999185, 1411.425360653129928, 255.2684105968979793 ) ) ;
#54885 = CARTESIAN_POINT ( 'NONE',  ( -20.38375079739999762, 1488.682100829629917, 192.7189053174979847 ) ) ;
#54887 = CARTESIAN_POINT ( 'NONE',  ( -17.99954561119999852, 1410.904693908129957, 195.2564680766979848 ) ) ;
#54886 = CARTESIAN_POINT ( 'NONE',  ( -10.94414388512420011, 1426.072984913399978, 95.13475895991039977 ) ) ;
#54888 = CARTESIAN_POINT ( 'NONE',  ( 20.66004299446625936, 1506.560172253944756, 201.3057618805298432 ) ) ;
#54889 = CARTESIAN_POINT ( 'NONE',  ( -16.98088666479999986, 1414.156373614329823, 255.1564980982979876 ) ) ;
#54890 = CARTESIAN_POINT ( 'NONE',  ( 20.21586999686489960, 1509.657102485760106, 230.8999660037090109 ) ) ;
#54891 = DIRECTION ( 'NONE',  ( 0.9858563016923833633, 0.000000000000000000, 0.1675928173085483863 ) ) ;
#54892 = CARTESIAN_POINT ( 'NONE',  ( 31.77002021779999552, 1450.515383802559882, 136.3085377226980199 ) ) ;
#54893 = EDGE_LOOP ( 'NONE', ( #69096, #27917, #17284, #102576 ) ) ;
#54894 = CARTESIAN_POINT ( 'NONE',  ( -1.510341393340000337E-11, 1395.913060387330006, 198.1220674062979867 ) ) ;
#54895 = CARTESIAN_POINT ( 'NONE',  ( 12.83556472445637731, 1513.363094763115669, 225.9021281388779698 ) ) ;
#54896 = DIRECTION ( 'NONE',  ( -5.980589973904019347E-17, 1.000000000000000000, -1.736889445713099699E-16 ) ) ;
#54897 = VERTEX_POINT ( 'NONE', #4407 ) ;
#54898 = EDGE_LOOP ( 'NONE', ( #61526, #70232, #91360, #27450, #104949, #50875, #72555, #1342 ) ) ;
#54899 = CARTESIAN_POINT ( 'NONE',  ( 10.10398322925309955, 1452.602376352069996, 209.9919527220669977 ) ) ;
#54900 = CARTESIAN_POINT ( 'NONE',  ( -22.92254907261380126, 1409.723441571369904, 208.9286969261789864 ) ) ;
#54901 = EDGE_CURVE ( 'NONE', #14236, #19394, #40838, .T. ) ;
#54902 = VERTEX_POINT ( 'NONE', #51918 ) ;
#54903 = CARTESIAN_POINT ( 'NONE',  ( 0.1075107530840000020, 1413.831150726530041, 184.8303454653980111 ) ) ;
#54904 = CIRCLE ( 'NONE', #56737, 29.84605316675209608 ) ;
#54905 = CARTESIAN_POINT ( 'NONE',  ( 13.86092937120069912, 1410.765486813650114, 191.1266627561969926 ) ) ;
#54906 = EDGE_CURVE ( 'NONE', #33283, #77824, #71641, .T. ) ;
#54907 = CARTESIAN_POINT ( 'NONE',  ( 0.3093786527580000278, 1452.335660944029769, 183.2932519483980229 ) ) ;
#54908 = CARTESIAN_POINT ( 'NONE',  ( -0.5380077850789999339, 1489.065930492329926, 236.5124582711980281 ) ) ;
#54909 = FACE_OUTER_BOUND ( 'NONE', #77529, .T. ) ;
#54910 = EDGE_LOOP ( 'NONE', ( #88712, #60714, #7718, #63279, #72934, #85047 ) ) ;
#54911 = CARTESIAN_POINT ( 'NONE',  ( -12.61115941400189833, 1416.521607925270018, 222.0431940980950003 ) ) ;
#54912 = CARTESIAN_POINT ( 'NONE',  ( 13.58657643929999992, 1452.821170783829984, 224.5924275984980056 ) ) ;
#54913 = EDGE_LOOP ( 'NONE', ( #37169, #51743, #15000, #67257, #100867, #86848, #29073, #22159, #4642 ) ) ;
#54914 = CARTESIAN_POINT ( 'NONE',  ( 2.480187016714999970, 1517.025470194390209, 204.4964864072570094 ) ) ;
#54915 = EDGE_LOOP ( 'NONE', ( #83275, #31943, #100305, #46287 ) ) ;
#54916 = CARTESIAN_POINT ( 'NONE',  ( 11.85313628462840008, 1431.434643513689934, 149.9078370975529708 ) ) ;
#54917 = EDGE_CURVE ( 'NONE', #52548, #32037, #27208, .T. ) ;
#54918 = CARTESIAN_POINT ( 'NONE',  ( 5.385523159618170297, 1511.435001054559962, 217.7746220610370074 ) ) ;
#54919 = ORIENTED_EDGE ( 'NONE', *, *, #120, .T. ) ;
#54920 = ORIENTED_EDGE ( 'NONE', *, *, #25479, .T. ) ;
#54921 = CARTESIAN_POINT ( 'NONE',  ( 2.792392588003544507, 1524.382868172863937, 176.8996806668726549 ) ) ;
#54922 = CARTESIAN_POINT ( 'NONE',  ( 4.483791294666029437, 1499.492573966179862, 198.5611395500710046 ) ) ;
#54923 = CIRCLE ( 'NONE', #35237, 6.842541678089994583 ) ;
#54924 = CARTESIAN_POINT ( 'NONE',  ( -3.295469101731109962, 1470.146704297040060, 218.7056315512149922 ) ) ;
#54925 = CARTESIAN_POINT ( 'NONE',  ( 11.95631296123499965, 1516.551704408390151, 202.1152804391970221 ) ) ;
#54926 = CARTESIAN_POINT ( 'NONE',  ( -1.646540591608269732E-05, 1410.389848909979946, 269.3346290179499647 ) ) ;
#54927 = CARTESIAN_POINT ( 'NONE',  ( -3.394303741754500336, 1476.460482402099842, 220.0906546599869955 ) ) ;
#54928 = CARTESIAN_POINT ( 'NONE',  ( 11.09516193571039011, 1433.859332616970960, 151.6914986173777038 ) ) ;
#54929 = CARTESIAN_POINT ( 'NONE',  ( -11.31243770530000070, 1433.012837821759831, 151.5204583838979886 ) ) ;
#54930 = CARTESIAN_POINT ( 'NONE',  ( 0.02437641270083376263, 1409.059024698960911, 232.4096207990013454 ) ) ;
#54932 = CARTESIAN_POINT ( 'NONE',  ( -107.0144454107080065, 1391.913060387289988, 307.4418187106899722 ) ) ;
#54931 = CARTESIAN_POINT ( 'NONE',  ( -20.32281514509999809, 1505.121794388689977, 209.3836844847139957 ) ) ;
#54933 = CARTESIAN_POINT ( 'NONE',  ( -68.39881485713311804, 1379.747709036739025, 279.9507912017972444 ) ) ;
#54934 =( REPRESENTATION_RELATIONSHIP ('NONE','NONE', #14372, #110199 ) REPRESENTATION_RELATIONSHIP_WITH_TRANSFORMATION ( #93551 )SHAPE_REPRESENTATION_RELATIONSHIP( ) );
#54935 = CARTESIAN_POINT ( 'NONE',  ( -24.38326756241049864, 1509.011140872309852, 222.4884894987410178 ) ) ;
#54936 = CARTESIAN_POINT ( 'NONE',  ( -6.329634402605000432, 1512.038636172069801, 200.9147609774469743 ) ) ;
#54937 = ORIENTED_EDGE ( 'NONE', *, *, #78331, .F. ) ;
#54938 = CARTESIAN_POINT ( 'NONE',  ( 26.42714720800000094, 1440.913060387330006, 243.9198229517980110 ) ) ;
#54939 = LINE ( 'NONE', #28061, #42607 ) ;
#54940 = AXIS2_PLACEMENT_3D ( 'NONE', #83879, #7183, #51387 ) ;
#54941 = CARTESIAN_POINT ( 'NONE',  ( -84.45939852480390186, 1384.982670101519943, 306.4352233390739570 ) ) ;
#54942 = DIRECTION ( 'NONE',  ( 0.8775825618903703162, 0.000000000000000000, 0.4794255386042073908 ) ) ;
#54943 = EDGE_CURVE ( 'NONE', #110516, #95904, #34676, .T. ) ;
#54944 = CARTESIAN_POINT ( 'NONE',  ( -8.491041205600000197, 1384.938468836829998, 199.8127951144290080 ) ) ;
#54945 = CARTESIAN_POINT ( 'NONE',  ( 44.92382426869910006, 1440.913067149190056, 269.6913831903979712 ) ) ;
#54947 = ORIENTED_EDGE ( 'NONE', *, *, #31676, .F. ) ;
#54946 = CARTESIAN_POINT ( 'NONE',  ( -113.4000000000000057, 1378.913060387289988, 304.2218459572590064 ) ) ;
#54948 = B_SPLINE_CURVE_WITH_KNOTS ( 'NONE', 5,
 ( #65074, #38201, #38745, #73478, #11370, #88630, #105419, #63448, #106513, #63990, #2986, #13529 ),
 .UNSPECIFIED., .F., .F.,
 ( 6, 3, 3, 6 ),
 ( 0.000000000000000000, 0.2983296735331202876, 0.5998977736818913442, 1.000000000000000000 ),
 .UNSPECIFIED. ) ;
#54949 = EDGE_CURVE ( 'NONE', #43414, #41410, #107614, .T. ) ;
#54950 = CARTESIAN_POINT ( 'NONE',  ( 12.89505231660000106, 1420.989630775359956, 203.4267439564690108 ) ) ;
#54951 = CARTESIAN_POINT ( 'NONE',  ( -2.500000000000000000, 1439.114301494319989, 157.7261950941980331 ) ) ;
#54952 = CARTESIAN_POINT ( 'NONE',  ( -76.99707197885180676, 1524.382868172863937, 19.35599459046246551 ) ) ;
#54953 = CARTESIAN_POINT ( 'NONE',  ( -0.3384141495062999994, 1430.231679807619912, 199.7147382543149945 ) ) ;
#54954 = CARTESIAN_POINT ( 'NONE',  ( 17.99954443082109989, 1410.904693892220166, 222.9872220945560173 ) ) ;
#54955 = CARTESIAN_POINT ( 'NONE',  ( 5.360207926212690488, 1422.242713656610022, 144.1549664376839814 ) ) ;
#54956 = CARTESIAN_POINT ( 'NONE',  ( 29.96266749478790103, 1509.959379792560185, 213.6203565918929996 ) ) ;
#54957 = DIRECTION ( 'NONE',  ( 1.755985294532469921E-16, -1.000000000000000000, 1.338183447452831989E-16 ) ) ;
#54958 = CARTESIAN_POINT ( 'NONE',  ( 12.89607781515299934, 1434.724834403989917, 149.2206011272099886 ) ) ;
#54959 = CARTESIAN_POINT ( 'NONE',  ( 11.75640697505575538, 1511.791180387471059, 224.3022927925875365 ) ) ;
#54960 = EDGE_CURVE ( 'NONE', #28184, #91418, #106293, .T. ) ;
#54961 = CARTESIAN_POINT ( 'NONE',  ( -3.523962691040000372, 1476.511731505490161, 220.0526012038990018 ) ) ;
#54962 = CARTESIAN_POINT ( 'NONE',  ( -20.98221433428902927, 1524.841055067849538, 237.1519650095371503 ) ) ;
#54963 = CARTESIAN_POINT ( 'NONE',  ( -0.7579844201469989606, 1516.883361325900069, 206.8353730456769881 ) ) ;
#54964 = CARTESIAN_POINT ( 'NONE',  ( 45.86410423099999889, 1436.891480617990283, 266.6830272419979906 ) ) ;
#54965 = CARTESIAN_POINT ( 'NONE',  ( -16.97531057559999823, 1409.505851295029970, 223.7086794493979767 ) ) ;
#54966 = AXIS2_PLACEMENT_3D ( 'NONE', #9875, #18259, #43495 ) ;
#54967 = CARTESIAN_POINT ( 'NONE',  ( 23.38999613540000055, 1436.126019947570057, 140.8856778375979957 ) ) ;
#54968 = CARTESIAN_POINT ( 'NONE',  ( 20.84753735790000206, 1488.585408351930027, 191.8019074006979849 ) ) ;
#54969 = EDGE_CURVE ( 'NONE', #48513, #20620, #89709, .T. ) ;
#54970 = CARTESIAN_POINT ( 'NONE',  ( 5.361102066162420243, 1423.469345717320039, 149.3894558389860094 ) ) ;
#54971 = CARTESIAN_POINT ( 'NONE',  ( -3.427369262309999609, 1475.739996263529974, 266.9564229772980752 ) ) ;
#54972 = CARTESIAN_POINT ( 'NONE',  ( -14.41990770658309984, 1417.158242887760025, 203.2539387402569844 ) ) ;
#54973 =( BOUNDED_CURVE ( )  B_SPLINE_CURVE ( 3, ( #104818, #19129, #103711, #95316 ),
 .UNSPECIFIED., .F., .F. ) 
 B_SPLINE_CURVE_WITH_KNOTS ( ( 4, 4 ),
 ( 3.141592653589793116, 4.712388980384695891 ),
 .UNSPECIFIED. ) 
 CURVE ( )  GEOMETRIC_REPRESENTATION_ITEM ( )  RATIONAL_B_SPLINE_CURVE ( ( 1.000000000000000000, 0.8047378541243634942, 0.8047378541243634942, 1.000000000000000000 ) ) 
 REPRESENTATION_ITEM ( '' )  );
#54974 = CARTESIAN_POINT ( 'NONE',  ( -33.92723761326109866, 1436.576419602210080, 136.5094945797809771 ) ) ;
#54975 = CARTESIAN_POINT ( 'NONE',  ( 0.2171626012915229831, 1453.344709657829981, 183.2386049330829962 ) ) ;
#54976 = CARTESIAN_POINT ( 'NONE',  ( -11.20005611260000045, 1409.304174965030143, 199.4475870259680050 ) ) ;
#54977 = CARTESIAN_POINT ( 'NONE',  ( 9.237335364602959231, 1428.214395631979869, 212.7147833259940057 ) ) ;
#54978 = CARTESIAN_POINT ( 'NONE',  ( -4.226426710960000221, 1515.477082012290111, 208.7508649547930020 ) ) ;
#54979 = CARTESIAN_POINT ( 'NONE',  ( -7.734417504676620148, 1383.405642709869880, 218.8913851597439759 ) ) ;
#54980 = CARTESIAN_POINT ( 'NONE',  ( 11.87973522909999957, 1433.311075274859832, 146.9202984917980359 ) ) ;
#54981 = CARTESIAN_POINT ( 'NONE',  ( -37.09403179692020558, 1436.457961865149855, 134.0999999968530005 ) ) ;
#54982 = CARTESIAN_POINT ( 'NONE',  ( 3.920880449199999784, 1439.701871945560015, 184.6839062468980046 ) ) ;
#54983 = ORIENTED_EDGE ( 'NONE', *, *, #23454, .T. ) ;
#54984 = CARTESIAN_POINT ( 'NONE',  ( 3.265660027580000069, 1477.001235074189935, 198.7922852500990132 ) ) ;
#54985 = CARTESIAN_POINT ( 'NONE',  ( -9.578270037681749116, 1409.247540947460038, 220.6126654330650183 ) ) ;
#54986 = CARTESIAN_POINT ( 'NONE',  ( 32.78250617288038171, 1511.187213306747708, 199.9357095655690841 ) ) ;
#54987 = ADVANCED_FACE ( 'NONE', ( #68189 ), #59359, .T. ) ;
#54988 = CARTESIAN_POINT ( 'NONE',  ( 17.72039215071724172, 1432.779376552643726, 213.8336839905872750 ) ) ;
#54989 = CARTESIAN_POINT ( 'NONE',  ( -12.78776258895079998, 1416.851343896850040, 195.5391574246120001 ) ) ;
#54990 = VECTOR ( 'NONE', #61052, 1000.000000000000000 ) ;
#54991 = CARTESIAN_POINT ( 'NONE',  ( -26.68774699959999808, 1468.726062758129956, 269.4193446826980107 ) ) ;
#54992 = CARTESIAN_POINT ( 'NONE',  ( -11.81191611200530112, 1481.532780713840111, 210.1673330252230016 ) ) ;
#54993 = CARTESIAN_POINT ( 'NONE',  ( -19.71128566253871384, 1498.214606263945370, 189.2503765500455586 ) ) ;
#54994 = ADVANCED_FACE ( 'NONE', ( #34549 ), #48647, .T. ) ;
#54995 = CARTESIAN_POINT ( 'NONE',  ( -27.59998769030000076, 1509.654128774529909, 212.1034408311279833 ) ) ;
#54996 = CARTESIAN_POINT ( 'NONE',  ( -91.63069530043399880, 1384.616216363609965, 309.2058898380819869 ) ) ;
#54997 = CARTESIAN_POINT ( 'NONE',  ( -40.96489448099129760, 1384.992258638779958, 213.8259286978779983 ) ) ;
#54998 = CARTESIAN_POINT ( 'NONE',  ( -12.04329576969499982, 1491.114171671750000, 206.7787137245340148 ) ) ;
#54999 = CARTESIAN_POINT ( 'NONE',  ( -3.605016531877470065, 1508.551704408389924, 204.3978405181830169 ) ) ;
#55000 = CARTESIAN_POINT ( 'NONE',  ( 14.63637096480000110, 1474.175152404529854, 223.6336467093979934 ) ) ;
#55001 = CARTESIAN_POINT ( 'NONE',  ( 17.74609922954199703, 1415.424669706240138, 224.3250650115680003 ) ) ;
#55003 = EDGE_LOOP ( 'NONE', ( #57532, #12221, #14275, #81119 ) ) ;
#55002 = DIRECTION ( 'NONE',  ( 0.9085883915379301401, 0.3022389680066620010, -0.2883032101465139996 ) ) ;
#55004 = CARTESIAN_POINT ( 'NONE',  ( 20.15452300067990166, 1507.845791525220193, 189.3412703910400126 ) ) ;
#55005 = CARTESIAN_POINT ( 'NONE',  ( 1.448755922665179829, 1499.001568892050045, 236.4189104725390109 ) ) ;
#55006 = CARTESIAN_POINT ( 'NONE',  ( 3.126158272763291279, 1370.057571174347913, 210.3709297514385810 ) ) ;
#55007 = CARTESIAN_POINT ( 'NONE',  ( -12.72284891840000043, 1416.311719779230089, 195.5584137648980061 ) ) ;
#55008 = DIRECTION ( 'NONE',  ( -0.1976597336227498836, -0.9325250109992564429, -0.3022047874621121566 ) ) ;
#55009 = CARTESIAN_POINT ( 'NONE',  ( 22.57032379820000045, 1409.701233462030132, 209.8663284536589799 ) ) ;
#55010 = CARTESIAN_POINT ( 'NONE',  ( -12.78614179230000047, 1434.663150159289899, 149.2928482040979929 ) ) ;
#55011 = CARTESIAN_POINT ( 'NONE',  ( -13.05160664115349789, 1467.538620789039896, 191.8992768326569660 ) ) ;
#55012 = CARTESIAN_POINT ( 'NONE',  ( -5.360091096029239388, 1422.252256049249809, 144.8358257923730150 ) ) ;
#55014 = CARTESIAN_POINT ( 'NONE',  ( -11.60666322014453655, 1426.782727568212294, 134.8522042001498278 ) ) ;
#55013 = CARTESIAN_POINT ( 'NONE',  ( -1.600048698852036821, 1401.254281879943164, 134.0999999980979851 ) ) ;
#55015 = CARTESIAN_POINT ( 'NONE',  ( 24.99661049207140096, 1430.498659694909747, 209.1806683305300112 ) ) ;
#55016 = CARTESIAN_POINT ( 'NONE',  ( -101.5731991332999513, 1376.302340817389677, 307.2417240775760092 ) ) ;
#55017 = DIRECTION ( 'NONE',  ( 9.500914144214121536E-47, -1.000000000000000000, 1.836970198721029688E-16 ) ) ;
#55018 = CARTESIAN_POINT ( 'NONE',  ( -113.4000000000000057, 1302.413060387289988, 304.2218459572590064 ) ) ;
#55019 = AXIS2_PLACEMENT_3D ( 'NONE', #83163, #65277, #23239 ) ;
#55020 = CARTESIAN_POINT ( 'NONE',  ( -5.013263847643504967, 1375.354125225655480, 203.5257469810366899 ) ) ;
#55021 = CARTESIAN_POINT ( 'NONE',  ( -6.946748557085000719, 1516.983995446890049, 204.1186252050270014 ) ) ;
#55022 = CARTESIAN_POINT ( 'NONE',  ( -23.42260982742433129, 1434.595599714059972, 214.6024343348293826 ) ) ;
#55023 = CARTESIAN_POINT ( 'NONE',  ( -16.31598018130440053, 1485.656693110169954, 187.6240192544399861 ) ) ;
#55024 = CARTESIAN_POINT ( 'NONE',  ( -9.227567128520000495, 1423.503386125029920, 208.4707392769450109 ) ) ;
#55025 = CARTESIAN_POINT ( 'NONE',  ( -4.263963421918809615, 1441.192140480630087, 158.8199918691270227 ) ) ;
#55027 = VERTEX_POINT ( 'NONE', #49717 ) ;
#55026 = CARTESIAN_POINT ( 'NONE',  ( -68.17361118975399847, 1379.746536065940063, 279.6965955867630100 ) ) ;
#55028 = ORIENTED_EDGE ( 'NONE', *, *, #38039, .F. ) ;
#55029 = CARTESIAN_POINT ( 'NONE',  ( 29.63837385289999915, 1509.975889318429836, 210.7975540006979998 ) ) ;
#55030 = ORIENTED_EDGE ( 'NONE', *, *, #41387, .F. ) ;
#55031 = CARTESIAN_POINT ( 'NONE',  ( 0.2129864158460960111, 1450.905623043510104, 126.7681030205719850 ) ) ;
#55032 = CARTESIAN_POINT ( 'NONE',  ( 1.471222536514999790, 1414.913526854310021, 192.0236705776529789 ) ) ;
#55034 = DIRECTION ( 'NONE',  ( 0.000000000000000000, 1.000000000000000000, 0.000000000000000000 ) ) ;
#55033 = CARTESIAN_POINT ( 'NONE',  ( 2.286265947080000416, 1427.727383903629971, 112.4493539157979995 ) ) ;
#55035 = DIRECTION ( 'NONE',  ( 0.9455185755993178454, 0.000000000000000000, -0.3255681544571537578 ) ) ;
#55036 = B_SPLINE_CURVE_WITH_KNOTS ( 'NONE', 5,
 ( #57200, #72346, #63411, #98615, #47678, #38165 ),
 .UNSPECIFIED., .F., .F.,
 ( 6, 6 ),
 ( 0.000000000000000000, 0.9643540072699122723 ),
 .UNSPECIFIED. ) ;
#55037 = CARTESIAN_POINT ( 'NONE',  ( -25.17722015988540107, 1451.311918859900061, 137.3180140832189693 ) ) ;
#55038 = CARTESIAN_POINT ( 'NONE',  ( 10.52994085932536272, 1438.877686223792125, 152.6194632825565236 ) ) ;
#55039 = CARTESIAN_POINT ( 'NONE',  ( 11.03217570710000039, 1409.298312452229993, 227.8647431501979952 ) ) ;
#55040 = CARTESIAN_POINT ( 'NONE',  ( 12.56049338238149815, 1501.076573751879778, 211.0976562363760252 ) ) ;
#55041 = PRESENTATION_STYLE_ASSIGNMENT (( #97033 ) ) ;
#55042 = CARTESIAN_POINT ( 'NONE',  ( 41.37151551531449911, 1441.555306590669943, 134.0999999980749919 ) ) ;
#55043 = CARTESIAN_POINT ( 'NONE',  ( 3.823234350589999941, 1434.969202599190112, 204.8006882687589894 ) ) ;
#55044 = EDGE_LOOP ( 'NONE', ( #11002, #44807, #26909, #108040, #108029 ) ) ;
#55045 = CARTESIAN_POINT ( 'NONE',  ( 8.129477481277049833, 1461.711625216570155, 228.8738004967299844 ) ) ;
#55046 = CARTESIAN_POINT ( 'NONE',  ( 6.485530625610728350, 1492.746195377240610, 218.1903392014115468 ) ) ;
#55047 = ORIENTED_EDGE ( 'NONE', *, *, #59635, .T. ) ;
#55048 = ORIENTED_EDGE ( 'NONE', *, *, #21584, .T. ) ;
#55049 = ORIENTED_EDGE ( 'NONE', *, *, #88350, .T. ) ;
#55050 = CARTESIAN_POINT ( 'NONE',  ( -6.852741844795000148, 1514.298059036119867, 217.0646729429169852 ) ) ;
#55051 = CARTESIAN_POINT ( 'NONE',  ( 16.78503325280423297, 1513.553906385955088, 195.8943387144314840 ) ) ;
#55052 = EDGE_CURVE ( 'NONE', #35056, #58564, #67642, .T. ) ;
#55053 = CARTESIAN_POINT ( 'NONE',  ( 15.12819912197481997, 1451.147586662198137, 149.6391027733497765 ) ) ;
#55054 = AXIS2_PLACEMENT_3D ( 'NONE', #69279, #52476, #86604 ) ;
#55055 = DIRECTION ( 'NONE',  ( 9.230617842401318720E-47, -1.000000000000000000, 1.836970198721029688E-16 ) ) ;
#55056 = CARTESIAN_POINT ( 'NONE',  ( -12.31987546760000107, 1378.182896874270000, 209.4394672709660199 ) ) ;
#55057 = CARTESIAN_POINT ( 'NONE',  ( -67.87117022811392530, 1379.746131644044226, 278.1675811678725267 ) ) ;
#55058 = CARTESIAN_POINT ( 'NONE',  ( -1.551174237339999928, 1463.265707418689999, 199.4651013571389910 ) ) ;
#55059 = CARTESIAN_POINT ( 'NONE',  ( -2.229731647334999955, 1512.142919181319940, 201.5278066827870020 ) ) ;
#55060 = CARTESIAN_POINT ( 'NONE',  ( 8.469420064130000370, 1416.216252248729916, 193.1369149110980175 ) ) ;
#55061 = CARTESIAN_POINT ( 'NONE',  ( -59.16060917409809861, 1384.667876448820152, 242.2189909261509797 ) ) ;
#55062 = ORIENTED_EDGE ( 'NONE', *, *, #4288, .F. ) ;
#55063 = CARTESIAN_POINT ( 'NONE',  ( -2.881548462575000080, 1516.909589401870107, 206.8382752989369919 ) ) ;
#55064 = VERTEX_POINT ( 'NONE', #16609 ) ;
#55065 = CARTESIAN_POINT ( 'NONE',  ( 27.48763482353140120, 1440.913060387330006, 246.3050835912150092 ) ) ;
#55066 = EDGE_CURVE ( 'NONE', #96612, #83385, #64143, .T. ) ;
#55067 = CARTESIAN_POINT ( 'NONE',  ( 11.57490036778929898, 1478.937116359260017, 207.0860133150080173 ) ) ;
#55068 = ORIENTED_EDGE ( 'NONE', *, *, #94509, .T. ) ;
#55069 = FACE_OUTER_BOUND ( 'NONE', #36849, .T. ) ;
#55070 = CARTESIAN_POINT ( 'NONE',  ( 7.518776976417130165, 1428.948321996720097, 214.9051160645190066 ) ) ;
#55071 = CARTESIAN_POINT ( 'NONE',  ( -22.53878221424140094, 1411.058442688259902, 212.0450776560099939 ) ) ;
#55073 = DIRECTION ( 'NONE',  ( -0.7074300732343287157, -0.02470400251501369063, -0.7063514732365258064 ) ) ;
#55072 = CARTESIAN_POINT ( 'NONE',  ( -24.90627924569999863, 1441.326908584029979, 210.4393126625480193 ) ) ;
#55074 = CARTESIAN_POINT ( 'NONE',  ( -7.691664047984310137, 1435.994123091719985, 215.1214903504479992 ) ) ;
#55075 = EDGE_CURVE ( 'NONE', #967, #42994, #72998, .T. ) ;
#55076 = CARTESIAN_POINT ( 'NONE',  ( 13.19226977985399962, 1436.077122747240082, 150.6574760380860312 ) ) ;
#55077 = CARTESIAN_POINT ( 'NONE',  ( -2.178197975999999869, 1509.061250285029928, 179.3703848074979987 ) ) ;
#55078 = CARTESIAN_POINT ( 'NONE',  ( 16.87207549522816308, 1516.551188142743058, 222.4161009436613483 ) ) ;
#55079 = CARTESIAN_POINT ( 'NONE',  ( -13.99196149959999858, 1471.299568757930047, 192.9718935549979903 ) ) ;
#55081 = CARTESIAN_POINT ( 'NONE',  ( -103.5806803890000083, 1389.940350142260058, 304.1776731731589507 ) ) ;
#55080 = CARTESIAN_POINT ( 'NONE',  ( 7.920313882610000356, 1463.549343347430067, 235.1949569295980211 ) ) ;
#55082 = VECTOR ( 'NONE', #69332, 1000.000000000000000 ) ;
#55083 = CARTESIAN_POINT ( 'NONE',  ( 5.005071008295000290, 1516.710692850270107, 216.4473877573669824 ) ) ;
#55084 = CARTESIAN_POINT ( 'NONE',  ( 7.717505752974999744, 1516.857914730730045, 201.4043401791270185 ) ) ;
#55085 = CARTESIAN_POINT ( 'NONE',  ( 0.1681681984989999989, 1405.973120458229914, 121.6099336315979969 ) ) ;
#55086 = CARTESIAN_POINT ( 'NONE',  ( 31.18494820112223209, 1524.152444737676660, 221.8763663153084167 ) ) ;
#55087 = CARTESIAN_POINT ( 'NONE',  ( 2.880592928985000079, 1516.859514182039902, 211.9868180862470126 ) ) ;
#55088 = CARTESIAN_POINT ( 'NONE',  ( -22.18308977499999912, 1506.802866779929900, 208.9507517862349744 ) ) ;
#55089 = CARTESIAN_POINT ( 'NONE',  ( 11.39861885689485277, 1453.593877275467094, 193.2142631562276449 ) ) ;
#55091 = ORIENTED_EDGE ( 'NONE', *, *, #8283, .T. ) ;
#55090 = CARTESIAN_POINT ( 'NONE',  ( -109.9987472819999965, 1388.002180556429948, 310.4334137642590008 ) ) ;
#55092 = CARTESIAN_POINT ( 'NONE',  ( -0.6414547015529999952, 1416.067629290630066, 227.6224876852980117 ) ) ;
#55093 = CARTESIAN_POINT ( 'NONE',  ( 27.85865497370000199, 1444.561642193520129, 231.9580019065979855 ) ) ;
#55094 = EDGE_CURVE ( 'NONE', #66425, #78889, #110551, .T. ) ;
#55095 = CARTESIAN_POINT ( 'NONE',  ( -10.22679430872973327, 1488.677234487174246, 215.7753183090639766 ) ) ;
#55096 = CARTESIAN_POINT ( 'NONE',  ( -15.70353555820000047, 1415.826269415930028, 208.9425385408250122 ) ) ;
#55097 = CARTESIAN_POINT ( 'NONE',  ( -0.2658002863356170309, 1507.120020817209934, 237.3289691923420150 ) ) ;
#55098 = ADVANCED_FACE ( 'NONE', ( #19386 ), #80314, .F. ) ;
#55099 = CARTESIAN_POINT ( 'NONE',  ( 16.81611548245179222, 1526.382868172864164, 183.6985842798745523 ) ) ;
#55100 = CIRCLE ( 'NONE', #94375, 1237.216328224680410 ) ;
#55101 = EDGE_CURVE ( 'NONE', #46504, #78944, #100914, .T. ) ;
#55103 = CYLINDRICAL_SURFACE ( 'NONE', #76560, 1.000000000000009548 ) ;
#55102 = CARTESIAN_POINT ( 'NONE',  ( -22.49223445950000055, 1444.795317305830167, 218.7498400625879924 ) ) ;
#55104 = CARTESIAN_POINT ( 'NONE',  ( -1.855538017380000015, 1485.200156903630159, 182.6439197069979912 ) ) ;
#55105 = CARTESIAN_POINT ( 'NONE',  ( -106.2761447790000062, 1378.746492803760020, 307.5519750587589556 ) ) ;
#55106 = EDGE_LOOP ( 'NONE', ( #51892, #21241, #99739, #10238 ) ) ;
#55108 = TOROIDAL_SURFACE ( 'NONE', #46393, 1.000000000000000000, 1.000000000000000000 ) ;
#55107 = CARTESIAN_POINT ( 'NONE',  ( 7.710610402995000001, 1516.594591938570147, 205.6677260153969939 ) ) ;
#55109 = CARTESIAN_POINT ( 'NONE',  ( 1.318101111460000086, 1406.519676335630038, 269.4981145789980133 ) ) ;
#55110 = CARTESIAN_POINT ( 'NONE',  ( 1.480872463499999903, 1515.456375364289897, 213.2974053764389737 ) ) ;
#55111 = AXIS2_PLACEMENT_3D ( 'NONE', #27141, #9236, #25999 ) ;
#55112 = EDGE_CURVE ( 'NONE', #23029, #1304, #21854, .T. ) ;
#55113 = AXIS2_PLACEMENT_3D ( 'NONE', #103742, #44405, #97549 ) ;
#55114 = CARTESIAN_POINT ( 'NONE',  ( 42.28244518683229813, 1445.873630544700063, 269.8809842817969411 ) ) ;
#55115 = CARTESIAN_POINT ( 'NONE',  ( -7.649034438594999763, 1514.243099272629934, 203.4721261815869866 ) ) ;
#55116 = CARTESIAN_POINT ( 'NONE',  ( 10.63894069730948466, 1424.089672982063576, 137.5854534913812586 ) ) ;
#55117 = LINE ( 'NONE', #5232, #56785 ) ;
#55118 = CARTESIAN_POINT ( 'NONE',  ( -2.318887826942909847, 1449.808491734400150, 155.3361412615429913 ) ) ;
#55119 = CARTESIAN_POINT ( 'NONE',  ( -40.07811080949989702, 1443.844543801569898, 135.1422523984039969 ) ) ;
#55120 = DIRECTION ( 'NONE',  ( 0.9774101051267759521, 0.000000000000000000, 0.2113515706023137153 ) ) ;
#55121 = CARTESIAN_POINT ( 'NONE',  ( -13.86388155186750026, 1415.301705645010088, 220.7860354755530068 ) ) ;
#55122 = CARTESIAN_POINT ( 'NONE',  ( 20.15452300067990166, 1507.845791525220193, 189.3412703910400126 ) ) ;
#55123 =( BOUNDED_SURFACE ( )  B_SPLINE_SURFACE ( 3, 2, ( 
 ( #67034, #90550, #83260 ),
 ( #82712, #84359, #100600 ),
 ( #40153, #64839, #74877 ),
 ( #109028, #32310, #16032 ),
 ( #22770, #66494, #58076 ),
 ( #92754, #14384, #41261 ) ),
 .UNSPECIFIED., .F., .F., .F. ) 
 B_SPLINE_SURFACE_WITH_KNOTS ( ( 4, 2, 4 ),
 ( 3, 3 ),
 ( -3.252606517456513302E-18, 0.001312027981647327559, 0.002624055963294658154 ),
 ( 0.000000000000000000, 1.000000000000000000 ),
 .UNSPECIFIED. ) 
 GEOMETRIC_REPRESENTATION_ITEM ( )  RATIONAL_B_SPLINE_SURFACE ( (
 ( 1.000000000000000000, 0.9376006582765876729, 1.000000000000000000),
 ( 1.000000000000000000, 0.9569320108031822425, 1.000000000000000000),
 ( 1.000000000000000000, 0.9725743441606675699, 1.000000000000000000),
 ( 1.000000000000000000, 0.9942095667147810012, 1.000000000000000000),
 ( 1.000000000000000000, 1.000043666449794255, 1.000000000000000000),
 ( 1.000000000000000000, 1.000000000000000000, 1.000000000000000000) ) ) 
 REPRESENTATION_ITEM ( '' )  SURFACE ( )  );
#55124 = ORIENTED_EDGE ( 'NONE', *, *, #53706, .T. ) ;
#55125 = CARTESIAN_POINT ( 'NONE',  ( -4.540901344669999951, 1419.211677879630088, 248.0989693021979861 ) ) ;
#55126 = EDGE_CURVE ( 'NONE', #19628, #35056, #78341, .T. ) ;
#55127 = CARTESIAN_POINT ( 'NONE',  ( 9.726769132718798616, 1469.060278453449882, 204.1925708335969887 ) ) ;
#55128 = CARTESIAN_POINT ( 'NONE',  ( -0.3397000419900000345, 1476.049357295929894, 268.4837298515980137 ) ) ;
#55130 = AXIS2_PLACEMENT_3D ( 'NONE', #72081, #106733, #38428 ) ;
#55129 = DIRECTION ( 'NONE',  ( -9.500021872036790217E-47, 1.000000000000000000, -1.836970198721029688E-16 ) ) ;
#55131 = CARTESIAN_POINT ( 'NONE',  ( -8.106555885276549134, 1438.741351455190170, 205.9368832915250209 ) ) ;
#55132 = EDGE_CURVE ( 'NONE', #48130, #64548, #38270, .T. ) ;
#55133 = DIRECTION ( 'NONE',  ( -0.8383970168982890492, -0.5450600352768950607, 0.000000000000000000 ) ) ;
#55134 = CARTESIAN_POINT ( 'NONE',  ( -30.71459829396640018, 1384.825797510230132, 228.8220148752180023 ) ) ;
#55135 = B_SPLINE_CURVE_WITH_KNOTS ( 'NONE', 3,
 ( #11108, #57526, #72134, #89450, #91650, #48005, #21666, #5993, #98939, #31189, #64273, #5442, #22214 ),
 .UNSPECIFIED., .F., .F.,
 ( 4, 2, 2, 1, 2, 2, 4 ),
 ( 0.000000000000000000, 0.2500000000000208722, 0.3750000000000297540, 0.4375000000000330846, 0.4687500000000325850, 0.5000000000000320854, 1.000000000000000000 ),
 .UNSPECIFIED. ) ;
#55136 = B_SPLINE_CURVE_WITH_KNOTS ( 'NONE', 5,
 ( #96981, #61199, #29214, #54988, #20244, #1264, #35965, #70154, #63402 ),
 .UNSPECIFIED., .F., .F.,
 ( 6, 3, 6 ),
 ( 0.000000000000000000, 0.02144875489016424136, 1.000000000000000000 ),
 .UNSPECIFIED. ) ;
#55137 = CARTESIAN_POINT ( 'NONE',  ( -105.0711645279999971, 1379.235653477059941, 303.4121855584589866 ) ) ;
#55138 = CARTESIAN_POINT ( 'NONE',  ( -9.933553457609999526, 1481.595314920090004, 205.4496293638590032 ) ) ;
#55139 = CARTESIAN_POINT ( 'NONE',  ( 8.412796040255942742, 1511.396722025158397, 204.4533818147023965 ) ) ;
#55141 = EDGE_CURVE ( 'NONE', #54528, #83462, #75567, .T. ) ;
#55140 = CARTESIAN_POINT ( 'NONE',  ( -4.104299670009800671, 1396.056385690520074, 219.3587915975870146 ) ) ;
#55142 = CARTESIAN_POINT ( 'NONE',  ( -15.36549427490000141, 1420.414141484729953, 227.0219848979980100 ) ) ;
#55143 = ORIENTED_EDGE ( 'NONE', *, *, #43130, .T. ) ;
#55144 = CARTESIAN_POINT ( 'NONE',  ( -11.35135138259924048, 1503.578306220690820, 207.0399780940998369 ) ) ;
#55145 = CARTESIAN_POINT ( 'NONE',  ( 2.196223613969999988, 1409.923853850330033, 231.8398400339980014 ) ) ;
#55146 = CARTESIAN_POINT ( 'NONE',  ( -10.31340658039999880, 1484.355420805929953, 185.0384118475980131 ) ) ;
#55148 = CARTESIAN_POINT ( 'NONE',  ( -14.64758698596499897, 1513.486273623730085, 193.6399990342670208 ) ) ;
#55147 = CARTESIAN_POINT ( 'NONE',  ( 11.23345602649999897, 1426.040909930530006, 115.7213397327980005 ) ) ;
#55149 = CARTESIAN_POINT ( 'NONE',  ( -0.2658540493943280514, 1507.120020986029886, 237.3289608297170048 ) ) ;
#55150 = FACE_OUTER_BOUND ( 'NONE', #86577, .T. ) ;
#55151 = CIRCLE ( 'NONE', #38958, 2.000000000000003553 ) ;
#55152 = CARTESIAN_POINT ( 'NONE',  ( -4.035490750684999739, 1516.630499592039996, 201.4102952541169884 ) ) ;
#55153 = CARTESIAN_POINT ( 'NONE',  ( 7.708772379780000072, 1427.786886959790081, 212.9376885971290108 ) ) ;
#55154 = CARTESIAN_POINT ( 'NONE',  ( -11.77905477449999871, 1483.168199375790209, 228.2502073304989949 ) ) ;
#55155 = CARTESIAN_POINT ( 'NONE',  ( 7.385876586370000219, 1509.171843810430119, 180.6941627112979916 ) ) ;
#55156 = LINE ( 'NONE', #54062, #11451 ) ;
#55157 = CARTESIAN_POINT ( 'NONE',  ( -77.18529333353220068, 1379.656469662269956, 292.4663616554850023 ) ) ;
#55158 = CARTESIAN_POINT ( 'NONE',  ( 8.653423937804200605, 1367.169888897642068, 210.6218459616987957 ) ) ;
#55160 = ORIENTED_EDGE ( 'NONE', *, *, #7895, .T. ) ;
#55159 = CARTESIAN_POINT ( 'NONE',  ( -19.18445155381639822, 1379.602224620720108, 212.8959267389929835 ) ) ;
#55161 = ORIENTED_EDGE ( 'NONE', *, *, #22928, .T. ) ;
#55162 = CARTESIAN_POINT ( 'NONE',  ( -10.19366155880000058, 1396.792506850929840, 201.2442953279479809 ) ) ;
#55163 = CARTESIAN_POINT ( 'NONE',  ( -15.12918126009999931, 1409.441383038730010, 192.4788841068979934 ) ) ;
#55164 = CARTESIAN_POINT ( 'NONE',  ( -17.78508617079999610, 1435.118679338368793, 145.5186544196980094 ) ) ;
#55165 = CARTESIAN_POINT ( 'NONE',  ( -7.552141952424999971, 1510.542924508009946, 212.9021323590669965 ) ) ;
#55167 = CARTESIAN_POINT ( 'NONE',  ( 17.60565453690000126, 1410.875554451929929, 225.2140679527979898 ) ) ;
#55166 = CARTESIAN_POINT ( 'NONE',  ( -8.856807571699999215, 1384.768264595860046, 218.6834643707789780 ) ) ;
#55168 = CARTESIAN_POINT ( 'NONE',  ( 8.522139242040001506, 1410.293599720429938, 187.8412052867980151 ) ) ;
#55169 = CARTESIAN_POINT ( 'NONE',  ( -1.828126493375330064, 1464.537186451630077, 199.0653043791290031 ) ) ;
#55170 = CARTESIAN_POINT ( 'NONE',  ( -40.20780054482000310, 1448.389597071610069, 135.4753047060349900 ) ) ;
#55171 = CARTESIAN_POINT ( 'NONE',  ( 39.12852302555769768, 1437.672249968900132, 135.5512840573979929 ) ) ;
#55172 = CARTESIAN_POINT ( 'NONE',  ( 4.112383809545077540, 1371.068065305577647, 209.6218459617033432 ) ) ;
#55173 = CARTESIAN_POINT ( 'NONE',  ( -26.96382314767709687, 1437.662753688059865, 136.8825050232889851 ) ) ;
#55174 = CARTESIAN_POINT ( 'NONE',  ( 11.82297588149999967, 1429.270096893229947, 149.5722024081979953 ) ) ;
#55175 = CARTESIAN_POINT ( 'NONE',  ( 41.15075515969999742, 1443.752813495769942, 136.9300362400979907 ) ) ;
#55176 = ORIENTED_EDGE ( 'NONE', *, *, #52178, .F. ) ;
#55177 = DIRECTION ( 'NONE',  ( 0.000000000000000000, 1.000000000000000000, 0.000000000000000000 ) ) ;
#55178 = CARTESIAN_POINT ( 'NONE',  ( 20.68299495989132808, 1525.856064936158418, 233.9549337258506227 ) ) ;
#55179 = ORIENTED_EDGE ( 'NONE', *, *, #76917, .F. ) ;
#55180 = AXIS2_PLACEMENT_3D ( 'NONE', #6307, #57833, #137 ) ;
#55181 = ORIENTED_EDGE ( 'NONE', *, *, #40174, .F. ) ;
#55182 = CARTESIAN_POINT ( 'NONE',  ( -17.26197377869999983, 1420.099051756930066, 204.7291993270589785 ) ) ;
#55183 = CARTESIAN_POINT ( 'NONE',  ( -13.88147930949999953, 1460.663431784329987, 231.8849065275979910 ) ) ;
#55184 = VECTOR ( 'NONE', #41728, 1000.000000000000000 ) ;
#55185 = CARTESIAN_POINT ( 'NONE',  ( 4.038637462725000127, 1516.734985836460055, 214.8955147850770118 ) ) ;
#55186 = CARTESIAN_POINT ( 'NONE',  ( -13.85438721787440031, 1379.977881741410101, 208.5176583983199805 ) ) ;
#55187 = CIRCLE ( 'NONE', #33627, 2.500000000000002220 ) ;
#55188 = ORIENTED_EDGE ( 'NONE', *, *, #30231, .T. ) ;
#55189 = CARTESIAN_POINT ( 'NONE',  ( 0.02955819112566530210, 1522.051704408389924, 193.2356110507530218 ) ) ;
#55190 = CARTESIAN_POINT ( 'NONE',  ( -59.28197579180000076, 1375.203196137529858, 258.5658342392590043 ) ) ;
#55191 = CIRCLE ( 'NONE', #35567, 1.000000000000015099 ) ;
#55192 = CARTESIAN_POINT ( 'NONE',  ( 17.17379625170000423, 1415.087974639930053, 212.6822280708980202 ) ) ;
#55193 = CARTESIAN_POINT ( 'NONE',  ( -6.948321743994999800, 1517.049325831759916, 205.0875650164470017 ) ) ;
#55194 = CARTESIAN_POINT ( 'NONE',  ( 11.01187563919999945, 1492.459055989690114, 212.4069243732789971 ) ) ;
#55195 = CARTESIAN_POINT ( 'NONE',  ( 11.68203264560385790, 1433.008677914359623, 150.9219369944972868 ) ) ;
#55196 = CARTESIAN_POINT ( 'NONE',  ( -3.200019046440000015, 1409.961299637529919, 232.4470946617979905 ) ) ;
#55198 = ORIENTED_EDGE ( 'NONE', *, *, #25421, .F. ) ;
#55197 = CARTESIAN_POINT ( 'NONE',  ( -9.668109322589998555, 1408.913060387329779, 193.5713027961979833 ) ) ;
#55199 = CARTESIAN_POINT ( 'NONE',  ( -113.4000000000000057, 1391.913060387289988, 304.2218459572590064 ) ) ;
#55200 = PLANE ( 'NONE',  #31751 ) ;
#55201 = CARTESIAN_POINT ( 'NONE',  ( -3.078458293520000222, 1384.558481699660206, 218.5731838834990128 ) ) ;
#55202 = VECTOR ( 'NONE', #75137, 1000.000000000000114 ) ;
#55203 = CARTESIAN_POINT ( 'NONE',  ( 20.15862645124139974, 1413.250162082850011, 270.0907330008120653 ) ) ;
#55204 = CARTESIAN_POINT ( 'NONE',  ( 0.7572979362240020995, 1516.829948096479939, 212.5714934102470011 ) ) ;
#55205 = CARTESIAN_POINT ( 'NONE',  ( -65.84461506920000318, 1379.745083454579799, 274.2711187272589655 ) ) ;
#55206 = CARTESIAN_POINT ( 'NONE',  ( 23.51556281730000109, 1410.708086401529954, 207.8137393032480134 ) ) ;
#55207 = DIRECTION ( 'NONE',  ( 0.000000000000000000, 1.000000000000000000, 0.000000000000000000 ) ) ;
#55208 = CARTESIAN_POINT ( 'NONE',  ( 8.632538001083871038, 1425.507033873999944, 193.3055192643680016 ) ) ;
#55209 = CARTESIAN_POINT ( 'NONE',  ( -7.708901244349819493, 1516.529320347400244, 211.1219528266759937 ) ) ;
#55210 = CARTESIAN_POINT ( 'NONE',  ( 7.726684687535000151, 1517.208444099459939, 210.2479840788170122 ) ) ;
#55211 = CARTESIAN_POINT ( 'NONE',  ( 4.325241530647730315, 1421.953609801759967, 183.9658289457019862 ) ) ;
#55212 = CARTESIAN_POINT ( 'NONE',  ( -2.344105919239999558, 1417.913736160830013, 233.0442052094980170 ) ) ;
#55213 = CARTESIAN_POINT ( 'NONE',  ( -96.24084593199999915, 1384.955172021569979, 310.5859090792589541 ) ) ;
#55214 = ORIENTED_EDGE ( 'NONE', *, *, #106560, .F. ) ;
#55216 = CARTESIAN_POINT ( 'NONE',  ( -22.41728899266079722, 1385.266610229700063, 222.0786659537150172 ) ) ;
#55215 = B_SPLINE_CURVE_WITH_KNOTS ( 'NONE', 3,
 ( #102693, #87597, #52350, #9763, #103831, #25988 ),
 .UNSPECIFIED., .F., .F.,
 ( 4, 2, 4 ),
 ( -1.131363979618622308E-05, 0.001067788114096023932, 0.002146889867988234155 ),
 .UNSPECIFIED. ) ;
#55217 = DIRECTION ( 'NONE',  ( -1.836970198721029688E-16, -1.000000000000000000, 0.000000000000000000 ) ) ;
#55218 = ADVANCED_FACE ( 'NONE', ( #29195 ), #95458, .T. ) ;
#55219 = CARTESIAN_POINT ( 'NONE',  ( 10.98083629090000102, 1433.016921068679949, 151.7694307944979926 ) ) ;
#55220 = CARTESIAN_POINT ( 'NONE',  ( -29.00779973304124937, 1526.382868172863937, 217.2942086403127178 ) ) ;
#55221 = CARTESIAN_POINT ( 'NONE',  ( 12.74774243120000072, 1426.600000495550148, 203.5345172987589990 ) ) ;
#55222 = DIRECTION ( 'NONE',  ( -0.6736849260863841948, 0.000000000000000000, 0.7390186874254148774 ) ) ;
#55224 = CARTESIAN_POINT ( 'NONE',  ( -16.62689959340567114, 1417.072749475663613, 207.5381517451929483 ) ) ;
#55223 = CARTESIAN_POINT ( 'NONE',  ( 3.261007131564999995, 1516.596789218710001, 216.4445556570670135 ) ) ;
#55225 = CARTESIAN_POINT ( 'NONE',  ( 18.67054467720000233, 1509.506033878430117, 187.1506692567980110 ) ) ;
#55226 = CARTESIAN_POINT ( 'NONE',  ( 9.953995014223000481, 1468.683952319419859, 207.9911765682120119 ) ) ;
#55227 = EDGE_LOOP ( 'NONE', ( #52485, #73900, #72259, #54612 ) ) ;
#55228 = CARTESIAN_POINT ( 'NONE',  ( -4.036119682645000317, 1516.647924054489977, 201.7978713257969900 ) ) ;
#55229 = CARTESIAN_POINT ( 'NONE',  ( 27.78452742954910093, 1508.000976259739900, 207.7754991261529938 ) ) ;
#55230 = ORIENTED_EDGE ( 'NONE', *, *, #78090, .F. ) ;
#55231 = CARTESIAN_POINT ( 'NONE',  ( 2.802883801854730184, 1485.536427198280080, 201.6817236178680162 ) ) ;
#55232 = ADVANCED_FACE ( 'NONE', ( #82350 ), #23599, .T. ) ;
#55233 = CARTESIAN_POINT ( 'NONE',  ( -14.94707557629999961, 1464.258769156330118, 228.3755978434980136 ) ) ;
#55234 = CARTESIAN_POINT ( 'NONE',  ( 7.993316216764522864, 1423.834663174395246, 195.8541102515277430 ) ) ;
#55235 = CARTESIAN_POINT ( 'NONE',  ( 1.198395538569999808, 1443.136157641690033, 218.0744600652089957 ) ) ;
#55236 = CARTESIAN_POINT ( 'NONE',  ( -26.76158160278550113, 1509.153336901769990, 201.3770876523819879 ) ) ;
#55237 = DIRECTION ( 'NONE',  ( -0.000000000000000000, -1.000000000000000000, -0.000000000000000000 ) ) ;
#55238 = CARTESIAN_POINT ( 'NONE',  ( -19.40520978109999817, 1426.254488764730240, 225.7391413128980275 ) ) ;
#55239 = CARTESIAN_POINT ( 'NONE',  ( -15.59584108210000153, 1436.279046110379795, 149.2248470810979768 ) ) ;
#55240 = CARTESIAN_POINT ( 'NONE',  ( -9.660544699540000835, 1432.353341358199941, 148.7316627034979888 ) ) ;
#55241 = CARTESIAN_POINT ( 'NONE',  ( 17.68711869539999881, 1428.828027849089949, 204.9896315466789929 ) ) ;
#55243 = CARTESIAN_POINT ( 'NONE',  ( 28.26971844670000422, 1508.651302070430120, 209.4063442215349937 ) ) ;
#55242 = CARTESIAN_POINT ( 'NONE',  ( 0.9518847404210000196, 1415.296882282229944, 191.1939211731979924 ) ) ;
#55244 = CARTESIAN_POINT ( 'NONE',  ( 0.5770119038902318254, 1525.581535527370534, 243.3912443123664673 ) ) ;
#55245 = ORIENTED_EDGE ( 'NONE', *, *, #4296, .T. ) ;
#55246 =( NAMED_UNIT ( * ) SI_UNIT ( $, .STERADIAN. ) SOLID_ANGLE_UNIT ( ) );
#55247 = DIRECTION ( 'NONE',  ( -0.5412924984494058567, 0.1391731009594480151, 0.8292365640103740443 ) ) ;
#55248 = CARTESIAN_POINT ( 'NONE',  ( 11.57168670579999947, 1440.669964955550086, 147.8294280051980252 ) ) ;
#55249 = B_SPLINE_CURVE_WITH_KNOTS ( 'NONE', 3,
 ( #44301, #19055, #45412, #94123 ),
 .UNSPECIFIED., .F., .F.,
 ( 4, 4 ),
 ( 0.000000000000000000, 1.000000000000000000 ),
 .UNSPECIFIED. ) ;
#55250 = CARTESIAN_POINT ( 'NONE',  ( -17.78793234590467875, 1523.919934424249959, 237.8334813054144661 ) ) ;
#55251 = CARTESIAN_POINT ( 'NONE',  ( -2.069830516030000123, 1485.439312555290144, 197.8250537956990058 ) ) ;
#55252 = CIRCLE ( 'NONE', #15788, 16.53861382824159421 ) ;
#55253 = CARTESIAN_POINT ( 'NONE',  ( -0.2626388801599250367, 1424.255108689230156, 227.7923674788299877 ) ) ;
#55254 = CARTESIAN_POINT ( 'NONE',  ( -2.458491834123362807, 1524.872178180562969, 242.3414668159568066 ) ) ;
#55255 = CARTESIAN_POINT ( 'NONE',  ( 15.28420222229999936, 1497.713060387329961, 224.4060481836980046 ) ) ;
#55256 = EDGE_CURVE ( 'NONE', #42516, #89999, #98656, .T. ) ;
#55257 = CARTESIAN_POINT ( 'NONE',  ( -24.80269070334470172, 1438.943490319260036, 210.4397421548250122 ) ) ;
#55258 = CARTESIAN_POINT ( 'NONE',  ( 3.300283013599780269, 1494.041687248919970, 219.7877414054240148 ) ) ;
#55259 = TOROIDAL_SURFACE ( 'NONE', #10472, 1.000000000000000000, 1.000000000000000000 ) ;
#55260 = CARTESIAN_POINT ( 'NONE',  ( 0.9103409915569969924, 1462.760008604990162, 230.5111369474990113 ) ) ;
#55261 = CARTESIAN_POINT ( 'NONE',  ( -15.31654147834860069, 1415.677402202140001, 208.8922298180530106 ) ) ;
#55262 = AXIS2_PLACEMENT_3D ( 'NONE', #35227, #69414, #103525 ) ;
#55263 = CARTESIAN_POINT ( 'NONE',  ( -109.6087247409329848, 1383.177901426799963, 311.2147930400129781 ) ) ;
#55265 = EDGE_CURVE ( 'NONE', #81551, #50617, #54025, .T. ) ;
#55264 = CARTESIAN_POINT ( 'NONE',  ( -8.486023334060126544, 1517.051704408389924, 211.0297173932031569 ) ) ;
#55267 = ORIENTED_EDGE ( 'NONE', *, *, #31835, .T. ) ;
#55266 = CARTESIAN_POINT ( 'NONE',  ( 22.22649075570000221, 1507.849990204029837, 192.4185849886980009 ) ) ;
#55268 = CARTESIAN_POINT ( 'NONE',  ( -103.6840079290000034, 1381.964784448540058, 297.7019806198590004 ) ) ;
#55269 = CARTESIAN_POINT ( 'NONE',  ( -0.4719925911955576980, 1416.019047136214112, 233.4884116122769910 ) ) ;
#55270 = EDGE_LOOP ( 'NONE', ( #5259, #105571, #63721, #64640 ) ) ;
#55271 = EDGE_LOOP ( 'NONE', ( #14149, #4306, #91440, #73389 ) ) ;
#55272 = CARTESIAN_POINT ( 'NONE',  ( -7.809009848659999697, 1492.243080287389830, 209.5285790274940041 ) ) ;
#55273 = B_SPLINE_CURVE_WITH_KNOTS ( 'NONE', 3,
 ( #44543, #11492, #4192, #28841, #104990, #20411 ),
 .UNSPECIFIED., .F., .F.,
 ( 4, 2, 4 ),
 ( 0.000000000000000000, 0.5000000000000000000, 1.000000000000000000 ),
 .UNSPECIFIED. ) ;
#55274 = CARTESIAN_POINT ( 'NONE',  ( -109.8948246550000079, 1384.907839483040107, 297.0284603415590254 ) ) ;
#55275 = CARTESIAN_POINT ( 'NONE',  ( 12.74312375647451923, 1442.824085801858928, 169.4555944935701746 ) ) ;
#55277 = CARTESIAN_POINT ( 'NONE',  ( -31.69751081680000127, 1445.012237272740094, 244.1892870111979903 ) ) ;
#55276 = CARTESIAN_POINT ( 'NONE',  ( 16.10313873473633706, 1412.736108363146059, 269.3694952781954726 ) ) ;
#55278 = CARTESIAN_POINT ( 'NONE',  ( 8.691006959535679144, 1437.158552202200099, 210.3927666437540154 ) ) ;
#55279 = CARTESIAN_POINT ( 'NONE',  ( -11.56494095969999947, 1433.721084582969979, 151.2190265359980117 ) ) ;
#55280 = CARTESIAN_POINT ( 'NONE',  ( 2.774288201250000085, 1480.748952858089979, 229.3996213013989802 ) ) ;
#55281 = CARTESIAN_POINT ( 'NONE',  ( -19.19763038940000044, 1485.731754976029833, 189.6998267162979914 ) ) ;
#55282 = CARTESIAN_POINT ( 'NONE',  ( 7.956123293573201138, 1465.862754146189900, 215.0084650448240211 ) ) ;
#55283 = CARTESIAN_POINT ( 'NONE',  ( -26.17054985310000248, 1441.643302933269752, 138.0857573384980128 ) ) ;
#55284 = CARTESIAN_POINT ( 'NONE',  ( -0.9886889294026209862, 1515.109643008300054, 213.4501202958599890 ) ) ;
#55285 = SPHERICAL_SURFACE ( 'NONE', #92654, 2.000000000000000000 ) ;
#55286 = CARTESIAN_POINT ( 'NONE',  ( 13.02959953899969925, 1428.519719725350114, 223.5607415246620064 ) ) ;
#55287 = CARTESIAN_POINT ( 'NONE',  ( -15.22421469840265473, 1509.566647593047492, 235.0174151826843172 ) ) ;
#55289 = ORIENTED_EDGE ( 'NONE', *, *, #836, .F. ) ;
#55288 = CARTESIAN_POINT ( 'NONE',  ( 4.323339341317169361E-09, 1410.103346783880170, 258.3459216912629586 ) ) ;
#55290 = ORIENTED_EDGE ( 'NONE', *, *, #23434, .F. ) ;
#55291 = CARTESIAN_POINT ( 'NONE',  ( -13.37159485409999959, 1504.309599599390140, 208.8294216085490120 ) ) ;
#55292 = CARTESIAN_POINT ( 'NONE',  ( -22.19118138694790332, 1483.601908343390051, 216.8115092454290220 ) ) ;
#55293 = CARTESIAN_POINT ( 'NONE',  ( -26.02835829340000018, 1468.278484548229926, 269.9886483896979712 ) ) ;
#55294 = CARTESIAN_POINT ( 'NONE',  ( -23.93171212618479515, 1435.912476962626442, 211.2679597967069753 ) ) ;
#55295 = CARTESIAN_POINT ( 'NONE',  ( -126.2838827870999836, 1371.894749952189613, 317.1057287443592827 ) ) ;
#55296 = CARTESIAN_POINT ( 'NONE',  ( -4.992349863779999453, 1391.620913471789891, 209.1218459612989875 ) ) ;
#55297 = CARTESIAN_POINT ( 'NONE',  ( 4.326992699989999913, 1515.158586642790169, 209.1218459614979963 ) ) ;
#55298 = CARTESIAN_POINT ( 'NONE',  ( -13.67687855990000045, 1421.535259874829990, 230.0823906799980136 ) ) ;
#55299 = CARTESIAN_POINT ( 'NONE',  ( -4.698255939499999201, 1458.218207492389865, 217.8981937722389830 ) ) ;
#55300 = CARTESIAN_POINT ( 'NONE',  ( 10.73349977660030419, 1361.841353345481366, 209.6218459617033432 ) ) ;
#55301 = CARTESIAN_POINT ( 'NONE',  ( -45.75303381261710456, 1435.540604548129977, 267.6079231741339868 ) ) ;
#55302 = ORIENTED_EDGE ( 'NONE', *, *, #90209, .T. ) ;
#55303 = CARTESIAN_POINT ( 'NONE',  ( -3.538418511287639845, 1496.496384395020186, 181.4297818474599922 ) ) ;
#55304 = ORIENTED_EDGE ( 'NONE', *, *, #25343, .F. ) ;
#55305 = EDGE_LOOP ( 'NONE', ( #25587, #60935, #83397 ) ) ;
#55306 = CARTESIAN_POINT ( 'NONE',  ( -7.321169269124999879, 1516.531533746980131, 210.8305669548069829 ) ) ;
#55307 = CARTESIAN_POINT ( 'NONE',  ( -33.23571934791657867, 1512.187213306747481, 219.4842663281467026 ) ) ;
#55308 = CARTESIAN_POINT ( 'NONE',  ( -20.59664500250000074, 1507.763472350229904, 190.3621299374980254 ) ) ;
#55309 = CARTESIAN_POINT ( 'NONE',  ( -15.76506831160000210, 1425.421718464029937, 190.4794369252980175 ) ) ;
#55310 = TOROIDAL_SURFACE ( 'NONE', #46367, 4.000000000000000000, 1.000000000000000000 ) ;
#55311 = CARTESIAN_POINT ( 'NONE',  ( -16.72257612350379929, 1470.459515107609832, 228.5670331555560040 ) ) ;
#55312 = B_SPLINE_SURFACE_WITH_KNOTS ( 'NONE', 5, 3, ( 
 ( #75976, #93861, #15494, #33401 ),
 ( #17129, #51319, #66508, #101704 ),
 ( #59199, #16580, #92223, #68161 ),
 ( #85455, #65948, #40720, #100074 ),
 ( #74892, #32327, #53003, #77635 ),
 ( #104487, #102805, #26101, #51891 ),
 ( #86580, #9872, #28336, #27780 ),
 ( #26662, #18255, #44596, #34521 ),
 ( #52451, #68700, #8753, #44039 ),
 ( #78178, #60863, #45160, #70931 ),
 ( #78740, #79300, #87136, #69253 ),
 ( #95535, #103360, #61970, #69816 ),
 ( #94987, #2055, #1489, #62529 ),
 ( #35072, #35620, #36736, #61412 ),
 ( #103933, #19359, #70372, #2611 ),
 ( #105047, #53560, #86028, #77094 ),
 ( #27232, #87707, #96651, #947 ),
 ( #60290, #9329, #94409, #18808 ),
 ( #19920, #96084, #10426, #36188 ),
 ( #10986, #54120, #17685, #42936 ),
 ( #404, #43492, #89887, #46816 ),
 ( #88248, #29975, #45716, #64167 ),
 ( #97740, #98285, #80945, #4244 ),
 ( #63088, #4775, #37844, #63624 ),
 ( #80400, #21011, #21562, #55772 ),
 ( #107797, #71487, #106684, #55213 ),
 ( #38379, #72031, #3164, #105608 ),
 ( #81472, #82030, #47894, #98840 ),
 ( #12079, #106147, #89342, #5334 ),
 ( #28892, #31082, #97186, #72554 ) ),
 .UNSPECIFIED., .F., .F., .F.,
 ( 6, 3, 3, 3, 3, 3, 3, 3, 3, 6 ),
 ( 4, 4 ),
 ( 0.000000000000000000, 15.39383910899999997, 27.58084801740000103, 41.39509552349999666, 65.53909258059999843, 90.91108773649999364, 117.6367619669999982, 132.4493970709999928, 144.8160795070000120, 161.8240513320000105 ),
 ( 68.11858234059999972, 68.97209088700000734 ),
 .UNSPECIFIED. ) ;
#55313 = ORIENTED_EDGE ( 'NONE', *, *, #109673, .F. ) ;
#55314 =( BOUNDED_CURVE ( )  B_SPLINE_CURVE ( 3, ( #71370, #4137, #47229, #47777 ),
 .UNSPECIFIED., .F., .F. ) 
 B_SPLINE_CURVE_WITH_KNOTS ( ( 4, 4 ),
 ( 6.031750460840100025, 6.430154037858700100 ),
 .UNSPECIFIED. ) 
 CURVE ( )  GEOMETRIC_REPRESENTATION_ITEM ( )  RATIONAL_B_SPLINE_CURVE ( ( 1.000000000000000000, 0.9868165638310153476, 0.9868165638310153476, 1.000000000000000000 ) ) 
 REPRESENTATION_ITEM ( '' )  );
#55315 = CARTESIAN_POINT ( 'NONE',  ( 0.7403205670290020635, 1517.139320148880188, 201.3969713189170250 ) ) ;
#55316 = AXIS2_PLACEMENT_3D ( 'NONE', #51545, #43150, #59414 ) ;
#55317 = CARTESIAN_POINT ( 'NONE',  ( 6.950546267860000071, 1473.247417472590087, 217.6958634347789712 ) ) ;
#55318 = CARTESIAN_POINT ( 'NONE',  ( -16.95855574732879845, 1384.526604847959788, 200.9892168643340256 ) ) ;
#55319 = VERTEX_POINT ( 'NONE', #5651 ) ;
#55320 = CARTESIAN_POINT ( 'NONE',  ( -8.333309592260910392, 1410.827525919379923, 269.6222470930029544 ) ) ;
#55321 = CARTESIAN_POINT ( 'NONE',  ( -33.52368697869999892, 1435.668148531879979, 135.0787117157979935 ) ) ;
#55322 = CARTESIAN_POINT ( 'NONE',  ( 9.788572749075168389, 1435.243968381529839, 208.4609852036589928 ) ) ;
#55324 = VERTEX_POINT ( 'NONE', #100777 ) ;
#55323 = CARTESIAN_POINT ( 'NONE',  ( -9.657355732032620210, 1366.083296228059908, 210.6218459616987957 ) ) ;
#55325 = ORIENTED_EDGE ( 'NONE', *, *, #105782, .T. ) ;
#55326 = CARTESIAN_POINT ( 'NONE',  ( 45.61858855260545909, 1441.895270504249311, 268.9752554369495670 ) ) ;
#55327 = CARTESIAN_POINT ( 'NONE',  ( -0.4964140083681939930, 1467.594909982409945, 220.2089270784179860 ) ) ;
#55328 = CARTESIAN_POINT ( 'NONE',  ( -13.72744925206639977, 1436.207725120319992, 150.3866072345499845 ) ) ;
#55329 = CARTESIAN_POINT ( 'NONE',  ( -1.097975305679999902, 1484.781735349930159, 182.0978467051980090 ) ) ;
#55330 = AXIS2_PLACEMENT_3D ( 'NONE', #74481, #91255, #32989 ) ;
#55331 = CARTESIAN_POINT ( 'NONE',  ( -18.05107215653380237, 1415.301705641620174, 207.5664288050670052 ) ) ;
#55332 = CARTESIAN_POINT ( 'NONE',  ( -20.05750684869999745, 1435.770533046819992, 223.2611708394980212 ) ) ;
#55333 = AXIS2_PLACEMENT_3D ( 'NONE', #45506, #28675, #18044 ) ;
#55334 = CARTESIAN_POINT ( 'NONE',  ( 10.62371075008579879, 1475.245696748350156, 266.9320703371920445 ) ) ;
#55335 = CARTESIAN_POINT ( 'NONE',  ( -1.521307588799736710, 1467.014991327842608, 235.3760082200168995 ) ) ;
#55336 = CARTESIAN_POINT ( 'NONE',  ( 8.370528965525000586, 1511.388520542559945, 204.5794305421269996 ) ) ;
#55337 = CARTESIAN_POINT ( 'NONE',  ( -7.337793750624999944, 1517.145312756229941, 206.2496372219370073 ) ) ;
#55338 = ORIENTED_EDGE ( 'NONE', *, *, #74340, .T. ) ;
#55339 = CARTESIAN_POINT ( 'NONE',  ( -40.71747595469150127, 1448.637563191999789, 135.6928038576120059 ) ) ;
#55340 = CARTESIAN_POINT ( 'NONE',  ( -1.781283055790834124, 1516.548117337739768, 201.8347555902114152 ) ) ;
#55341 = ORIENTED_EDGE ( 'NONE', *, *, #76138, .F. ) ;
#55342 = CARTESIAN_POINT ( 'NONE',  ( -5.199570074521043139, 1391.913060385946665, 214.4361776394624428 ) ) ;
#55343 = CARTESIAN_POINT ( 'NONE',  ( 25.32437023980250146, 1451.152985641890155, 137.2266721702760037 ) ) ;
#55344 = CARTESIAN_POINT ( 'NONE',  ( 14.34198504589999956, 1416.067629296030191, 196.9709775078979987 ) ) ;
#55345 = CARTESIAN_POINT ( 'NONE',  ( 2.446787376320000096, 1432.353341358199941, 150.2884730787980061 ) ) ;
#55346 = CARTESIAN_POINT ( 'NONE',  ( 20.84719162220000044, 1410.135659111530003, 199.9772158389280037 ) ) ;
#55347 = CARTESIAN_POINT ( 'NONE',  ( 21.92806520379999924, 1409.678805295229949, 207.4538581684380176 ) ) ;
#55348 = CARTESIAN_POINT ( 'NONE',  ( 16.47946573069999943, 1409.488537697930042, 225.3830611371980126 ) ) ;
#55349 = FACE_OUTER_BOUND ( 'NONE', #98963, .T. ) ;
#55350 = CARTESIAN_POINT ( 'NONE',  ( -1.393816646507353596, 1512.187213306747481, 175.1051575864439656 ) ) ;
#55351 = AXIS2_PLACEMENT_3D ( 'NONE', #81464, #23768, #75312 ) ;
#55352 = FACE_OUTER_BOUND ( 'NONE', #5429, .T. ) ;
#55353 = CARTESIAN_POINT ( 'NONE',  ( -5.776491133374999976, 1516.858301627840092, 214.9045953718370185 ) ) ;
#55354 = VERTEX_POINT ( 'NONE', #49309 ) ;
#55355 = CARTESIAN_POINT ( 'NONE',  ( 7.708856534992840182, 1516.527614422059742, 207.0328371564550025 ) ) ;
#55356 = CARTESIAN_POINT ( 'NONE',  ( -43.33646147129999804, 1450.475004575490175, 269.7148345228980020 ) ) ;
#55357 = CARTESIAN_POINT ( 'NONE',  ( -3.090150069089999896, 1448.281854555830023, 184.7281458456979806 ) ) ;
#55358 = EDGE_CURVE ( 'NONE', #97980, #109119, #80844, .T. ) ;
#55359 = DIRECTION ( 'NONE',  ( -1.000000000000000000, 0.000000000000000000, 0.000000000000000000 ) ) ;
#55360 = CARTESIAN_POINT ( 'NONE',  ( -40.24977539805779969, 1444.418635764679948, 137.0616282298240094 ) ) ;
#55361 = CARTESIAN_POINT ( 'NONE',  ( 10.89360413264559924, 1424.843095330547385, 138.2325533482020887 ) ) ;
#55362 = CARTESIAN_POINT ( 'NONE',  ( 1.871535769766313972, 1416.945233345094721, 232.8591253669631840 ) ) ;
#55363 = AXIS2_PLACEMENT_3D ( 'NONE', #83619, #104154, #103601 ) ;
#55364 = CARTESIAN_POINT ( 'NONE',  ( -1.736824869533450055, 1471.314969352929893, 183.3216726285400284 ) ) ;
#55365 = CARTESIAN_POINT ( 'NONE',  ( 11.42843422490000016, 1433.204776730410003, 151.3497024267980180 ) ) ;
#55366 = EDGE_CURVE ( 'NONE', #17126, #89621, #109753, .T. ) ;
#55367 = CARTESIAN_POINT ( 'NONE',  ( -0.2979719656898799918, 1474.175163955769904, 270.1377477033279888 ) ) ;
#55368 = CARTESIAN_POINT ( 'NONE',  ( 33.36193798735060057, 1440.913060383689981, 247.4361487871759948 ) ) ;
#55369 = CARTESIAN_POINT ( 'NONE',  ( -109.3535611529999869, 1385.012954933069977, 297.1394016240590759 ) ) ;
#55370 = DIRECTION ( 'NONE',  ( 0.000000000000000000, 0.000000000000000000, 1.000000000000000000 ) ) ;
#55371 = ORIENTED_EDGE ( 'NONE', *, *, #109623, .F. ) ;
#55372 = B_SPLINE_CURVE_WITH_KNOTS ( 'NONE', 3,
 ( #47544, #81664, #4969, #39114, #73294, #104417 ),
 .UNSPECIFIED., .F., .F.,
 ( 4, 2, 4 ),
 ( -1.285435071109504191E-05, 0.001079388306740602238, 0.002171630964192299267 ),
 .UNSPECIFIED. ) ;
#55373 = CARTESIAN_POINT ( 'NONE',  ( 10.66966122738459966, 1480.341429598930063, 208.7487408019889870 ) ) ;
#55374 = CARTESIAN_POINT ( 'NONE',  ( 21.63849897547177292, 1521.951704408389787, 202.6852139837136804 ) ) ;
#55375 = CARTESIAN_POINT ( 'NONE',  ( -6.036760179694757866, 1509.035273794851719, 201.6612099679530843 ) ) ;
#55376 = CARTESIAN_POINT ( 'NONE',  ( 2.366960022969999855, 1499.008374605230074, 235.6905257228980020 ) ) ;
#55377 = CARTESIAN_POINT ( 'NONE',  ( -16.77192111137985364, 1526.333389948038530, 234.9129815758640802 ) ) ;
#55378 = CARTESIAN_POINT ( 'NONE',  ( -10.16696763180000040, 1507.687626859330067, 234.4265286207979955 ) ) ;
#55379 = CARTESIAN_POINT ( 'NONE',  ( -17.93185251124669932, 1383.855712211560103, 220.0128206254979943 ) ) ;
#55380 = CARTESIAN_POINT ( 'NONE',  ( -2.402260219255893059, 1429.560837414985372, 200.7439439027626236 ) ) ;
#55381 = CARTESIAN_POINT ( 'NONE',  ( 9.874625061749998878, 1408.732483999830038, 219.1535762145979902 ) ) ;
#55382 = DIRECTION ( 'NONE',  ( 0.03489949670250328678, 0.9993908270190956511, 0.000000000000000000 ) ) ;
#55383 = CARTESIAN_POINT ( 'NONE',  ( 1.668433438889999954, 1465.936335742929941, 234.8595247571979883 ) ) ;
#55385 = VERTEX_POINT ( 'NONE', #58804 ) ;
#55384 = CARTESIAN_POINT ( 'NONE',  ( -0.4151546846821903003, 1501.977400791986611, 242.9330574173806951 ) ) ;
#55386 = CARTESIAN_POINT ( 'NONE',  ( -1.062268994950000156, 1452.003535646829960, 183.5021093084980066 ) ) ;
#55387 = VECTOR ( 'NONE', #76015, 1000.000000000000000 ) ;
#55388 = B_SPLINE_CURVE_WITH_KNOTS ( 'NONE', 5,
 ( #69266, #103372, #60875, #52462, #19934, #37306 ),
 .UNSPECIFIED., .F., .F.,
 ( 6, 6 ),
 ( -2.000000000000000000, 0.000000000000000000 ),
 .UNSPECIFIED. ) ;
#55389 = CARTESIAN_POINT ( 'NONE',  ( -8.753528060440000758, 1383.864184473070054, 218.4105340633189769 ) ) ;
#55390 = CARTESIAN_POINT ( 'NONE',  ( -3.674130623179999944, 1476.125971546490064, 199.4510817715890312 ) ) ;
#55392 = EDGE_LOOP ( 'NONE', ( #12542, #98093 ) ) ;
#55391 = CARTESIAN_POINT ( 'NONE',  ( -17.78809123684730054, 1415.431750870129918, 208.6136599671049794 ) ) ;
#55393 = CARTESIAN_POINT ( 'NONE',  ( -3.071489522903089853, 1470.850346192869893, 187.3986287140659783 ) ) ;
#55394 = ORIENTED_EDGE ( 'NONE', *, *, #83572, .T. ) ;
#55395 = CARTESIAN_POINT ( 'NONE',  ( -10.04612998989999895, 1389.631361075330005, 216.4686791083889830 ) ) ;
#55396 = CARTESIAN_POINT ( 'NONE',  ( 0.1948465599140009885, 1484.368352875590062, 201.1680343295390117 ) ) ;
#55397 = SPHERICAL_SURFACE ( 'NONE', #97714, 2.000000000000000000 ) ;
#55398 = AXIS2_PLACEMENT_3D ( 'NONE', #191, #68494, #94207 ) ;
#55399 = CARTESIAN_POINT ( 'NONE',  ( -4.329791550921825660, 1515.051704408389924, 213.0376480771455761 ) ) ;
#55400 = DIRECTION ( 'NONE',  ( -0.3090169943749382919, 0.000000000000000000, 0.9510565162951565288 ) ) ;
#55401 = CARTESIAN_POINT ( 'NONE',  ( 19.94580949735431119, 1509.638862839826970, 187.1591372636853237 ) ) ;
#55402 = CARTESIAN_POINT ( 'NONE',  ( 3.284408969210909746, 1409.027754475830079, 194.4977616889150056 ) ) ;
#55403 = CARTESIAN_POINT ( 'NONE',  ( -7.966091435999130610, 1384.906085766829847, 199.4893022481589924 ) ) ;
#55404 = CARTESIAN_POINT ( 'NONE',  ( -99.99640236783429259, 1385.220859795530032, 296.2804087198049956 ) ) ;
#55405 = CARTESIAN_POINT ( 'NONE',  ( -19.22188682119999825, 1463.226638649430242, 191.5163928844979750 ) ) ;
#55406 = CARTESIAN_POINT ( 'NONE',  ( -67.25967724030000738, 1379.748837366600128, 277.1187736907589851 ) ) ;
#55407 = VECTOR ( 'NONE', #25302, 1000.000000000000000 ) ;
#55408 = ORIENTED_EDGE ( 'NONE', *, *, #12469, .T. ) ;
#55409 = VERTEX_POINT ( 'NONE', #65009 ) ;
#55410 = CARTESIAN_POINT ( 'NONE',  ( 18.88880210473057275, 1524.667648926078527, 238.8296805722605427 ) ) ;
#55411 = CARTESIAN_POINT ( 'NONE',  ( -11.20854089327220038, 1414.996442620800053, 195.7122650692939771 ) ) ;
#55412 = CARTESIAN_POINT ( 'NONE',  ( -5.445055359510000415, 1494.866998062989978, 198.0707221814990078 ) ) ;
#55413 = CARTESIAN_POINT ( 'NONE',  ( -5.978054922203370145E-10, 1467.128867830870149, 245.4363362049380157 ) ) ;
#55414 = CARTESIAN_POINT ( 'NONE',  ( -20.08192399753360036, 1491.083939665490107, 190.8757460896890166 ) ) ;
#55415 = CARTESIAN_POINT ( 'NONE',  ( -33.91376666158920017, 1435.681799711289841, 142.5056097235880088 ) ) ;
#55416 = CARTESIAN_POINT ( 'NONE',  ( -109.4004660420000050, 1385.924158871910095, 311.2011470452590061 ) ) ;
#55417 = CARTESIAN_POINT ( 'NONE',  ( 0.2140911838630000230, 1455.057671371630022, 183.1651298794979823 ) ) ;
#55418 = CARTESIAN_POINT ( 'NONE',  ( -11.23480159415162127, 1364.918251046870182, 210.6218459617030021 ) ) ;
#55419 = CARTESIAN_POINT ( 'NONE',  ( -26.53007446348713216, 1436.732360642813092, 136.8044313116533033 ) ) ;
#55420 = CARTESIAN_POINT ( 'NONE',  ( -21.91582132105330061, 1491.015012752149914, 208.5287076380759856 ) ) ;
#55421 = CARTESIAN_POINT ( 'NONE',  ( 3.253301381255000013, 1516.790374942449944, 207.9863856151469861 ) ) ;
#55422 = AXIS2_PLACEMENT_3D ( 'NONE', #17477, #93105, #8001 ) ;
#55423 = CARTESIAN_POINT ( 'NONE',  ( 11.31370220690210004, 1433.949489476620101, 151.5139277432949996 ) ) ;
#55424 = CARTESIAN_POINT ( 'NONE',  ( -13.38570636064689801, 1434.932240567770123, 149.1199053445120057 ) ) ;
#55425 = B_SPLINE_CURVE_WITH_KNOTS ( 'NONE', 3,
 ( #17836, #60444, #92915, #16188, #103516, #25143, #85603, #59347, #93456, #8904, #35219, #1093 ),
 .UNSPECIFIED., .F., .F.,
 ( 4, 2, 2, 2, 2, 4 ),
 ( 0.000000000000000000, 0.0007194225121804019834, 0.001079133768270288231, 0.001438845024360174262, 0.002158267536539345676, 0.002877690048718516656 ),
 .UNSPECIFIED. ) ;
#55426 = CARTESIAN_POINT ( 'NONE',  ( -8.600120389129999765, 1385.305366698150010, 218.6461194263490029 ) ) ;
#55427 = B_SPLINE_SURFACE_WITH_KNOTS ( 'NONE', 5, 5, ( 
 ( #91737, #49209, #107432, #83337, #109114, #66575 ),
 ( #100680, #99023, #23963, #7193, #92288, #30727 ),
 ( #75518, #67117, #24516, #58706, #64912, #18324 ),
 ( #17755, #92838, #26174, #34038, #95057, #16114 ),
 ( #9941, #68775, #1562, #52515, #93932, #25620 ),
 ( #33467, #44113, #102876, #103433, #34590, #35694 ),
 ( #35142, #69883, #43556, #77164, #78248, #7732 ),
 ( #466, #60361, #85527, #103999, #84446, #86645 ),
 ( #26739, #110194, #27296, #77706, #102335, #50319 ),
 ( #94483, #41893, #43006, #68229, #51394, #59812 ),
 ( #76050, #8821, #67668, #101774, #60927, #51958 ),
 ( #86100, #9393, #1016, #69325, #17198, #25065 ),
 ( #59268, #93385, #16652, #50849, #84978, #8272 ),
 ( #42437, #76596, #110747, #27853, #54186, #70997 ),
 ( #78812, #36806, #20528, #79367, #105679, #62034 ),
 ( #12147, #88313, #72097, #11606, #45784, #44671 ),
 ( #5829, #95604, #96157, #19434, #80468, #18872 ),
 ( #19993, #53634, #79919, #53070, #70439, #54734 ),
 ( #82533, #39968, #36251, #28407, #62605, #28963 ),
 ( #48390, #96720, #61477, #3232, #74144, #37360 ),
 ( #106212, #11058, #87777, #104558, #2681, #3784 ) ),
 .UNSPECIFIED., .F., .F., .F.,
 ( 6, 3, 3, 3, 3, 3, 6 ),
 ( 6, 6 ),
 ( 7.218912043000000445, 9.328012329869999064, 9.942138423719999452, 11.64113835680000086, 13.34013828990000050, 16.73813815620000156, 26.25736426930000178 ),
 ( 0.000000000000000000, 1.452619041900000019 ),
 .UNSPECIFIED. ) ;
#55428 = CARTESIAN_POINT ( 'NONE',  ( 0.9043163146260000396, 1416.826388498530150, 190.2146394413979920 ) ) ;
#55429 = DIRECTION ( 'NONE',  ( -0.9455185755993178454, 0.000000000000000000, 0.3255681544571537578 ) ) ;
#55430 = CARTESIAN_POINT ( 'NONE',  ( -0.03226023477341029982, 1410.297896964309984, 185.0217421575940193 ) ) ;
#55431 = ORIENTED_EDGE ( 'NONE', *, *, #12235, .F. ) ;
#55432 = CARTESIAN_POINT ( 'NONE',  ( 22.71362857069999919, 1419.354696852330108, 250.3594883046980044 ) ) ;
#55433 = CARTESIAN_POINT ( 'NONE',  ( -25.79285008269999935, 1449.806912625419727, 208.9767609917279856 ) ) ;
#55435 = CARTESIAN_POINT ( 'NONE',  ( -17.37499910009999837, 1409.684548448330133, 195.3411345723980048 ) ) ;
#55434 = CARTESIAN_POINT ( 'NONE',  ( -10.73442984997090122, 1425.687098426139983, 96.72829437425519927 ) ) ;
#55436 = EDGE_CURVE ( 'NONE', #89438, #4434, #50419, .T. ) ;
#55437 = CARTESIAN_POINT ( 'NONE',  ( -5.513435596746664835, 1508.909942010400982, 216.6312267329172130 ) ) ;
#55438 = AXIS2_PLACEMENT_3D ( 'NONE', #39848, #85691, #67818 ) ;
#55439 = CARTESIAN_POINT ( 'NONE',  ( -25.00557955649999897, 1440.913060507210048, 216.3898167415980254 ) ) ;
#55440 = CARTESIAN_POINT ( 'NONE',  ( -0.1956928720520010045, 1486.480037045490008, 220.3153739831990094 ) ) ;
#55441 = EDGE_CURVE ( 'NONE', #98871, #45131, #100497, .T. ) ;
#55442 = EDGE_CURVE ( 'NONE', #52269, #98270, #31520, .T. ) ;
#55443 = CARTESIAN_POINT ( 'NONE',  ( 19.93609162699999970, 1473.378341243790146, 206.2392384464789927 ) ) ;
#55444 = CARTESIAN_POINT ( 'NONE',  ( 30.22859042230000171, 1450.569347608749922, 136.3539440427979912 ) ) ;
#55445 = VERTEX_POINT ( 'NONE', #108089 ) ;
#55446 = CARTESIAN_POINT ( 'NONE',  ( 11.86100282799569960, 1492.894947744830006, 212.5846961511890072 ) ) ;
#55447 = CARTESIAN_POINT ( 'NONE',  ( 14.59148176577614286, 1514.407859707509942, 225.5030876066963685 ) ) ;
#55448 = CARTESIAN_POINT ( 'NONE',  ( 14.38071629740000112, 1509.494656480429967, 235.3234905946980007 ) ) ;
#55449 = EDGE_LOOP ( 'NONE', ( #12863, #29938, #57128, #103918 ) ) ;
#55450 = ORIENTED_EDGE ( 'NONE', *, *, #93946, .T. ) ;
#55451 = CARTESIAN_POINT ( 'NONE',  ( -10.75295827156603679, 1424.459136614693080, 137.8404512415733905 ) ) ;
#55452 = CARTESIAN_POINT ( 'NONE',  ( 5.898946028590000168, 1423.982493417579917, 194.4067087233990208 ) ) ;
#55453 = B_SPLINE_CURVE_WITH_KNOTS ( 'NONE', 5,
 ( #79458, #69978, #70529, #27943, #28495, #2222, #61564, #77797, #63237, #11692, #78916, #18965, #27385, #19525, #45866, #53160, #26838, #36335, #69422, #104093, #105766 ),
 .UNSPECIFIED., .F., .F.,
 ( 6, 3, 3, 3, 3, 3, 6 ),
 ( 0.000000000000000000, 0.08423072362349257047, 0.2167650270835284054, 0.3492993305435642126, 0.4887865076447485690, 0.6285375814380548265, 1.000000000000000000 ),
 .UNSPECIFIED. ) ;
#55454 = ORIENTED_EDGE ( 'NONE', *, *, #12755, .T. ) ;
#55455 = CARTESIAN_POINT ( 'NONE',  ( -12.09623089429489973, 1446.031664988779994, 193.6906620567080211 ) ) ;
#55456 = CARTESIAN_POINT ( 'NONE',  ( 7.630940151131325067, 1446.706835311024179, 154.1372093844152857 ) ) ;
